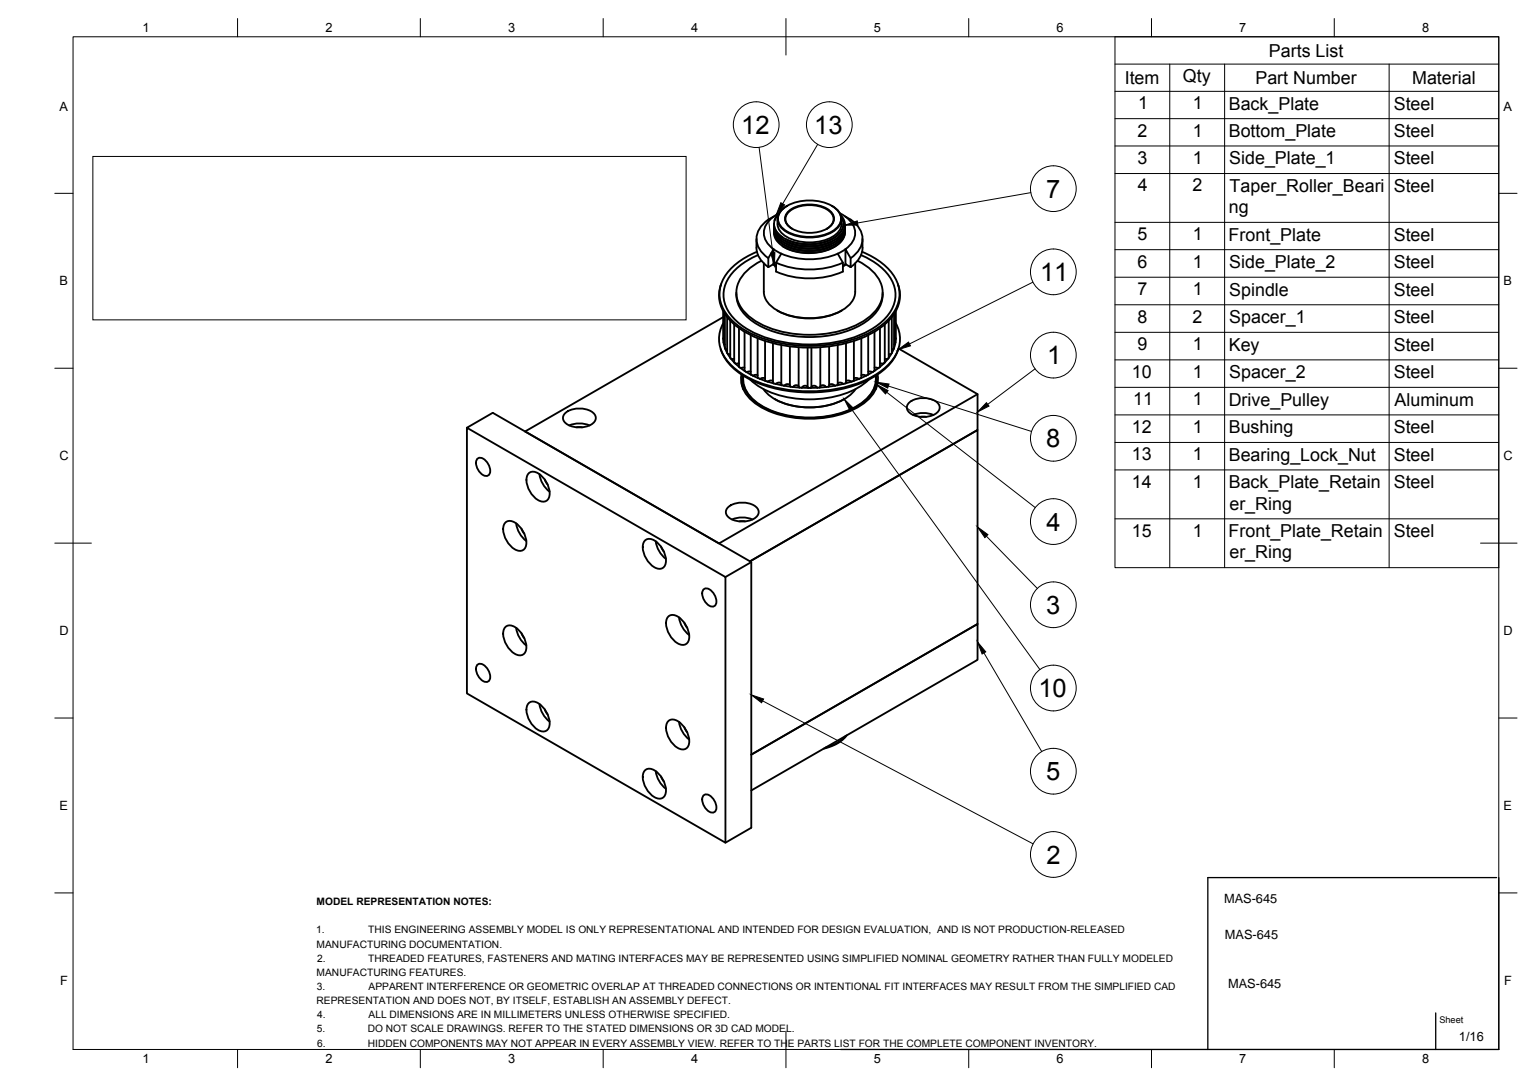
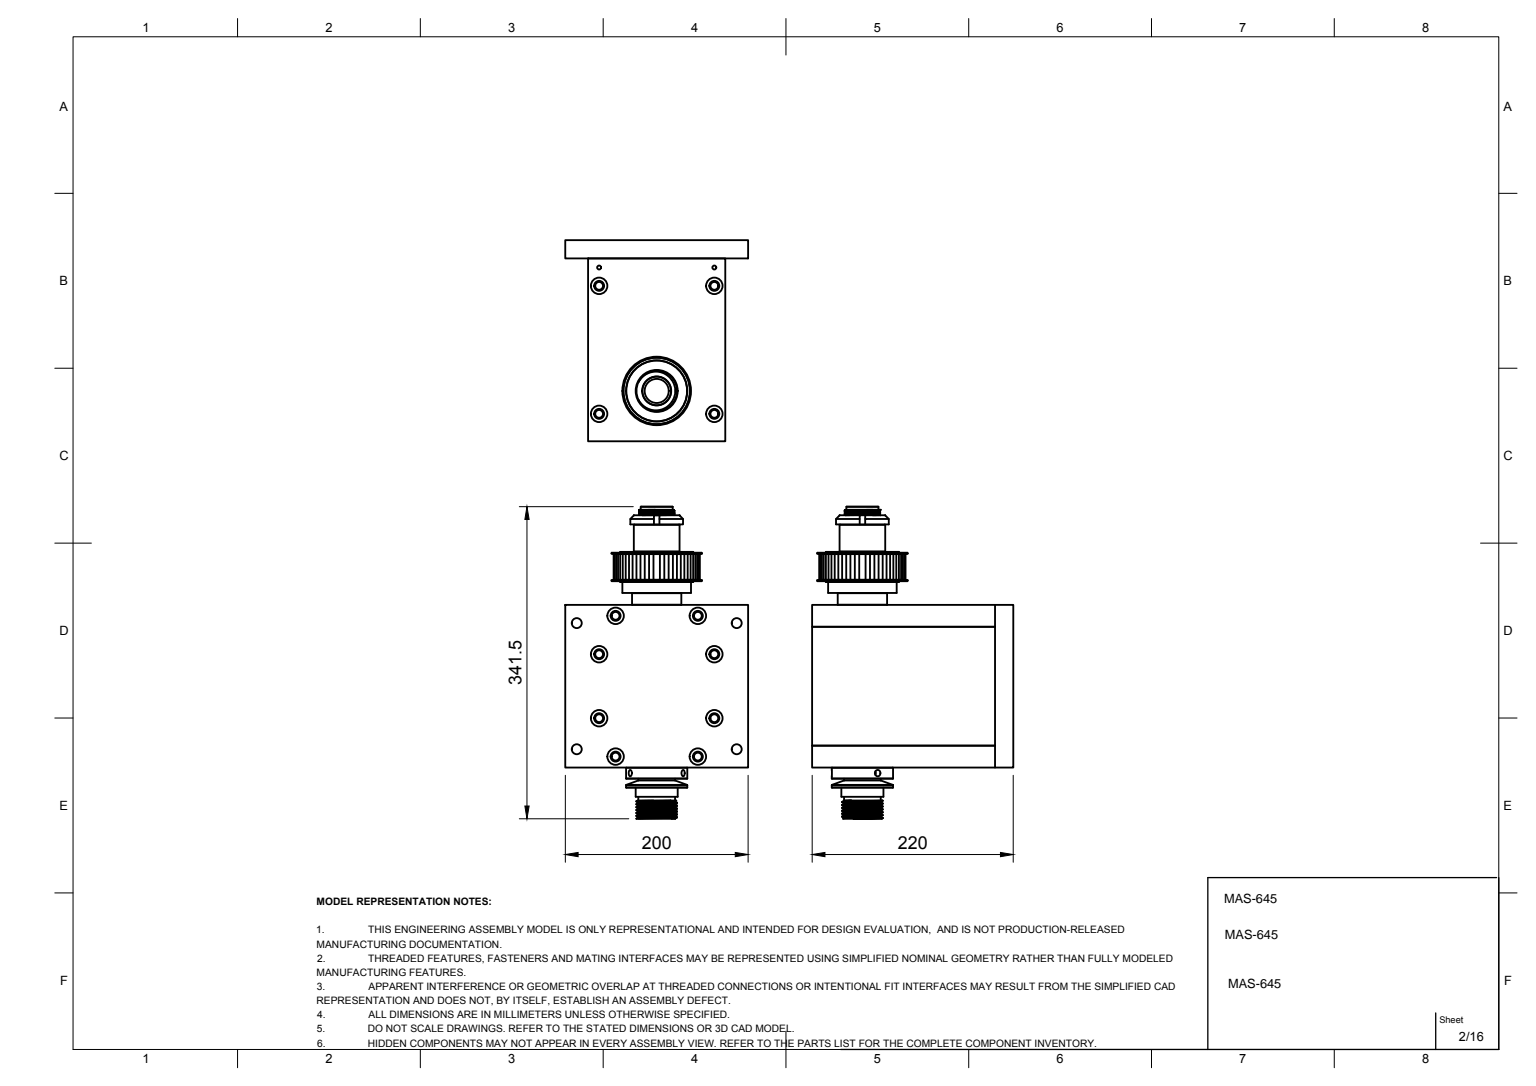
ISO-10303-21;
HEADER;
FILE_DESCRIPTION((''),'2;1');
FILE_NAME('MAS-645','2026-10-09T10:54:55-07:00',(''),(''),'','','');
FILE_SCHEMA (('AUTOMOTIVE_DESIGN { 1 0 10303 214 3 1 1 }'));
ENDSEC;
DATA;
#10 = MECHANICAL_DESIGN_GEOMETRIC_PRESENTATION_REPRESENTATION('',(#595,#596,
#597,#598,#599,#600,#601,#602,#603,#604,#605,#606,#607,#608,#609),#63824) ;
#11 = ITEM_DEFINED_TRANSFORMATION($,$,#15676,#17885) ;
#12 = ITEM_DEFINED_TRANSFORMATION($,$,#15762,#17886) ;
#13 = ITEM_DEFINED_TRANSFORMATION($,$,#15853,#17887) ;
#14 = ITEM_DEFINED_TRANSFORMATION($,$,#17272,#17888) ;
#15 = ITEM_DEFINED_TRANSFORMATION($,$,#15892,#17889) ;
#16 = ITEM_DEFINED_TRANSFORMATION($,$,#15986,#17890) ;
#17 = ITEM_DEFINED_TRANSFORMATION($,$,#16025,#17891) ;
#18 = ITEM_DEFINED_TRANSFORMATION($,$,#17802,#17892) ;
#19 = ITEM_DEFINED_TRANSFORMATION($,$,#16168,#17893) ;
#20 = ITEM_DEFINED_TRANSFORMATION($,$,#16191,#17894) ;
#21 = ITEM_DEFINED_TRANSFORMATION($,$,#16208,#17895) ;
#22 = ITEM_DEFINED_TRANSFORMATION($,$,#17207,#17896) ;
#23 = ITEM_DEFINED_TRANSFORMATION($,$,#17226,#17897) ;
#24 = ITEM_DEFINED_TRANSFORMATION($,$,#17272,#17898) ;
#25 = ITEM_DEFINED_TRANSFORMATION($,$,#17802,#17899) ;
#26 = ITEM_DEFINED_TRANSFORMATION($,$,#17819,#17900) ;
#27 = ITEM_DEFINED_TRANSFORMATION($,$,#17852,#17901) ;
#28 = (
REPRESENTATION_RELATIONSHIP($,$,#63879,#63878)
REPRESENTATION_RELATIONSHIP_WITH_TRANSFORMATION(#11)
SHAPE_REPRESENTATION_RELATIONSHIP()
) ;
#29 = (
REPRESENTATION_RELATIONSHIP($,$,#63880,#63878)
REPRESENTATION_RELATIONSHIP_WITH_TRANSFORMATION(#12)
SHAPE_REPRESENTATION_RELATIONSHIP()
) ;
#30 = (
REPRESENTATION_RELATIONSHIP($,$,#63881,#63878)
REPRESENTATION_RELATIONSHIP_WITH_TRANSFORMATION(#13)
SHAPE_REPRESENTATION_RELATIONSHIP()
) ;
#31 = (
REPRESENTATION_RELATIONSHIP($,$,#63890,#63878)
REPRESENTATION_RELATIONSHIP_WITH_TRANSFORMATION(#14)
SHAPE_REPRESENTATION_RELATIONSHIP()
) ;
#32 = (
REPRESENTATION_RELATIONSHIP($,$,#63882,#63878)
REPRESENTATION_RELATIONSHIP_WITH_TRANSFORMATION(#15)
SHAPE_REPRESENTATION_RELATIONSHIP()
) ;
#33 = (
REPRESENTATION_RELATIONSHIP($,$,#63883,#63878)
REPRESENTATION_RELATIONSHIP_WITH_TRANSFORMATION(#16)
SHAPE_REPRESENTATION_RELATIONSHIP()
) ;
#34 = (
REPRESENTATION_RELATIONSHIP($,$,#63884,#63878)
REPRESENTATION_RELATIONSHIP_WITH_TRANSFORMATION(#17)
SHAPE_REPRESENTATION_RELATIONSHIP()
) ;
#35 = (
REPRESENTATION_RELATIONSHIP($,$,#63891,#63878)
REPRESENTATION_RELATIONSHIP_WITH_TRANSFORMATION(#18)
SHAPE_REPRESENTATION_RELATIONSHIP()
) ;
#36 = (
REPRESENTATION_RELATIONSHIP($,$,#63885,#63878)
REPRESENTATION_RELATIONSHIP_WITH_TRANSFORMATION(#19)
SHAPE_REPRESENTATION_RELATIONSHIP()
) ;
#37 = (
REPRESENTATION_RELATIONSHIP($,$,#63886,#63878)
REPRESENTATION_RELATIONSHIP_WITH_TRANSFORMATION(#20)
SHAPE_REPRESENTATION_RELATIONSHIP()
) ;
#38 = (
REPRESENTATION_RELATIONSHIP($,$,#63887,#63878)
REPRESENTATION_RELATIONSHIP_WITH_TRANSFORMATION(#21)
SHAPE_REPRESENTATION_RELATIONSHIP()
) ;
#39 = (
REPRESENTATION_RELATIONSHIP($,$,#63888,#63878)
REPRESENTATION_RELATIONSHIP_WITH_TRANSFORMATION(#22)
SHAPE_REPRESENTATION_RELATIONSHIP()
) ;
#40 = (
REPRESENTATION_RELATIONSHIP($,$,#63889,#63878)
REPRESENTATION_RELATIONSHIP_WITH_TRANSFORMATION(#23)
SHAPE_REPRESENTATION_RELATIONSHIP()
) ;
#41 = (
REPRESENTATION_RELATIONSHIP($,$,#63890,#63878)
REPRESENTATION_RELATIONSHIP_WITH_TRANSFORMATION(#24)
SHAPE_REPRESENTATION_RELATIONSHIP()
) ;
#42 = (
REPRESENTATION_RELATIONSHIP($,$,#63891,#63878)
REPRESENTATION_RELATIONSHIP_WITH_TRANSFORMATION(#25)
SHAPE_REPRESENTATION_RELATIONSHIP()
) ;
#43 = (
REPRESENTATION_RELATIONSHIP($,$,#63892,#63878)
REPRESENTATION_RELATIONSHIP_WITH_TRANSFORMATION(#26)
SHAPE_REPRESENTATION_RELATIONSHIP()
) ;
#44 = (
REPRESENTATION_RELATIONSHIP($,$,#63893,#63878)
REPRESENTATION_RELATIONSHIP_WITH_TRANSFORMATION(#27)
SHAPE_REPRESENTATION_RELATIONSHIP()
) ;
#45 = CONTEXT_DEPENDENT_SHAPE_REPRESENTATION(#28,#63861) ;
#46 = CONTEXT_DEPENDENT_SHAPE_REPRESENTATION(#29,#63862) ;
#47 = CONTEXT_DEPENDENT_SHAPE_REPRESENTATION(#30,#63863) ;
#48 = CONTEXT_DEPENDENT_SHAPE_REPRESENTATION(#31,#63864) ;
#49 = CONTEXT_DEPENDENT_SHAPE_REPRESENTATION(#32,#63865) ;
#50 = CONTEXT_DEPENDENT_SHAPE_REPRESENTATION(#33,#63866) ;
#51 = CONTEXT_DEPENDENT_SHAPE_REPRESENTATION(#34,#63867) ;
#52 = CONTEXT_DEPENDENT_SHAPE_REPRESENTATION(#35,#63868) ;
#53 = CONTEXT_DEPENDENT_SHAPE_REPRESENTATION(#36,#63869) ;
#54 = CONTEXT_DEPENDENT_SHAPE_REPRESENTATION(#37,#63870) ;
#55 = CONTEXT_DEPENDENT_SHAPE_REPRESENTATION(#38,#63871) ;
#56 = CONTEXT_DEPENDENT_SHAPE_REPRESENTATION(#39,#63872) ;
#57 = CONTEXT_DEPENDENT_SHAPE_REPRESENTATION(#40,#63873) ;
#58 = CONTEXT_DEPENDENT_SHAPE_REPRESENTATION(#41,#63874) ;
#59 = CONTEXT_DEPENDENT_SHAPE_REPRESENTATION(#42,#63875) ;
#60 = CONTEXT_DEPENDENT_SHAPE_REPRESENTATION(#43,#63876) ;
#61 = CONTEXT_DEPENDENT_SHAPE_REPRESENTATION(#44,#63877) ;
#62 = NEXT_ASSEMBLY_USAGE_OCCURRENCE('Back_Plate:1','Back_Plate:1',
'Back_Plate:1',#63895,#63896,'Back_Plate:1') ;
#63 = NEXT_ASSEMBLY_USAGE_OCCURRENCE('Bottom_Plate:1','Bottom_Plate:1',
'Bottom_Plate:1',#63895,#63897,'Bottom_Plate:1') ;
#64 = NEXT_ASSEMBLY_USAGE_OCCURRENCE('Side_Plate_1:1','Side_Plate_1:1',
'Side_Plate_1:1',#63895,#63898,'Side_Plate_1:1') ;
#65 = NEXT_ASSEMBLY_USAGE_OCCURRENCE('Taper_Roller_Bearing:1',
'Taper_Roller_Bearing:1','Taper_Roller_Bearing:1',#63895,#63907,
'Taper_Roller_Bearing:1') ;
#66 = NEXT_ASSEMBLY_USAGE_OCCURRENCE('Front_Plate:1','Front_Plate:1',
'Front_Plate:1',#63895,#63899,'Front_Plate:1') ;
#67 = NEXT_ASSEMBLY_USAGE_OCCURRENCE('Side_Plate_2:1','Side_Plate_2:1',
'Side_Plate_2:1',#63895,#63900,'Side_Plate_2:1') ;
#68 = NEXT_ASSEMBLY_USAGE_OCCURRENCE('Spindle:1','Spindle:1','Spindle:1',
#63895,#63901,'Spindle:1') ;
#69 = NEXT_ASSEMBLY_USAGE_OCCURRENCE('Spacer_1:1','Spacer_1:1',
'Spacer_1:1',#63895,#63908,'Spacer_1:1') ;
#70 = NEXT_ASSEMBLY_USAGE_OCCURRENCE('Key:1','Key:1','Key:1',#63895,#63902,
'Key:1') ;
#71 = NEXT_ASSEMBLY_USAGE_OCCURRENCE('Spacer_2:1','Spacer_2:1',
'Spacer_2:1',#63895,#63903,'Spacer_2:1') ;
#72 = NEXT_ASSEMBLY_USAGE_OCCURRENCE('Drive_Pulley:1','Drive_Pulley:1',
'Drive_Pulley:1',#63895,#63904,'Drive_Pulley:1') ;
#73 = NEXT_ASSEMBLY_USAGE_OCCURRENCE('Bushing:1','Bushing:1','Bushing:1',
#63895,#63905,'Bushing:1') ;
#74 = NEXT_ASSEMBLY_USAGE_OCCURRENCE('Bearing_Lock_Nut:1',
'Bearing_Lock_Nut:1','Bearing_Lock_Nut:1',#63895,#63906,
'Bearing_Lock_Nut:1') ;
#75 = NEXT_ASSEMBLY_USAGE_OCCURRENCE('Taper_Roller_Bearing:2',
'Taper_Roller_Bearing:2','Taper_Roller_Bearing:2',#63895,#63907,
'Taper_Roller_Bearing:2') ;
#76 = NEXT_ASSEMBLY_USAGE_OCCURRENCE('Spacer_1:2','Spacer_1:2',
'Spacer_1:2',#63895,#63908,'Spacer_1:2') ;
#77 = NEXT_ASSEMBLY_USAGE_OCCURRENCE('Back_Plate_Retainer_Ring:1',
'Back_Plate_Retainer_Ring:1','Back_Plate_Retainer_Ring:1',#63895,#63909,
'Back_Plate_Retainer_Ring:1') ;
#78 = NEXT_ASSEMBLY_USAGE_OCCURRENCE('Front_Plate_Retainer_Ring:1',
'Front_Plate_Retainer_Ring:1','Front_Plate_Retainer_Ring:1',#63895,#63910,
'Front_Plate_Retainer_Ring:1') ;
#79 = TOROIDAL_SURFACE('',#17489,23.5,1.) ;
#80 = TOROIDAL_SURFACE('',#17493,36.5,1.) ;
#81 = TOROIDAL_SURFACE('',#17497,37.25,0.25) ;
#82 = TOROIDAL_SURFACE('',#17503,22.75,0.249999999999998) ;
#83 = (
BOUNDED_CURVE()
B_SPLINE_CURVE(2,(#53752,#53753,#53754),.UNSPECIFIED.,.F.,.F.)
B_SPLINE_CURVE_WITH_KNOTS((3,3),(0.,0.567460423251311),.UNSPECIFIED.)
CURVE()
GEOMETRIC_REPRESENTATION_ITEM()
RATIONAL_B_SPLINE_CURVE((1.,1.00278960134448,1.))
REPRESENTATION_ITEM('')
) ;
#84 = (
BOUNDED_CURVE()
B_SPLINE_CURVE(2,(#53763,#53764,#53765),.UNSPECIFIED.,.F.,.F.)
B_SPLINE_CURVE_WITH_KNOTS((3,3),(0.,0.567460423251311),.UNSPECIFIED.)
CURVE()
GEOMETRIC_REPRESENTATION_ITEM()
RATIONAL_B_SPLINE_CURVE((1.,1.00278960136551,1.))
REPRESENTATION_ITEM('')
) ;
#85 = (
BOUNDED_CURVE()
B_SPLINE_CURVE(2,(#53809,#53810,#53811),.UNSPECIFIED.,.F.,.F.)
B_SPLINE_CURVE_WITH_KNOTS((3,3),(0.,0.567460423251311),.UNSPECIFIED.)
CURVE()
GEOMETRIC_REPRESENTATION_ITEM()
RATIONAL_B_SPLINE_CURVE((1.,1.00278960136494,1.))
REPRESENTATION_ITEM('')
) ;
#86 = (
BOUNDED_CURVE()
B_SPLINE_CURVE(2,(#53815,#53816,#53817),.UNSPECIFIED.,.F.,.F.)
B_SPLINE_CURVE_WITH_KNOTS((3,3),(0.,0.567460423251311),.UNSPECIFIED.)
CURVE()
GEOMETRIC_REPRESENTATION_ITEM()
RATIONAL_B_SPLINE_CURVE((1.,1.0027896013635,1.))
REPRESENTATION_ITEM('')
) ;
#87 = (
BOUNDED_CURVE()
B_SPLINE_CURVE(2,(#53831,#53832,#53833),.UNSPECIFIED.,.F.,.F.)
B_SPLINE_CURVE_WITH_KNOTS((3,3),(0.,0.567460423251311),.UNSPECIFIED.)
CURVE()
GEOMETRIC_REPRESENTATION_ITEM()
RATIONAL_B_SPLINE_CURVE((1.,1.0027896013647,1.))
REPRESENTATION_ITEM('')
) ;
#88 = (
BOUNDED_CURVE()
B_SPLINE_CURVE(2,(#53837,#53838,#53839),.UNSPECIFIED.,.F.,.F.)
B_SPLINE_CURVE_WITH_KNOTS((3,3),(0.,0.567460423251311),.UNSPECIFIED.)
CURVE()
GEOMETRIC_REPRESENTATION_ITEM()
RATIONAL_B_SPLINE_CURVE((1.,1.002789601364,1.))
REPRESENTATION_ITEM('')
) ;
#89 = (
BOUNDED_CURVE()
B_SPLINE_CURVE(2,(#53853,#53854,#53855),.UNSPECIFIED.,.F.,.F.)
B_SPLINE_CURVE_WITH_KNOTS((3,3),(0.,0.56746042325131),.UNSPECIFIED.)
CURVE()
GEOMETRIC_REPRESENTATION_ITEM()
RATIONAL_B_SPLINE_CURVE((1.,1.00278960137803,1.))
REPRESENTATION_ITEM('')
) ;
#90 = (
BOUNDED_CURVE()
B_SPLINE_CURVE(2,(#53859,#53860,#53861),.UNSPECIFIED.,.F.,.F.)
B_SPLINE_CURVE_WITH_KNOTS((3,3),(0.,0.56746042325131),.UNSPECIFIED.)
CURVE()
GEOMETRIC_REPRESENTATION_ITEM()
RATIONAL_B_SPLINE_CURVE((1.,1.00278960137803,1.))
REPRESENTATION_ITEM('')
) ;
#91 = ELLIPSE('',#16171,7.07106781186547,5.) ;
#92 = ELLIPSE('',#16172,7.07106781186548,5.) ;
#93 = ELLIPSE('',#16174,7.07106781186548,5.) ;
#94 = ELLIPSE('',#16175,7.07106781186547,5.) ;
#95 = ELLIPSE('',#16178,7.07106781186546,4.99999999999999) ;
#96 = ELLIPSE('',#16180,7.07106781186546,4.99999999999999) ;
#97 = ELLIPSE('',#16181,7.07106781186546,4.99999999999999) ;
#98 = ELLIPSE('',#16183,7.07106781186546,4.99999999999999) ;
#99 = ELLIPSE('',#17336,29.1332609148258,28.6226076794831) ;
#100 = ELLIPSE('',#17338,29.1332609148259,28.622607679483) ;
#101 = ELLIPSE('',#17340,29.133260914826,28.6226076794829) ;
#102 = ELLIPSE('',#17342,29.1332609148258,28.622607679483) ;
#103 = ELLIPSE('',#17344,29.1332609148258,28.6226076794831) ;
#104 = ELLIPSE('',#17346,29.1332609148257,28.6226076794832) ;
#105 = ELLIPSE('',#17348,29.133260914826,28.6226076794829) ;
#106 = ELLIPSE('',#17350,29.1332609148257,28.6226076794832) ;
#107 = ELLIPSE('',#17353,29.1332609148258,28.622607679483) ;
#108 = ELLIPSE('',#17355,29.1332609148257,28.6226076794832) ;
#109 = ELLIPSE('',#17357,29.1332609148255,28.6226076794833) ;
#110 = ELLIPSE('',#17359,29.1332609148258,28.6226076794831) ;
#111 = ELLIPSE('',#17362,29.1332609148257,28.6226076794832) ;
#112 = ELLIPSE('',#17364,29.1332609148257,28.6226076794831) ;
#113 = ELLIPSE('',#17366,29.1332609148259,28.622607679483) ;
#114 = ELLIPSE('',#17368,29.1332609148258,28.6226076794831) ;
#115 = ELLIPSE('',#17370,29.1332609148257,28.6226076794831) ;
#116 = ELLIPSE('',#17372,29.1332609148258,28.6226076794831) ;
#117 = ELLIPSE('',#17374,29.1332609148258,28.6226076794831) ;
#118 = ELLIPSE('',#17376,29.1332609148258,28.6226076794831) ;
#119 = ELLIPSE('',#17378,29.1332609148259,28.622607679483) ;
#120 = ELLIPSE('',#17380,29.1332609148258,28.622607679483) ;
#121 = ELLIPSE('',#17382,29.1332609148258,28.6226076794831) ;
#122 = ELLIPSE('',#17384,29.1332609148258,28.622607679483) ;
#123 = ELLIPSE('',#17386,29.1332609148258,28.6226076794831) ;
#124 = ELLIPSE('',#17388,29.1332609148258,28.6226076794831) ;
#125 = ELLIPSE('',#17390,29.1332609148258,28.6226076794831) ;
#126 = ELLIPSE('',#17392,29.1332609148258,28.6226076794831) ;
#127 = ELLIPSE('',#17393,29.1332609148257,28.6226076794832) ;
#128 = ELLIPSE('',#17395,29.8160190680257,29.3077933083081) ;
#129 = ELLIPSE('',#17396,29.8160190680257,29.3077933083081) ;
#130 = ELLIPSE('',#17397,29.8160190680257,29.3077933083081) ;
#131 = ELLIPSE('',#17398,29.8160190680257,29.3077933083081) ;
#132 = ELLIPSE('',#17399,29.8160190680257,29.3077933083081) ;
#133 = ELLIPSE('',#17400,29.8160190680257,29.3077933083081) ;
#134 = ELLIPSE('',#17401,29.8160190680257,29.3077933083081) ;
#135 = ELLIPSE('',#17402,29.8160190680257,29.3077933083081) ;
#136 = ELLIPSE('',#17403,29.8160190680257,29.3077933083081) ;
#137 = ELLIPSE('',#17404,29.8160190680257,29.3077933083081) ;
#138 = ELLIPSE('',#17405,29.8160190680257,29.3077933083081) ;
#139 = ELLIPSE('',#17406,29.8160190680257,29.3077933083081) ;
#140 = ELLIPSE('',#17407,29.8160190680257,29.3077933083081) ;
#141 = ELLIPSE('',#17408,29.8160190680257,29.3077933083081) ;
#142 = ELLIPSE('',#17409,29.8160190680257,29.3077933083081) ;
#143 = ELLIPSE('',#17410,29.8160190680257,29.3077933083081) ;
#144 = ELLIPSE('',#17411,29.8160190680257,29.3077933083081) ;
#145 = ELLIPSE('',#17412,29.8160190680257,29.3077933083081) ;
#146 = ELLIPSE('',#17413,29.8160190680257,29.3077933083081) ;
#147 = ELLIPSE('',#17414,29.8160190680257,29.3077933083081) ;
#148 = ELLIPSE('',#17415,29.8160190680257,29.3077933083081) ;
#149 = ELLIPSE('',#17416,29.8160190680257,29.3077933083081) ;
#150 = ELLIPSE('',#17417,29.8160190680257,29.3077933083081) ;
#151 = ELLIPSE('',#17418,29.8160190680257,29.3077933083081) ;
#152 = ELLIPSE('',#17419,29.8160190680257,29.3077933083081) ;
#153 = ELLIPSE('',#17420,29.8160190680257,29.3077933083081) ;
#154 = ELLIPSE('',#17421,29.8160190680257,29.3077933083082) ;
#155 = ELLIPSE('',#17422,29.8160190680257,29.3077933083082) ;
#156 = ELLIPSE('',#17423,29.8160190680257,29.3077933083082) ;
#157 = ELLIPSE('',#17424,29.8160190680257,29.3077933083082) ;
#158 = ELLIPSE('',#17425,29.8160190680257,29.3077933083081) ;
#159 = ELLIPSE('',#17426,29.8160190680257,29.3077933083081) ;
#160 = ELLIPSE('',#17427,29.8160190680257,29.3077933083081) ;
#161 = ELLIPSE('',#17428,29.8160190680257,29.3077933083081) ;
#162 = ELLIPSE('',#17429,29.8160190680257,29.3077933083081) ;
#163 = ELLIPSE('',#17430,29.8160190680257,29.3077933083081) ;
#164 = ELLIPSE('',#17431,29.8160190680257,29.3077933083081) ;
#165 = ELLIPSE('',#17432,29.8160190680257,29.3077933083081) ;
#166 = ELLIPSE('',#17433,29.8160190680257,29.3077933083081) ;
#167 = ELLIPSE('',#17434,29.8160190680257,29.3077933083081) ;
#168 = ELLIPSE('',#17435,29.8160190680257,29.3077933083082) ;
#169 = ELLIPSE('',#17436,29.8160190680257,29.3077933083082) ;
#170 = ELLIPSE('',#17437,29.8160190680257,29.3077933083081) ;
#171 = ELLIPSE('',#17438,29.8160190680257,29.3077933083081) ;
#172 = ELLIPSE('',#17439,29.8160190680257,29.3077933083081) ;
#173 = ELLIPSE('',#17440,29.8160190680257,29.3077933083081) ;
#174 = ELLIPSE('',#17441,29.8160190680257,29.3077933083081) ;
#175 = ELLIPSE('',#17442,29.8160190680257,29.3077933083081) ;
#176 = ELLIPSE('',#17443,29.8160190680257,29.3077933083081) ;
#177 = ELLIPSE('',#17444,29.8160190680257,29.3077933083081) ;
#178 = ELLIPSE('',#17445,29.8160190680257,29.3077933083081) ;
#179 = ELLIPSE('',#17446,29.8160190680257,29.3077933083081) ;
#180 = ELLIPSE('',#17447,29.8160190680257,29.3077933083081) ;
#181 = ELLIPSE('',#17448,29.8160190680257,29.3077933083081) ;
#182 = ELLIPSE('',#17449,29.8160190680257,29.3077933083082) ;
#183 = ELLIPSE('',#17450,29.8160190680257,29.3077933083082) ;
#184 = ELLIPSE('',#17451,29.8160190680257,29.3077933083081) ;
#185 = ELLIPSE('',#17452,29.8160190680257,29.3077933083081) ;
#186 = ELLIPSE('',#17457,35.9515371622909,35.3123204328217) ;
#187 = ELLIPSE('',#17458,35.9515371622912,35.3123204328215) ;
#188 = ELLIPSE('',#17459,35.9515371622912,35.3123204328215) ;
#189 = ELLIPSE('',#17460,35.9515371622913,35.3123204328214) ;
#190 = ELLIPSE('',#17461,35.951537162291,35.3123204328217) ;
#191 = ELLIPSE('',#17462,35.9515371622911,35.3123204328216) ;
#192 = ELLIPSE('',#17463,35.9515371622911,35.3123204328216) ;
#193 = ELLIPSE('',#17464,35.9515371622911,35.3123204328216) ;
#194 = ELLIPSE('',#17465,35.9515371622913,35.3123204328214) ;
#195 = ELLIPSE('',#17466,35.951537162291,35.3123204328217) ;
#196 = ELLIPSE('',#17467,35.9515371622912,35.3123204328215) ;
#197 = ELLIPSE('',#17468,35.9515371622911,35.3123204328216) ;
#198 = ELLIPSE('',#17469,35.951537162291,35.3123204328217) ;
#199 = ELLIPSE('',#17470,35.9515371622913,35.3123204328214) ;
#200 = ELLIPSE('',#17471,35.951537162291,35.3123204328217) ;
#201 = ELLIPSE('',#17472,35.951537162291,35.3123204328217) ;
#202 = ELLIPSE('',#17473,35.9515371622912,35.3123204328215) ;
#203 = ELLIPSE('',#17474,35.9515371622911,35.3123204328216) ;
#204 = ELLIPSE('',#17475,35.9515371622911,35.3123204328216) ;
#205 = ELLIPSE('',#17476,35.951537162291,35.3123204328217) ;
#206 = ELLIPSE('',#17477,35.9515371622911,35.3123204328215) ;
#207 = ELLIPSE('',#17478,35.9515371622911,35.3123204328216) ;
#208 = ELLIPSE('',#17479,35.9515371622913,35.3123204328214) ;
#209 = ELLIPSE('',#17480,35.9515371622912,35.3123204328215) ;
#210 = ELLIPSE('',#17481,35.951537162291,35.3123204328217) ;
#211 = ELLIPSE('',#17482,35.9515371622911,35.3123204328216) ;
#212 = ELLIPSE('',#17483,35.9515371622913,35.3123204328214) ;
#213 = ELLIPSE('',#17484,35.9515371622912,35.3123204328215) ;
#214 = ELLIPSE('',#17485,35.9515371622911,35.3123204328216) ;
#215 = B_SPLINE_SURFACE_WITH_KNOTS('',3,1,((#48544,#48545),(#48546,#48547),
(#48548,#48549),(#48550,#48551),(#48552,#48553),(#48554,#48555),(#48556,
#48557),(#48558,#48559),(#48560,#48561),(#48562,#48563),(#48564,#48565),
(#48566,#48567),(#48568,#48569),(#48570,#48571),(#48572,#48573),(#48574,
#48575),(#48576,#48577),(#48578,#48579),(#48580,#48581),(#48582,#48583),
(#48584,#48585),(#48586,#48587),(#48588,#48589),(#48590,#48591),(#48592,
#48593),(#48594,#48595),(#48596,#48597),(#48598,#48599),(#48600,#48601),
(#48602,#48603),(#48604,#48605),(#48606,#48607),(#48608,#48609),(#48610,
#48611)),.UNSPECIFIED.,.T.,.F.,.F.,(4,2,2,2,2,2,2,2,2,2,2,2,2,2,2,2,4),
(2,2),(0.,0.131943994423176,0.263887988846351,0.395831447701094,0.527774906555838,
0.659718365410582,0.791661824265325,0.9236058186885,1.05554981311168,1.18749380753485,
1.31943780195803,1.45138126081277,1.58332471966751,1.71526817852226,1.847211637377,
1.97915563180018,2.11109962622335),(0.,1.00001320870816),.UNSPECIFIED.) ;
#216 = B_SPLINE_SURFACE_WITH_KNOTS('',3,1,((#48671,#48672),(#48673,#48674),
(#48675,#48676),(#48677,#48678),(#48679,#48680),(#48681,#48682),(#48683,
#48684),(#48685,#48686),(#48687,#48688),(#48689,#48690),(#48691,#48692),
(#48693,#48694),(#48695,#48696),(#48697,#48698),(#48699,#48700),(#48701,
#48702),(#48703,#48704),(#48705,#48706),(#48707,#48708),(#48709,#48710),
(#48711,#48712),(#48713,#48714),(#48715,#48716),(#48717,#48718),(#48719,
#48720),(#48721,#48722),(#48723,#48724),(#48725,#48726),(#48727,#48728),
(#48729,#48730),(#48731,#48732),(#48733,#48734),(#48735,#48736),(#48737,
#48738)),.UNSPECIFIED.,.T.,.F.,.F.,(4,2,2,2,2,2,2,2,2,2,2,2,2,2,2,2,4),
(2,2),(0.,0.131943994423175,0.263887988846351,0.395831447701094,0.527774906555838,
0.659718365410582,0.791661824265325,0.923605818688501,1.05554981311168,
1.18749380753485,1.31943780195803,1.45138126081277,1.58332471966751,1.71526817852226,
1.847211637377,1.97915563180018,2.11109962622335),(0.,1.00001320870815),
 .UNSPECIFIED.) ;
#217 = B_SPLINE_SURFACE_WITH_KNOTS('',3,1,((#48798,#48799),(#48800,#48801),
(#48802,#48803),(#48804,#48805),(#48806,#48807),(#48808,#48809),(#48810,
#48811),(#48812,#48813),(#48814,#48815),(#48816,#48817),(#48818,#48819),
(#48820,#48821),(#48822,#48823),(#48824,#48825),(#48826,#48827),(#48828,
#48829),(#48830,#48831),(#48832,#48833),(#48834,#48835),(#48836,#48837),
(#48838,#48839),(#48840,#48841),(#48842,#48843),(#48844,#48845),(#48846,
#48847),(#48848,#48849),(#48850,#48851),(#48852,#48853),(#48854,#48855),
(#48856,#48857),(#48858,#48859),(#48860,#48861),(#48862,#48863),(#48864,
#48865)),.UNSPECIFIED.,.T.,.F.,.F.,(4,2,2,2,2,2,2,2,2,2,2,2,2,2,2,2,4),
(2,2),(0.,0.131943994423175,0.26388798884635,0.395831447701094,0.527774906555837,
0.659718365410581,0.791661824265324,0.9236058186885,1.05554981311168,1.18749380753485,
1.31943780195803,1.45138126081277,1.58332471966751,1.71526817852226,1.847211637377,
1.97915563180018,2.11109962622335),(0.,1.00001320870816),.UNSPECIFIED.) ;
#218 = B_SPLINE_SURFACE_WITH_KNOTS('',3,3,((#48925,#48926,#48927,#48928,#48929,
#48930,#48931,#48932,#48933,#48934,#48935,#48936,#48937,#48938,#48939,#48940,
#48941,#48942,#48943,#48944,#48945,#48946,#48947,#48948,#48949,#48950,#48951,
#48952,#48953,#48954,#48955,#48956,#48957,#48958,#48959,#48960,#48961,#48962,
#48963,#48964,#48965,#48966,#48967,#48968,#48969,#48970,#48971,#48972,#48973,
#48974,#48975,#48976,#48977,#48978,#48979,#48980,#48981,#48982,#48983,#48984,
#48985,#48986,#48987,#48988,#48989,#48990,#48991,#48992,#48993,#48994,#48995,
#48996,#48997,#48998,#48999,#49000,#49001,#49002,#49003,#49004,#49005,#49006,
#49007,#49008,#49009,#49010,#49011,#49012,#49013,#49014,#49015,#49016,#49017,
#49018,#49019,#49020,#49021,#49022,#49023,#49024,#49025,#49026,#49027,#49028,
#49029,#49030,#49031,#49032,#49033,#49034,#49035,#49036,#49037,#49038,#49039,
#49040,#49041,#49042,#49043,#49044,#49045,#49046,#49047,#49048,#49049,#49050,
#49051,#49052,#49053,#49054,#49055,#49056,#49057,#49058,#49059,#49060,#49061,
#49062,#49063,#49064,#49065,#49066,#49067,#49068,#49069,#49070,#49071,#49072,
#49073,#49074,#49075,#49076,#49077,#49078,#49079,#49080,#49081,#49082,#49083,
#49084,#49085,#49086,#49087,#49088,#49089,#49090,#49091,#49092,#49093,#49094,
#49095,#49096,#49097),(#49098,#49099,#49100,#49101,#49102,#49103,#49104,
#49105,#49106,#49107,#49108,#49109,#49110,#49111,#49112,#49113,#49114,#49115,
#49116,#49117,#49118,#49119,#49120,#49121,#49122,#49123,#49124,#49125,#49126,
#49127,#49128,#49129,#49130,#49131,#49132,#49133,#49134,#49135,#49136,#49137,
#49138,#49139,#49140,#49141,#49142,#49143,#49144,#49145,#49146,#49147,#49148,
#49149,#49150,#49151,#49152,#49153,#49154,#49155,#49156,#49157,#49158,#49159,
#49160,#49161,#49162,#49163,#49164,#49165,#49166,#49167,#49168,#49169,#49170,
#49171,#49172,#49173,#49174,#49175,#49176,#49177,#49178,#49179,#49180,#49181,
#49182,#49183,#49184,#49185,#49186,#49187,#49188,#49189,#49190,#49191,#49192,
#49193,#49194,#49195,#49196,#49197,#49198,#49199,#49200,#49201,#49202,#49203,
#49204,#49205,#49206,#49207,#49208,#49209,#49210,#49211,#49212,#49213,#49214,
#49215,#49216,#49217,#49218,#49219,#49220,#49221,#49222,#49223,#49224,#49225,
#49226,#49227,#49228,#49229,#49230,#49231,#49232,#49233,#49234,#49235,#49236,
#49237,#49238,#49239,#49240,#49241,#49242,#49243,#49244,#49245,#49246,#49247,
#49248,#49249,#49250,#49251,#49252,#49253,#49254,#49255,#49256,#49257,#49258,
#49259,#49260,#49261,#49262,#49263,#49264,#49265,#49266,#49267,#49268,#49269,
#49270),(#49271,#49272,#49273,#49274,#49275,#49276,#49277,#49278,#49279,
#49280,#49281,#49282,#49283,#49284,#49285,#49286,#49287,#49288,#49289,#49290,
#49291,#49292,#49293,#49294,#49295,#49296,#49297,#49298,#49299,#49300,#49301,
#49302,#49303,#49304,#49305,#49306,#49307,#49308,#49309,#49310,#49311,#49312,
#49313,#49314,#49315,#49316,#49317,#49318,#49319,#49320,#49321,#49322,#49323,
#49324,#49325,#49326,#49327,#49328,#49329,#49330,#49331,#49332,#49333,#49334,
#49335,#49336,#49337,#49338,#49339,#49340,#49341,#49342,#49343,#49344,#49345,
#49346,#49347,#49348,#49349,#49350,#49351,#49352,#49353,#49354,#49355,#49356,
#49357,#49358,#49359,#49360,#49361,#49362,#49363,#49364,#49365,#49366,#49367,
#49368,#49369,#49370,#49371,#49372,#49373,#49374,#49375,#49376,#49377,#49378,
#49379,#49380,#49381,#49382,#49383,#49384,#49385,#49386,#49387,#49388,#49389,
#49390,#49391,#49392,#49393,#49394,#49395,#49396,#49397,#49398,#49399,#49400,
#49401,#49402,#49403,#49404,#49405,#49406,#49407,#49408,#49409,#49410,#49411,
#49412,#49413,#49414,#49415,#49416,#49417,#49418,#49419,#49420,#49421,#49422,
#49423,#49424,#49425,#49426,#49427,#49428,#49429,#49430,#49431,#49432,#49433,
#49434,#49435,#49436,#49437,#49438,#49439,#49440,#49441,#49442,#49443),
(#49444,#49445,#49446,#49447,#49448,#49449,#49450,#49451,#49452,#49453,
#49454,#49455,#49456,#49457,#49458,#49459,#49460,#49461,#49462,#49463,#49464,
#49465,#49466,#49467,#49468,#49469,#49470,#49471,#49472,#49473,#49474,#49475,
#49476,#49477,#49478,#49479,#49480,#49481,#49482,#49483,#49484,#49485,#49486,
#49487,#49488,#49489,#49490,#49491,#49492,#49493,#49494,#49495,#49496,#49497,
#49498,#49499,#49500,#49501,#49502,#49503,#49504,#49505,#49506,#49507,#49508,
#49509,#49510,#49511,#49512,#49513,#49514,#49515,#49516,#49517,#49518,#49519,
#49520,#49521,#49522,#49523,#49524,#49525,#49526,#49527,#49528,#49529,#49530,
#49531,#49532,#49533,#49534,#49535,#49536,#49537,#49538,#49539,#49540,#49541,
#49542,#49543,#49544,#49545,#49546,#49547,#49548,#49549,#49550,#49551,#49552,
#49553,#49554,#49555,#49556,#49557,#49558,#49559,#49560,#49561,#49562,#49563,
#49564,#49565,#49566,#49567,#49568,#49569,#49570,#49571,#49572,#49573,#49574,
#49575,#49576,#49577,#49578,#49579,#49580,#49581,#49582,#49583,#49584,#49585,
#49586,#49587,#49588,#49589,#49590,#49591,#49592,#49593,#49594,#49595,#49596,
#49597,#49598,#49599,#49600,#49601,#49602,#49603,#49604,#49605,#49606,#49607,
#49608,#49609,#49610,#49611,#49612,#49613,#49614,#49615,#49616)),
 .UNSPECIFIED.,.F.,.F.,.F.,(4,4),(4,1,1,1,1,1,1,1,1,1,1,1,1,1,1,1,1,1,1,
1,1,1,1,1,1,1,1,1,1,1,1,1,1,1,1,1,1,1,1,1,1,1,1,1,1,1,1,1,1,1,1,1,1,1,1,
1,1,1,1,1,1,1,1,1,1,1,1,1,1,1,1,1,1,1,1,1,1,1,1,1,1,1,1,1,1,1,1,1,1,1,1,
1,1,1,1,1,1,1,1,1,1,1,1,1,1,1,1,1,1,1,1,1,1,1,1,1,1,1,1,1,1,1,1,1,1,1,1,
1,1,1,1,1,1,1,1,1,1,1,1,1,1,1,1,1,1,1,1,1,1,1,1,1,1,1,1,1,1,1,1,1,1,1,1,
1,1,1,1,1,1,1,4),(-0.000231965532648874,0.0996290022117273),(8.29836425792185,
8.79750999747347,9.29636959945186,9.79522920143024,10.2940888034086,10.792948405387,
11.2918080073654,11.7906676093438,12.2895272113222,12.7883868133005,13.2872464152789,
13.7861060172573,14.2849656192357,14.7838252212141,15.2826848231925,15.7815444251708,
16.2804040271492,16.7792636291276,17.278123231106,17.7769828330844,18.2758424350628,
18.7747020370411,19.2735616390195,19.7724212409979,20.2712808429763,20.7701404449547,
21.2690000469331,21.7678596489115,22.2667192508898,22.7655788528682,23.2644384548466,
23.763298056825,24.2621576588034,24.7610172607818,25.2598768627601,25.7587364647385,
26.2575960667169,26.7564556686953,27.2553152706737,27.7541748726521,28.2530344746304,
28.7518940766088,29.2507536785872,29.7496132805656,30.248472882544,30.7473324845224,
31.2461920865007,31.7450516884791,32.2439112904575,32.7427708924359,33.2416304944143,
33.7404900963927,34.239349698371,34.7382093003494,35.2370689023278,35.7359285043062,
36.2347881062846,36.733647708263,37.2325073102413,37.7313669122197,38.2302265141981,
38.7290861161765,39.2279457181549,39.7268053201333,40.2256649221116,40.72452452409,
41.2233841260684,41.7222437280468,42.2211033300252,42.7199629320036,43.218822533982,
43.7176821359603,44.2165417379387,44.7154013399171,45.2142609418955,45.7131205438739,
46.2119801458523,46.7108397478306,47.209699349809,47.7085589517874,48.2074185537658,
48.7062781557442,49.2051377577226,49.7039973597009,50.2028569616793,50.7017165636577,
51.2005761656361,51.6994357676145,52.1982953695929,52.6971549715713,53.1960145735496,
53.694874175528,54.1937337775064,54.6925933794848,55.1914529814632,55.6903125834416,
56.1891721854199,56.6880317873983,57.1868913893767,57.6857509913551,58.1846105933335,
58.6834701953119,59.1823297972902,59.6811893992686,60.180049001247,60.6789086032254,
61.1777682052038,61.6766278071822,62.1754874091605,62.6743470111389,63.1732066131173,
63.6720662150957,64.1709258170741,64.6697854190525,65.1686450210308,65.6675046230092,
66.1663642249876,66.665223826966,67.1640834289444,67.6629430309227,68.1618026329011,
68.6606622348795,69.1595218368579,69.6583814388363,70.1572410408147,70.6561006427931,
71.1549602447714,71.6538198467498,72.1526794487282,72.6515390507066,73.150398652685,
73.6492582546634,74.1481178566417,74.6469774586201,75.1458370605985,75.6446966625769,
76.1435562645553,76.6424158665337,77.141275468512,77.6401350704904,78.1389946724688,
78.6378542744472,79.1367138764256,79.635573478404,80.1344330803824,80.6332926823607,
81.1321522843391,81.6310118863175,82.1298714882959,82.6287310902743,83.1275906922527,
83.626450294231,84.1253098962094,84.6241694981878,85.1230291001662,85.6218887021446,
86.120748304123,86.6196079061014,87.1184675080797,87.6173271100581,88.1161867120365,
88.6150463140149,89.1139059159933,89.6127655179716,90.11162511995,90.6104847219284,
91.1093443239068,91.6082039258852,92.1070635278636,92.605923129842,93.1050146973529),
 .UNSPECIFIED.) ;
#219 = B_SPLINE_SURFACE_WITH_KNOTS('',3,3,((#49897,#49898,#49899,#49900,#49901,
#49902,#49903,#49904,#49905,#49906,#49907,#49908,#49909,#49910,#49911,#49912,
#49913,#49914,#49915,#49916,#49917,#49918,#49919,#49920,#49921,#49922,#49923,
#49924,#49925,#49926,#49927,#49928,#49929,#49930,#49931,#49932,#49933,#49934,
#49935,#49936,#49937,#49938,#49939,#49940,#49941,#49942,#49943,#49944,#49945,
#49946,#49947,#49948,#49949,#49950,#49951,#49952,#49953,#49954,#49955,#49956,
#49957,#49958,#49959,#49960,#49961,#49962,#49963,#49964,#49965,#49966,#49967,
#49968,#49969,#49970,#49971,#49972,#49973,#49974,#49975,#49976,#49977,#49978,
#49979,#49980,#49981,#49982,#49983,#49984,#49985,#49986,#49987,#49988,#49989,
#49990,#49991,#49992,#49993,#49994,#49995,#49996,#49997,#49998,#49999,#50000,
#50001,#50002,#50003,#50004,#50005,#50006,#50007,#50008,#50009,#50010,#50011,
#50012,#50013,#50014,#50015,#50016,#50017,#50018,#50019,#50020,#50021,#50022,
#50023,#50024,#50025,#50026,#50027,#50028,#50029,#50030,#50031,#50032,#50033,
#50034,#50035,#50036,#50037,#50038,#50039,#50040,#50041,#50042,#50043,#50044,
#50045,#50046,#50047,#50048,#50049,#50050,#50051,#50052,#50053,#50054,#50055,
#50056,#50057,#50058,#50059,#50060,#50061,#50062,#50063,#50064,#50065,#50066,
#50067,#50068,#50069),(#50070,#50071,#50072,#50073,#50074,#50075,#50076,
#50077,#50078,#50079,#50080,#50081,#50082,#50083,#50084,#50085,#50086,#50087,
#50088,#50089,#50090,#50091,#50092,#50093,#50094,#50095,#50096,#50097,#50098,
#50099,#50100,#50101,#50102,#50103,#50104,#50105,#50106,#50107,#50108,#50109,
#50110,#50111,#50112,#50113,#50114,#50115,#50116,#50117,#50118,#50119,#50120,
#50121,#50122,#50123,#50124,#50125,#50126,#50127,#50128,#50129,#50130,#50131,
#50132,#50133,#50134,#50135,#50136,#50137,#50138,#50139,#50140,#50141,#50142,
#50143,#50144,#50145,#50146,#50147,#50148,#50149,#50150,#50151,#50152,#50153,
#50154,#50155,#50156,#50157,#50158,#50159,#50160,#50161,#50162,#50163,#50164,
#50165,#50166,#50167,#50168,#50169,#50170,#50171,#50172,#50173,#50174,#50175,
#50176,#50177,#50178,#50179,#50180,#50181,#50182,#50183,#50184,#50185,#50186,
#50187,#50188,#50189,#50190,#50191,#50192,#50193,#50194,#50195,#50196,#50197,
#50198,#50199,#50200,#50201,#50202,#50203,#50204,#50205,#50206,#50207,#50208,
#50209,#50210,#50211,#50212,#50213,#50214,#50215,#50216,#50217,#50218,#50219,
#50220,#50221,#50222,#50223,#50224,#50225,#50226,#50227,#50228,#50229,#50230,
#50231,#50232,#50233,#50234,#50235,#50236,#50237,#50238,#50239,#50240,#50241,
#50242),(#50243,#50244,#50245,#50246,#50247,#50248,#50249,#50250,#50251,
#50252,#50253,#50254,#50255,#50256,#50257,#50258,#50259,#50260,#50261,#50262,
#50263,#50264,#50265,#50266,#50267,#50268,#50269,#50270,#50271,#50272,#50273,
#50274,#50275,#50276,#50277,#50278,#50279,#50280,#50281,#50282,#50283,#50284,
#50285,#50286,#50287,#50288,#50289,#50290,#50291,#50292,#50293,#50294,#50295,
#50296,#50297,#50298,#50299,#50300,#50301,#50302,#50303,#50304,#50305,#50306,
#50307,#50308,#50309,#50310,#50311,#50312,#50313,#50314,#50315,#50316,#50317,
#50318,#50319,#50320,#50321,#50322,#50323,#50324,#50325,#50326,#50327,#50328,
#50329,#50330,#50331,#50332,#50333,#50334,#50335,#50336,#50337,#50338,#50339,
#50340,#50341,#50342,#50343,#50344,#50345,#50346,#50347,#50348,#50349,#50350,
#50351,#50352,#50353,#50354,#50355,#50356,#50357,#50358,#50359,#50360,#50361,
#50362,#50363,#50364,#50365,#50366,#50367,#50368,#50369,#50370,#50371,#50372,
#50373,#50374,#50375,#50376,#50377,#50378,#50379,#50380,#50381,#50382,#50383,
#50384,#50385,#50386,#50387,#50388,#50389,#50390,#50391,#50392,#50393,#50394,
#50395,#50396,#50397,#50398,#50399,#50400,#50401,#50402,#50403,#50404,#50405,
#50406,#50407,#50408,#50409,#50410,#50411,#50412,#50413,#50414,#50415),
(#50416,#50417,#50418,#50419,#50420,#50421,#50422,#50423,#50424,#50425,
#50426,#50427,#50428,#50429,#50430,#50431,#50432,#50433,#50434,#50435,#50436,
#50437,#50438,#50439,#50440,#50441,#50442,#50443,#50444,#50445,#50446,#50447,
#50448,#50449,#50450,#50451,#50452,#50453,#50454,#50455,#50456,#50457,#50458,
#50459,#50460,#50461,#50462,#50463,#50464,#50465,#50466,#50467,#50468,#50469,
#50470,#50471,#50472,#50473,#50474,#50475,#50476,#50477,#50478,#50479,#50480,
#50481,#50482,#50483,#50484,#50485,#50486,#50487,#50488,#50489,#50490,#50491,
#50492,#50493,#50494,#50495,#50496,#50497,#50498,#50499,#50500,#50501,#50502,
#50503,#50504,#50505,#50506,#50507,#50508,#50509,#50510,#50511,#50512,#50513,
#50514,#50515,#50516,#50517,#50518,#50519,#50520,#50521,#50522,#50523,#50524,
#50525,#50526,#50527,#50528,#50529,#50530,#50531,#50532,#50533,#50534,#50535,
#50536,#50537,#50538,#50539,#50540,#50541,#50542,#50543,#50544,#50545,#50546,
#50547,#50548,#50549,#50550,#50551,#50552,#50553,#50554,#50555,#50556,#50557,
#50558,#50559,#50560,#50561,#50562,#50563,#50564,#50565,#50566,#50567,#50568,
#50569,#50570,#50571,#50572,#50573,#50574,#50575,#50576,#50577,#50578,#50579,
#50580,#50581,#50582,#50583,#50584,#50585,#50586,#50587,#50588)),
 .UNSPECIFIED.,.F.,.F.,.F.,(4,4),(4,1,1,1,1,1,1,1,1,1,1,1,1,1,1,1,1,1,1,
1,1,1,1,1,1,1,1,1,1,1,1,1,1,1,1,1,1,1,1,1,1,1,1,1,1,1,1,1,1,1,1,1,1,1,1,
1,1,1,1,1,1,1,1,1,1,1,1,1,1,1,1,1,1,1,1,1,1,1,1,1,1,1,1,1,1,1,1,1,1,1,1,
1,1,1,1,1,1,1,1,1,1,1,1,1,1,1,1,1,1,1,1,1,1,1,1,1,1,1,1,1,1,1,1,1,1,1,1,
1,1,1,1,1,1,1,1,1,1,1,1,1,1,1,1,1,1,1,1,1,1,1,1,1,1,1,1,1,1,1,1,1,1,1,1,
1,1,1,1,1,1,1,4),(-0.000434450397776735,0.0994265044407978),(11.614740433148,
12.1138319898177,12.6126915917961,13.1115511937745,13.6104107957528,14.1092703977312,
14.6081299997096,15.106989601688,15.6058492036664,16.1047088056448,16.6035684076232,
17.1024280096015,17.6012876115799,18.1001472135583,18.5990068155367,19.0978664175151,
19.5967260194935,20.0955856214718,20.5944452234502,21.0933048254286,21.592164427407,
22.0910240293854,22.5898836313638,23.0887432333421,23.5876028353205,24.0864624372989,
24.5853220392773,25.0841816412557,25.5830412432341,26.0819008452124,26.5807604471908,
27.0796200491692,27.5784796511476,28.077339253126,28.5761988551044,29.0750584570828,
29.5739180590611,30.0727776610395,30.5716372630179,31.0704968649963,31.5693564669747,
32.0682160689531,32.5670756709314,33.0659352729098,33.5647948748882,34.0636544768666,
34.562514078845,35.0613736808234,35.5602332828017,36.0590928847801,36.5579524867585,
37.0568120887369,37.5556716907153,38.0545312926937,38.553390894672,39.0522504966504,
39.5511100986288,40.0499697006072,40.5488293025856,41.047688904564,41.5465485065424,
42.0454081085207,42.5442677104991,43.0431273124775,43.5419869144559,44.0408465164343,
44.5397061184127,45.038565720391,45.5374253223694,46.0362849243478,46.5351445263262,
47.0340041283046,47.532863730283,48.0317233322614,48.5305829342397,49.0294425362181,
49.5283021381965,50.0271617401749,50.5260213421533,51.0248809441317,51.52374054611,
52.0226001480884,52.5214597500668,53.0203193520452,53.5191789540236,54.018038556002,
54.5168981579803,55.0157577599587,55.5146173619371,56.0134769639155,56.5123365658939,
57.0111961678723,57.5100557698507,58.008915371829,58.5077749738074,59.0066345757858,
59.5054941777642,60.0043537797426,60.503213381721,61.0020729836993,61.5009325856777,
61.9997921876561,62.4986517896345,62.9975113916129,63.4963709935913,63.9952305955696,
64.494090197548,64.9929497995264,65.4918094015048,65.9906690034832,66.4895286054616,
66.98838820744,67.4872478094183,67.9861074113967,68.4849670133751,68.9838266153535,
69.4826862173319,69.9815458193102,70.4804054212886,70.979265023267,71.4781246252454,
71.9769842272238,72.4758438292022,72.9747034311806,73.4735630331589,73.9724226351373,
74.4712822371157,74.9701418390941,75.4690014410725,75.9678610430509,76.4667206450292,
76.9655802470076,77.464439848986,77.9632994509644,78.4621590529428,78.9610186549212,
79.4598782568995,79.9587378588779,80.4575974608563,80.9564570628347,81.4553166648131,
81.9541762667915,82.4530358687698,82.9518954707482,83.4507550727266,83.949614674705,
84.4484742766834,84.9473338786618,85.4461934806401,85.9450530826185,86.4439126845969,
86.9427722865753,87.4416318885537,87.9404914905321,88.4393510925105,88.9382106944888,
89.4370702964672,89.9359298984456,90.434789500424,90.9336491024024,91.4325087043808,
91.9313683063591,92.4302279083375,92.9290875103159,93.4279471122943,93.9268067142727,
94.4256663162511,94.9245259182294,95.4233855202078,95.9222451221862,96.421393347443),
 .UNSPECIFIED.) ;
#220 = B_SPLINE_SURFACE_WITH_KNOTS('',3,3,((#50861,#50862,#50863,#50864,#50865,
#50866,#50867,#50868,#50869,#50870,#50871,#50872,#50873,#50874,#50875,#50876,
#50877,#50878,#50879,#50880,#50881,#50882,#50883,#50884,#50885,#50886,#50887,
#50888,#50889,#50890,#50891,#50892,#50893,#50894,#50895,#50896,#50897,#50898,
#50899,#50900,#50901,#50902,#50903,#50904,#50905,#50906,#50907,#50908,#50909,
#50910,#50911,#50912,#50913,#50914,#50915,#50916,#50917,#50918,#50919,#50920,
#50921,#50922,#50923,#50924,#50925,#50926,#50927,#50928,#50929,#50930,#50931,
#50932,#50933,#50934,#50935,#50936,#50937,#50938,#50939,#50940,#50941,#50942,
#50943,#50944,#50945,#50946,#50947),(#50948,#50949,#50950,#50951,#50952,
#50953,#50954,#50955,#50956,#50957,#50958,#50959,#50960,#50961,#50962,#50963,
#50964,#50965,#50966,#50967,#50968,#50969,#50970,#50971,#50972,#50973,#50974,
#50975,#50976,#50977,#50978,#50979,#50980,#50981,#50982,#50983,#50984,#50985,
#50986,#50987,#50988,#50989,#50990,#50991,#50992,#50993,#50994,#50995,#50996,
#50997,#50998,#50999,#51000,#51001,#51002,#51003,#51004,#51005,#51006,#51007,
#51008,#51009,#51010,#51011,#51012,#51013,#51014,#51015,#51016,#51017,#51018,
#51019,#51020,#51021,#51022,#51023,#51024,#51025,#51026,#51027,#51028,#51029,
#51030,#51031,#51032,#51033,#51034),(#51035,#51036,#51037,#51038,#51039,
#51040,#51041,#51042,#51043,#51044,#51045,#51046,#51047,#51048,#51049,#51050,
#51051,#51052,#51053,#51054,#51055,#51056,#51057,#51058,#51059,#51060,#51061,
#51062,#51063,#51064,#51065,#51066,#51067,#51068,#51069,#51070,#51071,#51072,
#51073,#51074,#51075,#51076,#51077,#51078,#51079,#51080,#51081,#51082,#51083,
#51084,#51085,#51086,#51087,#51088,#51089,#51090,#51091,#51092,#51093,#51094,
#51095,#51096,#51097,#51098,#51099,#51100,#51101,#51102,#51103,#51104,#51105,
#51106,#51107,#51108,#51109,#51110,#51111,#51112,#51113,#51114,#51115,#51116,
#51117,#51118,#51119,#51120,#51121),(#51122,#51123,#51124,#51125,#51126,
#51127,#51128,#51129,#51130,#51131,#51132,#51133,#51134,#51135,#51136,#51137,
#51138,#51139,#51140,#51141,#51142,#51143,#51144,#51145,#51146,#51147,#51148,
#51149,#51150,#51151,#51152,#51153,#51154,#51155,#51156,#51157,#51158,#51159,
#51160,#51161,#51162,#51163,#51164,#51165,#51166,#51167,#51168,#51169,#51170,
#51171,#51172,#51173,#51174,#51175,#51176,#51177,#51178,#51179,#51180,#51181,
#51182,#51183,#51184,#51185,#51186,#51187,#51188,#51189,#51190,#51191,#51192,
#51193,#51194,#51195,#51196,#51197,#51198,#51199,#51200,#51201,#51202,#51203,
#51204,#51205,#51206,#51207,#51208)),.UNSPECIFIED.,.F.,.F.,.F.,(4,4),(4,
1,1,1,1,1,1,1,1,1,1,1,1,1,1,1,1,1,1,1,1,1,1,1,1,1,1,1,1,1,1,1,1,1,1,1,1,
1,1,1,1,1,1,1,1,1,1,1,1,1,1,1,1,1,1,1,1,1,1,1,1,1,1,1,1,1,1,1,1,1,1,1,1,
1,1,1,1,1,1,1,1,1,1,1,4),(-0.000240669354260341,0.207692603139416),(8.31441726003343,
8.81032130755511,9.30590986525221,9.8014984229493,10.2970869806464,10.7926755383435,
11.2882640960406,11.7838526537377,12.2794412114348,12.7750297691319,13.270618326829,
13.7662068845261,14.2617954422232,14.7573839999203,15.2529725576174,15.7485611153145,
16.2441496730116,16.7397382307087,17.2353267884057,17.7309153461028,18.2265039037999,
18.722092461497,19.2176810191941,19.7132695768912,20.2088581345883,20.7044466922854,
21.2000352499825,21.6956238076796,22.1912123653767,22.6868009230738,23.1823894807709,
23.677978038468,24.1735665961651,24.6691551538622,25.1647437115593,25.6603322692564,
26.1559208269535,26.6515093846506,27.1470979423477,27.6426865000448,28.1382750577419,
28.633863615439,29.1294521731361,29.6250407308331,30.1206292885302,30.6162178462273,
31.1118064039244,31.6073949616215,32.1029835193186,32.5985720770157,33.0941606347128,
33.5897491924099,34.085337750107,34.5809263078041,35.0765148655012,35.5721034231983,
36.0676919808954,36.5632805385925,37.0588690962896,37.5544576539867,38.0500462116838,
38.5456347693809,39.041223327078,39.5368118847751,40.0324004424722,40.5279890001693,
41.0235775578664,41.5191661155635,42.0147546732606,42.5103432309577,43.0059317886547,
43.5015203463518,43.9971089040489,44.492697461746,44.9882860194431,45.4838745771402,
45.9794631348373,46.4750516925344,46.9706402502315,47.4662288079286,47.9618173656257,
48.4574059233228,48.9529944810199,49.448583038717,49.9444122657684),
 .UNSPECIFIED.) ;
#221 = B_SPLINE_SURFACE_WITH_KNOTS('',3,3,((#51336,#51337,#51338,#51339,#51340,
#51341,#51342,#51343,#51344,#51345,#51346,#51347,#51348,#51349,#51350,#51351,
#51352,#51353,#51354,#51355,#51356,#51357,#51358,#51359,#51360,#51361,#51362,
#51363,#51364,#51365,#51366,#51367,#51368,#51369,#51370,#51371,#51372,#51373,
#51374,#51375,#51376,#51377,#51378,#51379,#51380,#51381,#51382,#51383,#51384,
#51385,#51386,#51387,#51388,#51389,#51390,#51391,#51392,#51393,#51394,#51395,
#51396,#51397,#51398,#51399,#51400,#51401,#51402,#51403,#51404,#51405,#51406,
#51407,#51408,#51409,#51410,#51411,#51412,#51413,#51414,#51415,#51416,#51417,
#51418,#51419,#51420,#51421,#51422),(#51423,#51424,#51425,#51426,#51427,
#51428,#51429,#51430,#51431,#51432,#51433,#51434,#51435,#51436,#51437,#51438,
#51439,#51440,#51441,#51442,#51443,#51444,#51445,#51446,#51447,#51448,#51449,
#51450,#51451,#51452,#51453,#51454,#51455,#51456,#51457,#51458,#51459,#51460,
#51461,#51462,#51463,#51464,#51465,#51466,#51467,#51468,#51469,#51470,#51471,
#51472,#51473,#51474,#51475,#51476,#51477,#51478,#51479,#51480,#51481,#51482,
#51483,#51484,#51485,#51486,#51487,#51488,#51489,#51490,#51491,#51492,#51493,
#51494,#51495,#51496,#51497,#51498,#51499,#51500,#51501,#51502,#51503,#51504,
#51505,#51506,#51507,#51508,#51509),(#51510,#51511,#51512,#51513,#51514,
#51515,#51516,#51517,#51518,#51519,#51520,#51521,#51522,#51523,#51524,#51525,
#51526,#51527,#51528,#51529,#51530,#51531,#51532,#51533,#51534,#51535,#51536,
#51537,#51538,#51539,#51540,#51541,#51542,#51543,#51544,#51545,#51546,#51547,
#51548,#51549,#51550,#51551,#51552,#51553,#51554,#51555,#51556,#51557,#51558,
#51559,#51560,#51561,#51562,#51563,#51564,#51565,#51566,#51567,#51568,#51569,
#51570,#51571,#51572,#51573,#51574,#51575,#51576,#51577,#51578,#51579,#51580,
#51581,#51582,#51583,#51584,#51585,#51586,#51587,#51588,#51589,#51590,#51591,
#51592,#51593,#51594,#51595,#51596),(#51597,#51598,#51599,#51600,#51601,
#51602,#51603,#51604,#51605,#51606,#51607,#51608,#51609,#51610,#51611,#51612,
#51613,#51614,#51615,#51616,#51617,#51618,#51619,#51620,#51621,#51622,#51623,
#51624,#51625,#51626,#51627,#51628,#51629,#51630,#51631,#51632,#51633,#51634,
#51635,#51636,#51637,#51638,#51639,#51640,#51641,#51642,#51643,#51644,#51645,
#51646,#51647,#51648,#51649,#51650,#51651,#51652,#51653,#51654,#51655,#51656,
#51657,#51658,#51659,#51660,#51661,#51662,#51663,#51664,#51665,#51666,#51667,
#51668,#51669,#51670,#51671,#51672,#51673,#51674,#51675,#51676,#51677,#51678,
#51679,#51680,#51681,#51682,#51683)),.UNSPECIFIED.,.F.,.F.,.F.,(4,4),(4,
1,1,1,1,1,1,1,1,1,1,1,1,1,1,1,1,1,1,1,1,1,1,1,1,1,1,1,1,1,1,1,1,1,1,1,1,
1,1,1,1,1,1,1,1,1,1,1,1,1,1,1,1,1,1,1,1,1,1,1,1,1,1,1,1,1,1,1,1,1,1,1,1,
1,1,1,1,1,1,1,1,1,1,1,4),(-0.000480856812830276,0.207452754717094),(11.6258564355357,
12.1216855816372,12.6172741393343,13.1128626970314,13.6084512547285,14.1040398124256,
14.5996283701227,15.0952169278198,15.5908054855169,16.086394043214,16.5819826009111,
17.0775711586082,17.5731597163053,18.0687482740024,18.5643368316995,19.0599253893966,
19.5555139470937,20.0511025047908,20.5466910624879,21.042279620185,21.5378681778821,
22.0334567355792,22.5290452932763,23.0246338509733,23.5202224086704,24.0158109663675,
24.5113995240646,25.0069880817617,25.5025766394588,25.9981651971559,26.493753754853,
26.9893423125501,27.4849308702472,27.9805194279443,28.4761079856414,28.9716965433385,
29.4672851010356,29.9628736587327,30.4584622164298,30.9540507741269,31.449639331824,
31.9452278895211,32.4408164472182,32.9364050049153,33.4319935626124,33.9275821203095,
34.4231706780066,34.9187592357037,35.4143477934008,35.9099363510978,36.4055249087949,
36.901113466492,37.3967020241891,37.8922905818862,38.3878791395833,38.8834676972804,
39.3790562549775,39.8746448126746,40.3702333703717,40.8658219280688,41.3614104857659,
41.856999043463,42.3525876011601,42.8481761588572,43.3437647165543,43.8393532742514,
44.3349418319485,44.8305303896456,45.3261189473427,45.8217075050398,46.3172960627369,
46.812884620434,47.3084731781311,47.8040617358281,48.2996502935252,48.7952388512223,
49.2908274089194,49.7864159666165,50.2820045243136,50.7775930820107,51.2731816397078,
51.7687701974049,52.264358755102,52.7599473127991,53.2558559415817),
 .UNSPECIFIED.) ;
#222 = B_SPLINE_CURVE_WITH_KNOTS('',3,(#23804,#23805,#23806,#23807,#23808,
#23809,#23810,#23811,#23812,#23813,#23814,#23815,#23816,#23817,#23818,#23819,
#23820,#23821,#23822,#23823,#23824,#23825,#23826,#23827,#23828,#23829,#23830,
#23831,#23832,#23833,#23834,#23835,#23836,#23837,#23838,#23839,#23840,#23841,
#23842,#23843,#23844,#23845,#23846,#23847,#23848,#23849,#23850,#23851,#23852,
#23853,#23854,#23855,#23856,#23857,#23858,#23859,#23860,#23861,#23862,#23863,
#23864,#23865,#23866,#23867,#23868,#23869,#23870,#23871,#23872,#23873,#23874,
#23875,#23876,#23877,#23878,#23879,#23880,#23881,#23882,#23883,#23884,#23885,
#23886,#23887,#23888,#23889,#23890,#23891,#23892,#23893,#23894,#23895,#23896,
#23897,#23898,#23899,#23900,#23901,#23902,#23903,#23904,#23905,#23906,#23907,
#23908,#23909,#23910,#23911,#23912,#23913,#23914,#23915,#23916,#23917,#23918,
#23919,#23920,#23921,#23922,#23923,#23924,#23925,#23926,#23927,#23928,#23929,
#23930,#23931,#23932,#23933,#23934,#23935),.UNSPECIFIED.,.F.,.F.,(4,2,2,
2,2,2,2,2,2,2,2,2,2,2,2,2,2,2,2,2,2,2,2,2,2,2,2,2,2,2,2,2,2,2,2,2,2,2,2,
2,2,2,2,2,2,2,2,2,2,2,2,2,2,2,2,2,2,2,2,2,2,2,2,2,2,4),(-16.1229693507328,
-15.9135799066995,-15.8630188232808,-15.8258339769541,-15.7900643273633,
-15.7493447314678,-15.6804351503378,-15.4438875959545,-15.382716929369,
-15.3511867583258,-15.3490515343236,-15.3474738962906,-15.3462861030307,
-15.3453772206255,-15.3446721805859,-15.3422209639646,-15.3399838267774,
-15.3379087228275,-15.335949913756,-15.3340653838625,-15.3322140707189,
-15.312299721018,-15.2933483093209,-15.2575988936463,-15.1101303960858,
-14.9770661832259,-14.9147347649729,-14.8645510943747,-14.8321428783299,
-14.7941984330884,-14.7474930119732,-14.5824427622385,-14.4236499865968,
-14.3733286233332,-14.3496260871508,-14.3296916779127,-14.3001338022836,
-14.205790025479,-14.1493019577269,-14.0104112561113,-13.9672600709325,
-13.902906436049,-13.8630630143224,-13.8252061120945,-13.7790024342338,
-13.6144737469252,-13.4558833048607,-13.4046920450664,-13.3808187973035,
-13.360892241764,-13.3315240504932,-13.239398973681,-13.112513364983,-12.9674714651803,
-12.9174417478242,-12.8799279430778,-12.838125864583,-12.7648688910664,
-12.7000821654783,-12.5248339492791,-12.4451057288507,-12.4174885325345,
-12.399593032763,-12.3756627482975,-12.3240898597893,-12.2072680143011),
 .UNSPECIFIED.) ;
#223 = B_SPLINE_CURVE_WITH_KNOTS('',3,(#23938,#23939,#23940,#23941,#23942,
#23943,#23944,#23945,#23946,#23947,#23948,#23949,#23950,#23951,#23952,#23953,
#23954,#23955,#23956,#23957,#23958,#23959,#23960,#23961,#23962,#23963,#23964,
#23965,#23966,#23967,#23968,#23969,#23970,#23971,#23972,#23973,#23974,#23975,
#23976,#23977,#23978,#23979,#23980,#23981,#23982,#23983,#23984,#23985,#23986,
#23987,#23988,#23989,#23990,#23991,#23992,#23993,#23994,#23995,#23996,#23997,
#23998,#23999,#24000,#24001,#24002,#24003,#24004,#24005,#24006,#24007,#24008,
#24009),.UNSPECIFIED.,.F.,.F.,(4,2,2,2,2,2,2,2,2,2,2,2,2,2,2,2,2,2,2,2,
2,2,2,2,2,2,2,2,2,2,2,2,2,2,2,4),(0.000310445151374366,0.0115408935467113,
0.0246665289368376,0.0621056912317256,0.260884109848728,0.378907191384278,
0.417457177688961,0.45359225385393,0.489222506445489,0.54948956411632,0.725511782450542,
0.865407477841949,0.915570228192533,0.936508372302185,0.957197100440422,
0.975194107826528,0.99626310266181,1.0317648914341,1.16397106478206,1.30320971966519,
1.36670318110169,1.40294750827005,1.41439432286191,1.44931608805952,1.48713481040049,
1.5418368243862,1.75235977753755,1.88243028398069,1.91902241857432,1.94008923532906,
1.9615202035756,1.99897338198793,2.08917556360275,2.10566915491795,2.13232522116834,
2.18817716271853),.UNSPECIFIED.) ;
#224 = B_SPLINE_CURVE_WITH_KNOTS('',3,(#24014,#24015,#24016,#24017,#24018,
#24019,#24020,#24021,#24022,#24023,#24024,#24025,#24026,#24027,#24028,#24029,
#24030,#24031,#24032,#24033,#24034,#24035,#24036,#24037,#24038,#24039,#24040,
#24041,#24042,#24043,#24044,#24045,#24046,#24047,#24048,#24049,#24050,#24051,
#24052,#24053,#24054,#24055,#24056,#24057,#24058,#24059,#24060,#24061,#24062,
#24063,#24064,#24065,#24066,#24067,#24068,#24069,#24070,#24071,#24072,#24073,
#24074,#24075,#24076,#24077,#24078,#24079,#24080,#24081,#24082,#24083,#24084,
#24085,#24086,#24087,#24088,#24089,#24090,#24091,#24092,#24093,#24094,#24095,
#24096,#24097,#24098,#24099,#24100,#24101,#24102,#24103,#24104,#24105,#24106,
#24107,#24108,#24109,#24110,#24111,#24112,#24113,#24114,#24115,#24116,#24117,
#24118,#24119,#24120,#24121,#24122,#24123,#24124,#24125,#24126,#24127,#24128,
#24129,#24130,#24131,#24132,#24133,#24134,#24135,#24136,#24137,#24138,#24139,
#24140,#24141,#24142,#24143,#24144,#24145,#24146,#24147,#24148,#24149,#24150,
#24151,#24152,#24153,#24154,#24155,#24156,#24157,#24158,#24159,#24160,#24161,
#24162,#24163,#24164,#24165,#24166,#24167,#24168,#24169,#24170,#24171,#24172,
#24173,#24174,#24175,#24176,#24177,#24178,#24179,#24180,#24181,#24182,#24183,
#24184,#24185,#24186,#24187,#24188,#24189,#24190,#24191,#24192,#24193,#24194,
#24195,#24196,#24197,#24198,#24199,#24200,#24201,#24202,#24203,#24204,#24205,
#24206,#24207,#24208,#24209,#24210,#24211,#24212,#24213,#24214,#24215,#24216,
#24217,#24218,#24219,#24220,#24221,#24222,#24223,#24224,#24225,#24226,#24227,
#24228,#24229,#24230,#24231,#24232,#24233,#24234,#24235,#24236,#24237,#24238,
#24239,#24240,#24241,#24242,#24243,#24244,#24245,#24246,#24247,#24248,#24249,
#24250,#24251,#24252,#24253,#24254,#24255,#24256,#24257,#24258,#24259,#24260,
#24261,#24262,#24263,#24264,#24265,#24266,#24267,#24268,#24269,#24270,#24271,
#24272,#24273,#24274,#24275,#24276,#24277,#24278,#24279,#24280,#24281,#24282,
#24283,#24284,#24285,#24286,#24287,#24288,#24289,#24290,#24291,#24292,#24293,
#24294,#24295,#24296,#24297,#24298,#24299,#24300,#24301,#24302,#24303,#24304,
#24305,#24306,#24307,#24308,#24309,#24310,#24311,#24312,#24313,#24314,#24315,
#24316,#24317,#24318,#24319,#24320,#24321,#24322,#24323,#24324,#24325,#24326,
#24327,#24328,#24329,#24330,#24331,#24332,#24333,#24334,#24335,#24336,#24337,
#24338,#24339,#24340,#24341,#24342,#24343,#24344,#24345,#24346,#24347,#24348,
#24349,#24350,#24351,#24352,#24353,#24354,#24355),.UNSPECIFIED.,.F.,.F.,
(4,2,2,2,2,2,2,2,2,2,2,2,2,2,2,2,2,2,2,2,2,2,2,2,2,2,2,2,2,2,2,2,2,2,2,
2,2,2,2,2,2,2,2,2,2,2,2,2,2,2,2,2,2,2,2,2,2,2,2,2,2,2,2,2,2,2,2,2,2,2,2,
2,2,2,2,2,2,2,2,2,2,2,2,2,2,2,2,2,2,2,2,2,2,2,2,2,2,2,2,2,2,2,2,2,2,2,2,
2,2,2,2,2,2,2,2,2,2,2,2,2,2,2,2,2,2,2,2,2,2,2,2,2,2,2,2,2,2,2,2,2,2,2,2,
2,2,2,2,2,2,2,2,2,2,2,2,2,2,2,2,2,2,2,2,2,2,2,2,2,2,2,4),(-12.2072680143011,
-12.1214316325864,-12.0348137295484,-11.9673727988363,-11.9269792152918,
-11.8889951798646,-11.8354617297945,-11.615155934698,-11.4926371450886,
-11.4567462368015,-11.4357130176028,-11.4169088168123,-11.3819692573798,
-11.2753908522613,-11.0659613648654,-10.9982933482017,-10.9578545775686,
-10.919881999828,-10.866456417054,-10.7484568701481,-10.5837678213848,-10.5450462648772,
-10.4960146050613,-10.4725095334352,-10.4524974952048,-10.4224502327544,
-10.3093369784509,-10.2224431927978,-10.1144447738829,-10.0365217618984,
-9.99428594351171,-9.95687012854156,-9.90853845623905,-9.7794505566006,
-9.61462525448062,-9.57588749294409,-9.52684296406612,-9.50333752228509,
-9.48332735686028,-9.45328875884435,-9.34062140172601,-9.21399657064198,
-9.12730295634282,-9.05982032737858,-9.01941609794039,-8.98143018783511,
-8.93636895026983,-8.80735611467015,-8.64484772170618,-8.60637781831352,
-8.55756026874535,-8.53409283329303,-8.51407078986009,-8.48395034743693,
-8.37518456547857,-8.34399557902459,-8.19873504568114,-8.10613967829615,
-8.06157709065096,-8.02810934960208,-7.98401608757255,-7.89456466392264,
-7.7582671599074,-7.61585865112676,-7.58000855002441,-7.56104370400703,
-7.5401903997776,-7.50523201263521,-7.26025892497224,-7.14755908688535,
-7.09984468888507,-7.06249093535267,-7.01988569946944,-6.93977085594752,
-6.69088410769133,-6.62674460165974,-6.60070971340099,-6.58101006716034,
-6.55508595815767,-6.49001828517347,-6.37409284031265,-6.31557441951567,
-6.18244765878282,-6.13318015851525,-6.09565470845379,-6.05391590447638,
-5.97889669698792,-5.8771619883261,-5.67448067858958,-5.64019149258949,
-5.62150014994861,-5.60031687680764,-5.56367573660035,-5.43426584477831,
-5.22452145485842,-5.16997775976138,-5.13221214200042,-5.0922198482054,
-5.02702365776805,-4.9830435683078,-4.83945447753678,-4.70766533110664,
-4.67208618909627,-4.65316940855279,-4.63226428501289,-4.59703789099837,
-4.42032405949409,-4.34154390172734,-4.23761631495814,-4.19022786076316,
-4.15296687672001,-4.10961863244128,-4.02495046492125,-3.82755257418756,
-3.7266387684387,-3.6970509612286,-3.67710061387468,-3.65336156746934,-3.60294539519532,
-3.44449865278867,-3.27845839873617,-3.23226040626606,-3.19440753104968,
-3.15456903235772,-3.09022638220154,-3.0470830704392,-2.90822062929407,
-2.84901726335752,-2.75694936493455,-2.72759521858757,-2.70767440564304,
-2.68380864659361,-2.63263287327469,-2.47402511406729,-2.30942096653791,
-2.26316889515377,-2.2253042136077,-2.18548599498706,-2.12125537850627,
-2.07822126784755,-1.93996303018653,-1.88739961108352,-1.78860071682233,
-1.75885926938661,-1.73888901059928,-1.71523115206963,-1.66529595529032,
-1.62550000660333,-1.45109008988929,-1.33257085340842,-1.2847708639072,
-1.2474088803859,-1.23704712794801,-1.23271077082133,-1.22810693380001,
-1.18084215915745,-1.12292612799538,-1.00764929421452,-0.825471155663644,
-0.792760620363109,-0.774333300655851,-0.759230550740772,-0.73650450015082,
-0.6598266807045,-0.49922070704633,-0.366888604665163,-0.317766506712928,
-0.280259080447408,-0.245357825619976,-0.203857388925526,-4.21440357605785E-5),
 .UNSPECIFIED.) ;
#225 = B_SPLINE_CURVE_WITH_KNOTS('',3,(#24356,#24357,#24358,#24359,#24360,
#24361,#24362,#24363,#24364,#24365,#24366,#24367,#24368,#24369,#24370,#24371,
#24372,#24373,#24374,#24375,#24376,#24377,#24378,#24379,#24380,#24381,#24382,
#24383,#24384,#24385,#24386,#24387,#24388,#24389,#24390,#24391,#24392,#24393,
#24394,#24395,#24396,#24397,#24398,#24399,#24400,#24401,#24402,#24403,#24404,
#24405,#24406,#24407,#24408,#24409,#24410,#24411,#24412,#24413,#24414,#24415,
#24416,#24417,#24418,#24419,#24420,#24421,#24422,#24423,#24424,#24425,#24426,
#24427,#24428,#24429,#24430,#24431,#24432,#24433,#24434,#24435,#24436,#24437,
#24438,#24439,#24440,#24441,#24442,#24443,#24444,#24445,#24446,#24447,#24448,
#24449,#24450,#24451,#24452,#24453,#24454,#24455,#24456,#24457,#24458,#24459,
#24460,#24461,#24462,#24463,#24464,#24465,#24466,#24467,#24468,#24469,#24470,
#24471,#24472,#24473,#24474,#24475,#24476,#24477,#24478,#24479,#24480,#24481,
#24482,#24483,#24484,#24485,#24486,#24487,#24488,#24489,#24490,#24491,#24492,
#24493,#24494,#24495,#24496,#24497,#24498,#24499,#24500,#24501,#24502,#24503,
#24504,#24505,#24506,#24507,#24508,#24509,#24510,#24511,#24512,#24513,#24514,
#24515,#24516,#24517,#24518,#24519,#24520,#24521,#24522,#24523,#24524,#24525,
#24526,#24527,#24528,#24529,#24530,#24531,#24532,#24533,#24534,#24535,#24536,
#24537,#24538,#24539,#24540,#24541,#24542,#24543,#24544,#24545,#24546,#24547,
#24548,#24549,#24550,#24551,#24552,#24553,#24554,#24555,#24556,#24557,#24558,
#24559,#24560,#24561,#24562,#24563,#24564,#24565,#24566,#24567,#24568,#24569,
#24570,#24571,#24572,#24573,#24574,#24575,#24576,#24577,#24578,#24579,#24580,
#24581,#24582,#24583,#24584,#24585,#24586,#24587,#24588,#24589,#24590,#24591,
#24592,#24593,#24594,#24595,#24596,#24597,#24598,#24599,#24600,#24601,#24602,
#24603,#24604,#24605,#24606,#24607,#24608,#24609,#24610,#24611,#24612,#24613,
#24614,#24615,#24616,#24617,#24618,#24619,#24620,#24621,#24622,#24623,#24624,
#24625,#24626,#24627,#24628,#24629,#24630,#24631,#24632,#24633,#24634,#24635,
#24636,#24637,#24638,#24639,#24640,#24641,#24642,#24643,#24644,#24645,#24646,
#24647,#24648,#24649,#24650,#24651,#24652,#24653,#24654,#24655,#24656,#24657,
#24658,#24659,#24660,#24661,#24662,#24663,#24664,#24665,#24666,#24667,#24668,
#24669,#24670,#24671,#24672,#24673,#24674,#24675,#24676,#24677,#24678,#24679,
#24680,#24681,#24682,#24683,#24684,#24685,#24686,#24687,#24688,#24689,#24690,
#24691,#24692,#24693,#24694,#24695,#24696,#24697,#24698,#24699,#24700,#24701,
#24702,#24703,#24704,#24705,#24706,#24707),.UNSPECIFIED.,.F.,.F.,(4,2,2,
2,2,2,2,2,2,2,2,2,2,2,2,2,2,2,2,2,2,2,2,2,2,2,2,2,2,2,2,2,2,2,2,2,2,2,2,
2,2,2,2,2,2,2,2,2,2,2,2,2,2,2,2,2,2,2,2,2,2,2,2,2,2,2,2,2,2,2,2,2,2,2,2,
2,2,2,2,2,2,2,2,2,2,2,2,2,2,2,2,2,2,2,2,2,2,2,2,2,2,2,2,2,2,2,2,2,2,2,2,
2,2,2,2,2,2,2,2,2,2,2,2,2,2,2,2,2,2,2,2,2,2,2,2,2,2,2,2,2,2,2,2,2,2,2,2,
2,2,2,2,2,2,2,2,2,2,2,2,2,2,2,2,2,2,2,2,2,2,2,2,2,2,2,2,4),(2.18817716271853,
2.27258985578313,2.31604363060642,2.38083993956034,2.42101112656157,2.45925672133389,
2.50608966252046,2.67030192185054,2.80070882856306,2.84896253681468,2.88582472444221,
2.90720085914843,2.92594015309928,2.96052122729631,3.13558019513664,3.29691169508635,
3.35412793258946,3.39256123443125,3.42709759077454,3.48388809280466,3.63441718908193,
3.76995307059931,3.84067309963547,3.86719537629394,3.88681756102699,3.9120457363662,
3.96990045621053,4.22743789373958,4.30759701363214,4.35027338084236,4.38772330967091,
4.43562518983659,4.5500003783448,4.72657464056413,4.7665750812795,4.81670405179479,
4.84044726256082,4.86045284261538,4.89026606925306,4.98883636689778,5.18495913352847,
5.2462668736371,5.29914506260869,5.33701066629752,5.37757909946605,5.44608794428359,
5.68485825800973,5.74625569619831,5.78987912174619,5.81239607270393,5.83250681328118,
5.86453556595654,6.0535504441511,6.1656218068973,6.24536847052205,6.28791548716059,
6.32528363131567,6.37310775308717,6.49117238849288,6.66574065634653,6.70554889136079,
6.75549574276886,6.77916055802478,6.79913681140632,6.82889398711347,6.92755915224754,
6.9646146930374,7.07893349649339,7.19783297962598,7.24568051399259,7.28297798784249,
7.32602002229107,7.40877437224083,7.61642909110148,7.71021325152551,7.73974802479294,
7.75969129539594,7.78345667537042,7.83403679037394,7.99229976566751,8.15831221921274,
8.20449621568462,8.24234309080218,8.28218038007358,8.34653217890775,8.38968559157436,
8.52860532650486,8.58521464561437,8.679350844392,8.70891274535028,8.72885850696504,
8.75260920747026,8.80309335979099,8.96146589839134,9.12751138397173,9.17369993230231,
9.21155217066301,9.25139742988831,9.31577013706904,9.35894245804052,9.49796962270571,
9.54934695754393,9.64811878745205,9.67786314318781,9.69783460214745,9.72149243353714,
9.77142886870925,9.81122661178085,9.98565408529672,10.1041854649933,10.1519711614567,
10.189330449529,10.2318884386356,10.3117264710507,10.4240185480195,10.612574726657,
10.644619733548,10.6647404808281,10.6872974545491,10.7310286658147,10.7637600340689,
10.8843189994301,10.9390691633499,11.0698512951672,11.1189664111175,11.1564731071566,
11.1982887945662,11.273753523903,11.3764315412984,11.5759792595209,11.6110296504896,
11.6298532425524,11.6508654825314,11.6866422059215,11.8081309959872,12.030510862482,
12.0836747704508,12.1216061472386,12.1621272563688,12.2302642106318,12.2771873613173,
12.4389310397248,12.5454060943917,12.5803373501216,12.599139745995,12.6201769173334,
12.6560810550213,12.7787069726977,12.9987615041652,13.0523392943701,13.0903327787884,
13.125102134132,13.179271971074,13.2485400062385,13.4155621854189,13.5241216925213,
13.5542315609061,13.573930635645,13.5888938238053,13.5907128182226,13.5925919389256,
13.5945711446099,13.5966932123652,13.5990062508306,13.6015661956319,13.602590316265,
13.6039528520496,13.6336689090568,13.6892734768506,13.8691088931611,13.9813352653587,
14.0289878310402,14.0663352143452,14.1013385267474,14.143671946755,14.3953830185734),
 .UNSPECIFIED.) ;
#226 = B_SPLINE_CURVE_WITH_KNOTS('',3,(#24712,#24713,#24714,#24715,#24716,
#24717,#24718,#24719,#24720,#24721,#24722,#24723,#24724,#24725,#24726,#24727,
#24728,#24729,#24730,#24731,#24732,#24733,#24734,#24735,#24736,#24737,#24738,
#24739,#24740,#24741,#24742,#24743,#24744,#24745,#24746,#24747,#24748,#24749,
#24750,#24751,#24752,#24753,#24754,#24755,#24756,#24757,#24758,#24759,#24760,
#24761,#24762,#24763,#24764,#24765,#24766,#24767,#24768,#24769,#24770,#24771,
#24772,#24773,#24774,#24775,#24776,#24777,#24778,#24779,#24780,#24781,#24782,
#24783,#24784,#24785,#24786,#24787,#24788,#24789,#24790,#24791,#24792,#24793,
#24794,#24795,#24796,#24797,#24798,#24799,#24800,#24801,#24802,#24803,#24804,
#24805,#24806,#24807,#24808,#24809,#24810,#24811,#24812,#24813,#24814,#24815,
#24816,#24817,#24818,#24819,#24820,#24821,#24822,#24823,#24824,#24825,#24826,
#24827,#24828,#24829,#24830,#24831,#24832,#24833,#24834,#24835,#24836,#24837,
#24838,#24839,#24840,#24841,#24842,#24843,#24844,#24845,#24846,#24847,#24848,
#24849,#24850,#24851,#24852,#24853,#24854,#24855,#24856,#24857,#24858,#24859,
#24860,#24861,#24862,#24863,#24864,#24865,#24866,#24867,#24868,#24869,#24870,
#24871,#24872,#24873,#24874,#24875,#24876,#24877,#24878,#24879,#24880,#24881,
#24882,#24883,#24884,#24885,#24886,#24887,#24888,#24889,#24890,#24891,#24892,
#24893,#24894,#24895,#24896,#24897,#24898,#24899,#24900,#24901,#24902,#24903,
#24904,#24905,#24906,#24907,#24908,#24909,#24910,#24911,#24912,#24913,#24914,
#24915,#24916,#24917,#24918,#24919,#24920,#24921,#24922,#24923,#24924,#24925,
#24926,#24927,#24928,#24929,#24930,#24931,#24932,#24933,#24934,#24935,#24936,
#24937,#24938,#24939,#24940,#24941,#24942,#24943,#24944,#24945,#24946,#24947,
#24948,#24949,#24950,#24951,#24952,#24953,#24954,#24955,#24956,#24957,#24958,
#24959,#24960,#24961,#24962,#24963,#24964,#24965,#24966,#24967,#24968,#24969,
#24970,#24971,#24972,#24973,#24974,#24975,#24976,#24977,#24978,#24979,#24980,
#24981,#24982,#24983,#24984,#24985,#24986,#24987,#24988,#24989,#24990,#24991,
#24992,#24993,#24994,#24995,#24996,#24997,#24998,#24999,#25000,#25001,#25002,
#25003,#25004,#25005,#25006,#25007,#25008,#25009,#25010,#25011,#25012,#25013,
#25014,#25015),.UNSPECIFIED.,.F.,.F.,(4,3,3,3,3,3,3,3,3,3,3,3,3,3,3,3,3,
3,3,3,3,3,3,3,3,3,3,3,3,3,3,3,3,3,3,3,3,3,3,3,3,3,3,3,3,3,3,3,3,3,3,3,3,
3,3,3,3,3,3,3,3,3,3,3,3,3,3,3,3,3,3,3,3,3,3,3,3,3,3,3,3,3,3,3,3,3,3,3,3,
3,3,3,3,3,3,3,3,3,3,3,3,4),(-16.6593614944316,-16.5954782572781,-16.5289225612824,
-16.4623668652867,-16.4000094150394,-16.3376992006281,-16.2753956730767,
-16.2130959318694,-16.1506987647291,-16.0883926326437,-16.025949947976,
-15.9635072633083,-15.901149813061,-15.8388395986498,-15.7765360710986,
-15.7142363298915,-15.6518391627511,-15.5895330306658,-15.5270903459979,
-15.4646476613299,-15.4022902110826,-15.3399799966714,-15.2776764691201,
-15.2153767279131,-15.1529795607727,-15.0906734286873,-15.0282307440194,
-14.9657880593515,-14.9034306091042,-14.841120394693,-14.7788168671418,
-14.7165171259347,-14.6541199587943,-14.5918138267091,-14.5293711420411,
-14.4669284573731,-14.4045710071258,-14.3422607927144,-14.2799572651628,
-14.2176575239555,-14.1552603568154,-14.0929542247299,-14.0305115400623,
-13.9680688553948,-13.9057114051475,-13.8434011907372,-13.7810976631868,
-13.7187979219806,-13.6564007548396,-13.5940946227552,-13.5316519380858,
-13.4692092534164,-13.4068518031691,-13.3445415887561,-13.282238061203,
-13.2199383199941,-13.1575411528551,-13.0952350207681,-13.0327923361031,
-12.970349651438,-12.9079922011907,-12.8456819867821,-12.7833784592334,
-12.7210787180288,-12.6586815508865,-12.5963754188038,-12.5339327341317,
-12.4714900494596,-12.4091325992123,-12.3468223847994,-12.2845188572466,
-12.2222191160378,-12.1598219488986,-12.0975158168117,-12.0350731321465,
-11.9726304474812,-11.9102729972339,-11.8479627828177,-11.7856592552614,
-11.7233595140491,-11.6609623469126,-11.5986562148222,-11.5362135301625,
-11.4737708455028,-11.4114133952555,-11.3491031808696,-11.2867996533438,
-11.2244999121623,-11.1621027450028,-11.0997966129428,-11.0373539282336,
-10.9749112435245,-10.9125537932772,-10.8502435787957,-10.7879400511739,
-10.7256403098962,-10.6632431428086,-10.6009370106539,-10.5384943261,-10.4760516415461,
-10.4098345567239,-10.3761761872893),.UNSPECIFIED.) ;
#227 = B_SPLINE_CURVE_WITH_KNOTS('',3,(#25016,#25017,#25018,#25019,#25020,
#25021,#25022,#25023,#25024,#25025,#25026,#25027,#25028,#25029,#25030,#25031,
#25032,#25033,#25034,#25035,#25036,#25037,#25038,#25039,#25040,#25041,#25042,
#25043,#25044,#25045,#25046,#25047,#25048,#25049,#25050,#25051,#25052,#25053,
#25054,#25055,#25056,#25057,#25058,#25059,#25060,#25061,#25062,#25063,#25064,
#25065,#25066,#25067,#25068,#25069,#25070,#25071,#25072,#25073,#25074,#25075,
#25076,#25077,#25078,#25079,#25080,#25081,#25082,#25083,#25084,#25085,#25086,
#25087,#25088,#25089,#25090,#25091,#25092,#25093,#25094,#25095,#25096,#25097,
#25098,#25099,#25100,#25101,#25102,#25103,#25104,#25105,#25106,#25107,#25108,
#25109,#25110,#25111,#25112,#25113,#25114,#25115,#25116,#25117,#25118,#25119,
#25120,#25121,#25122,#25123,#25124,#25125,#25126,#25127,#25128,#25129,#25130,
#25131,#25132,#25133,#25134,#25135,#25136,#25137,#25138,#25139,#25140,#25141,
#25142,#25143,#25144,#25145,#25146,#25147,#25148,#25149,#25150,#25151,#25152,
#25153,#25154,#25155,#25156,#25157,#25158,#25159,#25160,#25161,#25162,#25163,
#25164,#25165,#25166,#25167,#25168,#25169,#25170,#25171,#25172,#25173,#25174,
#25175,#25176,#25177,#25178,#25179,#25180,#25181,#25182,#25183,#25184,#25185,
#25186,#25187,#25188,#25189,#25190,#25191,#25192,#25193,#25194,#25195,#25196,
#25197,#25198,#25199,#25200,#25201,#25202,#25203,#25204,#25205,#25206,#25207,
#25208,#25209,#25210,#25211,#25212,#25213,#25214,#25215,#25216,#25217,#25218,
#25219,#25220,#25221,#25222,#25223,#25224,#25225,#25226,#25227,#25228,#25229,
#25230,#25231,#25232,#25233,#25234,#25235,#25236,#25237,#25238,#25239,#25240,
#25241,#25242,#25243,#25244,#25245,#25246,#25247,#25248,#25249,#25250,#25251,
#25252,#25253,#25254,#25255,#25256,#25257,#25258,#25259,#25260,#25261,#25262,
#25263,#25264,#25265,#25266,#25267,#25268,#25269,#25270,#25271,#25272,#25273,
#25274,#25275,#25276,#25277,#25278,#25279,#25280,#25281,#25282,#25283,#25284,
#25285,#25286,#25287,#25288,#25289,#25290,#25291,#25292,#25293,#25294,#25295,
#25296,#25297,#25298,#25299,#25300,#25301,#25302,#25303,#25304,#25305,#25306,
#25307,#25308,#25309,#25310,#25311,#25312,#25313,#25314,#25315,#25316,#25317,
#25318,#25319,#25320,#25321,#25322,#25323,#25324,#25325,#25326,#25327,#25328,
#25329,#25330,#25331,#25332,#25333,#25334,#25335,#25336,#25337,#25338,#25339,
#25340,#25341,#25342,#25343,#25344,#25345,#25346,#25347,#25348,#25349,#25350,
#25351,#25352,#25353,#25354,#25355,#25356,#25357,#25358,#25359,#25360,#25361,
#25362,#25363,#25364,#25365,#25366,#25367,#25368,#25369,#25370,#25371,#25372,
#25373,#25374,#25375,#25376,#25377,#25378,#25379,#25380,#25381,#25382,#25383,
#25384,#25385,#25386,#25387,#25388,#25389,#25390,#25391,#25392,#25393,#25394,
#25395,#25396,#25397,#25398,#25399,#25400,#25401,#25402,#25403,#25404,#25405),
 .UNSPECIFIED.,.F.,.F.,(4,2,2,2,2,2,2,2,2,2,2,2,2,2,2,2,2,2,2,2,2,2,2,2,
2,2,2,2,2,2,2,2,2,2,2,2,2,2,2,2,2,2,2,2,2,2,2,2,2,2,2,2,2,2,2,2,2,2,2,2,
2,2,2,2,2,2,2,2,2,2,2,2,2,2,2,2,2,2,2,2,2,2,2,2,2,2,2,2,2,2,2,2,2,2,2,2,
2,2,2,2,2,2,2,2,2,2,2,2,2,2,2,2,2,2,2,2,2,2,2,2,2,2,2,2,2,2,2,2,2,2,2,2,
2,2,2,2,2,2,2,2,2,2,2,2,2,2,2,2,2,2,2,2,2,2,2,2,2,2,2,2,2,2,2,2,2,2,2,2,
2,2,2,2,2,2,2,2,2,2,2,2,2,2,2,2,2,2,2,2,2,2,2,2,2,2,4),(6.54590052552168E-5,
0.0660743354571956,0.103646198129629,0.1252023219725,0.143355746835144,
0.16207812232254,0.196548198026947,0.364599260483942,0.530414938452012,
0.563373596596461,0.589086313045187,0.623967302147303,0.661850038598023,
0.708184547062534,0.96964444084449,1.03777847100332,1.07140718005652,1.09885832328466,
1.11306927385535,1.13190624320692,1.16703366806672,1.33681292915678,1.45677425094401,
1.51591602316336,1.52067111789573,1.52476468859033,1.52832269269611,1.53144559951978,
1.53421362971229,1.53669108928998,1.5389298436005,1.54097205554933,1.54285232749387,
1.54459937456026,1.54623733703716,1.54778681886104,1.54926572133688,1.55068992711668,
1.55207387897404,1.55343109095958,1.55477462589866,1.55611757297875,1.55747356314925,
1.5588573698539,1.59408144255242,1.63209985338781,1.67903832309788,1.84154000799963,
2.00028928923424,2.05155362069965,2.07543402909437,2.09535154223313,2.12467914335601,
2.21652710044626,2.24569141154283,2.4050812360259,2.45164657977742,2.51943120454188,
2.55988944332175,2.59784982310284,2.65120519507239,2.87248814984226,2.99452113975738,
3.03035923015238,3.05138364080831,3.07019711407189,3.10519029423227,3.2124988329447,
3.22937708618387,3.37879241285159,3.42376313105816,3.48995977422986,3.53013228964512,
3.56780382128332,3.62173376307465,3.83971854740559,3.96339735836579,3.99941880927593,
4.0204793111109,4.03926364197498,4.07408997537889,4.17913571272868,4.21352263299063,
4.35297971909989,4.39622995004449,4.46068209329239,4.50054032269965,4.53838163473991,
4.59340962187226,4.7035779351548,4.77050878541039,4.88795941750521,4.95349857385879,
4.97948430158276,4.99918292756109,5.02515497019942,5.08560122530602,5.17513098832738,
5.31957831295779,5.36370711060574,5.42905416069796,5.46907362879258,5.50682450200796,
5.55255303132238,5.6790786642144,5.84209677309376,5.88062597494018,5.92949393068853,
5.95296982544281,5.97298923678071,6.00309139095167,6.1069188961213,6.24168575063817,
6.3286708128752,6.39630705601036,6.43673881669355,6.47471170407527,6.52814902418533,
6.74898021993785,6.87123375025607,6.90709669588237,6.92812608271242,6.94693571741768,
6.98190649947664,7.08890827239652,7.25023590060713,7.29709675142791,7.36517279691773,
7.40568360148085,7.44362079455436,7.49681933001752,7.7190028270069,7.84059300385476,
7.87638152186083,7.89739631457088,7.9162180052221,7.95125752430234,8.1508609250141,
8.25353079054083,8.328992286189,8.37080771702598,8.40831483255875,8.45743136325945,
8.58895408285465,8.64289928696326,8.76350317435513,8.80985943264742,8.84560889744294,
8.86661597948867,8.88544394006687,8.9205194826862,9.10716755185701,9.12225749881739,
9.2236941365127,9.29857174501226,9.3402859599525,9.37781742511362,9.42713395574194,
9.5644409129488,9.72075816499905,9.75848990013041,9.80667613990164,9.83003414494448,
9.85008828593659,9.88043509359002,9.99059322055077,10.156125442796,10.2036112691254,
10.2359891066826,10.2886633017569,10.3265234965363,10.3672152888013,10.4363011155497,
10.6736725170651,10.734943384144,10.7785105700521,10.8010374018716,10.8211737117607,
10.8533063210872,11.0415303876383,11.18253517616,11.2460005498542,11.2856813892659,
11.3236317291432,11.3702673983871,11.533682275802,11.6923778519106,11.743607978469,
11.7674829130203,11.7874019596289,11.8167403325837,11.9086749671978,12.0355647832628,
12.1338726876243,12.2072456703103),.UNSPECIFIED.) ;
#228 = B_SPLINE_CURVE_WITH_KNOTS('',3,(#25410,#25411,#25412,#25413,#25414,
#25415,#25416,#25417,#25418,#25419,#25420,#25421,#25422,#25423,#25424,#25425,
#25426,#25427,#25428,#25429,#25430,#25431,#25432,#25433,#25434,#25435,#25436,
#25437,#25438,#25439,#25440,#25441,#25442,#25443,#25444,#25445,#25446,#25447,
#25448,#25449,#25450,#25451,#25452,#25453,#25454,#25455,#25456,#25457,#25458,
#25459,#25460,#25461,#25462,#25463,#25464,#25465,#25466,#25467,#25468,#25469,
#25470,#25471,#25472,#25473,#25474,#25475,#25476,#25477,#25478,#25479,#25480,
#25481,#25482,#25483,#25484,#25485,#25486,#25487,#25488,#25489,#25490,#25491,
#25492,#25493,#25494,#25495,#25496,#25497,#25498,#25499,#25500,#25501,#25502,
#25503,#25504,#25505,#25506,#25507,#25508,#25509,#25510,#25511,#25512,#25513,
#25514,#25515,#25516,#25517,#25518,#25519,#25520,#25521,#25522,#25523,#25524,
#25525,#25526,#25527,#25528,#25529,#25530,#25531,#25532,#25533,#25534,#25535,
#25536,#25537,#25538,#25539,#25540,#25541,#25542,#25543,#25544,#25545,#25546,
#25547,#25548,#25549,#25550,#25551,#25552,#25553,#25554,#25555,#25556,#25557,
#25558,#25559,#25560,#25561,#25562,#25563,#25564,#25565,#25566,#25567,#25568,
#25569,#25570,#25571,#25572,#25573,#25574,#25575,#25576,#25577,#25578,#25579,
#25580,#25581,#25582,#25583,#25584,#25585,#25586,#25587,#25588,#25589,#25590,
#25591,#25592,#25593,#25594,#25595,#25596,#25597,#25598,#25599,#25600,#25601,
#25602,#25603,#25604,#25605,#25606,#25607,#25608,#25609,#25610,#25611,#25612,
#25613,#25614,#25615,#25616,#25617,#25618,#25619,#25620,#25621,#25622,#25623,
#25624,#25625,#25626,#25627,#25628,#25629,#25630,#25631,#25632,#25633,#25634,
#25635,#25636,#25637,#25638,#25639,#25640,#25641,#25642,#25643,#25644,#25645,
#25646,#25647,#25648,#25649,#25650,#25651,#25652,#25653,#25654,#25655,#25656,
#25657,#25658,#25659,#25660,#25661,#25662,#25663,#25664,#25665,#25666,#25667,
#25668,#25669,#25670,#25671,#25672,#25673,#25674,#25675,#25676,#25677,#25678,
#25679,#25680,#25681,#25682,#25683,#25684,#25685,#25686,#25687,#25688,#25689,
#25690,#25691,#25692,#25693,#25694,#25695,#25696,#25697,#25698,#25699,#25700,
#25701,#25702,#25703,#25704,#25705,#25706,#25707,#25708,#25709,#25710,#25711,
#25712,#25713,#25714,#25715,#25716,#25717,#25718,#25719,#25720,#25721,#25722,
#25723,#25724,#25725,#25726,#25727,#25728,#25729,#25730,#25731,#25732,#25733,
#25734,#25735,#25736,#25737,#25738,#25739,#25740,#25741,#25742,#25743,#25744,
#25745,#25746,#25747,#25748,#25749,#25750,#25751,#25752,#25753,#25754,#25755,
#25756,#25757,#25758,#25759,#25760,#25761,#25762,#25763,#25764,#25765,#25766,
#25767,#25768,#25769,#25770,#25771,#25772,#25773,#25774,#25775,#25776,#25777,
#25778,#25779,#25780,#25781,#25782,#25783,#25784,#25785,#25786,#25787,#25788,
#25789,#25790,#25791,#25792,#25793,#25794,#25795,#25796,#25797,#25798,#25799,
#25800,#25801,#25802,#25803,#25804,#25805,#25806,#25807,#25808,#25809,#25810,
#25811,#25812,#25813,#25814,#25815,#25816,#25817,#25818,#25819,#25820,#25821,
#25822,#25823,#25824,#25825,#25826,#25827,#25828,#25829,#25830,#25831,#25832,
#25833,#25834,#25835,#25836,#25837,#25838,#25839,#25840,#25841,#25842,#25843,
#25844,#25845,#25846,#25847,#25848,#25849,#25850,#25851,#25852,#25853,#25854,
#25855,#25856,#25857,#25858,#25859,#25860,#25861,#25862,#25863,#25864,#25865,
#25866,#25867,#25868,#25869,#25870,#25871,#25872,#25873,#25874,#25875,#25876,
#25877,#25878,#25879,#25880,#25881),.UNSPECIFIED.,.F.,.F.,(4,2,2,2,2,2,
2,2,2,2,2,2,2,2,2,2,2,2,2,2,2,2,2,2,2,2,2,2,2,2,2,2,2,2,2,2,2,2,2,2,2,2,
2,2,2,2,2,2,2,2,2,2,2,2,2,2,2,2,2,2,2,2,2,2,2,2,2,2,2,2,2,2,2,2,2,2,2,2,
2,2,2,2,2,2,2,2,2,2,2,2,2,2,2,2,2,2,2,2,2,2,2,2,2,2,2,2,2,2,2,2,2,2,2,2,
2,2,2,2,2,2,2,2,2,2,2,2,2,2,2,2,2,2,2,2,2,2,2,2,2,2,2,2,2,2,2,2,2,2,2,2,
2,2,2,2,2,2,2,2,2,2,2,2,2,2,2,2,2,2,2,2,2,2,2,2,2,2,2,2,2,2,2,2,2,2,2,2,
2,2,2,2,2,2,2,2,2,2,2,2,2,2,2,2,2,2,2,2,2,2,2,2,2,2,2,2,2,2,2,2,2,2,2,2,
2,2,2,2,2,2,2,2,2,2,2,2,2,4),(12.2072906505637,12.2333995230658,12.2998920652981,
12.4204853076344,12.4746294858109,12.6059734111218,12.6550894061824,12.6925963981913,
12.7344119738802,12.8098747078753,12.9125471786017,13.1121343210669,13.1471771244674,
13.1659993677865,13.1870133994815,13.2227982146858,13.3443555734894,13.5666085535278,
13.619795761001,13.6577312089582,13.6982456861688,13.7663425696405,13.8132246011097,
13.9746937416869,14.0815144599795,14.1164717439445,14.1352789917533,14.1563111994805,
14.1921886888268,14.3145723171371,14.5351379620659,14.5886240749683,14.6266042491524,
14.6670199966474,14.7345675613066,14.8213843933541,14.9480065971356,15.0604443260453,
15.0904788517653,15.1104888354367,15.1339980265039,15.18306001687,15.2218179084713,
15.3868202369665,15.5148871547583,15.5635152706309,15.6009650600216,15.6430383627059,
15.7200011187959,15.8258947711875,15.8926597645677,15.9399753637726,16.0312743658349,
16.0605325499453,16.0804416019661,16.1043607935269,16.1558597319316,16.3149858635752,
16.4701698017627,16.5251213385783,16.562950421573,16.6028289716119,16.6673950459589,
16.7107567540235,16.8508379093865,16.8761607749545,16.906370006885,16.9999039644488,
17.0294141907173,17.0493544398992,17.0731346433331,17.1237973782612,17.2819685123973,
17.4479777167766,17.4941531132684,17.5320007288664,17.571847058112,17.6362348917337,
17.6794224762023,17.8185324364809,17.8665906361654,17.9370164162362,17.9846775334201,
18.0079436938594,18.0280262756519,18.0585692200623,18.1838462680258,18.4180055990733,
18.4638778223217,18.501659307889,18.5416213709074,18.6066518327291,18.6504690683125,
18.7931269099642,18.823958030315,18.9278349860858,18.9625848584942,18.9813557107571,
19.0024326816713,19.0385385652653,19.1629850145529,19.3799199640003,19.4339055464632,
19.471585145455,19.5117401022612,19.5778412768407,19.6227172196298,19.7715658839122,
19.8021551667263,19.9062357434439,19.9363309993209,19.9563491777512,19.9798277948077,
20.0287130877471,20.0672630437681,20.2304614994038,20.3560953414037,20.4020660760878,
20.4398687809886,20.4797923610338,20.5446100498309,20.7116044997462,20.7573909757551,
20.865623977585,20.9006842262204,20.9195092636372,20.9405190157294,20.9762835009882,
21.0008894822945,21.1590469701795,21.3248235295797,21.3709615298301,21.4088007590458,
21.4486607337168,21.5131253400588,21.5563880460295,21.695916972558,21.727860631611,
21.8349492965941,21.8699257819381,21.8887361337303,21.9097636543885,21.9456187257387,
22.0678060336367,22.2887686798031,22.3421808380487,22.380149271758,22.4205879504804,
22.4882662660198,22.575331937019,22.7019456534822,22.8139126481655,22.8439389453787,
22.8639474710601,22.8796255428054,22.8798710868697,22.8801208893376,22.8803751977609,
22.8806342700849,22.8808983754389,22.8811677948888,22.8814428223748,22.8817237656049,
22.8820109469831,22.8823047046758,22.882605393669,22.8829133869871,22.8832290768713,
22.8835528761049,22.8838852194455,22.8842265651085,22.8845773963741,22.8849382232655,
22.8853095843748,22.8856920488534,22.8860862184288,22.8864927296133,22.8869122561194,
22.8873455113299,22.8877932510179,22.8882562762144,22.8887354362864,22.8892316322082,
22.8897458200612,22.8902790147546,22.8908322940296,22.8914068027022,22.8920037571857,
22.8926244503446,22.893270256656,22.8939426377042,22.8946431480831,22.8953734416365,
22.8961352781657,22.8963728185666,22.8966383520258,22.8969353318644,22.8972676697636,
22.8976398025119,22.8980567694588,22.8985243020402,22.8990489274648,22.8996380885287,
22.9003002817726,22.901045216305,22.9018839955778,22.9028293242095,22.9038957414864,
22.9050998824483,22.9064607661696,22.9080001089037,22.9097426571472,22.9117165315429,
22.9553119449238,23.0625266937836,23.2514205529398,23.3077527107458,23.3454329646705,
23.3777691992466,23.4269424204246,23.4879482197223,23.5553218510742,23.6819455263177,
23.7834993556504,23.8133239900265,23.8333050193339,23.8519007961556,23.8816510206883,
23.8896786880865,23.9833988046422,24.1196332017496,24.2390329191062,24.2870761464822,
24.3229922517165,24.3578991392153,24.4142930285787),.UNSPECIFIED.) ;
#229 = B_SPLINE_CURVE_WITH_KNOTS('',3,(#25882,#25883,#25884,#25885,#25886,
#25887,#25888,#25889,#25890,#25891,#25892,#25893,#25894,#25895,#25896,#25897,
#25898,#25899,#25900,#25901,#25902,#25903,#25904,#25905,#25906,#25907,#25908,
#25909,#25910,#25911,#25912,#25913,#25914,#25915,#25916,#25917,#25918,#25919,
#25920,#25921,#25922,#25923,#25924,#25925,#25926,#25927,#25928,#25929,#25930,
#25931,#25932,#25933,#25934,#25935,#25936,#25937,#25938,#25939,#25940,#25941,
#25942,#25943,#25944,#25945,#25946,#25947,#25948,#25949,#25950,#25951,#25952,
#25953,#25954,#25955,#25956,#25957,#25958,#25959,#25960,#25961,#25962,#25963,
#25964,#25965,#25966,#25967,#25968,#25969,#25970,#25971,#25972,#25973,#25974,
#25975,#25976,#25977,#25978,#25979,#25980,#25981,#25982,#25983,#25984,#25985,
#25986,#25987,#25988,#25989,#25990,#25991,#25992,#25993,#25994,#25995,#25996,
#25997,#25998,#25999,#26000,#26001,#26002,#26003,#26004,#26005,#26006,#26007,
#26008,#26009,#26010,#26011,#26012,#26013,#26014,#26015,#26016,#26017,#26018,
#26019,#26020,#26021,#26022,#26023,#26024,#26025,#26026,#26027,#26028,#26029,
#26030,#26031,#26032,#26033,#26034,#26035,#26036,#26037,#26038,#26039,#26040,
#26041,#26042,#26043,#26044,#26045,#26046,#26047,#26048,#26049,#26050,#26051,
#26052,#26053,#26054,#26055,#26056,#26057,#26058,#26059,#26060,#26061,#26062,
#26063,#26064,#26065,#26066,#26067,#26068,#26069,#26070,#26071,#26072,#26073,
#26074,#26075,#26076,#26077,#26078,#26079,#26080,#26081,#26082,#26083,#26084,
#26085,#26086,#26087,#26088,#26089,#26090,#26091,#26092,#26093,#26094,#26095,
#26096,#26097,#26098,#26099,#26100,#26101,#26102,#26103,#26104,#26105,#26106,
#26107,#26108,#26109,#26110,#26111,#26112,#26113,#26114,#26115,#26116,#26117,
#26118,#26119,#26120,#26121,#26122,#26123,#26124,#26125,#26126,#26127,#26128,
#26129,#26130,#26131,#26132,#26133,#26134,#26135,#26136,#26137,#26138,#26139,
#26140,#26141,#26142,#26143,#26144,#26145,#26146,#26147,#26148,#26149,#26150,
#26151,#26152,#26153,#26154,#26155,#26156,#26157,#26158,#26159,#26160,#26161,
#26162,#26163,#26164,#26165,#26166,#26167,#26168,#26169,#26170,#26171,#26172,
#26173,#26174,#26175,#26176,#26177,#26178,#26179,#26180,#26181,#26182,#26183,
#26184,#26185,#26186,#26187,#26188,#26189,#26190,#26191,#26192,#26193,#26194,
#26195,#26196,#26197,#26198,#26199,#26200,#26201,#26202,#26203,#26204,#26205,
#26206,#26207,#26208,#26209,#26210,#26211,#26212,#26213,#26214,#26215,#26216,
#26217,#26218,#26219,#26220,#26221,#26222,#26223,#26224,#26225,#26226,#26227,
#26228,#26229,#26230,#26231,#26232,#26233,#26234,#26235),.UNSPECIFIED.,
 .F.,.F.,(4,2,2,2,2,2,2,2,2,2,2,2,2,2,2,2,2,2,2,2,2,2,2,2,2,2,2,2,2,2,2,
2,2,2,2,2,2,2,2,2,2,2,2,2,2,2,2,2,2,2,2,2,2,2,2,2,2,2,2,2,2,2,2,2,2,2,2,
2,2,2,2,2,2,2,2,2,2,2,2,2,2,2,2,2,2,2,2,2,2,2,2,2,2,2,2,2,2,2,2,2,2,2,2,
2,2,2,2,2,2,2,2,2,2,2,2,2,2,2,2,2,2,2,2,2,2,2,2,2,2,2,2,2,2,2,2,2,2,2,2,
2,2,2,2,2,2,2,2,2,2,2,2,2,2,2,2,2,2,2,2,2,2,2,2,2,2,2,2,2,2,2,2,2,2,2,2,
2,4),(12.2072456703103,12.2486977382348,12.2862991346331,12.3370675853609,
12.4955056945959,12.6723064111662,12.7165364236069,12.7391860550326,12.7595074682699,
12.7915485636307,12.8314569706321,12.9227553177696,13.1407849364068,13.1947105076481,
13.2323818102843,13.2725564714223,13.3387627942662,13.4561514293095,13.6585370836615,
13.6928946928717,13.7115979590741,13.7327653686174,13.7693258959595,13.8979719074965,
14.108548001842,14.1631311423434,14.2009032660361,14.2408851037059,14.3060212698353,
14.3499419636041,14.4931891857176,14.5541961935573,14.6395264434425,14.6680975226309,
14.6879299393261,14.7122594485561,14.7662943566752,14.8510953181161,15.0865196191968,
15.1323492953002,15.1701221666306,15.2101020929185,15.2752284435875,15.3191395794418,
15.4623325335554,15.4979301920437,15.6054949295739,15.6355678551499,15.6555832804525,
15.6790737572924,15.7280260735791,15.7666545126145,15.9305281011558,16.0528048640956,
16.0997150011174,16.1377272874295,16.1773138358134,16.2402544764528,16.2820392513916,
16.4135664983527,16.4593764288642,16.56517460133,16.6000563850533,16.6188504597195,
16.6398990102012,16.6758594576763,16.7989868423694,17.01802376967,17.0717863210419,
17.1094327589452,17.1496568773599,17.2161392823434,17.30095135273,17.4123212286938,
17.5329590784149,17.5686136285624,17.5875438179729,17.6084343884826,17.6435855486997,
17.6676047878321,17.707172586896,17.8794535122686,17.9648471064293,18.0294516412634,
18.0693374199954,18.107599066136,18.1628843422288,18.2280923016221,18.3740617889961,
18.4108101264105,18.5134536822447,18.5433407488112,18.5633306086471,18.5869139438179,
18.6364094567011,18.6756807452355,18.8452506629214,18.9464257791202,19.0047585507113,
19.039664322051,19.0781107971785,19.13452402533,19.2884483576653,19.4776528089821,
19.5099864957067,19.5301567007405,19.552611715689,19.5957942459034,19.6279335709638,
19.7448230752108,19.8090063387367,19.9357316367902,19.9847596060258,20.0222559995674,
20.0641168322337,20.139841803154,20.2430719388833,20.4191025263796,20.467737281041,
20.491173005453,20.5112040083972,20.5413885849518,20.6574709219083,20.9027636167975,
20.9482081267957,20.9858985819515,21.0260337314445,21.0920226627224,21.1759153590753,
21.2884491584225,21.3908037678933,21.4378195218731,21.4609722025259,21.4810928752659,
21.5118887521058,21.6459575211512,21.8635283825155,21.9175082296144,21.9551873756986,
21.9953448636759,22.0614578718175,22.106345289338,22.2552610128412,22.2839220264468,
22.3903933354499,22.4202267376629,22.4402093140805,22.4638198895315,22.513475814836,
22.5529380950516,22.7242489607561,22.8152070971007,22.8775374852681,22.9170144222158,
22.9555507746083,23.0081366376917,23.2596158863234,23.3598101309815,23.3890076525042,
23.4041051946206,23.4185004054957,23.4390365433674,23.4688488899205,23.5247468046023,
23.706992854538,23.817547422462,23.8652438975169,23.9025270406034,23.9376075996493,
23.9804287313472,24.1651712231583,24.2505805506159,24.3322618369051,24.3577837539985,
24.3775616024521,24.3948373796966,24.414543948155),.UNSPECIFIED.) ;
#230 = B_SPLINE_CURVE_WITH_KNOTS('',3,(#26240,#26241,#26242,#26243,#26244,
#26245,#26246,#26247,#26248,#26249,#26250,#26251,#26252,#26253,#26254,#26255,
#26256,#26257,#26258,#26259,#26260,#26261,#26262,#26263,#26264,#26265,#26266,
#26267,#26268,#26269,#26270,#26271,#26272,#26273,#26274,#26275,#26276,#26277,
#26278,#26279,#26280,#26281,#26282,#26283,#26284,#26285,#26286,#26287,#26288,
#26289,#26290,#26291,#26292,#26293,#26294,#26295,#26296,#26297,#26298,#26299,
#26300,#26301,#26302,#26303,#26304,#26305,#26306,#26307,#26308,#26309,#26310,
#26311,#26312,#26313,#26314,#26315,#26316,#26317,#26318,#26319,#26320,#26321,
#26322,#26323,#26324,#26325,#26326,#26327,#26328,#26329,#26330,#26331,#26332,
#26333,#26334,#26335,#26336,#26337,#26338,#26339,#26340,#26341,#26342,#26343,
#26344,#26345,#26346,#26347,#26348,#26349,#26350,#26351,#26352,#26353,#26354,
#26355,#26356,#26357,#26358,#26359,#26360,#26361,#26362,#26363,#26364,#26365,
#26366,#26367,#26368,#26369,#26370,#26371,#26372,#26373,#26374,#26375,#26376,
#26377,#26378,#26379,#26380,#26381,#26382,#26383,#26384,#26385,#26386,#26387,
#26388,#26389,#26390,#26391,#26392,#26393,#26394,#26395,#26396,#26397,#26398,
#26399,#26400,#26401,#26402,#26403,#26404,#26405,#26406,#26407,#26408,#26409,
#26410,#26411,#26412,#26413,#26414,#26415,#26416,#26417,#26418,#26419,#26420,
#26421,#26422,#26423,#26424,#26425,#26426,#26427,#26428,#26429,#26430,#26431,
#26432,#26433,#26434,#26435,#26436,#26437,#26438,#26439,#26440,#26441,#26442,
#26443,#26444,#26445,#26446,#26447,#26448,#26449,#26450,#26451,#26452,#26453,
#26454,#26455,#26456,#26457,#26458,#26459,#26460,#26461,#26462,#26463,#26464,
#26465,#26466,#26467,#26468,#26469,#26470,#26471,#26472,#26473,#26474,#26475,
#26476,#26477,#26478,#26479,#26480,#26481,#26482,#26483,#26484,#26485,#26486,
#26487,#26488,#26489,#26490,#26491,#26492,#26493,#26494,#26495,#26496,#26497,
#26498,#26499,#26500,#26501,#26502,#26503,#26504,#26505,#26506,#26507,#26508,
#26509,#26510,#26511,#26512,#26513,#26514,#26515,#26516,#26517,#26518,#26519,
#26520,#26521,#26522,#26523,#26524,#26525,#26526,#26527,#26528,#26529,#26530,
#26531,#26532,#26533,#26534,#26535,#26536,#26537,#26538,#26539,#26540,#26541,
#26542,#26543,#26544,#26545,#26546,#26547,#26548,#26549,#26550,#26551,#26552,
#26553,#26554,#26555,#26556,#26557,#26558,#26559,#26560,#26561,#26562,#26563,
#26564,#26565,#26566,#26567,#26568,#26569,#26570,#26571,#26572,#26573,#26574,
#26575,#26576,#26577,#26578,#26579,#26580,#26581,#26582,#26583,#26584,#26585,
#26586,#26587,#26588,#26589,#26590,#26591,#26592,#26593,#26594,#26595,#26596,
#26597,#26598,#26599,#26600,#26601,#26602,#26603,#26604,#26605,#26606,#26607,
#26608,#26609,#26610,#26611,#26612,#26613,#26614,#26615,#26616,#26617,#26618,
#26619,#26620,#26621,#26622,#26623,#26624,#26625,#26626,#26627,#26628,#26629,
#26630,#26631,#26632,#26633,#26634,#26635,#26636,#26637,#26638,#26639,#26640,
#26641,#26642,#26643,#26644,#26645,#26646,#26647,#26648,#26649,#26650,#26651,
#26652,#26653),.UNSPECIFIED.,.F.,.F.,(4,2,2,2,2,2,2,2,2,2,2,2,2,2,2,2,2,
2,2,2,2,2,2,2,2,2,2,2,2,2,2,2,2,2,2,2,2,2,2,2,2,2,2,2,2,2,2,2,2,2,2,2,2,
2,2,2,2,2,2,2,2,2,2,2,2,2,2,2,2,2,2,2,2,2,2,2,2,2,2,2,2,2,2,2,2,2,2,2,2,
2,2,2,2,2,2,2,2,2,2,2,2,2,2,2,2,2,2,2,2,2,2,2,2,2,2,2,2,2,2,2,2,2,2,2,2,
2,2,2,2,2,2,2,2,2,2,2,2,2,2,2,2,2,2,2,2,2,2,2,2,2,2,2,2,2,2,2,2,2,2,2,2,
2,2,2,2,2,2,2,2,2,2,2,2,2,2,2,2,2,2,2,2,2,2,2,2,2,2,2,2,2,2,2,2,2,2,2,2,
2,2,2,2,2,2,2,2,2,4),(8.33097403985845E-5,0.037924742923994,0.0723184899431885,
0.108380290041682,0.156714991299736,0.280103304901921,0.417705952640096,
0.420982404833398,0.425206806614123,0.430689472612384,0.454416149801046,
0.52869592538976,0.550033669237741,0.570400687153203,0.592952016895259,
0.636652157922749,0.813935734611086,0.920813221386165,0.97642504527676,
1.02383562632131,1.05434606689617,1.08921156671304,1.1453040955072,1.32097494979816,
1.43620600469129,1.4814893668784,1.48269234458807,1.48354804559005,1.4841557118606,
1.48458676224817,1.48655803406899,1.48830150331304,1.48984406973238,1.4912095796305,
1.49241909838386,1.49349118516626,1.49444215930972,1.49528635161025,1.49603633674722,
1.49670314481816,1.49729645157753,1.49782474777846,1.498295488897,1.49871522661799,
1.49908972385428,1.49942405501724,1.49972269326349,1.49998958623333,1.50022822184291,
1.50096734386075,1.50167606978337,1.52202439888614,1.53644654344062,1.55510281038928,
1.58918819506854,1.75838878910648,1.87988919515148,1.96362838272971,2.00682733499522,
2.04410319658965,2.09170609555358,2.20196652287321,2.21156263283878,2.38645095865376,
2.4262977436429,2.47627536272184,2.49994037767516,2.51990878827355,2.54963638925063,
2.64660470158102,2.70100888497496,2.83927934713902,2.88231565042999,2.94654849259009,
2.98636707769959,3.02423146550515,3.07048235755101,3.2350934482223,3.39369887739012,
3.44487325321878,3.46873876266709,3.48865960655727,3.51801413236063,3.61008539349427,
3.63884740392259,3.79832223152826,3.84490066303349,3.9126982415971,3.95315885195754,
3.9911182407047,4.04446668963585,4.26578912901904,4.38780317245995,4.42363917301473,
4.44466319658567,4.46347704422078,4.4984722576448,4.60580792659009,4.64956654788277,
4.78128857765866,4.84332530544383,4.89666764583297,4.93462618020398,4.97508891347651,
5.04289805390158,5.12067555119254,5.29431532066301,5.3340291652571,5.35811064851171,
5.39332715136781,5.41423032493115,5.43314881398654,5.46873769315376,5.60051985904766,
5.74410091778763,5.78807956191048,5.85327424280867,5.89326621779936,5.9310319155375,
5.98557643098345,6.19521783291394,6.32471181045928,6.36136178221986,6.38254678536875,
6.4012367865757,6.43551841279528,6.63823198419296,6.73995614476405,6.81497027405884,
6.85670810204116,6.89423362662374,6.94350260917837,7.07638563387608,7.13509845021154,
7.29555995338409,7.33130216692823,7.35230776716117,7.37113680573451,7.40621880436233,
7.51474489469923,7.67485389935436,7.72152941057088,7.78942274470131,7.82990053763285,
7.86785210557337,7.92114844542685,8.14276439872491,8.26463458314003,8.30045442391829,
8.32147526494929,8.3402917050924,8.37530177149167,8.48284009898151,8.52633597229078,
8.6580785394766,8.69990422582333,8.76288722725818,8.80248121932488,8.84048811415104,
8.89655058126913,9.00383877176518,9.17237633495223,9.21153292551815,9.26093187098583,
9.28449872510489,9.30449296336996,9.33441247871471,9.43774001426987,9.60883250797868,
9.65711220598767,9.72657348511125,9.76733241057447,9.80516566371884,9.85765296710003,
10.1191234071707,10.1857677606014,10.2319131742954,10.2549109195941,10.2748552302506,
10.3057903605918,10.3801341012346,10.6562804474052,10.710663549089,10.7487816986966,
10.7889203435939,10.8549283417174,10.9369559331857,11.1098303728143,11.1494620486647,
11.1735085210119,11.2086883037301,11.2295844051551,11.2485094706637,11.2841352330492,
11.4158790133166,11.5594414126286,11.6034168628817,11.6686083556248,11.708599831746,
11.7463659613795,11.7921652693021,11.9369634128778,11.967222552164,12.0932113976351,
12.1612847697981,12.1875932308972,12.2072906505637),.UNSPECIFIED.) ;
#231 = B_SPLINE_CURVE_WITH_KNOTS('',3,(#26654,#26655,#26656,#26657,#26658,
#26659,#26660,#26661,#26662,#26663,#26664,#26665,#26666,#26667,#26668,#26669,
#26670,#26671,#26672,#26673,#26674,#26675,#26676,#26677,#26678,#26679,#26680,
#26681,#26682,#26683,#26684,#26685,#26686,#26687,#26688,#26689,#26690,#26691,
#26692,#26693,#26694,#26695,#26696,#26697,#26698,#26699,#26700,#26701,#26702,
#26703,#26704,#26705,#26706,#26707,#26708,#26709,#26710,#26711,#26712,#26713,
#26714,#26715,#26716,#26717,#26718,#26719,#26720,#26721,#26722,#26723,#26724,
#26725,#26726,#26727,#26728,#26729,#26730,#26731,#26732,#26733,#26734,#26735,
#26736,#26737,#26738,#26739,#26740,#26741,#26742,#26743,#26744,#26745,#26746,
#26747,#26748,#26749,#26750,#26751,#26752,#26753,#26754,#26755,#26756,#26757,
#26758,#26759,#26760,#26761,#26762,#26763,#26764,#26765,#26766,#26767,#26768,
#26769,#26770,#26771,#26772,#26773,#26774,#26775,#26776,#26777,#26778,#26779,
#26780,#26781,#26782,#26783,#26784,#26785,#26786,#26787,#26788,#26789,#26790,
#26791,#26792,#26793,#26794,#26795,#26796,#26797,#26798,#26799,#26800,#26801,
#26802,#26803,#26804,#26805,#26806,#26807,#26808,#26809,#26810,#26811,#26812,
#26813,#26814,#26815,#26816,#26817,#26818,#26819,#26820,#26821,#26822,#26823,
#26824,#26825,#26826,#26827,#26828,#26829,#26830,#26831,#26832,#26833,#26834,
#26835,#26836,#26837,#26838,#26839,#26840,#26841,#26842,#26843,#26844,#26845,
#26846,#26847,#26848,#26849,#26850,#26851,#26852,#26853,#26854,#26855,#26856,
#26857,#26858,#26859,#26860,#26861,#26862,#26863,#26864,#26865,#26866,#26867,
#26868,#26869,#26870,#26871,#26872,#26873,#26874,#26875,#26876,#26877,#26878,
#26879,#26880,#26881,#26882,#26883,#26884,#26885,#26886,#26887,#26888,#26889,
#26890,#26891,#26892,#26893,#26894,#26895,#26896,#26897,#26898,#26899,#26900,
#26901,#26902,#26903,#26904,#26905,#26906,#26907,#26908,#26909,#26910,#26911,
#26912,#26913,#26914,#26915,#26916,#26917,#26918,#26919,#26920,#26921,#26922,
#26923,#26924,#26925,#26926,#26927,#26928,#26929,#26930,#26931,#26932,#26933,
#26934,#26935,#26936,#26937,#26938,#26939,#26940,#26941,#26942,#26943,#26944,
#26945,#26946,#26947,#26948,#26949,#26950,#26951,#26952,#26953,#26954,#26955,
#26956,#26957,#26958,#26959,#26960,#26961,#26962,#26963,#26964,#26965,#26966,
#26967,#26968,#26969,#26970,#26971,#26972,#26973,#26974,#26975,#26976,#26977,
#26978,#26979,#26980,#26981,#26982,#26983,#26984,#26985,#26986,#26987,#26988,
#26989,#26990,#26991,#26992,#26993,#26994,#26995,#26996,#26997,#26998,#26999,
#27000,#27001,#27002,#27003),.UNSPECIFIED.,.F.,.F.,(4,2,2,2,2,2,2,2,2,2,
2,2,2,2,2,2,2,2,2,2,2,2,2,2,2,2,2,2,2,2,2,2,2,2,2,2,2,2,2,2,2,2,2,2,2,2,
2,2,2,2,2,2,2,2,2,2,2,2,2,2,2,2,2,2,2,2,2,2,2,2,2,2,2,2,2,2,2,2,2,2,2,2,
2,2,2,2,2,2,2,2,2,2,2,2,2,2,2,2,2,2,2,2,2,2,2,2,2,2,2,2,2,2,2,2,2,2,2,2,
2,2,2,2,2,2,2,2,2,2,2,2,2,2,2,2,2,2,2,2,2,2,2,2,2,2,2,2,2,2,2,2,2,2,2,2,
2,2,2,2,2,2,2,2,2,2,2,2,2,2,2,2,2,2,2,2,4),(8.71340497090936E-5,0.0431462393397145,
0.181910412010808,0.302714611116052,0.362072461948706,0.402214388992738,
0.437051944320088,0.474994746927191,0.528233256846255,0.75017799640711,
0.839953070808968,0.879482969901102,0.903609086629516,0.906634849381504,
0.909353999597516,0.912022049628397,0.915012628127877,0.934015672618608,
0.957952767559258,1.00558432627594,1.19433084553241,1.29030967439327,1.34272491498296,
1.38047054742223,1.39814501856307,1.43540911818344,1.48284794697211,1.58893166624209,
1.6654774828848,1.84253608693549,1.87753985098077,1.89840180679442,1.9173582960463,
1.95316163448382,2.08463940622617,2.22815983867,2.27212777975579,2.33731142170937,
2.37730117437565,2.41506759426198,2.46961832702716,2.67980497491144,2.80882575826391,
2.84542549106478,2.86660038316869,2.88529741711737,2.91962055116382,3.11215955905958,
3.21958255490145,3.2972448655286,3.3394372176361,3.37686277535162,3.42527526889042,
3.55407063353732,3.71894157041404,3.75768410043355,3.80673297543037,3.83023980332077,
3.85025024582739,3.88028896781445,3.99296148202705,4.1195876398833,4.20627884229904,
4.27375983542273,4.31416341062241,4.35214883047807,4.40567119924325,4.62603025926647,
4.7485091963076,4.78439713372531,4.80543129520775,4.82423668190984,4.85918389276147,
4.96586967618732,5.12744806913989,5.17434658198585,5.24245946577088,5.28297660984649,
5.32091045160027,5.37408840784635,5.59638784963516,5.71791751129297,5.75369900268019,
5.77471228137251,5.79353487511399,5.82858024712498,6.02815762939676,6.13083354153618,
6.20629762365978,6.24811322208642,6.28561983795941,6.33473477056653,6.46581316357391,
6.62742172267578,6.66578636547734,6.7145141712988,6.73796583700825,6.75799201983952,
6.78814321635514,6.89738942528884,7.06386478617193,7.1114877160055,7.18031033146228,
7.22095481272212,7.25883410989398,7.31164121235167,7.53638617710364,7.62500520997337,
7.66424512477582,7.69588958143311,7.71614459764995,7.73894444327569,7.78399561338899,
7.96463276113703,8.08637008875333,8.15208915214763,8.19217549882729,8.22989065090505,
8.27545264837787,8.51791709249546,8.59875626306783,8.65117096721831,8.67524022380368,
8.69511861441865,8.72411589629726,8.81249850409033,8.87080148252813,9.01319238265485,
9.05696315441157,9.12194654049746,9.16190046891161,9.19968719212972,9.2543668302558,
9.36551960605822,9.53340711272466,9.57249116503908,9.62182896216429,9.64538538638823,
9.66538245307504,9.69532268345045,9.79911773625038,9.99818357310984,10.0794701347149,
10.1222696918792,10.1595951438513,10.2070039239542,10.318236627621,10.3720808854931,
10.5110095745858,10.5606997473462,10.5982860122506,10.6196580071804,10.6382222380849,
10.6717632605593,10.877981421532,10.9785429751086,11.0137461608897,11.0696045947159,
11.1079593650195,11.1429607274567,11.2019041813594,11.3217285549136,11.4755952362156,
11.5276685515026,11.5665353112394,11.5881610618419,11.6065771347512,11.6392174588903,
11.7096407439587,11.9011260415366,12.00661533188,12.0529301905531,12.0865352830313,
12.1292147869275,12.207327736701),.UNSPECIFIED.) ;
#232 = B_SPLINE_CURVE_WITH_KNOTS('',3,(#27008,#27009,#27010,#27011,#27012,
#27013,#27014,#27015,#27016,#27017,#27018,#27019,#27020,#27021,#27022,#27023,
#27024,#27025,#27026,#27027,#27028,#27029,#27030,#27031,#27032,#27033,#27034,
#27035,#27036,#27037,#27038,#27039,#27040,#27041,#27042,#27043,#27044,#27045,
#27046,#27047,#27048,#27049,#27050,#27051,#27052,#27053,#27054,#27055,#27056,
#27057,#27058,#27059,#27060,#27061,#27062,#27063,#27064,#27065,#27066,#27067,
#27068,#27069,#27070,#27071,#27072,#27073,#27074,#27075,#27076,#27077,#27078,
#27079,#27080,#27081,#27082,#27083,#27084,#27085,#27086,#27087,#27088,#27089,
#27090,#27091,#27092,#27093,#27094,#27095,#27096,#27097,#27098,#27099,#27100,
#27101,#27102,#27103,#27104,#27105,#27106,#27107,#27108,#27109,#27110,#27111,
#27112,#27113,#27114,#27115,#27116,#27117,#27118,#27119,#27120,#27121,#27122,
#27123,#27124,#27125,#27126,#27127,#27128,#27129,#27130,#27131,#27132,#27133,
#27134,#27135,#27136,#27137,#27138,#27139,#27140,#27141,#27142,#27143,#27144,
#27145,#27146,#27147,#27148,#27149,#27150,#27151,#27152,#27153,#27154,#27155,
#27156,#27157,#27158,#27159,#27160,#27161,#27162,#27163,#27164,#27165,#27166,
#27167,#27168,#27169,#27170,#27171,#27172,#27173,#27174,#27175,#27176,#27177,
#27178,#27179,#27180,#27181,#27182,#27183,#27184,#27185,#27186,#27187,#27188,
#27189,#27190,#27191,#27192,#27193,#27194,#27195,#27196,#27197,#27198,#27199,
#27200,#27201,#27202,#27203,#27204,#27205,#27206,#27207,#27208,#27209,#27210,
#27211,#27212,#27213,#27214,#27215,#27216,#27217,#27218,#27219,#27220,#27221,
#27222,#27223,#27224,#27225,#27226,#27227,#27228,#27229,#27230,#27231,#27232,
#27233,#27234,#27235,#27236,#27237,#27238,#27239,#27240,#27241,#27242,#27243,
#27244,#27245,#27246,#27247,#27248,#27249,#27250,#27251,#27252,#27253,#27254,
#27255,#27256,#27257,#27258,#27259,#27260,#27261,#27262,#27263,#27264,#27265,
#27266,#27267,#27268,#27269,#27270,#27271,#27272,#27273,#27274,#27275,#27276,
#27277,#27278,#27279,#27280,#27281,#27282,#27283,#27284,#27285,#27286,#27287,
#27288,#27289,#27290,#27291,#27292,#27293,#27294,#27295,#27296,#27297,#27298,
#27299,#27300,#27301,#27302,#27303,#27304,#27305,#27306,#27307,#27308,#27309,
#27310,#27311,#27312,#27313,#27314,#27315,#27316,#27317,#27318,#27319,#27320,
#27321,#27322,#27323,#27324,#27325,#27326,#27327,#27328,#27329,#27330,#27331,
#27332,#27333,#27334,#27335,#27336,#27337,#27338,#27339,#27340,#27341,#27342,
#27343,#27344,#27345,#27346,#27347,#27348,#27349,#27350,#27351,#27352,#27353,
#27354,#27355,#27356,#27357,#27358,#27359,#27360,#27361,#27362,#27363,#27364,
#27365,#27366,#27367),.UNSPECIFIED.,.F.,.F.,(4,2,2,2,2,2,2,2,2,2,2,2,2,
2,2,2,2,2,2,2,2,2,2,2,2,2,2,2,2,2,2,2,2,2,2,2,2,2,2,2,2,2,2,2,2,2,2,2,2,
2,2,2,2,2,2,2,2,2,2,2,2,2,2,2,2,2,2,2,2,2,2,2,2,2,2,2,2,2,2,2,2,2,2,2,2,
2,2,2,2,2,2,2,2,2,2,2,2,2,2,2,2,2,2,2,2,2,2,2,2,2,2,2,2,2,2,2,2,2,2,2,2,
2,2,2,2,2,2,2,2,2,2,2,2,2,2,2,2,2,2,2,2,2,2,2,2,2,2,2,2,2,2,2,2,2,2,2,2,
2,2,2,2,2,2,2,2,2,2,2,2,2,2,2,2,2,2,2,2,2,2,4),(12.2075745498797,12.3262656338311,
12.3619799132888,12.3809205220066,12.40179923522,12.4368901463382,12.4608521887084,
12.5002863457929,12.6713410935888,12.7637780156581,12.8255142107852,12.8648847006477,
12.9035025005532,12.9609363993553,13.0297220988503,13.1940375782104,13.3065495849622,
13.3365851096342,13.3565950453348,13.380103289859,13.4291607943439,13.467913616835,
13.6328736557849,13.7611697099932,13.8097291715017,13.8471708606928,13.8892810420357,
13.9664617258692,14.0728304943579,14.2488431086171,14.2938968453501,14.3166970330802,
14.3369516420502,14.3685944472407,14.5180413907856,14.7142330118598,14.7701250277482,
14.8081039637735,14.8477388963176,14.9109518103223,14.9529991818009,15.0859152238612,
15.1049128584893,15.1375766918174,15.2448629786792,15.274923039628,15.2949363417486,
15.3184323560644,15.3674187760068,15.5294021536682,15.6932977991888,15.7397747005401,
15.7776888813061,15.8174246025427,15.8811988808129,15.9610349670388,16.0916551067236,
16.1219689559579,16.2152561674053,16.2447424284249,16.2646794758532,16.2884722309518,
16.3392109897658,16.4972951791983,16.6632894705936,16.7094587940107,16.7473047942463,
16.7871528141012,16.8515516277932,16.8947501342632,17.033921858492,17.0793243534708,
17.1831088277998,17.2132110703781,17.2332301097813,17.2567050186198,17.3055693841273,
17.3440948555309,17.5070834158003,17.6337430137899,17.6794338420895,17.7171759490474,
17.757209060919,17.8226357099702,17.8668435123017,18.0117523825704,18.0534922684096,
18.1530689629708,18.1827909262348,18.2027582911727,18.226425495008,18.2764177677676,
18.316282522179,18.4913421604818,18.510414580487,18.6123123496834,18.659436163935,
18.6966788096134,18.7402145210129,18.8260699123708,18.8931276785117,19.0197420309939,
19.1219162354014,19.1517788528257,19.1717649053111,19.1953594498315,19.2449236235016,
19.2842771920227,19.4545999815899,19.5512977124525,19.6113494801581,19.6465255305553,
19.6847274228018,19.7396467257866,19.905489994391,20.0840613813005,20.1174047867361,
20.1359356258587,20.1573598092236,20.1952103209491,20.2453889442275,20.387243261883,
20.4033374639141,20.5369441268338,20.58941456322,20.6272444503295,20.6680076236605,
20.7374977202671,20.7858078662379,20.9571258856279,21.0601566271548,21.0900615246835,
21.1100532790556,21.1336263041982,21.183064223829,21.2222677242819,21.3912314081192,
21.4959662401701,21.5529624231092,21.5876612035588,21.6263293809405,21.6840624487702,
21.7533530491582,21.9205065892055,22.0288939434272,22.0589958410839,22.0790146702706,
22.1024893564889,22.1513533254384,22.1898785245784,22.3528664700775,22.4795196019357,
22.5252113609124,22.5629533806562,22.602985521628,22.6684083890041,22.7126126667274,
22.8575022074562,22.9004294695854,22.9987949696125,23.028539523143,23.0485097053532,
23.0679043092712,23.0923169440898,23.1326322607895,23.2255946490421,23.4407720122268,
23.4938299072249,23.5312696663016,23.5658907766766,23.6114338851711,23.792588410267,
23.9590681836148,23.9932717857122,24.0119479115602,24.0300697997594,24.0516791077489,
24.0844064158757,24.1495428583943,24.4143137504503),.UNSPECIFIED.) ;
#233 = B_SPLINE_CURVE_WITH_KNOTS('',3,(#27368,#27369,#27370,#27371,#27372,
#27373,#27374,#27375,#27376,#27377,#27378,#27379,#27380,#27381,#27382,#27383,
#27384,#27385,#27386,#27387,#27388,#27389,#27390,#27391,#27392,#27393,#27394,
#27395,#27396,#27397,#27398,#27399,#27400,#27401,#27402,#27403,#27404,#27405,
#27406,#27407,#27408,#27409,#27410,#27411,#27412,#27413,#27414,#27415,#27416,
#27417,#27418,#27419,#27420,#27421,#27422,#27423,#27424,#27425,#27426,#27427,
#27428,#27429,#27430,#27431,#27432,#27433,#27434,#27435,#27436,#27437,#27438,
#27439,#27440,#27441,#27442,#27443,#27444,#27445,#27446,#27447,#27448,#27449,
#27450,#27451,#27452,#27453,#27454,#27455,#27456,#27457,#27458,#27459,#27460,
#27461,#27462,#27463,#27464,#27465,#27466,#27467,#27468,#27469,#27470,#27471,
#27472,#27473,#27474,#27475,#27476,#27477,#27478,#27479,#27480,#27481,#27482,
#27483,#27484,#27485,#27486,#27487,#27488,#27489,#27490,#27491,#27492,#27493,
#27494,#27495,#27496,#27497,#27498,#27499,#27500,#27501,#27502,#27503,#27504,
#27505,#27506,#27507,#27508,#27509,#27510,#27511,#27512,#27513,#27514,#27515,
#27516,#27517,#27518,#27519,#27520,#27521,#27522,#27523,#27524,#27525,#27526,
#27527,#27528,#27529,#27530,#27531,#27532,#27533,#27534,#27535,#27536,#27537,
#27538,#27539,#27540,#27541,#27542,#27543,#27544,#27545,#27546,#27547,#27548,
#27549,#27550,#27551,#27552,#27553,#27554,#27555,#27556,#27557,#27558,#27559,
#27560,#27561,#27562,#27563,#27564,#27565,#27566,#27567,#27568,#27569,#27570,
#27571,#27572,#27573,#27574,#27575,#27576,#27577,#27578,#27579,#27580,#27581,
#27582,#27583,#27584,#27585,#27586,#27587,#27588,#27589,#27590,#27591,#27592,
#27593,#27594,#27595,#27596,#27597,#27598,#27599,#27600,#27601,#27602,#27603,
#27604,#27605,#27606,#27607,#27608,#27609,#27610,#27611,#27612,#27613,#27614,
#27615,#27616,#27617,#27618,#27619,#27620,#27621,#27622,#27623,#27624,#27625,
#27626,#27627,#27628,#27629,#27630,#27631,#27632,#27633,#27634,#27635,#27636,
#27637,#27638,#27639,#27640,#27641,#27642,#27643,#27644,#27645,#27646,#27647,
#27648,#27649,#27650,#27651,#27652,#27653,#27654,#27655,#27656,#27657,#27658,
#27659,#27660,#27661,#27662,#27663,#27664,#27665,#27666,#27667,#27668,#27669,
#27670,#27671,#27672,#27673,#27674,#27675,#27676,#27677,#27678,#27679,#27680,
#27681,#27682,#27683,#27684,#27685,#27686,#27687,#27688,#27689,#27690,#27691,
#27692,#27693,#27694,#27695,#27696,#27697,#27698,#27699,#27700,#27701,#27702,
#27703,#27704,#27705,#27706,#27707,#27708,#27709,#27710,#27711,#27712,#27713,
#27714,#27715,#27716,#27717,#27718,#27719,#27720,#27721,#27722,#27723,#27724,
#27725,#27726,#27727,#27728,#27729,#27730,#27731,#27732,#27733),
 .UNSPECIFIED.,.F.,.F.,(4,2,2,2,2,2,2,2,2,2,2,2,2,2,2,2,2,2,2,2,2,2,2,2,
2,2,2,2,2,2,2,2,2,2,2,2,2,2,2,2,2,2,2,2,2,2,2,2,2,2,2,2,2,2,2,2,2,2,2,2,
2,2,2,2,2,2,2,2,2,2,2,2,2,2,2,2,2,2,2,2,2,2,2,2,2,2,2,2,2,2,2,2,2,2,2,2,
2,2,2,2,2,2,2,2,2,2,2,2,2,2,2,2,2,2,2,2,2,2,2,2,2,2,2,2,2,2,2,2,2,2,2,2,
2,2,2,2,2,2,2,2,2,2,2,2,2,2,2,2,2,2,2,2,2,2,2,2,2,2,2,2,2,2,2,2,2,2,2,2,
2,2,2,2,2,2,2,2,2,2,2,2,2,2,4),(12.207327736701,12.3178091535815,12.5100743794467,
12.5418117813965,12.5618825409038,12.5845557468051,12.6289149326578,12.6918105994009,
12.9520503301033,13.0079775049734,13.0459622936337,13.085588895521,13.1487545277891,
13.1907561957183,13.3234292736677,13.3484659519424,13.37024182797,13.4828099779603,
13.5128466304612,13.5328567817399,13.5563646121386,13.6054193728659,13.6441688869385,
13.8090993676656,13.9375679680787,13.9860769341604,14.0235131123492,14.0656514968094,
14.1429969316421,14.2497252201926,14.4266607863629,14.4707378225575,14.4933589249592,
14.5136928400826,14.5458095020569,14.6954878462602,14.8901329126284,14.9461938982554,
14.984200324635,15.0237942440784,15.0867781451114,15.1286048024763,15.2603535862527,
15.3037427392678,15.4113596570535,15.4463751684567,15.4651924629181,15.4862119103093,
15.5220252580706,15.6438389155786,15.8655708085405,15.9188467216112,15.9567949966148,
15.9972790931677,16.0652088532836,16.111921452303,16.2722757918865,16.3804874319662,
16.415546306964,16.4343711876278,16.4553814189954,16.4911478746352,16.6068788644865,
16.8368836909677,16.8892617473599,16.9270789901272,16.9678770350268,17.0375595302559,
17.0860681619753,17.258817442158,17.3025004445771,17.3677833610841,17.3939329753429,
17.4136347980508,17.4394477574176,17.5036765935167,17.6169356864953,17.6615704496211,
17.8084344473779,17.8547379396401,17.8926137546589,17.9324125853187,17.9965368067468,
18.039467367389,18.1771560689096,18.3176876765218,18.3533854613398,18.3723231472201,
18.3932050273094,18.4283122853703,18.6052107732637,18.682904262808,18.7877998404064,
18.8352429535751,18.8725072571318,18.9158161638107,19.0002408803156,19.1234292203653,
19.289575381956,19.3238163707776,19.3424992520199,19.3636936472215,19.40039159649,
19.4484575823164,19.5781284894148,19.6060531490213,19.7475213408503,19.7935510376247,
19.831366781637,19.8712681793573,19.9359616162522,19.9794480723337,20.1202300879615,
20.1576768412232,20.2668746076173,20.2970218335619,20.3170473471543,20.3405006672809,
20.389238701331,20.4276155161417,20.5893276240276,20.720276259877,20.7693910090018,
20.8068973726441,20.8487125732679,20.9241756589133,21.0268497502248,21.2264229268091,
21.2614680033038,21.2802904532003,21.3013035745517,21.3370848289635,21.4586135417284,
21.6809163642699,21.7340937384932,21.7720272702546,21.8125441664727,21.8806569094721,
21.9275554030667,22.0891358617711,22.1958129621524,22.230759234421,22.2495643634196,
22.2705985026272,22.3064868979792,22.4289711190001,22.6493206586609,22.702844768519,
22.7408302258397,22.7812327937582,22.7825642676513,22.7839416949544,22.7853787528071,
22.7868907252314,22.7884950545104,22.790212008366,22.7920655063888,22.7940841609254,
22.7963026032125,22.8443807907027,22.9266898391829,23.0405125053488,23.0594391175267,
23.165137508115,23.2000113966874,23.2188038453493,23.2330053580524,23.2596792309956,
23.3346895057409,23.4944949105014,23.6274693338759,23.6767372189328,23.714262211541,
23.7520563198239,23.7760108174523,23.8855779476864,24.1118905529006,24.1596988100813,
24.1832773027337,24.2025205472974,24.2228626976231,24.2521404093967,24.4143563453461),
 .UNSPECIFIED.) ;
#234 = B_SPLINE_CURVE_WITH_KNOTS('',3,(#27738,#27739,#27740,#27741,#27742,
#27743,#27744,#27745,#27746,#27747,#27748,#27749,#27750,#27751,#27752,#27753,
#27754,#27755,#27756,#27757,#27758,#27759,#27760,#27761,#27762,#27763,#27764,
#27765,#27766,#27767,#27768,#27769,#27770,#27771,#27772,#27773,#27774,#27775,
#27776,#27777,#27778,#27779,#27780,#27781,#27782,#27783,#27784,#27785,#27786,
#27787,#27788,#27789,#27790,#27791,#27792,#27793,#27794,#27795,#27796,#27797,
#27798,#27799,#27800,#27801,#27802,#27803,#27804,#27805,#27806,#27807,#27808,
#27809,#27810,#27811,#27812,#27813,#27814,#27815,#27816,#27817,#27818,#27819,
#27820,#27821,#27822,#27823,#27824,#27825,#27826,#27827,#27828,#27829,#27830,
#27831,#27832,#27833,#27834,#27835,#27836,#27837,#27838,#27839,#27840,#27841,
#27842,#27843,#27844,#27845,#27846,#27847,#27848,#27849,#27850,#27851,#27852,
#27853,#27854,#27855,#27856,#27857,#27858,#27859,#27860,#27861,#27862,#27863,
#27864,#27865,#27866,#27867,#27868,#27869,#27870,#27871,#27872,#27873,#27874,
#27875,#27876,#27877,#27878,#27879,#27880,#27881,#27882,#27883,#27884,#27885,
#27886,#27887,#27888,#27889,#27890,#27891,#27892,#27893,#27894,#27895,#27896,
#27897,#27898,#27899,#27900,#27901,#27902,#27903,#27904,#27905,#27906,#27907,
#27908,#27909,#27910,#27911,#27912,#27913,#27914,#27915,#27916,#27917,#27918,
#27919,#27920,#27921,#27922,#27923,#27924,#27925,#27926,#27927,#27928,#27929,
#27930,#27931,#27932,#27933,#27934,#27935,#27936,#27937,#27938,#27939,#27940,
#27941,#27942,#27943,#27944,#27945,#27946,#27947,#27948,#27949,#27950,#27951,
#27952,#27953,#27954,#27955,#27956,#27957,#27958,#27959,#27960,#27961,#27962,
#27963,#27964,#27965,#27966,#27967,#27968,#27969,#27970,#27971,#27972,#27973,
#27974,#27975,#27976,#27977,#27978,#27979,#27980,#27981,#27982,#27983,#27984,
#27985,#27986,#27987,#27988,#27989,#27990,#27991,#27992,#27993,#27994,#27995,
#27996,#27997,#27998,#27999,#28000,#28001,#28002,#28003,#28004,#28005,#28006,
#28007,#28008,#28009,#28010,#28011,#28012,#28013,#28014,#28015,#28016,#28017,
#28018,#28019,#28020,#28021,#28022,#28023,#28024,#28025,#28026,#28027,#28028,
#28029,#28030,#28031,#28032,#28033,#28034,#28035,#28036,#28037,#28038,#28039,
#28040,#28041,#28042,#28043,#28044,#28045,#28046,#28047,#28048,#28049,#28050,
#28051,#28052,#28053,#28054,#28055,#28056,#28057,#28058,#28059,#28060,#28061,
#28062,#28063,#28064,#28065,#28066,#28067,#28068,#28069,#28070,#28071,#28072,
#28073,#28074,#28075,#28076,#28077),.UNSPECIFIED.,.F.,.F.,(4,2,2,2,2,2,
2,2,2,2,2,2,2,2,2,2,2,2,2,2,2,2,2,2,2,2,2,2,2,2,2,2,2,2,2,2,2,2,2,2,2,2,
2,2,2,2,2,2,2,2,2,2,2,2,2,2,2,2,2,2,2,2,2,2,2,2,2,2,2,2,2,2,2,2,2,2,2,2,
2,2,2,2,2,2,2,2,2,2,2,2,2,2,2,2,2,2,2,2,2,2,2,2,2,2,2,2,2,2,2,2,2,2,2,2,
2,2,2,2,2,2,2,2,2,2,2,2,2,2,2,2,2,2,2,2,2,2,2,2,2,2,2,2,2,2,2,2,2,2,2,2,
2,2,2,2,2,2,2,2,2,2,2,2,2,2,2,2,2,2,2,4),(0.000300129334749554,0.170465605201082,
0.214637287488896,0.249980507413532,0.283690260726543,0.327926523715331,
0.418325202517395,0.625914115324944,0.710601461913576,0.734601505583537,
0.75288144025282,0.771791205841507,0.807331235707942,0.922372580218292,
1.07735723027461,1.14439175336905,1.19718502406728,1.23119397558456,1.26885562888494,
1.32272110109602,1.5663565353341,1.64165365566064,1.66583171542758,1.70114944642875,
1.72207220203394,1.74097283993035,1.77646121213289,1.89073012681927,2.06011175954378,
2.10136034790645,2.16374171685343,2.20322772394761,2.24130902597476,2.29782783579101,
2.44545568475422,2.58202574778774,2.63131319296772,2.66868035420441,2.69000854808319,
2.70860064223467,2.74230781710601,2.94717425486887,3.04830685954465,3.08364420536323,
3.13965165022443,3.17803074202575,3.21300556545503,3.27178104262712,3.42241596180073,
3.55322533087405,3.60149741138596,3.63830885096753,3.65952591970968,3.67819284370369,
3.71234052207645,3.91564545314322,4.03249736151204,4.09870746168942,4.1388821666574,
4.17655212825755,4.23047331559905,4.44721933963644,4.57194332415861,4.60807974270388,
4.62916280319412,4.65063485526444,4.68872480648082,4.92902139295812,5.00763059519555,
5.07072319130099,5.11033650613542,5.14832968813457,5.20430984495815,5.40572489476059,
5.54326374723279,5.57826773895211,5.59912968855381,5.61808604561732,5.65388889218677,
5.78536681143262,5.92888681078269,5.9728546110497,6.03803803799565,6.07802765170954,
6.11579393536218,6.17034446111403,6.37968776190185,6.50941613108775,6.54609055206226,
6.56728025879866,6.58596647804041,6.62022697135088,6.82302906606593,6.92472319746984,
6.99972276014687,7.04145772361579,7.07898338791301,7.12825652116853,7.2634165000218,
7.42149409749689,7.45943896159524,7.50780792108265,7.53119743466352,7.55124167182216,
7.58152106393081,7.69155709053772,7.8572732465834,7.90478559705969,7.97350007778487,
8.01412496788776,8.05201203658566,8.1048739416702,8.22460674778463,8.25994604508097,
8.39706702613442,8.44644900246894,8.48386757826114,8.50520594649681,8.52379124003589,
8.55745857534416,8.76303535135153,8.87912816591802,8.94501396227604,8.98513011922795,
9.02282939732705,9.06831763163212,9.20844413813766,9.23043327241713,9.3665852366911,
9.41580029743774,9.45312790975155,9.47444807492814,9.4930450945367,9.52678216465161,
9.70430907774216,9.86525919965067,9.92256964739479,9.96116636547169,10.0005632205022,
10.0624478544322,10.1545107458112,10.3256265502277,10.3650670819695,10.3890318007783,
10.4241255136066,10.4450047085898,10.4639446937056,10.4996558087116,10.618226283471,
10.7705657941295,10.8370779122678,10.8931514127444,10.9315410977742,10.9712236694182,
11.0347024647697,11.122825319912,11.2946224940449,11.3341372028636,11.3838368902229,
11.4074546806538,11.4274349945917,11.457253245552,11.5634988816045,11.7326325700872,
11.7806363762068,11.8498296065167,11.890540121213,11.9283917584273,11.9810105037408,
12.2075745498797),.UNSPECIFIED.) ;
#235 = B_SPLINE_CURVE_WITH_KNOTS('',3,(#28078,#28079,#28080,#28081,#28082,
#28083,#28084,#28085,#28086,#28087,#28088,#28089,#28090,#28091,#28092,#28093,
#28094,#28095,#28096,#28097,#28098,#28099,#28100,#28101,#28102,#28103,#28104,
#28105,#28106,#28107,#28108,#28109,#28110,#28111,#28112,#28113,#28114,#28115,
#28116,#28117,#28118,#28119,#28120,#28121,#28122,#28123,#28124,#28125,#28126,
#28127,#28128,#28129,#28130,#28131,#28132,#28133,#28134,#28135,#28136,#28137,
#28138,#28139,#28140,#28141,#28142,#28143,#28144,#28145,#28146,#28147,#28148,
#28149,#28150,#28151,#28152,#28153,#28154,#28155,#28156,#28157,#28158,#28159,
#28160,#28161,#28162,#28163,#28164,#28165,#28166,#28167,#28168,#28169,#28170,
#28171,#28172,#28173,#28174,#28175,#28176,#28177,#28178,#28179,#28180,#28181,
#28182,#28183,#28184,#28185,#28186,#28187,#28188,#28189,#28190,#28191,#28192,
#28193,#28194,#28195,#28196,#28197,#28198,#28199,#28200,#28201,#28202,#28203,
#28204,#28205,#28206,#28207,#28208,#28209,#28210,#28211,#28212,#28213,#28214,
#28215,#28216,#28217,#28218,#28219,#28220,#28221,#28222,#28223,#28224,#28225,
#28226,#28227,#28228,#28229,#28230,#28231,#28232,#28233,#28234,#28235,#28236,
#28237,#28238,#28239,#28240,#28241,#28242,#28243,#28244,#28245,#28246,#28247,
#28248,#28249,#28250,#28251,#28252,#28253,#28254,#28255,#28256,#28257,#28258,
#28259,#28260,#28261,#28262,#28263,#28264,#28265,#28266,#28267,#28268,#28269,
#28270,#28271,#28272,#28273,#28274,#28275,#28276,#28277,#28278,#28279,#28280,
#28281,#28282,#28283,#28284,#28285,#28286,#28287,#28288,#28289,#28290,#28291,
#28292,#28293,#28294,#28295,#28296,#28297,#28298,#28299,#28300,#28301,#28302,
#28303,#28304,#28305,#28306,#28307,#28308,#28309,#28310,#28311,#28312,#28313,
#28314,#28315,#28316,#28317,#28318,#28319,#28320,#28321,#28322,#28323,#28324,
#28325,#28326,#28327,#28328,#28329,#28330,#28331,#28332,#28333,#28334,#28335,
#28336,#28337,#28338,#28339,#28340,#28341,#28342,#28343,#28344,#28345,#28346,
#28347,#28348,#28349,#28350,#28351,#28352,#28353,#28354,#28355,#28356,#28357,
#28358,#28359,#28360,#28361,#28362,#28363,#28364,#28365,#28366,#28367,#28368,
#28369,#28370,#28371,#28372,#28373,#28374,#28375,#28376,#28377,#28378,#28379,
#28380,#28381,#28382,#28383,#28384,#28385,#28386,#28387,#28388,#28389,#28390,
#28391,#28392,#28393,#28394,#28395,#28396,#28397,#28398,#28399,#28400,#28401,
#28402,#28403,#28404,#28405,#28406,#28407,#28408,#28409,#28410,#28411,#28412,
#28413,#28414,#28415,#28416,#28417,#28418,#28419,#28420,#28421,#28422,#28423,
#28424,#28425,#28426,#28427,#28428,#28429,#28430,#28431,#28432,#28433,#28434,
#28435,#28436,#28437,#28438,#28439),.UNSPECIFIED.,.F.,.F.,(4,2,2,2,2,2,
2,2,2,2,2,2,2,2,2,2,2,2,2,2,2,2,2,2,2,2,2,2,2,2,2,2,2,2,2,2,2,2,2,2,2,2,
2,2,2,2,2,2,2,2,2,2,2,2,2,2,2,2,2,2,2,2,2,2,2,2,2,2,2,2,2,2,2,2,2,2,2,2,
2,2,2,2,2,2,2,2,2,2,2,2,2,2,2,2,2,2,2,2,2,2,2,2,2,2,2,2,2,2,2,2,2,2,2,2,
2,2,2,2,2,2,2,2,2,2,2,2,2,2,2,2,2,2,2,2,2,2,2,2,2,2,2,2,2,2,2,2,2,2,2,2,
2,2,2,2,2,2,2,2,2,2,2,2,2,2,2,2,2,2,2,2,2,2,2,2,2,2,2,2,2,2,4),(4.23208308298446E-5,
0.125359044082082,0.188807359086395,0.226619635936491,0.261894632939479,
0.301516669984305,0.364656721856589,0.61174494231358,0.701792257972909,
0.726120374666445,0.7443308594801,0.763137486151525,0.798091618841933,0.904870341165865,
1.06637480891283,1.1346478809672,1.18801517880547,1.22249963161744,1.26051544834448,
1.31423745572013,1.55868437822124,1.63369005301111,1.68361916086748,1.7072760983078,
1.72724677703,1.75699053571378,1.85474710861021,1.87800506345815,1.92125906900328,
2.08751035155991,2.1528800725541,2.19290369839278,2.23065248806155,2.27637097063721,
2.41948400187062,2.56957920845577,2.62107711579589,2.65963718064942,2.68120248947268,
2.69965185280298,2.73249751267298,2.91344854070258,3.07305960022707,3.13020302263844,
3.16877198440148,3.20820629324407,3.27029768947247,3.36184935782567,3.53305642683296,
3.57250728691684,3.59647654667502,3.63157520846381,3.65245561014531,3.67139515469671,
3.70710253008245,3.84781568567189,3.98538126159972,4.02828973948332,4.09239148125162,
4.13218662328738,4.17006543016343,4.21638090087466,4.36464709054382,4.40849224309567,
4.52130023446569,4.58538569184048,4.6111797275287,4.6308823001479,4.65705252053155,
4.72247211276768,4.79779163748163,4.91060303536709,4.99420300781514,5.0600341082905,
5.10014084484866,5.13784586064497,5.18335914962703,5.42701725234172,5.50720117219997,
5.55934285500671,5.58336772698827,5.60325506408137,5.63232890046331,5.72125832396878,
5.84828674542808,5.94848543588946,5.98360317020306,6.03936667202018,6.07770613764213,
6.1174675128258,6.18138062525257,6.26844950686896,6.44043502187367,6.47997068112303,
6.52968833490125,6.55330954558013,6.57328960624022,6.60310304900225,6.70924258213049,
6.76838856406456,6.89762208222835,6.93896693259228,7.00144919678329,7.04095371300572,
7.07902292296772,7.13546531115045,7.24171428897968,7.30926201508716,7.42686290205341,
7.45911835407648,7.47987746782347,7.51151874063607,7.53177340356168,7.55457489041168,
7.59963416754486,7.77566893744542,7.92260413226695,7.97807940928382,8.01637185866739,
8.05620748142914,8.12053330743185,8.20659960122973,8.37876032725485,8.41831494587016,
8.46804846269441,8.49167234136789,8.51165166613299,8.54145979676041,8.64720944667967,
8.66543450543302,8.6900939667173,8.83004828358448,8.87338770827212,8.93793126485065,
8.97780620088743,9.01563831209363,9.06174053721773,9.17318043634505,9.34743776759368,
9.38721780003057,9.43713997440076,9.46079587793659,9.48076705789845,9.5105134961185,
9.60872403283247,9.63158564408396,9.67396915947893,9.80444882423844,9.86619223250518,
9.91935329872147,9.95728516743988,9.99780902479776,10.0659565583404,10.1195530796605,
10.3124948241768,10.3954032270064,10.4233305459428,10.4431037317468,10.4678643137253,
10.5246840232667,10.7851174757713,10.8650978148507,10.907680974549,10.9450386874909,
10.9927901013387,11.1112053664767,11.2858111189896,11.3256282138407,11.3755813085676,
11.3992424135982,11.419212220799,11.4489485073966,11.5462389152137,11.5902958510401,
11.7351763810448,11.7793800795842,11.8448032398245,11.8848367095948,11.9225806732416,
11.9682756484446,12.2073821909332),.UNSPECIFIED.) ;
#236 = B_SPLINE_CURVE_WITH_KNOTS('',3,(#28444,#28445,#28446,#28447,#28448,
#28449,#28450,#28451,#28452,#28453,#28454,#28455,#28456,#28457,#28458,#28459,
#28460,#28461,#28462,#28463,#28464,#28465,#28466,#28467,#28468,#28469,#28470,
#28471,#28472,#28473,#28474,#28475,#28476,#28477,#28478,#28479,#28480,#28481,
#28482,#28483,#28484,#28485,#28486,#28487,#28488,#28489,#28490,#28491,#28492,
#28493,#28494,#28495,#28496,#28497,#28498,#28499,#28500,#28501,#28502,#28503,
#28504,#28505,#28506,#28507,#28508,#28509,#28510,#28511,#28512,#28513,#28514,
#28515,#28516,#28517,#28518,#28519,#28520,#28521,#28522,#28523,#28524,#28525,
#28526,#28527,#28528,#28529,#28530,#28531,#28532,#28533,#28534,#28535,#28536,
#28537,#28538,#28539,#28540,#28541,#28542,#28543,#28544,#28545,#28546,#28547,
#28548,#28549,#28550,#28551,#28552,#28553,#28554,#28555,#28556,#28557,#28558,
#28559,#28560,#28561,#28562,#28563,#28564,#28565,#28566,#28567,#28568,#28569,
#28570,#28571,#28572,#28573,#28574,#28575,#28576,#28577,#28578,#28579,#28580,
#28581,#28582,#28583,#28584,#28585,#28586,#28587,#28588,#28589,#28590,#28591,
#28592,#28593,#28594,#28595,#28596,#28597,#28598,#28599,#28600,#28601,#28602,
#28603,#28604,#28605,#28606,#28607,#28608,#28609,#28610,#28611,#28612,#28613,
#28614,#28615,#28616,#28617,#28618,#28619,#28620,#28621,#28622,#28623,#28624,
#28625,#28626,#28627,#28628,#28629,#28630,#28631,#28632,#28633,#28634,#28635,
#28636,#28637,#28638,#28639,#28640,#28641,#28642,#28643,#28644,#28645,#28646,
#28647,#28648,#28649,#28650,#28651,#28652,#28653,#28654,#28655,#28656,#28657,
#28658,#28659,#28660,#28661,#28662,#28663,#28664,#28665,#28666,#28667,#28668,
#28669,#28670,#28671,#28672,#28673,#28674,#28675,#28676,#28677,#28678,#28679,
#28680,#28681,#28682,#28683,#28684,#28685,#28686,#28687,#28688,#28689,#28690,
#28691,#28692,#28693,#28694,#28695,#28696,#28697,#28698,#28699,#28700,#28701,
#28702,#28703,#28704,#28705,#28706,#28707,#28708,#28709,#28710,#28711,#28712,
#28713,#28714,#28715,#28716,#28717,#28718,#28719,#28720,#28721,#28722,#28723,
#28724,#28725,#28726,#28727,#28728,#28729,#28730,#28731,#28732,#28733,#28734,
#28735,#28736,#28737,#28738,#28739,#28740,#28741,#28742,#28743,#28744,#28745,
#28746,#28747),.UNSPECIFIED.,.F.,.F.,(4,3,3,3,3,3,3,3,3,3,3,3,3,3,3,3,3,
3,3,3,3,3,3,3,3,3,3,3,3,3,3,3,3,3,3,3,3,3,3,3,3,3,3,3,3,3,3,3,3,3,3,3,3,
3,3,3,3,3,3,3,3,3,3,3,3,3,3,3,3,3,3,3,3,3,3,3,3,3,3,3,3,3,3,3,3,3,3,3,3,
3,3,3,3,3,3,3,3,3,3,3,3,4),(-48.0752879938944,-48.0111765274951,-47.9470448098061,
-47.8905217899249,-47.8281643396776,-47.7658541252663,-47.7035505977148,
-47.6412508565077,-47.5788536893674,-47.5165475572819,-47.4541048726142,
-47.3916621879465,-47.3293047376992,-47.266994523288,-47.2046909957368,
-47.1423912545299,-47.0799940873895,-47.0176879553043,-46.9552452706362,
-46.8928025859681,-46.8304451357208,-46.7681349213095,-46.7058313937583,
-46.643531652551,-46.5811344854107,-46.5188283533254,-46.4563856686576,
-46.3939429839897,-46.3315855337424,-46.2692753193313,-46.2069717917801,
-46.144672050573,-46.0822748834326,-46.0199687513474,-45.9575260666794,
-45.8950833820114,-45.8327259317641,-45.7704157173528,-45.7081121898015,
-45.6458124485943,-45.583415281454,-45.5211091493687,-45.4586664647008,
-45.396223780033,-45.3338663297857,-45.2715561153745,-45.2092525878232,
-45.1469528466161,-45.0845556794757,-45.0222495473905,-44.9598068627226,
-44.8973641780546,-44.8350067278073,-44.7726965133961,-44.7103929858449,
-44.6480932446378,-44.5856960774974,-44.5233899454122,-44.4609472607442,
-44.3985045760762,-44.3361471258289,-44.2738369114177,-44.2115333838663,
-44.1492336426592,-44.0868364755189,-44.0245303434336,-43.9620876587657,
-43.8996449740978,-43.8372875238505,-43.7749773094393,-43.712673781888,
-43.6503740406809,-43.5879768735405,-43.5256707414552,-43.4632280567873,
-43.4007853721194,-43.3384279218721,-43.2761177074608,-43.2138141799096,
-43.1515144387025,-43.0891172715621,-43.0268111394768,-42.9643684548089,
-42.901925770141,-42.8395683198937,-42.7772581054827,-42.7149545779317,
-42.6526548367248,-42.5902576695843,-42.527951537499,-42.4655088528309,
-42.4030661681627,-42.3407087179154,-42.2783985035042,-42.2160949759529,
-42.153795234746,-42.0913980676056,-42.0290919355203,-41.9666492508523,
-41.9042065661843,-41.8383523791251,-41.7921027231872),.UNSPECIFIED.) ;
#237 = B_SPLINE_CURVE_WITH_KNOTS('',3,(#28748,#28749,#28750,#28751,#28752,
#28753,#28754,#28755,#28756,#28757,#28758,#28759,#28760,#28761,#28762,#28763,
#28764,#28765,#28766,#28767,#28768,#28769,#28770,#28771,#28772,#28773,#28774,
#28775,#28776,#28777,#28778,#28779,#28780,#28781,#28782,#28783,#28784,#28785,
#28786,#28787,#28788,#28789,#28790,#28791,#28792,#28793,#28794,#28795,#28796,
#28797,#28798,#28799,#28800,#28801,#28802,#28803,#28804,#28805,#28806,#28807,
#28808,#28809,#28810,#28811,#28812,#28813,#28814,#28815,#28816,#28817,#28818,
#28819,#28820,#28821,#28822,#28823,#28824,#28825,#28826,#28827,#28828,#28829,
#28830,#28831,#28832,#28833,#28834,#28835,#28836,#28837,#28838,#28839,#28840,
#28841,#28842,#28843,#28844,#28845,#28846,#28847,#28848,#28849,#28850,#28851,
#28852,#28853,#28854,#28855,#28856,#28857,#28858,#28859,#28860,#28861,#28862,
#28863,#28864,#28865,#28866,#28867,#28868,#28869,#28870,#28871,#28872,#28873,
#28874,#28875,#28876,#28877,#28878,#28879,#28880,#28881,#28882,#28883,#28884,
#28885,#28886,#28887,#28888,#28889,#28890,#28891,#28892,#28893,#28894,#28895,
#28896,#28897,#28898,#28899,#28900,#28901,#28902,#28903,#28904,#28905,#28906,
#28907,#28908,#28909,#28910,#28911,#28912,#28913,#28914,#28915,#28916,#28917,
#28918,#28919,#28920,#28921,#28922,#28923,#28924,#28925,#28926,#28927,#28928,
#28929,#28930,#28931,#28932,#28933,#28934,#28935,#28936,#28937,#28938,#28939,
#28940,#28941,#28942,#28943,#28944,#28945,#28946,#28947,#28948,#28949,#28950,
#28951,#28952,#28953,#28954,#28955,#28956,#28957,#28958,#28959,#28960,#28961,
#28962,#28963,#28964,#28965,#28966,#28967,#28968,#28969,#28970,#28971,#28972,
#28973,#28974,#28975,#28976,#28977,#28978,#28979,#28980,#28981,#28982,#28983,
#28984,#28985,#28986,#28987,#28988,#28989,#28990,#28991,#28992,#28993,#28994,
#28995,#28996,#28997,#28998,#28999,#29000,#29001,#29002,#29003,#29004,#29005,
#29006,#29007,#29008,#29009,#29010,#29011,#29012,#29013,#29014,#29015,#29016,
#29017,#29018,#29019,#29020,#29021,#29022,#29023,#29024,#29025,#29026,#29027,
#29028,#29029,#29030,#29031,#29032,#29033,#29034,#29035,#29036,#29037,#29038,
#29039,#29040,#29041,#29042,#29043,#29044,#29045,#29046,#29047,#29048,#29049,
#29050,#29051,#29052,#29053,#29054,#29055,#29056,#29057,#29058,#29059,#29060,
#29061,#29062,#29063,#29064,#29065,#29066,#29067,#29068,#29069,#29070,#29071,
#29072,#29073,#29074,#29075,#29076,#29077,#29078,#29079,#29080,#29081,#29082,
#29083,#29084,#29085,#29086,#29087,#29088,#29089,#29090,#29091,#29092,#29093,
#29094,#29095,#29096,#29097,#29098,#29099,#29100,#29101,#29102,#29103,#29104,
#29105,#29106,#29107),.UNSPECIFIED.,.F.,.F.,(4,2,2,2,2,2,2,2,2,2,2,2,2,
2,2,2,2,2,2,2,2,2,2,2,2,2,2,2,2,2,2,2,2,2,2,2,2,2,2,2,2,2,2,2,2,2,2,2,2,
2,2,2,2,2,2,2,2,2,2,2,2,2,2,2,2,2,2,2,2,2,2,2,2,2,2,2,2,2,2,2,2,2,2,2,2,
2,2,2,2,2,2,2,2,2,2,2,2,2,2,2,2,2,2,2,2,2,2,2,2,2,2,2,2,2,2,2,2,2,2,2,2,
2,2,2,2,2,2,2,2,2,2,2,2,2,2,2,2,2,2,2,2,2,2,2,2,2,2,2,2,2,2,2,2,2,2,2,2,
2,2,2,2,2,2,2,2,2,2,2,2,2,2,2,2,2,2,2,2,2,2,4),(12.2073821909332,12.2335108175185,
12.3299598799027,12.359669725321,12.379636103873,12.4033111185916,12.4533462044853,
12.4932615289407,12.66879152795,12.6866512872709,12.7890113437492,12.8362015980871,
12.8734497250337,12.9169400247124,13.0025007637647,13.1285337363769,13.2892804868801,
13.3239529316366,13.3427106131057,13.3638055097289,13.4000005239578,13.6698456745913,
13.763805228594,13.8091048954636,13.846284188843,13.8913684087509,13.9875932290115,
14.1440986993087,14.1602490901029,14.2676653884496,14.2977332044632,14.3177478629965,
14.3412407243228,14.3902072356886,14.4288524664773,14.592872378819,14.7144029361213,
14.7666914242695,14.8044963844781,14.8453284056641,14.9151990047304,14.9639021863386,
15.1380718922427,15.2375839381707,15.2673088456427,15.2872770337817,15.3109437657025,
15.3609308073712,15.4007887503178,15.5757787134379,15.5801640021051,15.6932087792408,
15.7411479955948,15.7785240519513,15.8209922723131,15.9002867660881,16.0113452242571,
16.2016950323066,16.233895139588,16.2540426958676,16.2765450004068,16.3199810428799,
16.3523932020669,16.4709609251633,16.5407207889432,16.6301590977717,16.6931043977956,
16.7326916193452,16.7711479806587,16.8276208164989,16.9820013316163,17.1710067511695,
17.2031455466139,17.2232827939903,17.2458071437963,17.2893615554697,17.3506067208589,
17.5876451688366,17.6569439452046,17.6976736459204,17.735518169528,17.7880852689427,
17.9692824278461,18.1363571134062,18.1705080951362,18.1891756527205,18.210392060249,
18.247199862594,18.2954653410335,18.4262365426923,18.5742167558884,18.6343215100856,
18.6695067476063,18.7077031839726,18.7625828700015,18.7969096618638,18.8937932623165,
19.0205917530423,19.1147345320124,19.1442990317169,19.164246283408,19.1879975186905,
19.2384868622976,19.3968527023198,19.5628872508156,19.6090775458069,19.6469285652457,
19.6867696000186,19.7511273021494,19.7942853784863,19.9332309222493,19.9885447352403,
20.0837452695773,20.1133884240324,20.1333457652756,20.1570550352196,20.2072950257437,
20.2474569200636,20.4253465244089,20.5393278456696,20.5872168681035,20.624587592034,
20.6670854383346,20.7465582805782,20.8058214030132,20.9189734423972,20.952383185187,
21.0528086576659,21.0824986058953,21.1024619896055,21.1261464813385,21.1762398477189,
21.2162255841325,21.3924288319422,21.4236285255905,21.5174088990174,21.5626807125665,
21.5998592239767,21.6449692039608,21.7413815390771,21.8985009085148,21.9281635907577,
22.0222563778361,22.0518164267903,22.0717629267108,22.0955160994496,22.1460180188203,
22.3043673793578,22.4703984770611,22.5165870426842,22.5544373713324,22.5942784111169,
22.6586379002873,22.7017979415561,22.8407555262912,22.8954534513049,22.9911796912393,
23.0208541392432,23.0408153794863,23.0574552138452,23.0807058927684,23.1178562351819,
23.1984496194167,23.4275355100229,23.4830345879557,23.5208986404524,23.5544995671929,
23.6090937621864,23.6741041743715,23.8191415988856,23.8541325148862,23.9600830243459,
23.9898913709594,24.0098702272613,24.0284682795909,24.0524962523772,24.0917586445026,
24.1804682782649,24.3558152153503,24.41439747201),.UNSPECIFIED.) ;
#238 = B_SPLINE_CURVE_WITH_KNOTS('',3,(#29112,#29113,#29114,#29115,#29116,
#29117,#29118,#29119,#29120,#29121,#29122,#29123,#29124,#29125,#29126,#29127,
#29128,#29129,#29130,#29131,#29132,#29133,#29134,#29135,#29136,#29137,#29138,
#29139,#29140,#29141,#29142,#29143,#29144,#29145,#29146,#29147,#29148,#29149,
#29150,#29151,#29152,#29153,#29154,#29155,#29156,#29157,#29158,#29159,#29160,
#29161,#29162,#29163,#29164,#29165,#29166,#29167,#29168,#29169,#29170,#29171,
#29172,#29173,#29174,#29175,#29176,#29177,#29178,#29179,#29180,#29181,#29182,
#29183,#29184,#29185,#29186,#29187,#29188,#29189,#29190,#29191,#29192,#29193,
#29194,#29195,#29196,#29197,#29198,#29199,#29200,#29201,#29202,#29203,#29204,
#29205,#29206,#29207,#29208,#29209,#29210,#29211,#29212,#29213,#29214,#29215,
#29216,#29217,#29218,#29219,#29220,#29221,#29222,#29223,#29224,#29225,#29226,
#29227,#29228,#29229,#29230,#29231,#29232,#29233,#29234,#29235,#29236,#29237,
#29238,#29239,#29240,#29241,#29242,#29243,#29244,#29245,#29246,#29247,#29248,
#29249,#29250,#29251,#29252,#29253,#29254,#29255,#29256,#29257,#29258,#29259,
#29260,#29261,#29262,#29263,#29264,#29265,#29266,#29267,#29268,#29269,#29270,
#29271,#29272,#29273,#29274,#29275,#29276,#29277,#29278,#29279,#29280,#29281,
#29282,#29283,#29284,#29285,#29286,#29287,#29288,#29289,#29290,#29291,#29292,
#29293,#29294,#29295,#29296,#29297,#29298,#29299,#29300,#29301,#29302,#29303,
#29304,#29305,#29306,#29307,#29308,#29309,#29310,#29311,#29312,#29313,#29314,
#29315,#29316,#29317,#29318,#29319,#29320,#29321,#29322,#29323,#29324,#29325,
#29326,#29327,#29328,#29329,#29330,#29331,#29332,#29333,#29334,#29335,#29336,
#29337,#29338,#29339,#29340,#29341,#29342,#29343,#29344,#29345,#29346,#29347,
#29348,#29349,#29350,#29351,#29352,#29353,#29354,#29355,#29356,#29357,#29358,
#29359,#29360,#29361,#29362,#29363,#29364,#29365,#29366,#29367,#29368,#29369,
#29370,#29371,#29372,#29373,#29374,#29375,#29376,#29377,#29378,#29379,#29380,
#29381,#29382,#29383,#29384,#29385,#29386,#29387,#29388,#29389,#29390,#29391,
#29392,#29393,#29394,#29395,#29396,#29397,#29398,#29399,#29400,#29401,#29402,
#29403,#29404,#29405,#29406,#29407,#29408,#29409,#29410,#29411,#29412,#29413,
#29414,#29415),.UNSPECIFIED.,.F.,.F.,(4,3,3,3,3,3,3,3,3,3,3,3,3,3,3,3,3,
3,3,3,3,3,3,3,3,3,3,3,3,3,3,3,3,3,3,3,3,3,3,3,3,3,3,3,3,3,3,3,3,3,3,3,3,
3,3,3,3,3,3,3,3,3,3,3,3,3,3,3,3,3,3,3,3,3,3,3,3,3,3,3,3,3,3,3,3,3,3,3,3,
3,3,3,3,3,3,3,3,3,3,3,3,4),(-54.3584733375017,-54.2962473358395,-54.2340310509242,
-54.1718213867751,-54.1096152496348,-54.0474030002711,-53.9851897965479,
-53.9229636429728,-53.8768370136655,-53.8144795634182,-53.752169349007,
-53.6898658214558,-53.6275660802489,-53.5651689131085,-53.5028627810232,
-53.4404200963551,-53.3779774116871,-53.3156199614398,-53.2533097470287,
-53.1910062194775,-53.1287064782702,-53.0663093111299,-53.0040031790443,
-52.9415604943765,-52.8791178097087,-52.8167603594614,-52.7544501450502,
-52.6921466174993,-52.6298468762923,-52.5674497091518,-52.5051435770666,
-52.4427008923984,-52.3802582077303,-52.317900757483,-52.2555905430719,
-52.1932870155204,-52.1309872743138,-52.0685901071733,-52.0062839750878,
-51.9438412904198,-51.8813986057519,-51.8190411555046,-51.7567309410938,
-51.6944274135426,-51.6321276723354,-51.569730505195,-51.5074243731099,
-51.4449816884418,-51.3825390037736,-51.3201815535263,-51.2578713391152,
-51.1955678115636,-51.1332680703565,-51.0708709032162,-51.0085647711309,
-50.9461220864631,-50.8836794017952,-50.8213219515479,-50.7590117371368,
-50.6967082095859,-50.6344084683787,-50.5720113012383,-50.5097051691533,
-50.447262484485,-50.3848197998168,-50.3224623495695,-50.2601521351584,
-50.1978486076073,-50.1355488664007,-50.0731516992601,-50.0108455671745,
-49.9484028825064,-49.8859601978384,-49.8236027475911,-49.7612925331797,
-49.6989890056283,-49.6366892644216,-49.5742920972812,-49.5119859651957,
-49.4495432805279,-49.38710059586,-49.3247431456127,-49.2624329312014,-49.2001294036503,
-49.1378296624429,-49.0754324953026,-49.0131263632179,-48.9506836785498,
-48.8882409938817,-48.8258835436344,-48.7635733292232,-48.7012698016721,
-48.6389700604652,-48.5765728933247,-48.5142667612395,-48.4518240765714,
-48.3893813919033,-48.3269379190192,-48.264025446856,-48.2015992973433,
-48.138443663855,-48.0752880303667),.UNSPECIFIED.) ;
#239 = B_SPLINE_CURVE_WITH_KNOTS('',3,(#29416,#29417,#29418,#29419,#29420,
#29421,#29422,#29423,#29424,#29425,#29426,#29427,#29428,#29429,#29430,#29431,
#29432,#29433,#29434,#29435,#29436,#29437,#29438,#29439,#29440,#29441,#29442,
#29443,#29444,#29445,#29446,#29447,#29448,#29449,#29450,#29451,#29452,#29453,
#29454,#29455,#29456,#29457,#29458,#29459,#29460,#29461,#29462,#29463,#29464,
#29465,#29466,#29467,#29468,#29469,#29470,#29471,#29472,#29473,#29474,#29475,
#29476,#29477,#29478,#29479,#29480,#29481,#29482,#29483,#29484,#29485,#29486,
#29487,#29488,#29489,#29490,#29491,#29492,#29493,#29494,#29495,#29496,#29497,
#29498,#29499,#29500,#29501,#29502,#29503,#29504,#29505,#29506,#29507,#29508,
#29509,#29510,#29511,#29512,#29513,#29514,#29515,#29516,#29517,#29518,#29519,
#29520,#29521,#29522,#29523,#29524,#29525,#29526,#29527,#29528,#29529,#29530,
#29531,#29532,#29533,#29534,#29535,#29536,#29537,#29538,#29539,#29540,#29541,
#29542,#29543,#29544,#29545,#29546,#29547,#29548,#29549,#29550,#29551,#29552,
#29553,#29554,#29555,#29556,#29557,#29558,#29559,#29560,#29561,#29562,#29563,
#29564,#29565,#29566,#29567,#29568,#29569,#29570,#29571,#29572,#29573,#29574,
#29575,#29576,#29577,#29578,#29579,#29580,#29581,#29582,#29583,#29584,#29585,
#29586,#29587,#29588,#29589,#29590,#29591,#29592,#29593,#29594,#29595,#29596,
#29597,#29598,#29599,#29600,#29601,#29602,#29603,#29604,#29605,#29606,#29607,
#29608,#29609,#29610,#29611,#29612,#29613,#29614,#29615,#29616,#29617,#29618,
#29619,#29620,#29621,#29622,#29623,#29624,#29625,#29626,#29627,#29628,#29629,
#29630,#29631,#29632,#29633,#29634,#29635,#29636,#29637,#29638,#29639,#29640,
#29641,#29642,#29643,#29644,#29645,#29646,#29647,#29648,#29649,#29650,#29651,
#29652,#29653,#29654,#29655,#29656,#29657,#29658,#29659,#29660,#29661,#29662,
#29663,#29664,#29665,#29666,#29667,#29668,#29669,#29670,#29671,#29672,#29673,
#29674,#29675,#29676,#29677,#29678,#29679,#29680,#29681,#29682,#29683,#29684,
#29685,#29686,#29687,#29688,#29689,#29690,#29691,#29692,#29693,#29694,#29695,
#29696,#29697,#29698,#29699,#29700,#29701,#29702,#29703,#29704,#29705,#29706,
#29707,#29708,#29709,#29710,#29711,#29712,#29713,#29714,#29715,#29716,#29717,
#29718,#29719,#29720,#29721,#29722,#29723,#29724,#29725,#29726,#29727,#29728,
#29729,#29730,#29731,#29732,#29733,#29734,#29735,#29736,#29737,#29738,#29739,
#29740,#29741,#29742,#29743,#29744,#29745,#29746,#29747,#29748,#29749,#29750,
#29751,#29752,#29753,#29754,#29755,#29756,#29757,#29758,#29759,#29760,#29761,
#29762,#29763,#29764,#29765,#29766,#29767,#29768,#29769,#29770,#29771,#29772,
#29773,#29774,#29775,#29776,#29777,#29778,#29779,#29780,#29781,#29782,#29783,
#29784,#29785,#29786,#29787,#29788,#29789,#29790,#29791,#29792,#29793,#29794,
#29795,#29796,#29797,#29798,#29799,#29800,#29801,#29802,#29803,#29804,#29805,
#29806,#29807,#29808,#29809),.UNSPECIFIED.,.F.,.F.,(4,2,2,2,2,2,2,2,2,2,
2,2,2,2,2,2,2,2,2,2,2,2,2,2,2,2,2,2,2,2,2,2,2,2,2,2,2,2,2,2,2,2,2,2,2,2,
2,2,2,2,2,2,2,2,2,2,2,2,2,2,2,2,2,2,2,2,2,2,2,2,2,2,2,2,2,2,2,2,2,2,2,2,
2,2,2,2,2,2,2,2,2,2,2,2,2,2,2,2,2,2,2,2,2,2,2,2,2,2,2,2,2,2,2,2,2,2,2,2,
2,2,2,2,2,2,2,2,2,2,2,2,2,2,2,2,2,2,2,2,2,2,2,2,2,2,2,2,2,2,2,2,2,2,2,2,
2,2,2,2,2,2,2,2,2,2,2,2,2,2,2,2,2,2,2,2,2,2,2,2,2,2,2,2,2,2,2,2,2,2,2,2,
2,2,2,2,2,2,4),(8.42914463236037E-5,0.0379717091092616,0.0736004856464233,
0.111473526474535,0.167020001785984,0.317233552160938,0.505139405702036,
0.534949880889817,0.55357464234073,0.573529591958853,0.603153569578424,
0.698067353575928,0.824841874188393,0.921254879414346,0.973802149138873,
1.01159198463408,1.04328096525734,1.08124253197859,1.13727922809431,1.31362105569038,
1.42846726630663,1.47367222863448,1.475123949699,1.47616049958101,1.47826043255324,
1.48011910574621,1.48176445634631,1.48322140215602,1.48451207107788,1.4856560462315,
1.48667061299986,1.48757099891463,1.48837060052546,1.48908119374871,1.48971312584074,
1.49027548848422,1.49077627235489,1.49122250407503,1.49162036687352,1.49197530637639,
1.4922921231375,1.49257505325408,1.49282783861581,1.49356172595305,1.49426540413618,
1.51454008506316,1.52896115409072,1.54771820193755,1.58238781940073,1.743496899363,
1.92963920949245,1.98222828653364,2.02007603697584,2.06079794993105,2.13005292476935,
2.36715764379405,2.42840755269984,2.47196437793416,2.49448920784632,2.51462629013244,
2.54676395544301,2.73577335762321,2.89015668344801,2.94663001587642,2.98508651664267,
3.02467371278034,3.0876186215798,3.17705649078552,3.34862863024698,3.38811925433987,
3.43779904785868,3.46141373843161,3.48139534210748,3.51122103003068,3.61278413786048,
3.81457167343543,3.89570451511808,3.93847874779858,3.9758077862152,4.02325584262599,
4.13461652018255,4.14179323143894,4.31696781496736,4.35684517903941,4.40684849789668,
4.43051802538501,4.45048558308685,4.48020536235353,4.57988215993593,4.630397590054,
4.76945331042978,4.81263152939806,4.87701005759037,4.91685518757331,4.95470452532019,
5.0008856662727,5.16690394656811,5.32514240431074,5.37574589160291,5.3995164322811,
5.41945938440006,5.44898877434882,5.54272584624629,5.59981405266092,5.73872353145172,
5.78187549420257,5.84622720775365,5.88606762328978,5.92391998744518,5.97011438487237,
6.13615207424831,6.29455448153151,6.3450121274628,6.36875828692691,6.38870716422874,
6.41828234765136,6.51254958461194,6.56898841175525,6.7079126232618,6.75106731360748,
6.81542190354679,6.85526295200383,6.89311519239849,6.93930851464101,7.10534542211121,
7.2637337335032,7.28812340851755,7.3236626930908,7.34462883399883,7.36349196989876,
7.39876669505061,7.59746873301997,7.70040152346541,7.77598702393112,7.81782410906911,
7.85532652117246,7.90440190090633,8.03097055259366,8.19623428326075,8.23502212293775,
8.28410973392786,8.30762352669691,8.32763259646727,8.35765893967885,8.46955534934651,
8.59617419100339,8.68328405047701,8.75098629434154,8.79143024598732,8.82939818498459,
8.88280028053755,9.10383230051427,9.22599132024928,9.26184394033772,9.28287146140896,
9.30168304254138,9.33666410090269,9.44380113818884,9.60502335128768,9.65186851590099,
9.71992938011551,9.76043778765256,9.79837669551035,9.85158440980379,10.0737203701549,
10.1953370549295,10.2311288128344,10.2521444038105,10.2709658545005,10.3060031643562,
10.5056190625521,10.6082871429532,10.6837481119395,10.7255637860518,10.7630713946087,
10.812188969959,10.9438134631646,11.1049940917399,11.1433088797067,11.1919945336148,
11.2154392507245,11.235468013524,11.2656351550321,11.3750567230316,11.4127992358692,
11.553222914681,11.5966462616358,11.6612757849033,11.7011664832244,11.7389900921116,
11.7850521901086,11.9269428949954,12.0772646034911,12.1287980077517,12.1673772153281,
12.1889465269692,12.2073941385125),.UNSPECIFIED.) ;
#240 = B_SPLINE_CURVE_WITH_KNOTS('',3,(#29814,#29815,#29816,#29817,#29818,
#29819,#29820,#29821,#29822,#29823,#29824,#29825,#29826,#29827,#29828,#29829,
#29830,#29831,#29832,#29833,#29834,#29835,#29836,#29837,#29838,#29839,#29840,
#29841,#29842,#29843,#29844,#29845,#29846,#29847,#29848,#29849,#29850,#29851,
#29852,#29853,#29854,#29855,#29856,#29857,#29858,#29859,#29860,#29861,#29862,
#29863,#29864,#29865,#29866,#29867,#29868,#29869,#29870,#29871,#29872,#29873,
#29874,#29875,#29876,#29877,#29878,#29879,#29880,#29881,#29882,#29883,#29884,
#29885,#29886,#29887,#29888,#29889,#29890,#29891,#29892,#29893,#29894,#29895,
#29896,#29897,#29898,#29899,#29900,#29901,#29902,#29903,#29904,#29905,#29906,
#29907,#29908,#29909,#29910,#29911,#29912,#29913,#29914,#29915,#29916,#29917,
#29918,#29919,#29920,#29921,#29922,#29923,#29924,#29925,#29926,#29927,#29928,
#29929,#29930,#29931,#29932,#29933,#29934,#29935,#29936,#29937,#29938,#29939,
#29940,#29941,#29942,#29943,#29944,#29945,#29946,#29947,#29948,#29949,#29950,
#29951,#29952,#29953,#29954,#29955,#29956,#29957,#29958,#29959,#29960,#29961,
#29962,#29963,#29964,#29965,#29966,#29967,#29968,#29969,#29970,#29971,#29972,
#29973,#29974,#29975,#29976,#29977,#29978,#29979,#29980,#29981,#29982,#29983,
#29984,#29985,#29986,#29987,#29988,#29989,#29990,#29991,#29992,#29993,#29994,
#29995,#29996,#29997,#29998,#29999,#30000,#30001,#30002,#30003,#30004,#30005,
#30006,#30007,#30008,#30009,#30010,#30011,#30012,#30013,#30014,#30015,#30016,
#30017,#30018,#30019,#30020,#30021,#30022,#30023,#30024,#30025,#30026,#30027,
#30028,#30029,#30030,#30031,#30032,#30033,#30034,#30035,#30036,#30037,#30038,
#30039,#30040,#30041,#30042,#30043,#30044,#30045,#30046,#30047,#30048,#30049,
#30050,#30051,#30052,#30053,#30054,#30055,#30056,#30057,#30058,#30059,#30060,
#30061,#30062,#30063,#30064,#30065,#30066,#30067,#30068,#30069,#30070,#30071,
#30072,#30073,#30074,#30075,#30076,#30077,#30078,#30079,#30080,#30081,#30082,
#30083,#30084,#30085,#30086,#30087,#30088,#30089,#30090,#30091,#30092,#30093,
#30094,#30095,#30096,#30097,#30098,#30099,#30100,#30101,#30102,#30103,#30104,
#30105,#30106,#30107,#30108,#30109,#30110,#30111,#30112,#30113,#30114,#30115,
#30116,#30117,#30118,#30119,#30120,#30121,#30122,#30123,#30124,#30125,#30126,
#30127,#30128,#30129,#30130,#30131,#30132,#30133,#30134,#30135,#30136,#30137,
#30138,#30139,#30140,#30141,#30142,#30143,#30144,#30145,#30146,#30147,#30148,
#30149,#30150,#30151,#30152,#30153,#30154,#30155,#30156,#30157,#30158,#30159,
#30160,#30161,#30162,#30163,#30164,#30165,#30166,#30167,#30168,#30169,#30170,
#30171,#30172,#30173,#30174,#30175,#30176,#30177,#30178,#30179,#30180,#30181,
#30182,#30183,#30184,#30185,#30186,#30187,#30188,#30189,#30190,#30191),
 .UNSPECIFIED.,.F.,.F.,(4,2,2,2,2,2,2,2,2,2,2,2,2,2,2,2,2,2,2,2,2,2,2,2,
2,2,2,2,2,2,2,2,2,2,2,2,2,2,2,2,2,2,2,2,2,2,2,2,2,2,2,2,2,2,2,2,2,2,2,2,
2,2,2,2,2,2,2,2,2,2,2,2,2,2,2,2,2,2,2,2,2,2,2,2,2,2,2,2,2,2,2,2,2,2,2,2,
2,2,2,2,2,2,2,2,2,2,2,2,2,2,2,2,2,2,2,2,2,2,2,2,2,2,2,2,2,2,2,2,2,2,2,2,
2,2,2,2,2,2,2,2,2,2,2,2,2,2,2,2,2,2,2,2,2,2,2,2,2,2,2,2,2,2,2,2,2,2,2,2,
2,2,2,2,2,2,2,2,2,2,2,2,2,2,2,2,2,2,2,2,4),(12.2074643523629,12.2510803881761,
12.2883180320074,12.3353371243011,12.4466774321583,12.6682126897982,12.7204788088286,
12.7445241480605,12.7624004881259,12.7898456193121,12.8678923586911,13.0347194994456,
13.1521854717311,13.2047004583025,13.2425381103645,13.2832878345502,13.3526954514402,
13.4009193969484,13.5716118896449,13.6758492046428,13.7056014738285,13.72557350327,
13.7492265568158,13.7991314627909,13.8388907598491,14.0129509107426,14.0976376388995,
14.1614522369843,14.2011960752979,14.2395472969524,14.2953814613993,14.3305625597964,
14.4310296607404,14.637522630409,14.6710105909773,14.6895661291709,14.7109526919714,
14.7486110615429,14.7984339371305,14.9381464093486,15.0815732664283,15.1381033189386,
15.1761870585934,15.2156715395401,15.2780412003025,15.3553589401022,15.5816945830979,
15.6294915144264,15.6530683724527,15.6730604222033,15.7029616079101,15.813172166321,
16.054776135241,16.1095205494218,16.1473178936361,16.1872547210646,16.252140473882,
16.295814959929,16.437656944076,16.5719371037958,16.6075966722555,16.6265279426321,
16.6474179656736,16.682565196325,16.7065805514402,16.7461389990475,16.9183306199123,
17.0042489247897,17.0686379592868,17.1084853493193,17.1467713642115,17.2022045788382,
17.2370257813654,17.5022201977551,17.5612904440889,17.5870846028357,17.6067822251668,
17.6329485882213,17.6998887355955,17.8219833864515,17.8374754768821,17.9940003069029,
18.0484104745623,18.0861561469217,18.1261879729017,18.1915998603211,18.2357920985166,
18.3806051357199,18.4299954355254,18.5227153760692,18.5521439148391,18.5720743712274,
18.5959001827515,18.6468333446375,18.805055771765,18.9707261747319,19.0168654435275,
19.0547059901497,19.0945676323238,19.1590356171313,19.202300884865,19.341840284446,
19.3736248368375,19.4808515432485,19.5158392026574,19.5346519865175,19.5556781893222,
19.5915238804521,19.7136200462538,19.9347883507604,19.9881669652328,20.0261314839503,
20.0665833334768,20.1343290372588,20.2215211384079,20.3481368979375,20.4573827572483,
20.488607745454,20.5085968812826,20.531473449926,20.5769455195891,20.6421622662813,
20.8944472580128,20.9521848115145,20.9869984733818,21.0255408652821,21.0825251729922,
21.2408749872914,21.4235403121264,21.4563279828499,21.4747680524404,21.4963505854128,
21.5349972264426,21.5866571617766,21.737799702797,21.8788098486998,21.9248047933719,
21.9626135807268,22.0025295478043,22.0673003824412,22.1108622458796,22.2520671713703,
22.2707721174684,22.3881315118216,22.4233417510973,22.4421935090534,22.4631728105367,
22.4987796572793,22.52323410308,22.6814825622351,22.847505797266,22.8936874985564,
22.9315371282327,22.9669806785719,22.9685774877449,22.9702809011894,22.9721163437289,
22.9741135066938,22.976307552976,22.978740559645,22.9814632409231,22.9845369755012,
22.9880361193795,22.9920504992698,22.996687822658,22.9987967732181,23.0019792913726,
23.1299912527637,23.237551300046,23.3568775224537,23.3916479673123,23.406909112261,
23.4214491618102,23.4406719877125,23.4667344349675,23.5116352457113,23.6250013681698,
23.6699341512628,23.8162833611432,23.8626152147707,23.9004979981165,23.9353795627966,
23.974761624626,24.1173917648754,24.3050605783251,24.3522425303142,24.3759138015097,
24.3947801408357,24.4149503713271),.UNSPECIFIED.) ;
#241 = B_SPLINE_CURVE_WITH_KNOTS('',3,(#30192,#30193,#30194,#30195,#30196,
#30197,#30198,#30199,#30200,#30201,#30202,#30203,#30204,#30205,#30206,#30207,
#30208,#30209,#30210,#30211,#30212,#30213,#30214,#30215,#30216,#30217,#30218,
#30219,#30220,#30221,#30222,#30223,#30224,#30225,#30226,#30227,#30228,#30229,
#30230,#30231,#30232,#30233,#30234,#30235,#30236,#30237,#30238,#30239,#30240,
#30241,#30242,#30243,#30244,#30245,#30246,#30247,#30248,#30249,#30250,#30251,
#30252,#30253,#30254,#30255,#30256,#30257,#30258,#30259,#30260,#30261,#30262,
#30263,#30264,#30265,#30266,#30267,#30268,#30269,#30270,#30271,#30272,#30273,
#30274,#30275,#30276,#30277,#30278,#30279,#30280,#30281,#30282,#30283,#30284,
#30285,#30286,#30287,#30288,#30289,#30290,#30291,#30292,#30293,#30294,#30295,
#30296,#30297,#30298,#30299,#30300,#30301,#30302,#30303,#30304,#30305,#30306,
#30307,#30308,#30309,#30310,#30311,#30312,#30313,#30314,#30315,#30316,#30317,
#30318,#30319,#30320,#30321,#30322,#30323,#30324,#30325,#30326,#30327,#30328,
#30329,#30330,#30331,#30332,#30333,#30334,#30335,#30336,#30337,#30338,#30339,
#30340,#30341,#30342,#30343,#30344,#30345,#30346,#30347,#30348,#30349,#30350,
#30351,#30352,#30353,#30354,#30355,#30356,#30357,#30358,#30359,#30360,#30361,
#30362,#30363,#30364,#30365,#30366,#30367,#30368,#30369,#30370,#30371,#30372,
#30373,#30374,#30375,#30376,#30377,#30378,#30379,#30380,#30381,#30382,#30383,
#30384,#30385,#30386,#30387,#30388,#30389,#30390,#30391,#30392,#30393,#30394,
#30395,#30396,#30397,#30398,#30399,#30400,#30401,#30402,#30403,#30404,#30405,
#30406,#30407,#30408,#30409,#30410,#30411,#30412,#30413,#30414,#30415,#30416,
#30417,#30418,#30419,#30420,#30421,#30422,#30423,#30424,#30425,#30426,#30427,
#30428,#30429,#30430,#30431,#30432,#30433,#30434,#30435,#30436,#30437,#30438,
#30439,#30440,#30441,#30442,#30443,#30444,#30445,#30446,#30447,#30448,#30449,
#30450,#30451,#30452,#30453,#30454,#30455,#30456,#30457,#30458,#30459,#30460,
#30461,#30462,#30463,#30464,#30465,#30466,#30467,#30468,#30469,#30470,#30471,
#30472,#30473,#30474,#30475,#30476,#30477,#30478,#30479,#30480,#30481,#30482,
#30483,#30484,#30485,#30486,#30487,#30488,#30489,#30490,#30491,#30492,#30493,
#30494,#30495,#30496,#30497,#30498,#30499,#30500,#30501,#30502,#30503,#30504,
#30505,#30506,#30507,#30508,#30509,#30510,#30511,#30512,#30513,#30514,#30515,
#30516,#30517,#30518,#30519,#30520,#30521,#30522,#30523,#30524,#30525,#30526,
#30527,#30528,#30529,#30530,#30531,#30532,#30533,#30534,#30535,#30536,#30537,
#30538,#30539,#30540,#30541,#30542,#30543,#30544,#30545,#30546,#30547,#30548,
#30549,#30550,#30551,#30552,#30553,#30554,#30555,#30556,#30557,#30558,#30559,
#30560,#30561,#30562,#30563,#30564,#30565,#30566,#30567,#30568,#30569,#30570,
#30571,#30572,#30573,#30574,#30575,#30576,#30577,#30578,#30579,#30580,#30581,
#30582,#30583,#30584,#30585,#30586,#30587,#30588,#30589,#30590,#30591,#30592,
#30593,#30594,#30595),.UNSPECIFIED.,.F.,.F.,(4,2,2,2,2,2,2,2,2,2,2,2,2,
2,2,2,2,2,2,2,2,2,2,2,2,2,2,2,2,2,2,2,2,2,2,2,2,2,2,2,2,2,2,2,2,2,2,2,2,
2,2,2,2,2,2,2,2,2,2,2,2,2,2,2,2,2,2,2,2,2,2,2,2,2,2,2,2,2,2,2,2,2,2,2,2,
2,2,2,2,2,2,2,2,2,2,2,2,2,2,2,2,2,2,2,2,2,2,2,2,2,2,2,2,2,2,2,2,2,2,2,2,
2,2,2,2,2,2,2,2,2,2,2,2,2,2,2,2,2,2,2,2,2,2,2,2,2,2,2,2,2,2,2,2,2,2,2,2,
2,2,2,2,2,2,2,2,2,2,2,2,2,2,2,2,2,2,2,2,2,2,2,2,2,2,2,2,2,2,2,2,2,2,2,2,
2,2,2,2,2,2,2,2,4),(12.2073941385125,12.2402277463726,12.2620763310274,
12.3272670935593,12.5802781988266,12.6376944261202,12.672458709584,12.7110554746234,
12.7683607958391,12.929260864507,13.1070412498584,13.1406838558017,13.1592653645263,
13.1806110691908,13.2180644095471,13.2675098091101,13.4049956667988,13.4603376119083,
13.5718096540163,13.6192907211529,13.6566232879607,13.6993774303379,13.7803859555984,
13.985102861166,14.0841261389353,14.1138642469289,14.133834455417,14.1574949936934,
14.2074438455509,14.2472556898354,14.4218081857704,14.5402824015585,14.5880396880502,
14.6253982920502,14.6679785308719,14.7479397534326,15.0101718030228,15.0650846189291,
15.0898977721188,15.1094767154397,15.1371860434586,15.2178389622492,15.3979808805493,
15.5099669470672,15.557576848642,15.5949215325385,15.637594074765,15.7181090672836,
15.8319512896149,16.0170989026736,16.0495351425806,16.0697231547625,16.0921431083163,
16.1351367198853,16.1952448931677,16.4184621045062,16.4961897031074,16.5388011696546,
16.5724162675553,16.6188316749206,16.7251238282469,16.9202378288812,16.9373526937547,
16.9997737458706,17.0257826125564,17.0454821922326,17.0714327270402,17.1366993754574,
17.2532640785524,17.3156173902785,17.4401716471949,17.4864430803509,17.5243127165114,
17.5641251944169,17.6283200941376,17.6713188645151,17.8093800675466,17.8327271117422,
17.9498780016721,17.9852861878183,18.0041729606285,18.0251123281562,18.0605137665094,
18.0847715613042,18.1248997809032,18.3024587782809,18.4169858554173,18.4648290923152,
18.5021962697318,18.544724127103,18.6243709266633,18.6838364470958,18.8196312704273,
18.9292916969126,18.9594869148141,18.9795196804231,19.0029508627655,19.0515578999591,
19.0897805304463,19.2501783583851,19.3827794571685,19.4319061182526,19.4694148995634,
19.5112260819638,19.5866607633317,19.6892728136684,19.8890747185072,19.9240638087518,
19.9428768412877,19.9639027354199,19.9997468652963,20.1218291408583,20.3430258769336,
20.396399366038,20.4343631114911,20.4748166376966,20.5425716953716,20.6297815788976,
20.756396931293,20.8659003903521,20.8969824554747,20.9169494013343,20.9398852354991,
20.9856854428877,21.051595639326,21.2372716604169,21.3338551891554,21.3789900859218,
21.4161695752109,21.4614187244392,21.5588225609816,21.7192223136479,21.8273847351294,
21.8624407136265,21.8812654043188,21.902276959806,21.9380483773288,21.9626607089466,
22.1208406636643,22.2865907302731,22.3327294816639,22.3705697553468,22.4104312634578,
22.4748994070042,22.5181649442971,22.6577064435626,22.6894020266327,22.7967023059467,
22.8316952164351,22.8505088468344,22.8647992054061,22.8839837746901,22.8845685791001,
22.8851763591001,22.8858084486113,22.8864662668027,22.8871513239457,22.8878652276767,
22.8886096896721,22.8893865327876,22.8896415311894,22.8899266823925,22.8902457310949,
22.8906029244097,22.8910030861364,22.89145170288,22.8919550240197,22.8925201774645,
22.8931553036475,22.8938697102046,22.8946740498672,22.8955805241163,22.8966031147916,
22.8977578452999,22.8990630721213,22.9005398055998,22.9022120567559,22.9041072032384,
22.947517097388,23.0538776382587,23.2440538574769,23.3003757495573,23.3384253462907,
23.3709547725524,23.4205897152378,23.4823122802948,23.6127045873432,23.6546966511943,
23.6758343404169,23.7764285743187,23.8061122741945,23.8260752302238,23.8446917280693,
23.8747983291818,23.8838035469633,23.9768535759189,24.1132601416553,24.2318215601649,
24.2798122853754,24.3157026486367,24.3506131919194,24.4148629559983),
 .UNSPECIFIED.) ;
#242 = B_SPLINE_CURVE_WITH_KNOTS('',3,(#30600,#30601,#30602,#30603,#30604,
#30605,#30606,#30607,#30608,#30609,#30610,#30611,#30612,#30613,#30614,#30615,
#30616,#30617,#30618,#30619,#30620,#30621,#30622,#30623,#30624,#30625,#30626,
#30627,#30628,#30629,#30630,#30631,#30632,#30633,#30634,#30635,#30636,#30637,
#30638,#30639,#30640,#30641,#30642,#30643,#30644,#30645,#30646,#30647,#30648,
#30649,#30650,#30651,#30652,#30653,#30654,#30655,#30656,#30657,#30658,#30659,
#30660,#30661,#30662,#30663,#30664,#30665,#30666,#30667,#30668,#30669,#30670,
#30671,#30672,#30673,#30674,#30675,#30676,#30677,#30678,#30679,#30680,#30681,
#30682,#30683,#30684,#30685,#30686,#30687,#30688,#30689,#30690,#30691,#30692,
#30693,#30694,#30695,#30696,#30697,#30698,#30699,#30700,#30701,#30702,#30703,
#30704,#30705,#30706,#30707,#30708,#30709,#30710,#30711,#30712,#30713,#30714,
#30715,#30716,#30717,#30718,#30719,#30720,#30721,#30722,#30723,#30724,#30725,
#30726,#30727,#30728,#30729,#30730,#30731,#30732,#30733,#30734,#30735,#30736,
#30737,#30738,#30739,#30740,#30741,#30742,#30743,#30744,#30745,#30746,#30747,
#30748,#30749,#30750,#30751,#30752,#30753,#30754,#30755,#30756,#30757,#30758,
#30759,#30760,#30761,#30762,#30763,#30764,#30765,#30766,#30767,#30768,#30769,
#30770,#30771,#30772,#30773,#30774,#30775,#30776,#30777,#30778,#30779,#30780,
#30781,#30782,#30783,#30784,#30785,#30786,#30787,#30788,#30789,#30790,#30791,
#30792,#30793,#30794,#30795,#30796,#30797,#30798,#30799,#30800,#30801,#30802,
#30803,#30804,#30805,#30806,#30807,#30808,#30809,#30810,#30811,#30812,#30813,
#30814,#30815,#30816,#30817,#30818,#30819,#30820,#30821,#30822,#30823,#30824,
#30825,#30826,#30827,#30828,#30829,#30830,#30831,#30832,#30833,#30834,#30835,
#30836,#30837,#30838,#30839,#30840,#30841,#30842,#30843,#30844,#30845,#30846,
#30847,#30848,#30849,#30850,#30851,#30852,#30853,#30854,#30855,#30856,#30857,
#30858,#30859,#30860,#30861,#30862,#30863,#30864,#30865,#30866,#30867,#30868,
#30869,#30870,#30871,#30872,#30873,#30874,#30875,#30876,#30877,#30878,#30879,
#30880,#30881,#30882,#30883,#30884,#30885,#30886,#30887,#30888,#30889,#30890,
#30891,#30892,#30893,#30894,#30895,#30896,#30897,#30898,#30899,#30900,#30901,
#30902,#30903,#30904,#30905,#30906,#30907,#30908,#30909,#30910,#30911,#30912,
#30913,#30914,#30915,#30916,#30917,#30918,#30919,#30920,#30921,#30922,#30923,
#30924,#30925,#30926,#30927,#30928,#30929,#30930,#30931,#30932,#30933,#30934,
#30935,#30936,#30937,#30938,#30939,#30940,#30941,#30942,#30943,#30944,#30945,
#30946,#30947,#30948,#30949,#30950,#30951,#30952,#30953,#30954,#30955,#30956,
#30957,#30958,#30959,#30960,#30961,#30962,#30963,#30964,#30965,#30966,#30967,
#30968,#30969,#30970,#30971,#30972,#30973,#30974,#30975,#30976,#30977,#30978,
#30979,#30980,#30981,#30982,#30983,#30984,#30985,#30986,#30987,#30988,#30989,
#30990,#30991,#30992,#30993,#30994,#30995,#30996,#30997,#30998,#30999,#31000,
#31001),.UNSPECIFIED.,.F.,.F.,(4,2,2,2,2,2,2,2,2,2,2,2,2,2,2,2,2,2,2,2,
2,2,2,2,2,2,2,2,2,2,2,2,2,2,2,2,2,2,2,2,2,2,2,2,2,2,2,2,2,2,2,2,2,2,2,2,
2,2,2,2,2,2,2,2,2,2,2,2,2,2,2,2,2,2,2,2,2,2,2,2,2,2,2,2,2,2,2,2,2,2,2,2,
2,2,2,2,2,2,2,2,2,2,2,2,2,2,2,2,2,2,2,2,2,2,2,2,2,2,2,2,2,2,2,2,2,2,2,2,
2,2,2,2,2,2,2,2,2,2,2,2,2,2,2,2,2,2,2,2,2,2,2,2,2,2,2,2,2,2,2,2,2,2,2,2,
2,2,2,2,2,2,2,2,2,2,2,2,2,2,2,2,2,2,2,2,2,2,2,2,2,2,2,2,2,2,2,2,2,2,2,2,
4),(0.000300064236370683,0.0723647523763316,0.111708964416556,0.133287846849445,
0.151427998569037,0.17013081821157,0.204487533123056,0.373915727662253,
0.537245797439023,0.570889420460193,0.596385588041295,0.631244919618651,
0.668999717700598,0.714747735427124,0.952409100978459,1.03593112393576,
1.07385966190513,1.10398883900008,1.11932044457847,1.13772612486928,1.17030222790595,
1.35876937254578,1.47049448971958,1.52745299964897,1.53168771270016,1.53535849172675,
1.53857162794452,1.54141187276103,1.5439470340794,1.54623167307539,1.54831002122938,
1.55021826097559,1.55198630429099,1.55363918342455,1.55519814630363,1.55668153004232,
1.55810547054093,1.559484494541,1.56083203232386,1.56216088437471,1.56348367356664,
1.56481331618967,1.56616355164705,1.60155322785786,1.63946693853557,1.68594048847265,
1.94848653822088,2.01577373849035,2.06221959112931,2.08527095315853,2.10519629497473,
2.13084457801574,2.21445944474567,2.23554690278583,2.3621746902663,2.42952807234498,
2.47051079859878,2.53261391621636,2.57205030529448,2.61016783628193,2.66690564154787,
2.81677996189875,2.97663844412068,3.0285960169111,3.05259073381019,3.07248411879497,
3.10161000549298,3.1919375061799,3.23252290104051,3.38535656667436,3.45196785765083,
3.50810142678944,3.54650165838166,3.58617065584388,3.64957052680161,3.73789184711398,
3.80749417098868,3.92634500745432,3.95880285775157,4.00228136249625,4.02479165207644,
4.04493560566148,4.07711391642218,4.26440509197348,4.40632405735721,4.46975103458349,
4.50942489693709,4.54737955021244,4.59403475245416,4.75738974052942,4.91941144723466,
4.96841971448581,4.99191978946321,5.01193249829625,5.04198595384655,5.14906647062526,
5.18878183592139,5.32960245465832,5.39370579429852,5.44831832084239,5.48647268635229,
5.52171219460949,5.58215554063168,5.67786011361571,5.84835696426342,5.88773025204314,
5.91166638340001,5.94673027626426,5.96760405128236,5.98655002035884,6.02229310404073,
6.16357791017453,6.16860445723978,6.30251128132899,6.34474497558316,6.40815118598117,
6.44782139163533,6.48577857146016,6.53244468854559,6.69576748855268,6.85779174181329,
6.90680135080787,6.93030169649483,6.95031440070281,6.98036751682532,7.08733849819573,
7.11498834189863,7.12643693941062,7.26773736289183,7.33194569648429,7.38662239240289,
7.42478697794578,7.46484105145289,7.53037852391577,7.61353026912302,7.78620615773346,
7.82581658647806,7.84985405055683,7.88502445212145,7.90591884726129,7.92484577643522,
7.96048149047412,8.09221411801463,8.23577394466106,8.27974909469319,8.34494044159996,
8.38493211014731,8.42269859623056,8.47724622664784,8.68674670184714,8.8163574987617,
8.85302003660045,8.8742076859909,8.89289613642419,8.92716796190361,9.09303206713614,
9.1304372160529,9.23185397379078,9.30672239106383,9.34843529249482,9.38596755269279,
9.4352880210662,9.57271885683992,9.59274033742292,9.73358572025248,9.78359783189059,
9.82135874652594,9.84276566457034,9.86130838133924,9.89471999765144,10.1016103456568,
10.201940253525,10.2370889597033,10.2928869478137,10.3312320888182,10.3709847738933,
10.4348494268077,10.522036558219,10.6940016560854,10.7335351245911,10.7832509602547,
10.8068718782516,10.8268520418335,10.8566661305089,10.9628188449026,10.9918644932046,
11.1407696282762,11.1856556229305,11.2517673867061,11.2919249703653,11.3296047038382,
11.3835863047801,11.6004953681049,11.7249773570164,11.7610876730576,11.7821658752364,
11.8009366502485,11.8356842599261,11.9930366547178,12.1211061577448,12.2074643523629),
 .UNSPECIFIED.) ;
#243 = B_SPLINE_CURVE_WITH_KNOTS('',3,(#31002,#31003,#31004,#31005,#31006,
#31007,#31008,#31009,#31010,#31011,#31012,#31013,#31014,#31015,#31016,#31017,
#31018,#31019,#31020,#31021,#31022,#31023,#31024,#31025,#31026,#31027,#31028,
#31029,#31030,#31031,#31032,#31033,#31034,#31035,#31036,#31037,#31038,#31039,
#31040,#31041,#31042,#31043,#31044,#31045,#31046,#31047,#31048,#31049,#31050,
#31051,#31052,#31053,#31054,#31055,#31056,#31057,#31058,#31059,#31060,#31061,
#31062,#31063,#31064,#31065,#31066,#31067,#31068,#31069,#31070,#31071,#31072,
#31073,#31074,#31075,#31076,#31077,#31078,#31079,#31080,#31081,#31082,#31083,
#31084,#31085,#31086,#31087,#31088,#31089,#31090,#31091,#31092,#31093,#31094,
#31095,#31096,#31097,#31098,#31099,#31100,#31101,#31102,#31103,#31104,#31105,
#31106,#31107,#31108,#31109,#31110,#31111,#31112,#31113,#31114,#31115,#31116,
#31117,#31118,#31119,#31120,#31121,#31122,#31123,#31124,#31125,#31126,#31127,
#31128,#31129,#31130,#31131,#31132,#31133,#31134,#31135,#31136,#31137,#31138,
#31139,#31140,#31141,#31142,#31143,#31144,#31145,#31146,#31147,#31148,#31149,
#31150,#31151,#31152,#31153,#31154,#31155,#31156,#31157,#31158,#31159,#31160,
#31161,#31162,#31163,#31164,#31165,#31166,#31167,#31168,#31169,#31170,#31171,
#31172,#31173,#31174,#31175,#31176,#31177,#31178,#31179,#31180,#31181,#31182,
#31183,#31184,#31185,#31186,#31187,#31188,#31189,#31190,#31191,#31192,#31193,
#31194,#31195,#31196,#31197,#31198,#31199,#31200,#31201,#31202,#31203,#31204,
#31205,#31206,#31207,#31208,#31209,#31210,#31211,#31212,#31213,#31214,#31215,
#31216,#31217,#31218,#31219,#31220,#31221,#31222,#31223,#31224,#31225,#31226,
#31227,#31228,#31229,#31230,#31231,#31232,#31233,#31234,#31235,#31236,#31237,
#31238,#31239,#31240,#31241,#31242,#31243,#31244,#31245,#31246,#31247,#31248,
#31249,#31250,#31251,#31252,#31253,#31254,#31255,#31256,#31257,#31258,#31259,
#31260,#31261,#31262,#31263,#31264,#31265,#31266,#31267,#31268,#31269,#31270,
#31271,#31272,#31273,#31274,#31275,#31276,#31277,#31278,#31279,#31280,#31281,
#31282,#31283,#31284,#31285,#31286,#31287,#31288,#31289,#31290,#31291,#31292,
#31293,#31294,#31295,#31296,#31297,#31298,#31299,#31300,#31301,#31302,#31303,
#31304,#31305,#31306,#31307,#31308,#31309,#31310,#31311,#31312,#31313,#31314,
#31315,#31316,#31317,#31318,#31319,#31320,#31321,#31322,#31323,#31324,#31325,
#31326,#31327,#31328,#31329,#31330,#31331,#31332,#31333,#31334,#31335,#31336,
#31337,#31338,#31339,#31340,#31341,#31342,#31343,#31344,#31345,#31346,#31347,
#31348,#31349,#31350,#31351,#31352,#31353,#31354,#31355,#31356,#31357,#31358,
#31359,#31360,#31361,#31362,#31363,#31364,#31365,#31366,#31367,#31368,#31369,
#31370,#31371,#31372,#31373),.UNSPECIFIED.,.F.,.F.,(4,2,2,2,2,2,2,2,2,2,
2,2,2,2,2,2,2,2,2,2,2,2,2,2,2,2,2,2,2,2,2,2,2,2,2,2,2,2,2,2,2,2,2,2,2,2,
2,2,2,2,2,2,2,2,2,2,2,2,2,2,2,2,2,2,2,2,2,2,2,2,2,2,2,2,2,2,2,2,2,2,2,2,
2,2,2,2,2,2,2,2,2,2,2,2,2,2,2,2,2,2,2,2,2,2,2,2,2,2,2,2,2,2,2,2,2,2,2,2,
2,2,2,2,2,2,2,2,2,2,2,2,2,2,2,2,2,2,2,2,2,2,2,2,2,2,2,2,2,2,2,2,2,2,2,2,
2,2,2,2,2,2,2,2,2,2,2,2,2,2,2,2,2,2,2,2,2,2,2,2,2,2,2,2,2,2,2,4),(7.92263036594461E-5,
0.285439410797672,0.325676368230994,0.350060823789353,0.368760547286798,
0.388654969438788,0.417789629828308,0.507173101801483,0.689783397735617,
0.761619798396612,0.806150156115514,0.827146881759627,0.861764633508179,
0.896566139823352,0.954226345151844,1.13569588276715,1.24609044475653,1.29036866305543,
1.32257183830718,1.32300963011027,1.32346132062348,1.3239268511748,1.3244061461291,
1.32489911478138,1.32540565331693,1.32592564675978,1.32613706685496,1.32638366586913,
1.32667045895257,1.32700290726294,1.34528641022483,1.36420141855042,1.39977043093359,
1.51981062658116,1.62960186208969,1.71559627827994,1.7827085910791,1.82304611173117,
1.86106343668104,1.91479418490189,2.13400773413672,2.25704484647675,2.2929952128078,
2.31404178075911,2.3328374434696,2.36772835947233,2.47364901716055,2.50518289537555,
2.64586136325104,2.68932978949199,2.75400507063272,2.7939036207803,2.83172188411034,
2.87776125777176,3.01935189475744,3.07313293165803,3.18418266974929,3.22859936087,
3.26325525692269,3.28405066236122,3.30588196070914,3.34579788186677,3.4662822281287,
3.47076102233836,3.6138137466388,3.65770040213656,3.72280170143627,3.76277694874762,
3.80055202583491,3.85515631618018,4.06586733540959,4.16094638922756,4.20177335680755,
4.23435557358773,4.25477000579239,4.27722637779772,4.32041608244396,4.50351224128716,
4.60756120622037,4.68366923759432,4.7255960500385,4.76307743179355,4.8119789307011,
4.92772763216422,5.10200867745599,5.14179105332943,5.16590172698441,5.20114885299746,
5.22205796169431,5.24097105199415,5.27652947274814,5.39645726740062,5.50594777158999,
5.59216120249817,5.65938958444144,5.69974789728489,5.73775505200043,5.79141963594927,
6.01100098193801,6.1338570920963,6.16978724043466,6.19082978590478,6.20962858270671,
6.24453766784338,6.35070530251803,6.51270087106321,6.61057590871916,6.65588980040333,
6.69306901824452,6.73813895419844,6.83426310658243,7.03479453419374,7.1189348794266,
7.14697721537695,7.16675976898853,7.1914391192938,7.24772529496063,7.50892187453285,
7.58889300767342,7.63147429440938,7.66883179318164,7.71658489294355,7.83401819784822,
8.00940902891725,8.04930912411433,8.07346985049825,8.10876940680438,8.12968861911999,
8.14859240034251,8.18409860511552,8.378267319018,8.48350894297163,8.56017071346663,
8.60219237603552,8.63965275564109,8.68837534228286,8.81611979692329,8.98117508921895,
9.01993874606655,9.06900556021672,9.09251549839319,9.11252513281466,9.14255775762738,
9.25488838855663,9.38151021911214,9.46838523109454,9.53596328585282,9.57638437438618,
9.61436176961882,9.66783051638161,9.88848482264557,10.0108220173771,10.0466941582192,
10.0677252465313,10.0865332200554,10.121495054378,10.2283782003239,10.2589239251033,
10.3995307482353,10.4429863047724,10.5076483007207,10.5475442572115,10.5853635758931,
10.6314086883711,10.7730793282653,10.9235986574593,10.9606072834236,11.0081686762797,
11.0314174879324,11.0515059445415,11.0820875706546,11.1922514526446,11.3574293215483,
11.4263707271137,11.4838971873268,11.5225310618414,11.5572614879215,11.6144595637865,
11.7972060660193,11.9073918645691,11.9516257385787,11.9861775610999,12.0069530834011,
12.0259950927627,12.0622764357232,12.2072718274533),.UNSPECIFIED.) ;
#244 = B_SPLINE_CURVE_WITH_KNOTS('',3,(#31378,#31379,#31380,#31381,#31382,
#31383,#31384,#31385,#31386,#31387,#31388,#31389,#31390,#31391,#31392,#31393,
#31394,#31395,#31396,#31397,#31398,#31399,#31400,#31401,#31402,#31403,#31404,
#31405,#31406,#31407,#31408,#31409,#31410,#31411,#31412,#31413,#31414,#31415,
#31416,#31417,#31418,#31419,#31420,#31421,#31422,#31423,#31424,#31425,#31426,
#31427,#31428,#31429,#31430,#31431,#31432,#31433,#31434,#31435,#31436,#31437,
#31438,#31439,#31440,#31441,#31442,#31443,#31444,#31445,#31446,#31447,#31448,
#31449,#31450,#31451,#31452,#31453,#31454,#31455,#31456,#31457,#31458,#31459,
#31460,#31461,#31462,#31463,#31464,#31465,#31466,#31467,#31468,#31469,#31470,
#31471,#31472,#31473,#31474,#31475,#31476,#31477,#31478,#31479,#31480,#31481,
#31482,#31483,#31484,#31485,#31486,#31487,#31488,#31489,#31490,#31491,#31492,
#31493,#31494,#31495,#31496,#31497,#31498,#31499,#31500,#31501,#31502,#31503,
#31504,#31505,#31506,#31507,#31508,#31509,#31510,#31511,#31512,#31513,#31514,
#31515,#31516,#31517,#31518,#31519,#31520,#31521,#31522,#31523,#31524,#31525,
#31526,#31527,#31528,#31529,#31530,#31531,#31532,#31533,#31534,#31535,#31536,
#31537,#31538,#31539,#31540,#31541,#31542,#31543,#31544,#31545,#31546,#31547,
#31548,#31549,#31550,#31551,#31552,#31553,#31554,#31555,#31556,#31557,#31558,
#31559,#31560,#31561,#31562,#31563,#31564,#31565,#31566,#31567,#31568,#31569,
#31570,#31571,#31572,#31573,#31574,#31575,#31576,#31577,#31578,#31579,#31580,
#31581,#31582,#31583,#31584,#31585,#31586,#31587,#31588,#31589,#31590,#31591,
#31592,#31593,#31594,#31595,#31596,#31597,#31598,#31599,#31600,#31601,#31602,
#31603,#31604,#31605,#31606,#31607,#31608,#31609,#31610,#31611,#31612,#31613,
#31614,#31615,#31616,#31617,#31618,#31619,#31620,#31621,#31622,#31623,#31624,
#31625,#31626,#31627,#31628,#31629,#31630,#31631,#31632,#31633,#31634,#31635,
#31636,#31637,#31638,#31639,#31640,#31641,#31642,#31643,#31644,#31645,#31646,
#31647,#31648,#31649,#31650,#31651,#31652,#31653,#31654,#31655,#31656,#31657,
#31658,#31659,#31660,#31661,#31662,#31663,#31664,#31665,#31666,#31667,#31668,
#31669,#31670,#31671,#31672,#31673,#31674,#31675,#31676,#31677,#31678,#31679,
#31680,#31681),.UNSPECIFIED.,.F.,.F.,(4,3,3,3,3,3,3,3,3,3,3,3,3,3,3,3,3,
3,3,3,3,3,3,3,3,3,3,3,3,3,3,3,3,3,3,3,3,3,3,3,3,3,3,3,3,3,3,3,3,3,3,3,3,
3,3,3,3,3,3,3,3,3,3,3,3,3,3,3,3,3,3,3,3,3,3,3,3,3,3,3,3,3,3,3,3,3,3,3,3,
3,3,3,3,3,3,3,3,3,3,3,3,4),(-73.2080292590851,-73.1459143162487,-73.083804333767,
-73.0212287225363,-72.9591134095751,-72.8963076492096,-72.8335018888441,
-72.7711444385968,-72.7088342241839,-72.6465306966311,-72.5842309554224,
-72.5218337882832,-72.4595276561961,-72.3970849715309,-72.3346422868657,
-72.2722848366184,-72.2099746222097,-72.147671094661,-72.0853713534566,
-72.0229741863143,-71.9606680542315,-71.8982253695594,-71.8357826848873,
-71.77342523464,-71.711115020227,-71.6488114926738,-71.5865117514652,-71.5241145843261,
-71.4618084522392,-71.399365767574,-71.3369230829089,-71.2745656326616,
-71.2122554182513,-71.1499518907003,-71.0876521494938,-71.025254982353,
-70.9629488502689,-70.9005061655997,-70.8380634809305,-70.7757060306832,
-70.7133958162715,-70.6510922887201,-70.5887925475126,-70.5263953803724,
-70.4640892482871,-70.4016465636196,-70.3392038789521,-70.2768464287048,
-70.2145362142939,-70.1522326867427,-70.0899329455366,-70.0275357783959,
-69.9652296463107,-69.9027869616422,-69.8403442769738,-69.7779868267265,
-69.7156766123153,-69.6533730847636,-69.5910733435567,-69.5286761764164,
-69.4663700443315,-69.4039273596635,-69.3414846749954,-69.2791272247481,
-69.2168170103367,-69.1545134827852,-69.0922137415786,-69.0298165744382,
-68.9675104423528,-68.9050677576849,-68.842625073017,-68.7802676227697,
-68.7179574083583,-68.6556538808074,-68.5933541396007,-68.5309569724601,
-68.4686508403746,-68.4062081557066,-68.3437654710386,-68.2814080207913,
-68.2190978063795,-68.1567942788276,-68.09449453762,-68.0320973704801,-67.9697912383952,
-67.9073485537277,-67.8449058690602,-67.7825484188129,-67.7202382044018,
-67.6579346768496,-67.5956349356414,-67.5332377685015,-67.4709316364168,
-67.4084889517493,-67.3460462670818,-67.2839762765568,-67.2219166211779,
-67.1598638956407,-67.0978094185812,-67.0357563242646,-66.9736929977926,
-66.9248439817473),.UNSPECIFIED.) ;
#245 = B_SPLINE_CURVE_WITH_KNOTS('',3,(#31682,#31683,#31684,#31685,#31686,
#31687,#31688,#31689,#31690,#31691,#31692,#31693,#31694,#31695,#31696,#31697,
#31698,#31699,#31700,#31701,#31702,#31703,#31704,#31705,#31706,#31707,#31708,
#31709,#31710,#31711,#31712,#31713,#31714,#31715,#31716,#31717,#31718,#31719,
#31720,#31721,#31722,#31723,#31724,#31725,#31726,#31727,#31728,#31729,#31730,
#31731,#31732,#31733,#31734,#31735,#31736,#31737,#31738,#31739,#31740,#31741,
#31742,#31743,#31744,#31745,#31746,#31747,#31748,#31749,#31750,#31751,#31752,
#31753,#31754,#31755,#31756,#31757,#31758,#31759,#31760,#31761,#31762,#31763,
#31764,#31765,#31766,#31767,#31768,#31769,#31770,#31771,#31772,#31773,#31774,
#31775,#31776,#31777,#31778,#31779,#31780,#31781,#31782,#31783,#31784,#31785,
#31786,#31787,#31788,#31789,#31790,#31791,#31792,#31793,#31794,#31795,#31796,
#31797,#31798,#31799,#31800,#31801,#31802,#31803,#31804,#31805,#31806,#31807,
#31808,#31809,#31810,#31811,#31812,#31813,#31814,#31815,#31816,#31817,#31818,
#31819,#31820,#31821,#31822,#31823,#31824,#31825,#31826,#31827,#31828,#31829,
#31830,#31831,#31832,#31833,#31834,#31835,#31836,#31837,#31838,#31839,#31840,
#31841,#31842,#31843,#31844,#31845,#31846,#31847,#31848,#31849,#31850,#31851,
#31852,#31853,#31854,#31855,#31856,#31857,#31858,#31859,#31860,#31861,#31862,
#31863,#31864,#31865,#31866,#31867,#31868,#31869,#31870,#31871,#31872,#31873,
#31874,#31875,#31876,#31877,#31878,#31879,#31880,#31881,#31882,#31883,#31884,
#31885,#31886,#31887,#31888,#31889,#31890,#31891,#31892,#31893,#31894,#31895,
#31896,#31897,#31898,#31899,#31900,#31901,#31902,#31903,#31904,#31905,#31906,
#31907,#31908,#31909,#31910,#31911,#31912,#31913,#31914,#31915,#31916,#31917,
#31918,#31919,#31920,#31921,#31922,#31923,#31924,#31925,#31926,#31927,#31928,
#31929,#31930,#31931,#31932,#31933,#31934,#31935,#31936,#31937,#31938,#31939,
#31940,#31941,#31942,#31943,#31944,#31945,#31946,#31947,#31948,#31949,#31950,
#31951,#31952,#31953,#31954,#31955,#31956,#31957,#31958,#31959,#31960,#31961,
#31962,#31963,#31964,#31965,#31966,#31967,#31968,#31969,#31970,#31971,#31972,
#31973,#31974,#31975,#31976,#31977,#31978,#31979,#31980,#31981,#31982,#31983,
#31984,#31985,#31986,#31987,#31988,#31989,#31990,#31991,#31992,#31993,#31994,
#31995,#31996,#31997,#31998,#31999,#32000,#32001,#32002,#32003,#32004,#32005,
#32006,#32007,#32008,#32009,#32010,#32011,#32012,#32013,#32014,#32015,#32016,
#32017,#32018,#32019,#32020,#32021,#32022,#32023,#32024,#32025,#32026,#32027,
#32028,#32029,#32030,#32031,#32032,#32033,#32034,#32035,#32036,#32037,#32038,
#32039,#32040,#32041,#32042,#32043,#32044,#32045,#32046,#32047,#32048,#32049,
#32050,#32051),.UNSPECIFIED.,.F.,.F.,(4,2,2,2,2,2,2,2,2,2,2,2,2,2,2,2,2,
2,2,2,2,2,2,2,2,2,2,2,2,2,2,2,2,2,2,2,2,2,2,2,2,2,2,2,2,2,2,2,2,2,2,2,2,
2,2,2,2,2,2,2,2,2,2,2,2,2,2,2,2,2,2,2,2,2,2,2,2,2,2,2,2,2,2,2,2,2,2,2,2,
2,2,2,2,2,2,2,2,2,2,2,2,2,2,2,2,2,2,2,2,2,2,2,2,2,2,2,2,2,2,2,2,2,2,2,2,
2,2,2,2,2,2,2,2,2,2,2,2,2,2,2,2,2,2,2,2,2,2,2,2,2,2,2,2,2,2,2,2,2,2,2,2,
2,2,2,2,2,2,2,2,2,2,2,2,2,2,2,2,2,2,2,2,2,2,2,4),(12.2072718274533,12.3977497167711,
12.4542601641789,12.492340157742,12.5318281998818,12.5942206404381,12.6354797337976,
12.8330913798462,12.9304389954081,12.9601760835259,12.9801458178146,13.0038060585305,
13.0537550543852,13.0935674945261,13.2681298160631,13.3865875607127,13.4343428119366,
13.4717005257048,13.5142804954632,13.5942438157573,13.8561141395262,13.906722921667,
13.9307678299505,13.9506034283396,13.9749116314301,14.0288133857135,14.1132843107081,
14.345980084663,14.3930210529472,14.4310628889466,14.4706052945446,14.5333012545417,
14.5748511353524,14.7051500962768,14.7469377194739,14.768758474474,14.8689820838145,
14.8986805456691,14.9186451485686,14.9423254319356,14.9923932900624,15.0323482812315,
15.2082579481845,15.2554131694779,15.3399116421206,15.3832324915028,15.4204957737368,
15.467922240178,15.5828877701329,15.815116838862,15.8573604795725,15.8796388035456,
15.9001484229358,15.9332670072165,16.0831770575733,16.2749317396433,16.3313129842835,
16.369371793282,16.4088898500396,16.4714498617669,16.549106901566,16.7789207200217,
16.8245616193987,16.8474685011202,16.8676799806685,16.8990561683132,16.9195755448626,
16.9793178593975,17.1984043708695,17.2800333779453,17.3228892807793,17.3564722659033,
17.4025394623861,17.5060744367043,17.6892054292528,17.7780476655874,17.807109446059,
17.8269953075165,17.8510269814867,17.9032107517015,17.9834956909541,18.2269717953508,
18.2724926696637,18.3101991603103,18.3503025013178,18.4161155464988,18.4996820679835,
18.6125184861236,18.6843704966532,18.7523022276742,18.7765449539403,18.7964094801789,
18.8205513045987,18.8734142187059,18.9553366890172,19.1958506793755,19.2414905949628,
19.279222241373,19.3192767259005,19.3848195962123,19.4291419028953,19.5747160340016,
19.6135170462254,19.707978132078,19.7411832809283,19.7596914432612,19.7811542150584,
19.8191975518346,19.8697330190019,20.0137621064173,20.1632170884288,20.2095196347705,
20.247395277952,20.2871945323048,20.3513208955801,20.3942535155513,20.531953412779,
20.6724696534244,20.7081667428062,20.7271043221114,20.7479863724557,20.7830944133269,
20.9599919924138,21.0376929821642,21.1425816252534,21.1900246095976,21.2272889499342,
21.2705980495207,21.3550237204654,21.4782143097203,21.6443564483648,21.6785979390088,
21.6972809236204,21.7184752379256,21.7551726872479,21.8032377402809,21.9329033386672,
21.9602240229548,22.1031732687599,22.1488840141077,22.1866308273941,22.2266568842223,
22.2920419213765,22.3362083313097,22.4808751952126,22.5437265258313,22.625444393919,
22.6510891019342,22.6710135673878,22.6940667156398,22.7405233697114,22.7762714348927,
22.9172470237126,22.9361918323935,23.0744560047225,23.1238018227702,23.1613365295802,
23.1999601848588,23.2691837177158,23.3602921810928,23.4629378081837,23.5046776914714,
23.5932273095291,23.6222480465391,23.642128924908,23.6590527974992,23.660973926847,
23.6630216957833,23.6652412710208,23.6676848669956,23.6682091844828,23.6688922373065,
23.6697911582846,23.6709889349966,23.6726089671795,23.6748389801266,23.7445416256931,
23.8828363914229,23.946311966082,24.0502159880961,24.0976017790855,24.1348620029846,
24.1699782283782,24.2130079824613,24.4145864482893),.UNSPECIFIED.) ;
#246 = B_SPLINE_CURVE_WITH_KNOTS('',3,(#32056,#32057,#32058,#32059,#32060,
#32061,#32062,#32063,#32064,#32065,#32066,#32067,#32068,#32069,#32070,#32071,
#32072,#32073,#32074,#32075,#32076,#32077,#32078,#32079,#32080,#32081,#32082,
#32083,#32084,#32085,#32086,#32087,#32088,#32089,#32090,#32091,#32092,#32093,
#32094,#32095,#32096,#32097,#32098,#32099,#32100,#32101,#32102,#32103,#32104,
#32105,#32106,#32107,#32108,#32109,#32110,#32111,#32112,#32113,#32114,#32115,
#32116,#32117,#32118,#32119,#32120,#32121,#32122,#32123,#32124,#32125,#32126,
#32127,#32128,#32129,#32130,#32131,#32132,#32133,#32134,#32135,#32136,#32137,
#32138,#32139,#32140,#32141,#32142,#32143,#32144,#32145,#32146,#32147,#32148,
#32149,#32150,#32151,#32152,#32153,#32154,#32155,#32156,#32157,#32158,#32159,
#32160,#32161,#32162,#32163,#32164,#32165,#32166,#32167,#32168,#32169,#32170,
#32171,#32172,#32173,#32174,#32175,#32176,#32177,#32178,#32179,#32180,#32181,
#32182,#32183,#32184,#32185,#32186,#32187,#32188,#32189,#32190,#32191,#32192,
#32193,#32194,#32195,#32196,#32197,#32198,#32199,#32200,#32201,#32202,#32203,
#32204,#32205,#32206,#32207,#32208,#32209,#32210,#32211,#32212,#32213,#32214,
#32215,#32216,#32217,#32218,#32219,#32220,#32221,#32222,#32223,#32224,#32225,
#32226,#32227,#32228,#32229,#32230,#32231,#32232,#32233,#32234,#32235,#32236,
#32237,#32238,#32239,#32240,#32241,#32242,#32243,#32244,#32245,#32246,#32247,
#32248,#32249,#32250,#32251,#32252,#32253,#32254,#32255,#32256,#32257,#32258,
#32259,#32260,#32261,#32262,#32263,#32264,#32265,#32266,#32267,#32268,#32269,
#32270,#32271,#32272,#32273,#32274,#32275,#32276,#32277,#32278,#32279,#32280,
#32281,#32282,#32283,#32284,#32285,#32286,#32287,#32288,#32289,#32290,#32291,
#32292,#32293,#32294,#32295,#32296,#32297,#32298,#32299,#32300,#32301,#32302,
#32303,#32304,#32305,#32306,#32307,#32308,#32309,#32310,#32311,#32312,#32313,
#32314,#32315,#32316,#32317,#32318,#32319,#32320,#32321,#32322,#32323,#32324,
#32325,#32326,#32327,#32328,#32329,#32330,#32331,#32332,#32333,#32334,#32335,
#32336,#32337,#32338,#32339,#32340,#32341,#32342,#32343,#32344,#32345,#32346,
#32347,#32348,#32349,#32350,#32351,#32352,#32353,#32354,#32355,#32356,#32357,
#32358,#32359),.UNSPECIFIED.,.F.,.F.,(4,3,3,3,3,3,3,3,3,3,3,3,3,3,3,3,3,
3,3,3,3,3,3,3,3,3,3,3,3,3,3,3,3,3,3,3,3,3,3,3,3,3,3,3,3,3,3,3,3,3,3,3,3,
3,3,3,3,3,3,3,3,3,3,3,3,3,3,3,3,3,3,3,3,3,3,3,3,3,3,3,3,3,3,3,3,3,3,3,3,
3,3,3,3,3,3,3,3,3,3,3,3,4),(-79.4912145612532,-79.4268580816011,-79.3624817745964,
-79.3186767145631,-79.2563192643158,-79.194009049235,-79.1317055211391,
-79.0694057795137,-79.0070086127814,-78.9447024805901,-78.8822597965874,
-78.8198171125847,-78.7574596623374,-78.6951494239939,-78.6328458722586,
-78.5705461066667,-78.5081489576516,-78.445842800927,-78.3834001557667,
-78.3209575106063,-78.258600060359,-78.1962898663862,-78.1339863594574,
-78.0716866390136,-78.0092894564172,-77.9469833452384,-77.8845406269331,
-77.8220979086279,-77.7597404583806,-77.6974302322208,-77.6351266928235,
-77.5728269396977,-77.5104297814357,-77.44812363737,-77.3856809720097,-77.3232383066495,
-77.2608808564022,-77.1985706471886,-77.1362671248746,-77.0739673889335,
-77.0115702178679,-76.9492640910678,-76.8868213978695,-76.8243787046712,
-76.7620212544239,-76.6997110383436,-76.6374075091123,-76.5751077662177,
-76.5127106003365,-76.4504044665619,-76.3879617846274,-76.3255191026928,
-76.2631616524455,-76.2008514382385,-76.1385479108915,-76.0762481698883,
-76.0138510025948,-75.9515448707106,-75.8891021857125,-75.8266595007144,
-75.7643020504671,-75.7019918362715,-75.6396883089383,-75.5773885679514,
-75.5149914006475,-75.4526852687853,-75.3902425837607,-75.327799898736,
-75.2654424484887,-75.2031322338472,-75.1408287060635,-75.0785289646224,
-75.0161317976562,-74.9538256653351,-74.8913829810463,-74.8289402967576,
-74.7665828465103,-74.704272632244,-74.641969104839,-74.5796693637792,-74.5172721965292,
-74.454966064592,-74.3925233796856,-74.3300806947792,-74.2677232445319,
-74.2054130300514,-74.1431095024306,-74.0808097611533,-74.0184125940652,
-73.9561064619095,-73.8936637773551,-73.8312210928008,-73.7688636425535,
-73.7065534281674,-73.6442499006414,-73.5819501594596,-73.5195529923003,
-73.4572468602403,-73.3948041755314,-73.3323614908225,-73.2668472050594,
-73.2080292600168),.UNSPECIFIED.) ;
#247 = B_SPLINE_CURVE_WITH_KNOTS('',3,(#32360,#32361,#32362,#32363,#32364,
#32365,#32366,#32367,#32368,#32369,#32370,#32371,#32372,#32373,#32374,#32375,
#32376,#32377,#32378,#32379,#32380,#32381,#32382,#32383,#32384,#32385,#32386,
#32387,#32388,#32389,#32390,#32391,#32392,#32393,#32394,#32395,#32396,#32397,
#32398,#32399,#32400,#32401,#32402,#32403,#32404,#32405,#32406,#32407,#32408,
#32409,#32410,#32411,#32412,#32413,#32414,#32415,#32416,#32417,#32418,#32419,
#32420,#32421,#32422,#32423,#32424,#32425,#32426,#32427,#32428,#32429,#32430,
#32431,#32432,#32433,#32434,#32435,#32436,#32437,#32438,#32439,#32440,#32441,
#32442,#32443,#32444,#32445,#32446,#32447,#32448,#32449,#32450,#32451,#32452,
#32453,#32454,#32455,#32456,#32457,#32458,#32459,#32460,#32461,#32462,#32463,
#32464,#32465,#32466,#32467,#32468,#32469,#32470,#32471,#32472,#32473,#32474,
#32475,#32476,#32477,#32478,#32479,#32480,#32481,#32482,#32483,#32484,#32485,
#32486,#32487,#32488,#32489,#32490,#32491,#32492,#32493,#32494,#32495,#32496,
#32497,#32498,#32499,#32500,#32501,#32502,#32503,#32504,#32505,#32506,#32507,
#32508,#32509,#32510,#32511,#32512,#32513,#32514,#32515,#32516,#32517,#32518,
#32519,#32520,#32521,#32522,#32523,#32524,#32525,#32526,#32527,#32528,#32529,
#32530,#32531,#32532,#32533,#32534,#32535,#32536,#32537,#32538,#32539,#32540,
#32541,#32542,#32543,#32544,#32545,#32546,#32547,#32548,#32549,#32550,#32551,
#32552,#32553,#32554,#32555,#32556,#32557,#32558,#32559,#32560,#32561,#32562,
#32563,#32564,#32565,#32566,#32567,#32568,#32569,#32570,#32571,#32572,#32573,
#32574,#32575,#32576,#32577,#32578,#32579,#32580,#32581,#32582,#32583,#32584,
#32585,#32586,#32587,#32588,#32589,#32590,#32591,#32592,#32593,#32594,#32595,
#32596,#32597,#32598,#32599,#32600,#32601,#32602,#32603,#32604,#32605,#32606,
#32607,#32608,#32609,#32610,#32611,#32612,#32613,#32614,#32615,#32616,#32617,
#32618,#32619,#32620,#32621,#32622,#32623,#32624,#32625,#32626,#32627,#32628,
#32629,#32630,#32631,#32632,#32633,#32634,#32635,#32636,#32637,#32638,#32639,
#32640,#32641,#32642,#32643,#32644,#32645,#32646,#32647,#32648,#32649,#32650,
#32651,#32652,#32653,#32654,#32655,#32656,#32657,#32658,#32659,#32660,#32661,
#32662,#32663,#32664,#32665,#32666,#32667,#32668,#32669,#32670,#32671,#32672,
#32673,#32674,#32675,#32676,#32677,#32678,#32679,#32680,#32681,#32682,#32683,
#32684,#32685,#32686,#32687,#32688,#32689,#32690,#32691,#32692,#32693,#32694,
#32695,#32696,#32697,#32698,#32699,#32700,#32701,#32702,#32703,#32704,#32705,
#32706,#32707,#32708,#32709,#32710,#32711,#32712,#32713,#32714,#32715,#32716,
#32717,#32718,#32719,#32720,#32721,#32722,#32723,#32724,#32725,#32726,#32727,
#32728,#32729,#32730,#32731,#32732,#32733,#32734,#32735,#32736,#32737,#32738,
#32739,#32740,#32741,#32742,#32743),.UNSPECIFIED.,.F.,.F.,(4,2,2,2,2,2,
2,2,2,2,2,2,2,2,2,2,2,2,2,2,2,2,2,2,2,2,2,2,2,2,2,2,2,2,2,2,2,2,2,2,2,2,
2,2,2,2,2,2,2,2,2,2,2,2,2,2,2,2,2,2,2,2,2,2,2,2,2,2,2,2,2,2,2,2,2,2,2,2,
2,2,2,2,2,2,2,2,2,2,2,2,2,2,2,2,2,2,2,2,2,2,2,2,2,2,2,2,2,2,2,2,2,2,2,2,
2,2,2,2,2,2,2,2,2,2,2,2,2,2,2,2,2,2,2,2,2,2,2,2,2,2,2,2,2,2,2,2,2,2,2,2,
2,2,2,2,2,2,2,2,2,2,2,2,2,2,2,2,2,2,2,2,2,2,2,2,2,2,2,2,2,2,2,2,2,2,2,2,
2,2,2,2,2,4),(5.2387363187429E-5,0.1405308078795,0.165124190737373,0.183885119107637,
0.203738040115377,0.232506750144318,0.319290774131082,0.371642125817686,
0.519414229923385,0.60985617636824,0.636520703677487,0.671400516008268,
0.709276099436823,0.75557745570598,0.902321740580871,0.949174461745862,
1.06096782730526,1.12291765042536,1.14829962710164,1.14917706987226,1.14954701645056,
1.15025320562604,1.15158559594079,1.15271509751055,1.16637849569789,1.19067113203141,
1.2444751441704,1.42807348775699,1.52295990086329,1.57504189836203,1.57808789692835,
1.58078667485465,1.58320080112759,1.58538064790428,1.58736709006859,1.5891936032842,
1.59088789389522,1.59247317004041,1.59396914073202,1.5953928107427,1.59675912418272,
1.5980814985439,1.59937228309313,1.60064317046535,1.60190558840903,1.63800769101212,
1.67595402831942,1.72921571476367,1.95102839234152,2.07280111762692,2.10860996914406,
2.12962862765459,2.14844680189936,2.18346689838626,2.29114286070091,2.45192942298535,
2.4987081052802,2.56670309223246,2.60719912377983,2.64514246625316,2.69838384251997,
2.92031401043612,3.04202877521207,3.07783113743871,3.09884853868992,3.11766779297178,
3.15269396899841,3.26045260830269,3.4211734331033,3.46794215432795,3.53592735543642,
3.57642166201242,3.61436584012224,3.66761258984043,3.88951236659545,4.01124248192391,
4.04704659527464,4.0680643562044,4.08688335485402,4.12190798922611,4.22964512057845,
4.39038340247107,4.43715480200092,4.50514266638918,4.54563748378574,4.58358149785494,
4.63682691619637,4.8587349765706,4.98046124868621,5.01626495545068,5.03728265270326,
5.05610174569895,5.0911268348381,5.19886975695654,5.35960369772108,5.40637446330416,
5.47436172849374,5.51485647088167,5.5528005831335,5.60604642787711,5.86649630065179,
5.93270562666728,5.97864667804191,6.00160770838509,6.0215651460436,6.05258644346674,
6.16219854515578,6.2888140889046,6.37603201315851,6.44379098055487,6.48424491503088,
6.52220786735582,6.57557823168696,6.69375388075133,6.85842528766969,6.89714530466782,
6.9461753718782,6.96967923000966,6.98969095468523,7.01973698793249,7.13275354873733,
7.25938679694259,7.34589523015528,7.41328000525393,7.45366675955542,7.49166104476944,
7.53676175779244,7.6753807065217,7.70864742204927,7.83836787042646,7.88644321797574,
7.92314659309218,7.9443423614454,7.96302496087448,7.99726278780776,8.16345188463413,
8.28662582603297,8.3710454478524,8.41435417208961,8.45161934510122,8.49906496438502,
8.60403012089681,8.68165096613729,8.85855072499019,8.89365876266852,8.91454108634465,
8.93347914361499,8.96917759230719,9.10970932898925,9.2474057180307,9.29033812857189,
9.35446460887873,9.39426442675673,9.43214090035472,9.47844483613853,9.64443274742685,
9.80554922683034,9.85403831555512,9.87744897776189,9.89748754233686,9.92772462730858,
10.0376180736525,10.1732045969089,10.232623032307,10.3122293422575,10.3547501960325,
10.3921181337826,10.4399718695478,10.5584051231605,10.732774186249,10.7725662042014,
10.8224984500119,10.8461561121503,10.8661269329768,10.8958702435779,10.994578182696,
11.0460476076368,11.1850829479737,11.2282576846174,11.2926328486577,11.3324776536624,
11.3703277908964,11.4165113183186,11.5825345314837,11.7408001323303,11.7913812512808,
11.8151482008142,11.835092272962,11.8598176811538,11.9309094264544,12.1305249554991,
12.2072423730149),.UNSPECIFIED.) ;
#248 = B_SPLINE_CURVE_WITH_KNOTS('',3,(#32749,#32750,#32751,#32752,#32753,
#32754,#32755,#32756,#32757,#32758,#32759,#32760,#32761,#32762,#32763,#32764,
#32765,#32766,#32767,#32768,#32769,#32770,#32771,#32772,#32773,#32774,#32775,
#32776,#32777,#32778,#32779,#32780,#32781,#32782,#32783,#32784,#32785,#32786,
#32787,#32788,#32789,#32790,#32791,#32792,#32793,#32794,#32795,#32796,#32797,
#32798),.UNSPECIFIED.,.F.,.F.,(4,2,2,2,2,2,2,2,2,2,2,2,2,2,2,2,2,2,2,2,
2,2,2,2,4),(41.7287185600906,41.8375642754602,41.9723397523482,42.0760090490107,
42.223976254466,42.4899520935777,42.6571500039819,42.8888759482191,43.0565538258593,
43.1530925035041,43.4139782595738,43.6194950036453,43.7994553691564,44.0331432752365,
44.1674373114751,44.271451812564,44.4207260572351,44.6841181869952,44.8508350319949,
45.0843043610434,45.2522594766109,45.3495974165661,45.7530389442282,45.906737536888,
46.2267394719888),.UNSPECIFIED.) ;
#249 = B_SPLINE_CURVE_WITH_KNOTS('',3,(#32801,#32802,#32803,#32804,#32805,
#32806,#32807,#32808,#32809,#32810,#32811,#32812,#32813,#32814,#32815,#32816,
#32817,#32818,#32819,#32820,#32821,#32822,#32823,#32824,#32825,#32826,#32827,
#32828,#32829,#32830,#32831,#32832),.UNSPECIFIED.,.F.,.F.,(4,2,2,2,2,2,
2,2,2,2,2,2,2,2,2,4),(0.000341622627806292,0.0673400657444466,0.227847209082467,
0.411559779210653,0.57815132892849,0.812417356253106,1.04496426355356,1.13432835898471,
1.33790194751096,1.52715641261998,1.69498193634874,1.96835421119834,2.11155443311271,
2.21386703158126,2.42160026776052,2.45788151536469),.UNSPECIFIED.) ;
#250 = B_SPLINE_CURVE_WITH_KNOTS('',3,(#32837,#32838,#32839,#32840,#32841,
#32842,#32843,#32844,#32845,#32846,#32847,#32848,#32849,#32850,#32851,#32852,
#32853,#32854,#32855,#32856,#32857,#32858,#32859,#32860,#32861,#32862,#32863,
#32864,#32865,#32866,#32867,#32868,#32869,#32870,#32871,#32872,#32873,#32874,
#32875,#32876,#32877,#32878,#32879,#32880,#32881,#32882,#32883,#32884,#32885,
#32886,#32887,#32888,#32889,#32890,#32891,#32892,#32893,#32894,#32895,#32896,
#32897,#32898,#32899,#32900,#32901,#32902,#32903,#32904,#32905,#32906,#32907,
#32908,#32909,#32910,#32911,#32912,#32913,#32914,#32915,#32916,#32917,#32918,
#32919,#32920,#32921,#32922,#32923,#32924,#32925,#32926,#32927,#32928,#32929,
#32930,#32931,#32932,#32933,#32934,#32935,#32936,#32937,#32938,#32939,#32940,
#32941,#32942,#32943,#32944,#32945,#32946,#32947,#32948,#32949,#32950,#32951,
#32952,#32953,#32954,#32955,#32956,#32957,#32958,#32959,#32960,#32961,#32962,
#32963,#32964,#32965,#32966,#32967,#32968,#32969,#32970,#32971,#32972,#32973,
#32974,#32975,#32976,#32977,#32978,#32979,#32980,#32981,#32982,#32983,#32984,
#32985,#32986,#32987,#32988,#32989,#32990),.UNSPECIFIED.,.F.,.F.,(4,2,2,
2,2,2,2,2,2,2,2,2,2,2,2,2,2,2,2,2,2,2,2,2,2,2,2,2,2,2,2,2,2,2,2,2,2,2,2,
2,2,2,2,2,2,2,2,2,2,2,2,2,2,2,2,2,2,2,2,2,2,2,2,2,2,2,2,2,2,2,2,2,2,2,2,
2,4),(27.8190516686995,28.0540235284573,28.2596408606393,28.4393565434381,
28.6723158521103,28.8069846106989,28.9108641731384,29.0595232512103,29.3239631514734,
29.4910804091608,29.7230468328308,29.8906690727476,29.9870524844356,30.2446291280341,
30.4523398010245,30.6312239858078,30.8610367252987,31.0025169158246,31.1075312692734,
31.2598656914219,31.5169605627561,31.6838216517124,31.9173531199209,32.0850718077781,
32.1815366645503,32.4423589581098,32.6479885134352,32.8277093378174,33.0606711957569,
33.1953481304821,33.299225384594,33.4478701785114,33.7123598734217,33.8794843925669,
34.1114512397397,34.2790790990271,34.375465620232,34.633051245024,34.840771283573,
35.0196619820374,35.2494823254115,35.3909693236478,35.4959885973176,35.6483316549986,
35.9054290247319,36.0722964432488,36.3058352920589,36.4735590354038,36.570023962846,
36.8308511488704,37.0364974251052,37.2162166432378,37.4491597061846,37.5838559375489,
37.687721235687,37.8363163400969,38.1009267038591,38.2680694397395,38.4999965555923,
38.6676240359239,38.7639977290439,39.0215672768671,39.2293360539831,39.4081912845709,
39.637886369621,39.7795604418841,39.8845711602258,40.0368694462086,40.294084744372,
40.4609885606339,40.69445452348,40.8621804866196,40.958636438836,41.2194417914166,
41.4251129111561,41.6047817746195,41.7287185600906),.UNSPECIFIED.) ;
#251 = B_SPLINE_CURVE_WITH_KNOTS('',3,(#32991,#32992,#32993,#32994,#32995,
#32996,#32997,#32998,#32999,#33000,#33001,#33002,#33003,#33004,#33005,#33006,
#33007,#33008,#33009,#33010,#33011,#33012,#33013,#33014,#33015,#33016,#33017,
#33018,#33019,#33020,#33021,#33022,#33023,#33024,#33025,#33026,#33027,#33028,
#33029,#33030,#33031,#33032,#33033,#33034,#33035,#33036,#33037,#33038,#33039,
#33040,#33041,#33042,#33043,#33044,#33045,#33046,#33047,#33048,#33049,#33050,
#33051,#33052,#33053,#33054,#33055,#33056,#33057,#33058,#33059,#33060,#33061,
#33062,#33063,#33064,#33065,#33066,#33067,#33068,#33069,#33070,#33071,#33072,
#33073,#33074,#33075,#33076,#33077,#33078,#33079,#33080,#33081,#33082,#33083,
#33084,#33085,#33086,#33087,#33088,#33089,#33090,#33091,#33092,#33093,#33094,
#33095,#33096,#33097,#33098,#33099,#33100,#33101,#33102,#33103,#33104,#33105,
#33106,#33107,#33108,#33109,#33110,#33111,#33112,#33113,#33114,#33115,#33116,
#33117,#33118,#33119,#33120,#33121,#33122,#33123,#33124,#33125,#33126,#33127,
#33128,#33129,#33130,#33131,#33132,#33133,#33134,#33135,#33136,#33137,#33138,
#33139,#33140,#33141,#33142),.UNSPECIFIED.,.F.,.F.,(4,2,2,2,2,2,2,2,2,2,
2,2,2,2,2,2,2,2,2,2,2,2,2,2,2,2,2,2,2,2,2,2,2,2,2,2,2,2,2,2,2,2,2,2,2,2,
2,2,2,2,2,2,2,2,2,2,2,2,2,2,2,2,2,2,2,2,2,2,2,2,2,2,2,2,2,4),(2.45788151536469,
2.61572539621936,2.78598388195183,3.08078171023571,3.21465083221518,3.31432199203162,
3.46437731498878,3.68336366443902,3.85866608787174,4.06937792176419,4.32664895588177,
4.42141259903627,4.58806490653788,4.81302279923895,4.98186528234662,5.2643125384097,
5.40439542228602,5.5058086928236,5.63875899112841,5.86989141345836,6.04899095963599,
6.25466890087166,6.51329933433767,6.61027514846681,6.79807166592806,6.99695763716408,
7.16745943789951,7.47298648500569,7.60501576704184,7.70392271308596,7.92851927930397,
8.18428585977036,8.35194201046475,8.58095157831059,8.74838260263357,8.84457212200991,
9.10183145747964,9.31016312720026,9.48877639729143,9.71759798271826,9.8605031233545,
9.96525293206253,10.1167206115351,10.3755787449451,10.5425322324869,10.7756652500631,
10.9433779405392,11.0398442315285,11.3006610830669,11.506319792173,11.6860162797535,
11.9188817453385,12.0536204870947,12.157383004324,12.3056508006402,12.5709461774572,
12.7381165289833,12.9699010332766,13.1375293398637,13.2339189450469,13.4915109933954,
13.6992538133391,13.8781451816648,14.1079472058251,14.249486161008,14.3544968433405,
14.5068036390699,14.76400349011,14.9308824549095,15.1644181044631,15.332151221201,
15.428624657939,15.6894701986197,15.8951196283019,16.0475649733886,16.3682710977173),
 .UNSPECIFIED.) ;
#252 = B_SPLINE_CURVE_WITH_KNOTS('',3,(#33147,#33148,#33149,#33150,#33151,
#33152,#33153,#33154,#33155,#33156,#33157,#33158,#33159,#33160,#33161,#33162,
#33163,#33164,#33165,#33166,#33167,#33168,#33169,#33170,#33171,#33172,#33173,
#33174,#33175,#33176,#33177,#33178,#33179,#33180,#33181,#33182,#33183,#33184,
#33185,#33186,#33187,#33188,#33189,#33190,#33191,#33192,#33193,#33194,#33195,
#33196,#33197,#33198,#33199,#33200,#33201,#33202,#33203,#33204,#33205,#33206,
#33207,#33208,#33209,#33210,#33211,#33212,#33213,#33214,#33215,#33216,#33217,
#33218,#33219,#33220,#33221,#33222,#33223,#33224,#33225,#33226,#33227,#33228,
#33229,#33230,#33231,#33232,#33233,#33234,#33235,#33236,#33237,#33238,#33239,
#33240,#33241,#33242,#33243,#33244,#33245,#33246,#33247,#33248,#33249,#33250,
#33251,#33252,#33253,#33254,#33255,#33256,#33257,#33258,#33259,#33260,#33261,
#33262,#33263,#33264,#33265,#33266,#33267,#33268,#33269,#33270,#33271,#33272,
#33273,#33274,#33275,#33276,#33277,#33278,#33279,#33280,#33281,#33282,#33283,
#33284,#33285,#33286,#33287,#33288,#33289,#33290,#33291,#33292,#33293,#33294,
#33295,#33296,#33297,#33298,#33299,#33300,#33301,#33302),.UNSPECIFIED.,
 .F.,.F.,(4,2,2,2,2,2,2,2,2,2,2,2,2,2,2,2,2,2,2,2,2,2,2,2,2,2,2,2,2,2,2,
2,2,2,2,2,2,2,2,2,2,2,2,2,2,2,2,2,2,2,2,2,2,2,2,2,2,2,2,2,2,2,2,2,2,2,2,
2,2,2,2,2,2,2,2,2,2,4),(13.9103642396951,14.059290140731,14.3237983625056,
14.4724210040941,14.5762901521091,14.7109677686707,14.943922753552,15.123638578108,
15.329262085377,15.5900705656506,15.6865317966044,15.8542477597018,16.0877656548719,
16.2546245954422,16.511761847043,16.6640612199289,16.7690634207516,16.9105862528965,
17.1403657262307,17.3192378820909,17.5269617415358,17.7845148316813,17.8808886684624,
18.048500856383,18.2803347085067,18.4474698768279,18.7124781184351,18.8608450506072,
18.9646331944916,19.0993477918314,19.3322130954862,19.511900790291,19.7175675247081,
19.978338496364,20.0747801450231,20.242471329193,20.4756670603556,20.6425710537004,
20.9012441620136,21.0527546018228,21.1575112070697,21.3003433500153,21.5291973969586,
21.7078186505762,21.9161865574636,22.1733999212904,22.2695732864486,22.4369325533377,
22.6649689996637,22.8327644295761,23.1136426005817,23.3162890235833,23.4164490753815,
23.5528962226204,23.8237852586347,23.9883724044378,24.0776389286475,24.4097814047875,
24.5080062088504,24.6377712884637,24.9354426049739,25.1024882127116,25.3348355091553,
25.5024751812084,25.598874840555,25.8564748147422,26.0641135164308,26.2430155267256,
26.4729116887741,26.6142560450411,26.7192918204235,26.871702545449,27.1286270367516,
27.2954768834071,27.529031415055,27.6967457248573,27.7932084143236,27.8190516686995),
 .UNSPECIFIED.) ;
#253 = B_SPLINE_CURVE_WITH_KNOTS('',3,(#33303,#33304,#33305,#33306,#33307,
#33308,#33309,#33310,#33311,#33312,#33313,#33314,#33315,#33316,#33317,#33318,
#33319,#33320,#33321,#33322,#33323,#33324,#33325,#33326,#33327,#33328,#33329,
#33330,#33331,#33332,#33333,#33334,#33335,#33336,#33337,#33338,#33339,#33340,
#33341,#33342,#33343,#33344,#33345,#33346,#33347,#33348,#33349,#33350,#33351,
#33352,#33353,#33354,#33355,#33356,#33357,#33358,#33359,#33360,#33361,#33362,
#33363,#33364,#33365,#33366,#33367,#33368,#33369,#33370,#33371,#33372,#33373,
#33374,#33375,#33376,#33377,#33378,#33379,#33380,#33381,#33382,#33383,#33384,
#33385,#33386,#33387,#33388,#33389,#33390,#33391,#33392,#33393,#33394,#33395,
#33396,#33397,#33398,#33399,#33400,#33401,#33402,#33403,#33404,#33405,#33406,
#33407,#33408,#33409,#33410,#33411,#33412,#33413,#33414,#33415,#33416,#33417,
#33418,#33419,#33420,#33421,#33422,#33423,#33424,#33425,#33426,#33427,#33428,
#33429,#33430,#33431,#33432,#33433,#33434,#33435,#33436,#33437,#33438,#33439,
#33440,#33441,#33442,#33443,#33444,#33445,#33446,#33447,#33448,#33449,#33450,
#33451,#33452,#33453,#33454,#33455,#33456,#33457,#33458),.UNSPECIFIED.,
 .F.,.F.,(4,2,2,2,2,2,2,2,2,2,2,2,2,2,2,2,2,2,2,2,2,2,2,2,2,2,2,2,2,2,2,
2,2,2,2,2,2,2,2,2,2,2,2,2,2,2,2,2,2,2,2,2,2,2,2,2,2,2,2,2,2,2,2,2,2,2,2,
2,2,2,2,2,2,2,2,2,2,4),(8.88234718024114E-5,0.0601731981236326,0.110544207433153,
0.280019453746977,0.526557105931961,0.686420100604339,0.94582691662437,
1.0970123777365,1.2016778533486,1.34515029285172,1.573614889418,1.75215096620334,
1.96086205048697,2.21796096889079,2.31405837721316,2.48132234554296,2.71655350383365,
2.88303392076658,3.12529198286448,3.28553078281349,3.39298102298311,3.53575118406741,
3.76636756107163,3.94547424543211,4.15265776878262,4.41052553945569,4.50708440246902,
4.6749158123924,4.91021311217619,5.07680440524432,5.32415911551499,5.48160075826832,
5.58819192173581,5.73025418571335,5.96076037630328,6.13983557684914,6.34708723007708,
6.60491304823191,6.70144736191669,6.86925036137248,7.10409881782883,7.27075703608349,
7.52082435426871,7.67681151042562,7.78295420614849,7.92462507781732,8.15507438766519,
8.33413226772008,8.54141594843493,8.79921842941794,8.89573962148368,9.06352678642508,
9.29814912360071,9.46483942112775,9.71618375185056,9.87149161696981,9.97742405377179,
10.1189058542712,10.3493268332367,10.5283749724368,10.7356711879939,10.9934603611286,
11.0899745710014,11.257752759487,11.4922692505847,11.6589725815367,11.910884678648,
12.0658891807724,12.1717270734666,12.3052477517957,12.5402382400976,12.7204909057877,
12.9248764487335,13.1863693694132,13.2832324775336,13.4935240406713,13.7449391001076,
13.9098688392401),.UNSPECIFIED.) ;
#254 = B_SPLINE_CURVE_WITH_KNOTS('',3,(#33463,#33464,#33465,#33466,#33467,
#33468,#33469,#33470,#33471,#33472,#33473,#33474,#33475,#33476,#33477,#33478,
#33479,#33480,#33481,#33482,#33483,#33484,#33485,#33486,#33487,#33488,#33489,
#33490,#33491,#33492,#33493,#33494,#33495,#33496,#33497,#33498,#33499,#33500,
#33501,#33502,#33503,#33504,#33505,#33506,#33507,#33508,#33509,#33510,#33511,
#33512,#33513,#33514,#33515,#33516,#33517,#33518,#33519,#33520,#33521,#33522,
#33523,#33524,#33525,#33526,#33527,#33528,#33529,#33530,#33531,#33532,#33533,
#33534,#33535,#33536,#33537,#33538,#33539,#33540,#33541,#33542,#33543,#33544,
#33545,#33546,#33547,#33548,#33549,#33550,#33551,#33552,#33553,#33554,#33555,
#33556,#33557,#33558,#33559,#33560,#33561,#33562,#33563,#33564,#33565,#33566,
#33567,#33568,#33569,#33570,#33571,#33572,#33573,#33574,#33575,#33576,#33577,
#33578,#33579,#33580,#33581,#33582,#33583,#33584,#33585,#33586,#33587,#33588,
#33589,#33590,#33591,#33592,#33593,#33594,#33595,#33596,#33597,#33598,#33599,
#33600,#33601,#33602,#33603,#33604,#33605,#33606,#33607,#33608,#33609,#33610,
#33611,#33612,#33613,#33614,#33615,#33616,#33617,#33618),.UNSPECIFIED.,
 .F.,.F.,(4,2,2,2,2,2,2,2,2,2,2,2,2,2,2,2,2,2,2,2,2,2,2,2,2,2,2,2,2,2,2,
2,2,2,2,2,2,2,2,2,2,2,2,2,2,2,2,2,2,2,2,2,2,2,2,2,2,2,2,2,2,2,2,2,2,2,2,
2,2,2,2,2,2,2,2,2,2,4),(0.000358256576057275,0.228881878662184,0.285883905039836,
0.392988116828161,0.733898218813132,0.893503238773272,1.15802559996168,
1.3066728138271,1.41055610600951,1.54524765423352,1.77823150756874,1.95796833075757,
2.16361352921898,2.42445237999845,2.52092502082217,2.68866053278439,2.92221456396537,
3.08909080129259,3.34620855128427,3.49854988914389,3.60357160178668,3.7450705602412,
3.97490407266984,4.15380392840545,4.36153168449772,4.61912391930075,4.71551468909243,
4.88315305759357,5.11513116765748,5.28226528591404,5.54677768360417,5.69541928404525,
5.79929865587834,5.93398512494897,6.16696018842095,6.34669023172362,6.55232767503622,
6.81315668675464,6.90962568839495,7.07735487321628,7.31090008676587,7.47777003123677,
7.73487812554999,7.88721369588314,7.99223144067999,8.13372509674368,8.36354991594576,
8.54244301745753,8.75016295551668,9.00774546577109,9.1041325946582,9.27176463391636,
9.5037338916022,9.67086172323557,9.93536460275411,10.084000371521,10.1878757558121,
10.3225571827991,10.5555233861152,10.735246631149,10.9408763640544,11.2016955129446,
11.2981608616184,11.4658837034878,11.6994198261313,11.8662835226502,12.1233833316115,
12.2757124374329,12.3807259994421,12.5222154765817,12.7520308131936,12.9309169506701,
13.1386296230641,13.396202127569,13.4925854459245,13.6602109532714,13.8921680337048,
13.9103642396951),.UNSPECIFIED.) ;
#255 = B_SPLINE_CURVE_WITH_KNOTS('',3,(#33619,#33620,#33621,#33622,#33623,
#33624,#33625,#33626,#33627,#33628,#33629,#33630,#33631,#33632,#33633,#33634,
#33635,#33636,#33637,#33638,#33639,#33640,#33641,#33642,#33643,#33644,#33645,
#33646,#33647,#33648,#33649,#33650,#33651,#33652,#33653,#33654,#33655,#33656,
#33657,#33658,#33659,#33660,#33661,#33662,#33663,#33664,#33665,#33666,#33667,
#33668,#33669,#33670,#33671,#33672,#33673,#33674,#33675,#33676,#33677,#33678,
#33679,#33680,#33681,#33682,#33683,#33684,#33685,#33686,#33687,#33688,#33689,
#33690,#33691,#33692,#33693,#33694,#33695,#33696,#33697,#33698,#33699,#33700,
#33701,#33702,#33703,#33704,#33705,#33706,#33707,#33708,#33709,#33710,#33711,
#33712,#33713,#33714,#33715,#33716,#33717,#33718,#33719,#33720,#33721,#33722,
#33723,#33724,#33725,#33726,#33727,#33728,#33729,#33730,#33731,#33732,#33733,
#33734,#33735,#33736,#33737,#33738,#33739,#33740,#33741,#33742,#33743,#33744,
#33745,#33746,#33747,#33748,#33749,#33750,#33751,#33752,#33753,#33754,#33755,
#33756,#33757,#33758,#33759,#33760,#33761,#33762,#33763,#33764,#33765,#33766,
#33767,#33768,#33769,#33770,#33771,#33772),.UNSPECIFIED.,.F.,.F.,(4,2,2,
2,2,2,2,2,2,2,2,2,2,2,2,2,2,2,2,2,2,2,2,2,2,2,2,2,2,2,2,2,2,2,2,2,2,2,2,
2,2,2,2,2,2,2,2,2,2,2,2,2,2,2,2,2,2,2,2,2,2,2,2,2,2,2,2,2,2,2,2,2,2,2,2,
2,4),(13.9098688392401,14.1556640945556,14.3228458792463,14.4188879587625,
14.6758880360635,14.8847408681272,15.0632003858644,15.2914213689572,15.4351943825689,
15.5397975605937,15.6907999063745,15.9505284316708,16.1174774019243,16.3504696402124,
16.5181559164659,16.6145926296687,16.8753658706323,17.0810835460594,17.2607658518236,
17.4935838069903,17.6283345220276,17.7320751647221,17.8802772177466,18.1456688450993,
18.3128274245213,18.5445902888266,18.7122051875404,18.8085807795861,19.0661478292541,
19.2739013729509,19.4527775282826,19.6825454438916,19.8241052324821,19.9291087000797,
20.0814014988205,20.3385969942852,20.5054666418987,20.7389878885708,20.9067110744443,
21.0031778248,21.264006667204,21.4696471635165,21.6493715566429,21.882332452245,
22.0170184957055,22.1208909453636,22.269513722124,22.5340676516857,22.7012001115818,
22.933162201478,23.100794947581,23.1971838319584,23.4547765389269,23.6625060379139,
23.8414008388903,24.0712225297513,24.2127230657623,24.3177427228717,24.4700810655704,
24.7272075613882,24.8940807985462,25.1276263420014,25.2953566309189,25.3918277354045,
25.6526675765619,25.858313103886,26.0380451905918,26.2710187231217,26.4057076175683,
26.5095877573895,26.6582285391607,26.9227667038272,27.082368010658,27.4239759561574,
27.5307307926211,27.585780009175,27.8196846114232),.UNSPECIFIED.) ;
#256 = B_SPLINE_CURVE_WITH_KNOTS('',3,(#33777,#33778,#33779,#33780,#33781,
#33782,#33783,#33784,#33785,#33786,#33787,#33788,#33789,#33790,#33791,#33792,
#33793,#33794,#33795,#33796,#33797,#33798,#33799,#33800,#33801,#33802,#33803,
#33804,#33805,#33806,#33807,#33808,#33809,#33810,#33811,#33812,#33813,#33814,
#33815,#33816,#33817,#33818,#33819,#33820,#33821,#33822,#33823,#33824,#33825,
#33826,#33827,#33828,#33829,#33830,#33831,#33832,#33833,#33834,#33835,#33836,
#33837,#33838,#33839,#33840,#33841,#33842,#33843,#33844,#33845,#33846,#33847,
#33848,#33849,#33850,#33851,#33852,#33853,#33854,#33855,#33856,#33857,#33858,
#33859,#33860,#33861,#33862,#33863,#33864,#33865,#33866,#33867,#33868,#33869,
#33870,#33871,#33872,#33873,#33874,#33875,#33876,#33877,#33878,#33879,#33880,
#33881,#33882,#33883,#33884,#33885,#33886,#33887,#33888,#33889,#33890,#33891,
#33892,#33893,#33894,#33895,#33896,#33897,#33898,#33899,#33900,#33901,#33902,
#33903,#33904,#33905,#33906,#33907,#33908,#33909,#33910,#33911,#33912,#33913,
#33914,#33915,#33916,#33917,#33918,#33919,#33920,#33921,#33922,#33923,#33924,
#33925,#33926,#33927,#33928,#33929,#33930,#33931,#33932,#33933,#33934,#33935,
#33936,#33937,#33938,#33939,#33940,#33941,#33942,#33943,#33944,#33945,#33946,
#33947,#33948,#33949,#33950,#33951,#33952,#33953,#33954,#33955,#33956,#33957,
#33958,#33959,#33960,#33961,#33962,#33963,#33964,#33965,#33966,#33967,#33968,
#33969,#33970,#33971,#33972,#33973,#33974,#33975,#33976,#33977,#33978,#33979,
#33980,#33981,#33982,#33983,#33984,#33985,#33986,#33987,#33988,#33989,#33990,
#33991,#33992,#33993,#33994,#33995,#33996,#33997,#33998,#33999,#34000,#34001,
#34002,#34003,#34004,#34005,#34006,#34007,#34008,#34009,#34010,#34011,#34012,
#34013,#34014,#34015,#34016,#34017,#34018,#34019,#34020,#34021,#34022,#34023,
#34024,#34025,#34026,#34027,#34028,#34029,#34030,#34031,#34032,#34033,#34034,
#34035,#34036,#34037,#34038,#34039,#34040,#34041,#34042,#34043,#34044,#34045,
#34046,#34047,#34048,#34049,#34050,#34051,#34052,#34053,#34054,#34055,#34056,
#34057,#34058,#34059,#34060,#34061,#34062,#34063,#34064,#34065,#34066,#34067,
#34068,#34069,#34070,#34071,#34072,#34073,#34074,#34075,#34076,#34077,#34078,
#34079,#34080,#34081,#34082,#34083,#34084,#34085,#34086,#34087,#34088,#34089,
#34090,#34091,#34092,#34093,#34094,#34095,#34096,#34097,#34098,#34099,#34100,
#34101,#34102,#34103,#34104,#34105,#34106,#34107,#34108,#34109,#34110,#34111,
#34112,#34113,#34114,#34115,#34116),.UNSPECIFIED.,.F.,.F.,(4,3,3,3,3,3,
3,3,3,3,3,3,3,3,3,3,3,3,3,3,3,3,3,3,3,3,3,3,3,3,3,3,3,3,3,3,3,3,3,3,3,3,
3,3,3,3,3,3,3,3,3,3,3,3,3,3,3,3,3,3,3,3,3,3,3,3,3,3,3,3,3,3,3,3,3,3,3,3,
3,3,3,3,3,3,3,3,3,3,3,3,3,3,3,3,3,3,3,3,3,3,3,3,3,3,3,3,3,3,3,3,3,3,3,4),
(-29.2146074456426,-29.1543978565729,-29.0941972193378,-29.034002687827,
-28.9738114178698,-28.9136143857649,-28.8534164946886,-28.7932062199675,
-28.7441363464316,-28.6821877767195,-28.6218625733065,-28.5615435728776,
-28.501228171081,-28.4380580754944,-28.3777368279562,-28.317412879575,-28.2570789068001,
-28.2485477887345,-28.1865992190224,-28.126274015621,-28.065955015204,-28.0056396134189,
-27.9424695178235,-27.8821482702971,-27.8218243219273,-27.7614903491642,
-27.7529592310374,-27.6910106613253,-27.630685457917,-27.5703664574931,
-27.5100510557013,-27.4468809601111,-27.3865597125778,-27.3262357642009,
-27.2659017914312,-27.2573706733403,-27.1954221036282,-27.1350969002231,
-27.0747778998024,-27.0144624980132,-26.9512924024207,-26.8909711548904,
-26.8306472065173,-26.7703132337501,-26.7617821156432,-26.6998335459311,
-26.639508342525,-26.5791893421032,-26.5188739403131,-26.4557038447214,
-26.3953825971904,-26.3350586488164,-26.2747246760482,-26.2661935579461,
-26.204244988234,-26.1439197848279,-26.0836007844062,-26.0232853826161,
-25.9601152870243,-25.8997940394931,-25.83947009112,-25.7791361183522,-25.770605000249,
-25.7086564305369,-25.6483312271311,-25.5880122267092,-25.5276968249196,
-25.4645267293277,-25.4042054817964,-25.3438815334227,-25.2835475606549,
-25.2750164425519,-25.2130678728398,-25.1527426694337,-25.0924236690117,
-25.0321082672212,-24.9689381716296,-24.9086169240982,-24.8482929757248,
-24.7879590029576,-24.7794278848548,-24.7174793151427,-24.6571541117367,
-24.5968351113151,-24.536519709526,-24.4733496139339,-24.4130283664028,
-24.3527044180278,-24.292370445261,-24.2838393271577,-24.2218907574456,
-24.1615655540396,-24.101246553618,-24.0409311518278,-23.977761056236,-23.9174398087045,
-23.8571158603309,-23.7967818875636,-23.7882507694606,-23.7263021997485,
-23.6659769963423,-23.6056579959201,-23.5453425941303,-23.4821724985386,
-23.4218512510077,-23.361527302633,-23.3011933298654,-23.2926622117635,
-23.2324753090154,-23.1722980607319,-23.1120790869358,-23.0519100205918,
-22.9916660930697,-22.9314221655476),.UNSPECIFIED.) ;
#257 = B_SPLINE_CURVE_WITH_KNOTS('',3,(#34117,#34118,#34119,#34120,#34121,
#34122,#34123,#34124,#34125,#34126,#34127,#34128,#34129,#34130,#34131,#34132,
#34133,#34134,#34135,#34136,#34137,#34138,#34139,#34140,#34141,#34142,#34143,
#34144,#34145,#34146,#34147,#34148,#34149,#34150,#34151,#34152,#34153,#34154,
#34155,#34156,#34157,#34158,#34159,#34160,#34161,#34162,#34163,#34164,#34165,
#34166,#34167,#34168,#34169,#34170,#34171,#34172,#34173,#34174,#34175,#34176,
#34177,#34178,#34179,#34180,#34181,#34182,#34183,#34184,#34185,#34186,#34187,
#34188,#34189,#34190,#34191,#34192,#34193,#34194,#34195,#34196,#34197,#34198,
#34199,#34200,#34201,#34202,#34203,#34204,#34205,#34206,#34207,#34208,#34209,
#34210,#34211,#34212,#34213,#34214,#34215,#34216,#34217,#34218,#34219,#34220,
#34221,#34222,#34223,#34224,#34225,#34226,#34227,#34228,#34229,#34230,#34231,
#34232,#34233,#34234,#34235,#34236,#34237,#34238,#34239,#34240,#34241,#34242,
#34243,#34244,#34245,#34246,#34247,#34248,#34249,#34250,#34251,#34252,#34253,
#34254,#34255,#34256,#34257,#34258,#34259,#34260,#34261,#34262,#34263,#34264,
#34265,#34266,#34267,#34268,#34269,#34270,#34271,#34272,#34273,#34274,#34275,
#34276,#34277,#34278,#34279,#34280,#34281,#34282,#34283,#34284,#34285,#34286,
#34287,#34288,#34289,#34290,#34291,#34292,#34293,#34294,#34295,#34296,#34297,
#34298,#34299,#34300,#34301,#34302,#34303,#34304,#34305,#34306,#34307,#34308,
#34309,#34310,#34311,#34312,#34313,#34314,#34315,#34316,#34317,#34318,#34319,
#34320,#34321,#34322,#34323,#34324,#34325,#34326,#34327,#34328,#34329,#34330,
#34331,#34332,#34333,#34334,#34335,#34336,#34337,#34338,#34339,#34340,#34341,
#34342,#34343,#34344,#34345,#34346,#34347,#34348,#34349,#34350,#34351,#34352,
#34353,#34354,#34355,#34356,#34357,#34358,#34359,#34360,#34361,#34362,#34363,
#34364,#34365,#34366,#34367,#34368,#34369,#34370,#34371,#34372,#34373,#34374,
#34375,#34376,#34377,#34378,#34379,#34380,#34381,#34382,#34383,#34384,#34385,
#34386,#34387,#34388,#34389,#34390,#34391,#34392,#34393,#34394,#34395,#34396,
#34397,#34398,#34399,#34400,#34401,#34402,#34403,#34404,#34405,#34406,#34407,
#34408,#34409,#34410,#34411,#34412,#34413,#34414,#34415,#34416,#34417,#34418,
#34419,#34420,#34421,#34422,#34423,#34424,#34425,#34426,#34427,#34428,#34429,
#34430,#34431,#34432,#34433,#34434,#34435,#34436,#34437,#34438,#34439,#34440,
#34441,#34442,#34443,#34444,#34445,#34446,#34447,#34448,#34449,#34450,#34451,
#34452,#34453,#34454,#34455,#34456),.UNSPECIFIED.,.F.,.F.,(4,3,3,3,3,3,
3,3,3,3,3,3,3,3,3,3,3,3,3,3,3,3,3,3,3,3,3,3,3,3,3,3,3,3,3,3,3,3,3,3,3,3,
3,3,3,3,3,3,3,3,3,3,3,3,3,3,3,3,3,3,3,3,3,3,3,3,3,3,3,3,3,3,3,3,3,3,3,3,
3,3,3,3,3,3,3,3,3,3,3,3,3,3,3,3,3,3,3,3,3,3,3,3,3,3,3,3,3,3,3,3,3,3,3,4),
(19.9596011324501,20.0197790710957,20.079953312403,20.1401332122979,20.2003136007354,
20.2605071303629,20.3191308655809,20.381079435293,20.4414046386991,20.5017236391209,
20.5620390409103,20.6252091365022,20.6855303840333,20.7458543324078,20.8061883051758,
20.814719423278,20.8766679929901,20.9369931963961,20.9973121968177,21.0576275986076,
21.1207976941995,21.1811189417305,21.2414428901052,21.301776862873,21.3103079809751,
21.3722565506872,21.4325817540933,21.492900754515,21.5532161563048,21.6163862518967,
21.6767074994277,21.7370314478021,21.7973654205698,21.8058965386722,21.8678451083843,
21.9281703117903,21.988489312212,22.0488047140018,22.1119748095937,22.1722960571249,
22.2326200054995,22.292953978267,22.3014850963693,22.3634336660814,22.4237588694873,
22.4840778699091,22.5443932716994,22.6075633672911,22.6678846148225,22.7282085631966,
22.7885425359647,22.7970736540664,22.8590222237785,22.9193474271845,22.9796664276061,
23.0399818293961,23.103151924988,23.1634731725189,23.2237971208939,23.2841310936618,
23.2926622117635,23.3546107814756,23.4149359848817,23.4752549853033,23.5355703870933,
23.5987404826852,23.6590617302163,23.7193856785906,23.7797196513582,23.7882507694606,
23.8501993391727,23.9105245425788,23.9708435430002,24.0311589447903,24.0943290403821,
24.1546502879132,24.2149742362876,24.2753082090551,24.2838393271577,24.3457878968698,
24.4061131002758,24.4664321006976,24.5267475024869,24.5899175980789,24.6502388456092,
24.7105627939837,24.7708967667503,24.7794278848548,24.8413764545669,24.9017016579728,
24.9620206583941,25.0223360601837,25.0855061557758,25.145827403307,25.2061513516832,
25.2664853244505,25.2750164425519,25.336965012264,25.3972902156699,25.4576092160917,
25.517924617882,25.5810947134737,25.6414159610052,25.7017399093814,25.7620738821499,
25.770605000249,25.8308224790742,25.8910307598749,25.9512326757154,26.0114310576459,
26.0716348337217,26.1318391994483,26.1920557052503,26.2427864138602),
 .UNSPECIFIED.) ;
#258 = B_SPLINE_CURVE_WITH_KNOTS('',3,(#34461,#34462,#34463,#34464,#34465,
#34466,#34467,#34468,#34469,#34470,#34471,#34472,#34473,#34474,#34475,#34476,
#34477,#34478,#34479,#34480,#34481,#34482,#34483,#34484,#34485,#34486,#34487,
#34488,#34489,#34490,#34491,#34492,#34493,#34494,#34495,#34496,#34497,#34498,
#34499,#34500,#34501,#34502,#34503,#34504,#34505,#34506,#34507,#34508,#34509,
#34510,#34511,#34512,#34513,#34514,#34515,#34516,#34517,#34518,#34519,#34520,
#34521,#34522,#34523,#34524,#34525,#34526,#34527,#34528,#34529,#34530,#34531,
#34532,#34533,#34534,#34535,#34536,#34537,#34538,#34539,#34540,#34541,#34542,
#34543,#34544,#34545,#34546,#34547,#34548,#34549,#34550,#34551,#34552,#34553,
#34554,#34555,#34556,#34557,#34558,#34559,#34560,#34561,#34562,#34563,#34564,
#34565,#34566,#34567,#34568,#34569,#34570,#34571,#34572,#34573,#34574,#34575,
#34576,#34577,#34578,#34579,#34580,#34581,#34582,#34583,#34584,#34585,#34586,
#34587,#34588,#34589,#34590,#34591,#34592,#34593,#34594,#34595,#34596,#34597,
#34598,#34599,#34600,#34601,#34602,#34603,#34604,#34605,#34606,#34607,#34608,
#34609,#34610,#34611,#34612,#34613,#34614,#34615,#34616,#34617,#34618,#34619,
#34620,#34621,#34622,#34623,#34624,#34625,#34626,#34627,#34628,#34629,#34630,
#34631,#34632,#34633,#34634,#34635,#34636,#34637,#34638,#34639,#34640,#34641,
#34642,#34643,#34644,#34645,#34646,#34647,#34648,#34649,#34650,#34651,#34652,
#34653,#34654,#34655,#34656,#34657,#34658,#34659,#34660,#34661,#34662,#34663,
#34664,#34665,#34666,#34667,#34668,#34669,#34670,#34671,#34672,#34673,#34674,
#34675,#34676,#34677,#34678,#34679,#34680,#34681,#34682,#34683,#34684,#34685,
#34686,#34687,#34688,#34689,#34690,#34691,#34692,#34693,#34694,#34695,#34696,
#34697,#34698,#34699,#34700,#34701,#34702,#34703,#34704,#34705,#34706,#34707,
#34708,#34709,#34710,#34711,#34712,#34713,#34714,#34715,#34716,#34717,#34718,
#34719,#34720,#34721,#34722,#34723,#34724,#34725,#34726,#34727,#34728,#34729,
#34730,#34731,#34732,#34733,#34734,#34735,#34736,#34737,#34738,#34739,#34740,
#34741,#34742,#34743,#34744,#34745,#34746,#34747,#34748,#34749,#34750,#34751,
#34752,#34753,#34754,#34755,#34756,#34757,#34758,#34759,#34760,#34761,#34762,
#34763,#34764,#34765,#34766,#34767,#34768,#34769,#34770,#34771,#34772,#34773,
#34774,#34775,#34776,#34777,#34778,#34779,#34780,#34781,#34782,#34783,#34784,
#34785,#34786,#34787,#34788,#34789,#34790,#34791,#34792,#34793,#34794,#34795,
#34796,#34797,#34798,#34799,#34800,#34801,#34802,#34803,#34804,#34805,#34806),
 .UNSPECIFIED.,.F.,.F.,(4,3,3,3,3,3,3,3,3,3,3,3,3,3,3,3,3,3,3,3,3,3,3,3,
3,3,3,3,3,3,3,3,3,3,3,3,3,3,3,3,3,3,3,3,3,3,3,3,3,3,3,3,3,3,3,3,3,3,3,3,
3,3,3,3,3,3,3,3,3,3,3,3,3,3,3,3,3,3,3,3,3,3,3,3,3,3,3,3,3,3,3,3,3,3,3,3,
3,3,3,3,3,3,3,3,3,3,3,3,3,3,3,3,3,3,3,4),(-35.4977927799067,-35.4373549022818,
-35.3747130758348,-35.314266582531,-35.2538167087216,-35.1933564437769,
-35.1867875964938,-35.1248390267817,-35.0645138625596,-35.0041949016703,
-34.9438795396833,-34.8807094144617,-34.8203882070317,-34.7600642987708,
-34.699730365999,-34.6911990387967,-34.6292504690846,-34.5689252380228,
-34.5086062097224,-34.4482907798863,-34.3851207051896,-34.3247994294596,
-34.2644754528975,-34.2041414520523,-34.1956104810996,-34.1336619113875,
-34.0733367226025,-34.0130177369113,-33.9527023499317,-33.8895322432994,
-33.8292110106377,-33.7688870771199,-33.7085531191401,-33.7000219234025,
-33.6380733536904,-33.577748144358,-33.5174291379697,-33.4571137301851,
-33.3939436390652,-33.3336223855255,-33.2732984311522,-33.2129644524189,
-33.2044333657054,-33.1424847959933,-33.0821595941034,-33.0218405952054,
-32.9615251949437,-32.8983550982098,-32.8380338522037,-32.7777099053508,
-32.7173759340923,-32.7088448080083,-32.6468962382962,-32.5865710350704,
-32.5262520348324,-32.4659366332302,-32.4027665375005,-32.3424452901631,
-32.2821213419845,-32.2217873694142,-32.2132562503113,-32.1513076805991,
-32.0909824766373,-32.0306634756543,-31.9703480732994,-31.9071779781281,
-31.8468567300272,-31.7865327810836,-31.7261988077471,-31.7176676926141,
-31.655719122902,-31.5953939199476,-31.5350749199809,-31.4747595186488,
-31.4115894227158,-31.3512681756456,-31.2909442277319,-31.2306102554234,
-31.2220791349171,-31.160130565205,-31.0998053615387,-31.0394863608549,
-30.9791709588018,-30.9160008634064,-30.8556796156103,-30.7953556669706,
-30.7350216939395,-30.72649057722,-30.6645420075079,-30.604216804218,-30.5438978039128,
-30.4835824022401,-30.4204123065608,-30.3600910591481,-30.2997671108904,
-30.2394331382394,-30.2309020195229,-30.1689534498108,-30.108628246368,
-30.0483092459097,-29.9879938440825,-29.9248237485183,-29.8645025009507,
-29.8041785525403,-29.7438445797366,-29.7353134618258,-29.6733648921137,
-29.6130396887101,-29.5527206882902,-29.4924052865024,-29.429235190909,
-29.36891394338,-29.3085899950081,-29.2482560222431,-29.2397249041287,-29.2146074727272),
 .UNSPECIFIED.) ;
#259 = B_SPLINE_CURVE_WITH_KNOTS('',3,(#34807,#34808,#34809,#34810,#34811,
#34812,#34813,#34814,#34815,#34816,#34817,#34818,#34819,#34820,#34821,#34822,
#34823,#34824,#34825,#34826,#34827,#34828,#34829,#34830,#34831,#34832,#34833,
#34834,#34835,#34836,#34837,#34838,#34839,#34840,#34841,#34842,#34843,#34844,
#34845,#34846,#34847,#34848,#34849,#34850,#34851,#34852,#34853,#34854,#34855,
#34856,#34857,#34858,#34859,#34860,#34861,#34862,#34863,#34864,#34865,#34866,
#34867,#34868,#34869,#34870,#34871,#34872,#34873,#34874,#34875,#34876,#34877,
#34878,#34879,#34880,#34881,#34882,#34883,#34884,#34885,#34886,#34887,#34888,
#34889,#34890,#34891,#34892,#34893,#34894,#34895,#34896,#34897,#34898,#34899,
#34900,#34901,#34902,#34903,#34904,#34905,#34906,#34907,#34908,#34909,#34910,
#34911,#34912,#34913,#34914,#34915,#34916,#34917,#34918,#34919,#34920,#34921,
#34922,#34923,#34924,#34925,#34926,#34927,#34928,#34929,#34930,#34931,#34932,
#34933,#34934,#34935,#34936,#34937,#34938,#34939,#34940,#34941,#34942,#34943,
#34944,#34945,#34946,#34947,#34948,#34949,#34950,#34951,#34952,#34953,#34954,
#34955,#34956,#34957,#34958,#34959,#34960,#34961,#34962,#34963,#34964,#34965,
#34966,#34967,#34968,#34969,#34970,#34971,#34972,#34973,#34974,#34975,#34976,
#34977,#34978,#34979,#34980,#34981,#34982,#34983,#34984,#34985,#34986,#34987,
#34988,#34989,#34990,#34991,#34992,#34993,#34994,#34995,#34996,#34997,#34998,
#34999,#35000,#35001,#35002,#35003,#35004,#35005,#35006,#35007,#35008,#35009,
#35010,#35011,#35012,#35013,#35014,#35015,#35016,#35017,#35018,#35019,#35020,
#35021,#35022,#35023,#35024,#35025,#35026,#35027,#35028,#35029,#35030,#35031,
#35032,#35033,#35034,#35035,#35036,#35037,#35038,#35039,#35040,#35041,#35042,
#35043,#35044,#35045,#35046,#35047,#35048,#35049,#35050,#35051,#35052,#35053,
#35054,#35055,#35056,#35057,#35058,#35059,#35060,#35061,#35062,#35063,#35064,
#35065,#35066,#35067,#35068,#35069,#35070,#35071,#35072,#35073,#35074,#35075,
#35076,#35077,#35078,#35079,#35080,#35081,#35082,#35083,#35084,#35085,#35086,
#35087,#35088,#35089,#35090,#35091,#35092,#35093,#35094,#35095,#35096,#35097,
#35098,#35099,#35100,#35101,#35102,#35103,#35104,#35105,#35106,#35107,#35108,
#35109,#35110,#35111,#35112,#35113,#35114,#35115,#35116,#35117,#35118,#35119,
#35120,#35121,#35122,#35123,#35124,#35125,#35126,#35127,#35128,#35129,#35130,
#35131,#35132,#35133,#35134,#35135,#35136,#35137,#35138,#35139,#35140,#35141,
#35142,#35143,#35144,#35145,#35146,#35147,#35148,#35149,#35150,#35151,#35152),
 .UNSPECIFIED.,.F.,.F.,(4,3,3,3,3,3,3,3,3,3,3,3,3,3,3,3,3,3,3,3,3,3,3,3,
3,3,3,3,3,3,3,3,3,3,3,3,3,3,3,3,3,3,3,3,3,3,3,3,3,3,3,3,3,3,3,3,3,3,3,3,
3,3,3,3,3,3,3,3,3,3,3,3,3,3,3,3,3,3,3,3,3,3,3,3,3,3,3,3,3,3,3,3,3,3,3,3,
3,3,3,3,3,3,3,3,3,3,3,3,3,3,3,3,3,3,3,4),(26.2427864396297,26.2661935579461,
26.3281421276582,26.388467331065,26.4487863314875,26.509101733278,26.5722718288693,
26.6325930764013,26.6929170247759,26.7532509975444,26.7617821156432,26.8237306853553,
26.8840558887602,26.9443748891806,27.0046902909692,27.067860386562,27.128181634092,
27.1885055824644,27.2488395552309,27.2573706733403,27.3193192430524,27.3796444464606,
27.4399634468845,27.5002788486765,27.5634489442667,27.6237701918,27.6840941401761,
27.744428112946,27.7529592310374,27.8149078007495,27.875233004151,27.9355520045683,
27.9958674063536,28.0590375019488,28.1193587494755,28.1796826978451,28.2400166706085,
28.2485477887345,28.3104963584466,28.3708215618596,28.4311405622883,28.4914559640852,
28.5546260596718,28.6149473072098,28.6752712555904,28.735605228365,28.7441363464316,
28.8060849161437,28.8664101195424,28.9267291199569,28.9870445217396,29.0502146173369,
29.1105358648609,29.1708598132279,29.2311937859887,29.2397249041287,29.3016734738408,
29.3619986772444,29.4223176776636,29.482633079451,29.5458031750447,29.6061244225732,
29.6664483709447,29.7267823437097,29.7353134618258,29.7972620315379,29.8575872349799,
29.9179062354377,29.9782216372637,30.0413917328285,30.1017129803954,30.1620369288052,
30.2223709016083,30.2309020195229,30.292850589235,30.3531757925255,30.4134947928316,
30.4738101945057,30.5369802901843,30.597301537601,30.6576254858612,30.7179594585165,
30.72649057722,30.7884391469321,30.848764350598,30.9090833512799,30.9693987533295,
31.0325688487264,31.0928900965141,31.1532140451428,31.2135480181622,31.2220791349171,
31.2840277046292,31.3443529075824,31.4046719075513,31.4649873088892,31.5281574048204,
31.5884786519057,31.6488025998371,31.709136572168,31.7176676926141,31.7796162623263,
31.839941466294,31.9002604672771,31.9605758696268,32.0237459647979,32.0840672128796,
32.1443911617988,32.2047251351045,32.2132562503113,32.2737037987142,32.336770785738,
32.397202128338,32.457628314494,32.5180533031214,32.5259717468093),
 .UNSPECIFIED.) ;
#260 = B_SPLINE_CURVE_WITH_KNOTS('',3,(#35159,#35160,#35161,#35162,#35163,
#35164,#35165,#35166,#35167,#35168,#35169,#35170,#35171,#35172,#35173,#35174,
#35175,#35176,#35177,#35178,#35179,#35180,#35181,#35182,#35183,#35184,#35185,
#35186,#35187,#35188,#35189,#35190,#35191,#35192,#35193,#35194,#35195,#35196,
#35197,#35198,#35199,#35200,#35201,#35202,#35203,#35204,#35205,#35206,#35207,
#35208,#35209,#35210,#35211,#35212,#35213,#35214,#35215,#35216,#35217,#35218,
#35219,#35220,#35221,#35222,#35223,#35224,#35225,#35226,#35227,#35228,#35229,
#35230,#35231,#35232,#35233,#35234,#35235,#35236,#35237,#35238,#35239,#35240,
#35241,#35242,#35243,#35244,#35245,#35246,#35247,#35248,#35249,#35250,#35251,
#35252,#35253,#35254,#35255,#35256,#35257,#35258,#35259,#35260,#35261,#35262,
#35263,#35264,#35265,#35266,#35267,#35268,#35269,#35270,#35271,#35272,#35273,
#35274,#35275,#35276,#35277,#35278,#35279,#35280,#35281,#35282,#35283,#35284,
#35285,#35286,#35287,#35288,#35289,#35290,#35291,#35292,#35293,#35294,#35295,
#35296,#35297,#35298,#35299,#35300,#35301,#35302,#35303,#35304,#35305,#35306,
#35307,#35308,#35309,#35310,#35311,#35312,#35313,#35314,#35315,#35316,#35317,
#35318,#35319,#35320,#35321,#35322,#35323,#35324,#35325,#35326,#35327,#35328,
#35329,#35330,#35331,#35332,#35333,#35334,#35335,#35336,#35337,#35338,#35339,
#35340,#35341,#35342,#35343,#35344,#35345,#35346,#35347,#35348,#35349,#35350,
#35351,#35352,#35353,#35354,#35355,#35356,#35357,#35358,#35359,#35360,#35361,
#35362,#35363,#35364,#35365,#35366,#35367,#35368,#35369,#35370,#35371,#35372,
#35373,#35374,#35375,#35376,#35377,#35378,#35379,#35380,#35381,#35382,#35383,
#35384,#35385,#35386,#35387,#35388,#35389,#35390,#35391,#35392,#35393,#35394,
#35395,#35396,#35397,#35398,#35399,#35400,#35401,#35402,#35403,#35404,#35405,
#35406,#35407,#35408,#35409,#35410,#35411,#35412,#35413,#35414,#35415,#35416,
#35417,#35418,#35419,#35420,#35421,#35422,#35423,#35424,#35425,#35426,#35427,
#35428,#35429,#35430,#35431,#35432,#35433,#35434,#35435,#35436,#35437,#35438,
#35439,#35440,#35441,#35442,#35443,#35444,#35445,#35446,#35447,#35448,#35449,
#35450,#35451,#35452,#35453,#35454,#35455,#35456,#35457,#35458,#35459,#35460,
#35461,#35462,#35463,#35464,#35465,#35466,#35467,#35468,#35469,#35470,#35471,
#35472,#35473,#35474,#35475,#35476,#35477,#35478,#35479,#35480,#35481,#35482,
#35483,#35484,#35485,#35486,#35487,#35488,#35489,#35490,#35491,#35492),
 .UNSPECIFIED.,.F.,.F.,(4,3,3,3,3,3,3,3,3,3,3,3,3,3,3,3,3,3,3,3,3,3,3,3,
3,3,3,3,3,3,3,3,3,3,3,3,3,3,3,3,3,3,3,3,3,3,3,3,3,3,3,3,3,3,3,3,3,3,3,3,
3,3,3,3,3,3,3,3,3,3,3,3,3,3,3,3,3,3,3,3,3,3,3,3,3,3,3,3,3,3,3,3,3,3,3,3,
3,3,3,3,3,3,3,3,3,3,3,3,3,3,3,4),(-41.6294388465561,-41.567490276844,-41.5068129036286,
-41.4461373909485,-41.3854619060442,-41.3225590017479,-41.2618724615581,
-41.2011823182609,-41.1404821935598,-41.133850288859,-41.0719017191469,
-41.0117574354034,-40.9516209847975,-40.8914894119347,-40.8313597630322,
-40.7712239022798,-40.7110856043998,-40.650936698952,-40.6382617311619,
-40.5763131614498,-40.5158900890388,-40.4554724366547,-40.3950577994203,
-40.3319616429314,-40.2715406611331,-40.2111170377586,-40.1506838110237,
-40.1426731734648,-40.0807246037527,-40.0204417302746,-39.9601653570302,
-39.8998927959327,-39.8366907508915,-39.7764124738498,-39.7161314439029,
-39.6558401732367,-39.6470846157677,-39.5851360460556,-39.5247976669795,
-39.4644654135086,-39.4041367076079,-39.3409765452236,-39.2806419927029,
-39.2203047694599,-39.1599576085501,-39.1514960580706,-39.0895474883585,
-39.0292231358422,-38.968904978419,-38.9085904100647,-38.8454196826419,
-38.7850992366082,-38.7247760768171,-38.6644428719227,-38.6559075003735,
-38.5939589306614,-38.5336363799959,-38.4733200593599,-38.4130073590988,
-38.3498352549932,-38.2895167377735,-38.2291955234812,-38.1688642808967,
-38.1603189426764,-38.0983703729643,-38.038042569437,-37.9777209466698,
-37.9174029055051,-37.8542347753736,-37.7939108709406,-37.7335842656406,
-37.6732476448322,-37.6647303849793,-37.6027818152672,-37.5424582539623,
-37.4821409085262,-37.4218271713306,-37.3586558353185,-37.2983362606098,
-37.2380139841017,-37.1776816762533,-37.1691418272822,-37.1071932575701,
-37.0468672569077,-36.9865474534408,-36.9262312444077,-36.863061750702,
-36.8027396930987,-36.7424149355172,-36.6820801574679,-36.6735532695851,
-36.611604699873,-36.551279784747,-36.4909610744466,-36.4306459640453,-36.367475651006,
-36.3071546952618,-36.2468310381478,-36.1864973549261,-36.177964711888,
-36.1160161421759,-36.0556908873698,-35.9953718354003,-35.9350563820169,
-35.8718863250604,-35.811565026313,-35.7512410269701,-35.6909070037518,
-35.6823761541909,-35.6203299863175,-35.5582978922954,-35.4977928149021),
 .UNSPECIFIED.) ;
#261 = B_SPLINE_CURVE_WITH_KNOTS('',3,(#35493,#35494,#35495,#35496,#35497,
#35498,#35499,#35500,#35501,#35502,#35503,#35504,#35505,#35506,#35507,#35508,
#35509,#35510,#35511,#35512,#35513,#35514,#35515,#35516,#35517,#35518,#35519,
#35520,#35521,#35522,#35523,#35524,#35525,#35526,#35527,#35528,#35529,#35530,
#35531,#35532,#35533,#35534,#35535,#35536,#35537,#35538,#35539,#35540,#35541,
#35542,#35543,#35544,#35545,#35546,#35547,#35548,#35549,#35550,#35551,#35552,
#35553,#35554,#35555,#35556,#35557,#35558,#35559,#35560,#35561,#35562,#35563,
#35564,#35565,#35566,#35567,#35568,#35569,#35570,#35571,#35572,#35573,#35574,
#35575,#35576,#35577,#35578,#35579,#35580,#35581,#35582,#35583,#35584,#35585,
#35586,#35587,#35588,#35589,#35590,#35591,#35592,#35593,#35594,#35595,#35596,
#35597,#35598,#35599,#35600,#35601,#35602,#35603,#35604,#35605,#35606,#35607,
#35608,#35609,#35610,#35611,#35612,#35613,#35614,#35615,#35616,#35617,#35618,
#35619,#35620,#35621,#35622,#35623,#35624,#35625,#35626,#35627,#35628,#35629,
#35630,#35631,#35632,#35633,#35634,#35635,#35636,#35637,#35638,#35639,#35640,
#35641,#35642,#35643,#35644,#35645,#35646,#35647,#35648,#35649,#35650,#35651,
#35652,#35653,#35654,#35655,#35656,#35657,#35658,#35659,#35660,#35661,#35662,
#35663,#35664,#35665,#35666,#35667,#35668,#35669,#35670,#35671,#35672,#35673,
#35674,#35675,#35676,#35677,#35678,#35679,#35680,#35681,#35682,#35683,#35684,
#35685,#35686,#35687,#35688,#35689,#35690,#35691,#35692,#35693,#35694,#35695,
#35696,#35697,#35698,#35699,#35700,#35701,#35702,#35703,#35704,#35705,#35706,
#35707,#35708,#35709,#35710,#35711,#35712,#35713,#35714,#35715,#35716,#35717,
#35718,#35719,#35720,#35721,#35722,#35723,#35724,#35725,#35726,#35727,#35728,
#35729,#35730,#35731,#35732,#35733,#35734,#35735,#35736,#35737,#35738,#35739,
#35740,#35741,#35742,#35743,#35744,#35745,#35746,#35747,#35748,#35749,#35750,
#35751,#35752,#35753,#35754,#35755,#35756,#35757,#35758,#35759,#35760,#35761,
#35762,#35763,#35764,#35765,#35766,#35767,#35768,#35769,#35770,#35771,#35772,
#35773,#35774,#35775,#35776,#35777,#35778,#35779,#35780,#35781,#35782,#35783,
#35784,#35785,#35786,#35787,#35788,#35789,#35790,#35791,#35792,#35793,#35794,
#35795,#35796,#35797,#35798,#35799,#35800,#35801,#35802,#35803,#35804,#35805,
#35806,#35807,#35808,#35809,#35810,#35811,#35812,#35813,#35814,#35815,#35816,
#35817,#35818,#35819,#35820,#35821,#35822,#35823,#35824,#35825,#35826,#35827,
#35828,#35829,#35830,#35831,#35832,#35833,#35834,#35835),.UNSPECIFIED.,
 .F.,.F.,(4,3,3,3,3,3,3,3,3,3,3,3,3,3,3,3,3,3,3,3,3,3,3,3,3,3,3,3,3,3,3,
3,3,3,3,3,3,3,3,3,3,3,3,3,3,3,3,3,3,3,3,3,3,3,3,3,3,3,3,3,3,3,3,3,3,3,3,
3,3,3,3,3,3,3,3,3,3,3,3,3,3,3,3,3,3,3,3,3,3,3,3,3,3,3,3,3,3,3,3,3,3,3,3,
3,3,3,3,3,3,3,3,3,3,3,4),(32.5259717819584,32.588029893979,32.6501070318688,
32.7088448080084,32.7707933777205,32.8311185796354,32.8914375785607,32.951752978852,
33.0149230755653,33.0752443216065,33.1355682684968,33.1959022397947,33.2044333657054,
33.2663819354175,33.3267071447261,33.3870261510605,33.4473415587615,33.5105116499217,
33.5708329033046,33.6311568574965,33.6914908360153,33.7000219234025,33.7619704931146,
33.8222956818779,33.8826146676421,33.9429300547883,34.0061001613661,34.066421394426,
34.1267453284214,34.1870792869874,34.1956104810996,34.2575590508117,34.3178842820452,
34.3782033103068,34.4385187398944,34.50168881462,34.5620100895816,34.6223340651971,
34.6826680648513,34.6911990387967,34.7531476085088,34.8134727722351,34.8737917329921,
34.9341070952092,34.9972772205304,35.0575984290914,35.1179223387918,35.1782562734283,
35.1867875964938,35.2487361662059,35.3090613994056,35.369380429522,35.4296958608503,
35.4928659341855,35.5531872105891,35.6135111875406,35.6738451883794,35.6823761541909,
35.744324723903,35.8046499773561,35.8649690281093,35.9252844804149,35.9884545382831,
36.0487758363077,36.1090998350517,36.1694338578468,36.177964711888,36.2399132816001,
36.300238197271,36.3605569093567,36.4208720227762,36.4840423344784,36.5443632962832,
36.6046869604949,36.6650206522349,36.6735532695851,36.7355018392972,36.7958278437611,
36.8561476462205,36.9164638494562,36.9796333439127,37.0399553838398,37.1002801196819,
37.1606148704077,37.1691418272822,37.2310903969943,37.291413942665,37.3517312842844,
37.4120450294478,37.4752163683307,37.5355359802912,37.5958583040811,37.6561906730196,
37.6647303849793,37.7266789546914,37.7870067972581,37.8473284367508,37.9076464723714,
37.9708145899476,38.031138433411,38.0914649587342,38.1518014733698,38.1603189426764,
38.2222675123885,38.2825899914703,38.3429062719906,38.4032189635737,38.4663910977737,
38.5267096847223,38.5870309956665,38.6473623720695,38.6559075003735,38.7185947802169,
38.7812660984336,38.8091570245189),.UNSPECIFIED.) ;
#262 = B_SPLINE_CURVE_WITH_KNOTS('',3,(#35841,#35842,#35843,#35844,#35845,
#35846,#35847,#35848,#35849,#35850,#35851,#35852,#35853,#35854,#35855,#35856,
#35857,#35858,#35859,#35860,#35861,#35862,#35863,#35864,#35865,#35866,#35867,
#35868,#35869,#35870,#35871,#35872,#35873,#35874,#35875,#35876,#35877,#35878,
#35879,#35880,#35881,#35882,#35883,#35884,#35885,#35886,#35887,#35888,#35889,
#35890,#35891,#35892,#35893,#35894,#35895,#35896,#35897,#35898,#35899,#35900,
#35901,#35902,#35903,#35904,#35905,#35906,#35907,#35908,#35909,#35910,#35911,
#35912,#35913,#35914,#35915,#35916,#35917,#35918,#35919,#35920,#35921,#35922,
#35923,#35924,#35925,#35926,#35927,#35928,#35929,#35930,#35931,#35932,#35933,
#35934,#35935,#35936,#35937,#35938),.UNSPECIFIED.,.F.,.F.,(4,2,2,2,2,2,
2,2,2,2,2,2,2,2,2,2,2,2,2,2,2,2,2,2,2,2,2,2,2,2,2,2,2,2,2,2,2,2,2,2,2,2,
2,2,2,2,2,2,4),(-8.6283049271654,-8.44563511642056,-8.26252267487022,-8.09546352263789,
-7.93482896054982,-7.81992734806337,-7.62625451933204,-7.42468926409441,
-7.23019569314527,-6.99118982362461,-6.89161836480484,-6.7080558318219,
-6.44464309997694,-6.27048108699121,-6.05333123482325,-5.92170915794646,
-5.81119227905867,-5.63452184767797,-5.42175995687018,-5.23923964233179,
-5.11200558695375,-4.92271658910161,-4.82048727563227,-4.67440773777088,
-4.43080365520216,-4.25778980550549,-4.04526002899663,-3.90739432205506,
-3.79929099426129,-3.63162373705064,-3.42044304635338,-3.24652543009668,
-3.03042830592731,-2.89736788090823,-2.78721938360196,-2.61200305571173,
-2.39899408459298,-2.21760220863657,-1.97106907021256,-1.8636225674043,
-1.67308020303453,-1.4019990020959,-1.22784167090017,-1.01012824950624,
-0.871498618028422,-0.746912125939072,-0.403443808576563,-0.30289397028493,
-1.00000000635703E-6),.UNSPECIFIED.) ;
#263 = B_SPLINE_CURVE_WITH_KNOTS('',3,(#35941,#35942,#35943,#35944,#35945,
#35946,#35947,#35948,#35949,#35950,#35951,#35952,#35953,#35954,#35955,#35956,
#35957,#35958,#35959,#35960,#35961,#35962,#35963,#35964,#35965,#35966,#35967,
#35968,#35969,#35970,#35971,#35972,#35973,#35974,#35975,#35976,#35977,#35978,
#35979,#35980,#35981,#35982,#35983,#35984,#35985,#35986,#35987,#35988,#35989,
#35990,#35991,#35992,#35993,#35994,#35995,#35996,#35997,#35998,#35999,#36000,
#36001,#36002,#36003,#36004,#36005,#36006,#36007,#36008,#36009,#36010,#36011,
#36012),.UNSPECIFIED.,.F.,.F.,(4,2,2,2,2,2,2,2,2,2,2,2,2,2,2,2,2,2,2,2,
2,2,2,2,2,2,2,2,2,2,2,2,2,2,2,4),(-80.5246266814036,-80.1666400655345,-80.0053224599515,
-79.7602571484243,-79.6065532257719,-79.5034892892416,-79.3649560014289,
-79.149023933939,-78.9752478356705,-78.7288342161045,-78.5853061673665,
-78.4835684711015,-78.3013460459308,-78.1711839038137,-77.986351085049,
-77.7720026203175,-77.5968503405372,-77.4864799335814,-77.3241970195642,
-77.124749503217,-76.9556934438728,-76.6796488708706,-76.5012330945668,
-76.3898224188898,-76.1560480763953,-75.9710887556106,-75.7582801102011,
-75.5807809927086,-75.4699172140184,-75.3359737020451,-75.1206153925808,
-74.9470295109835,-74.7403046328623,-74.569427574836,-74.4605084889714,
-74.4589523653195),.UNSPECIFIED.) ;
#264 = B_SPLINE_CURVE_WITH_KNOTS('',3,(#36017,#36018,#36019,#36020,#36021,
#36022,#36023,#36024,#36025,#36026,#36027,#36028,#36029,#36030,#36031,#36032,
#36033,#36034,#36035,#36036,#36037,#36038,#36039,#36040,#36041,#36042,#36043,
#36044,#36045,#36046,#36047,#36048,#36049,#36050,#36051,#36052,#36053,#36054,
#36055,#36056,#36057,#36058,#36059,#36060,#36061,#36062,#36063,#36064,#36065,
#36066,#36067,#36068,#36069,#36070,#36071,#36072,#36073,#36074,#36075,#36076,
#36077,#36078,#36079,#36080,#36081,#36082,#36083,#36084,#36085,#36086,#36087,
#36088,#36089,#36090,#36091,#36092,#36093,#36094,#36095,#36096,#36097,#36098,
#36099,#36100,#36101,#36102,#36103,#36104,#36105,#36106,#36107,#36108,#36109,
#36110,#36111,#36112,#36113,#36114,#36115,#36116,#36117,#36118,#36119,#36120,
#36121,#36122,#36123,#36124,#36125,#36126,#36127,#36128,#36129,#36130,#36131,
#36132,#36133,#36134,#36135,#36136,#36137,#36138,#36139,#36140,#36141,#36142,
#36143,#36144,#36145,#36146,#36147,#36148,#36149,#36150,#36151,#36152,#36153,
#36154,#36155,#36156,#36157,#36158,#36159,#36160),.UNSPECIFIED.,.F.,.F.,
(4,2,2,2,2,2,2,2,2,2,2,2,2,2,2,2,2,2,2,2,2,2,2,2,2,2,2,2,2,2,2,2,2,2,2,
2,2,2,2,2,2,2,2,2,2,2,2,2,2,2,2,2,2,2,2,2,2,2,2,2,2,2,2,2,2,2,2,2,2,2,2,
4),(-21.4112482236887,-21.395018839335,-21.1786168465405,-21.0460115238846,
-20.9359359568184,-20.7609107582667,-20.5479128146165,-20.3669372388779,
-20.1219005459217,-20.01212254847,-19.8210807003159,-19.5511547240092,-19.3765640904682,
-19.1576946106882,-19.0206800954041,-18.8974475163927,-18.5178607380296,
-18.3260088901507,-18.0897196278096,-17.9872267539132,-17.7957545253425,
-17.5358887773981,-17.3619377606238,-17.1456460818616,-17.0129023635293,
-16.9028860341006,-16.7280790286043,-16.5150805001345,-16.3343156219491,
-16.0901169990782,-15.9796193960046,-15.7901984333427,-15.517685168774,
-15.3429409300139,-15.1234403336084,-14.9873344434116,-14.8636672269134,
-14.4862875752506,-14.2959466369376,-14.0612755975542,-13.9567916457698,
-13.7788983270654,-13.5003576759277,-13.3252913165706,-13.10447614829,-12.9775670876658,
-12.8648511184702,-12.6797428835252,-12.4739818922446,-12.2873174175172,
-11.9780281867481,-11.8741210996828,-11.7218506369985,-11.489466218588,
-11.3168413061589,-11.105915354737,-10.9663548850042,-10.8594637224488,
-10.6962625606892,-10.4804969704791,-10.3075555629212,-10.0953574493798,
-9.95702541736544,-9.84903262735902,-9.68177387436709,-9.47012502269245,
-9.29625963443787,-9.08033275022843,-8.94708756555045,-8.83727055637995,
-8.66321978929217,-8.6283049271654),.UNSPECIFIED.) ;
#265 = B_SPLINE_CURVE_WITH_KNOTS('',3,(#36161,#36162,#36163,#36164,#36165,
#36166,#36167,#36168,#36169,#36170,#36171,#36172,#36173,#36174,#36175,#36176,
#36177,#36178,#36179,#36180,#36181,#36182,#36183,#36184,#36185,#36186,#36187,
#36188,#36189,#36190,#36191,#36192,#36193,#36194,#36195,#36196,#36197,#36198,
#36199,#36200,#36201,#36202,#36203,#36204,#36205,#36206,#36207,#36208,#36209,
#36210,#36211,#36212,#36213,#36214,#36215,#36216,#36217,#36218,#36219,#36220,
#36221,#36222,#36223,#36224,#36225,#36226,#36227,#36228,#36229,#36230,#36231,
#36232,#36233,#36234,#36235,#36236,#36237,#36238,#36239,#36240,#36241,#36242,
#36243,#36244,#36245,#36246,#36247,#36248,#36249,#36250,#36251,#36252,#36253,
#36254,#36255,#36256,#36257,#36258,#36259,#36260,#36261,#36262,#36263,#36264,
#36265,#36266,#36267,#36268,#36269,#36270,#36271,#36272,#36273,#36274,#36275,
#36276,#36277,#36278,#36279,#36280,#36281,#36282,#36283,#36284,#36285,#36286,
#36287,#36288,#36289,#36290,#36291,#36292,#36293,#36294,#36295,#36296,#36297,
#36298,#36299,#36300,#36301,#36302,#36303,#36304,#36305,#36306,#36307,#36308,
#36309,#36310,#36311,#36312),.UNSPECIFIED.,.F.,.F.,(4,2,2,2,2,2,2,2,2,2,
2,2,2,2,2,2,2,2,2,2,2,2,2,2,2,2,2,2,2,2,2,2,2,2,2,2,2,2,2,2,2,2,2,2,2,2,
2,2,2,2,2,2,2,2,2,2,2,2,2,2,2,2,2,2,2,2,2,2,2,2,2,2,2,2,2,4),(-74.4589523653195,
-74.3265007778098,-74.1110963267903,-73.9373025312386,-73.7347057927969,
-73.561860568035,-73.4523376858543,-73.3176312089985,-73.1027395663676,
-72.9291097723617,-72.726632241673,-72.5536717587562,-72.4441399440812,
-72.3004543074962,-72.0903185907499,-71.9178862184339,-71.6982031634796,
-71.5382433967428,-71.4322305051113,-71.292424008278,-71.0820984090018,
-70.9095934273694,-70.6889884263145,-70.5295921806519,-70.4237274826831,
-70.2838865719299,-70.0737103989504,-69.9012631469297,-69.6810805418431,
-69.5214303218753,-69.41550305007,-69.2756816129106,-69.0654273530361,-68.8929521476015,
-68.6726317279836,-68.5130705959056,-68.4071647676874,-68.2673383955658,
-68.0571217499896,-67.884661524328,-67.6645673682827,-67.5048663734266,
-67.3989249106178,-67.2591098422661,-67.0488598611346,-66.8763918770729,
-66.658651669558,-66.4974507682909,-66.3911002858384,-66.2513826672066,
-66.0408439496718,-65.8683060418149,-65.6401772541515,-65.4309829879885,
-65.3350553589436,-65.0929076908778,-64.8950377985158,-64.6972644760291,
-64.4491847467691,-64.4060739836119,-64.2986816063683,-64.0508943899226,
-63.8691274930506,-63.6561956981757,-63.4803176045911,-63.3700110952462,
-63.2379366317503,-63.0211171077155,-62.8470246104173,-62.6395444686835,
-62.4692160690279,-62.3603925705269,-62.2244718845535,-62.0105182173817,
-61.8371361301002,-61.6753285154585),.UNSPECIFIED.) ;
#266 = B_SPLINE_CURVE_WITH_KNOTS('',3,(#36317,#36318,#36319,#36320,#36321,
#36322,#36323,#36324,#36325,#36326,#36327,#36328,#36329,#36330,#36331,#36332,
#36333,#36334,#36335,#36336,#36337,#36338,#36339,#36340,#36341,#36342,#36343,
#36344,#36345,#36346,#36347,#36348,#36349,#36350,#36351,#36352,#36353,#36354,
#36355,#36356,#36357,#36358,#36359,#36360,#36361,#36362,#36363,#36364,#36365,
#36366,#36367,#36368,#36369,#36370,#36371,#36372,#36373,#36374,#36375,#36376,
#36377,#36378,#36379,#36380,#36381,#36382,#36383,#36384,#36385,#36386,#36387,
#36388,#36389,#36390,#36391,#36392,#36393,#36394,#36395,#36396,#36397,#36398,
#36399,#36400,#36401,#36402,#36403,#36404,#36405,#36406,#36407,#36408,#36409,
#36410,#36411,#36412,#36413,#36414,#36415,#36416,#36417,#36418,#36419,#36420,
#36421,#36422,#36423,#36424,#36425,#36426,#36427,#36428,#36429,#36430,#36431,
#36432,#36433,#36434,#36435,#36436,#36437,#36438,#36439,#36440,#36441,#36442,
#36443,#36444,#36445,#36446,#36447,#36448,#36449,#36450,#36451,#36452,#36453,
#36454,#36455,#36456,#36457,#36458,#36459,#36460,#36461,#36462,#36463,#36464),
 .UNSPECIFIED.,.F.,.F.,(4,2,2,2,2,2,2,2,2,2,2,2,2,2,2,2,2,2,2,2,2,2,2,2,
2,2,2,2,2,2,2,2,2,2,2,2,2,2,2,2,2,2,2,2,2,2,2,2,2,2,2,2,2,2,2,2,2,2,2,2,
2,2,2,2,2,2,2,2,2,2,2,2,2,4),(-34.1936391063407,-34.1526970834958,-34.0424813560459,
-33.8669170704365,-33.6539735846087,-33.4724917747383,-33.2253958642913,
-33.1173551327557,-32.9264081971104,-32.6582814268131,-32.483810603873,
-32.265402438362,-32.1277449105955,-32.0048155318769,-31.62374016017,-31.4308157047062,
-31.1934125312668,-31.0922100941797,-31.046804554797,-30.9172170606046,
-30.640647352708,-30.4656834280484,-30.2452703249294,-30.1184391905269,
-30.0066984351524,-29.825338795797,-29.6181078581474,-29.4345881974818,
-29.1783538943782,-29.0766484422157,-29.0314901472356,-28.903181133213,
-28.6240155892456,-28.4489244570544,-28.2279958106869,-28.101300372818,
-27.9885874062051,-27.8034838329686,-27.5977287160442,-27.4110695718176,
-27.1017882629211,-26.9978834700024,-26.8456153892239,-26.6132401534391,
-26.4406194907526,-26.2296982363399,-26.090141922616,-25.9832525168262,
-25.8200514725944,-25.6042957006854,-25.4313581532595,-25.2191616273762,
-25.0808395456631,-24.9728489461978,-24.8055916252599,-24.5939515075186,
-24.4200907745686,-24.2041691860031,-24.0709281545374,-23.9611090447325,
-23.7870453902097,-23.569558169572,-23.3864923558574,-23.2164704392175,
-23.0586180687099,-22.9436096408969,-22.7495001276715,-22.5483067922997,
-22.353543415325,-22.1142890470351,-22.0149792499618,-21.8292879644468,
-21.568999457946,-21.4112482236887),.UNSPECIFIED.) ;
#267 = B_SPLINE_CURVE_WITH_KNOTS('',3,(#36465,#36466,#36467,#36468,#36469,
#36470,#36471,#36472,#36473,#36474,#36475,#36476,#36477,#36478,#36479,#36480,
#36481,#36482,#36483,#36484,#36485,#36486,#36487,#36488,#36489,#36490,#36491,
#36492,#36493,#36494,#36495,#36496,#36497,#36498,#36499,#36500,#36501,#36502,
#36503,#36504,#36505,#36506,#36507,#36508,#36509,#36510,#36511,#36512,#36513,
#36514,#36515,#36516,#36517,#36518,#36519,#36520,#36521,#36522,#36523,#36524,
#36525,#36526,#36527,#36528,#36529,#36530,#36531,#36532,#36533,#36534,#36535,
#36536,#36537,#36538,#36539,#36540,#36541,#36542,#36543,#36544,#36545,#36546,
#36547,#36548,#36549,#36550,#36551,#36552,#36553,#36554,#36555,#36556,#36557,
#36558,#36559,#36560,#36561,#36562,#36563,#36564,#36565,#36566,#36567,#36568,
#36569,#36570,#36571,#36572,#36573,#36574,#36575,#36576,#36577,#36578,#36579,
#36580,#36581,#36582,#36583,#36584,#36585,#36586,#36587,#36588,#36589,#36590,
#36591,#36592,#36593,#36594,#36595,#36596,#36597,#36598,#36599,#36600,#36601,
#36602,#36603,#36604,#36605,#36606,#36607,#36608,#36609,#36610,#36611,#36612),
 .UNSPECIFIED.,.F.,.F.,(4,2,2,2,2,2,2,2,2,2,2,2,2,2,2,2,2,2,2,2,2,2,2,2,
2,2,2,2,2,2,2,2,2,2,2,2,2,2,2,2,2,2,2,2,2,2,2,2,2,2,2,2,2,2,2,2,2,2,2,2,
2,2,2,2,2,2,2,2,2,2,2,2,2,4),(-61.6753285154585,-61.6228359350141,-61.4580058246525,
-61.3506687888318,-61.2112613683406,-60.9999976335177,-60.82728245136,-60.6109254773445,
-60.4484481206533,-60.3417516253654,-60.202128704269,-59.9913443765748,
-59.8187492239848,-59.6021458502637,-59.4400166941392,-59.333415823976,
-59.1937688820631,-58.9830552850426,-58.8104791396269,-58.5801878127834,
-58.4266935186611,-58.3224509856121,-58.0123777319399,-57.8258717399889,
-57.6200037585776,-57.4350862756363,-57.3224177640415,-57.1958753725372,
-56.9748722836351,-56.7997560142291,-56.5202163191938,-56.3431495648183,
-56.2386178812058,-56.0039804817052,-55.8136681421047,-55.4363229335071,
-55.3126407866901,-55.1765513551912,-54.9570357797179,-54.7822842467627,
-54.5097109125687,-54.3222211715738,-54.2137989371203,-53.9671522627128,
-53.7857752745581,-53.5728020054108,-53.3973461293979,-53.2871555118113,
-53.1548254634903,-52.9382182238007,-52.7641853742159,-52.5549825616221,
-52.3858738418835,-52.2773823413023,-52.1405410142872,-51.9272766375091,
-51.7540723281387,-51.5071681601972,-51.3121195888342,-51.2138263409947,
-50.973471975645,-50.7775697538017,-50.5777247821068,-50.3307160871589,
-50.2881713296445,-50.1786052451498,-49.9333229491322,-49.7522852299641,
-49.5392844508873,-49.3641886634143,-49.2540937423335,-49.1215300736148,
-48.9050993610572,-48.8923243137223),.UNSPECIFIED.) ;
#268 = B_SPLINE_CURVE_WITH_KNOTS('',3,(#36617,#36618,#36619,#36620,#36621,
#36622,#36623,#36624,#36625,#36626,#36627,#36628,#36629,#36630,#36631,#36632,
#36633,#36634,#36635,#36636,#36637,#36638,#36639,#36640,#36641,#36642,#36643,
#36644,#36645,#36646,#36647,#36648,#36649,#36650,#36651,#36652,#36653,#36654,
#36655,#36656,#36657,#36658,#36659,#36660,#36661,#36662,#36663,#36664,#36665,
#36666,#36667,#36668,#36669,#36670,#36671,#36672,#36673,#36674,#36675,#36676,
#36677,#36678,#36679,#36680,#36681,#36682,#36683,#36684,#36685,#36686,#36687,
#36688,#36689,#36690,#36691,#36692,#36693,#36694,#36695,#36696,#36697,#36698,
#36699,#36700,#36701,#36702,#36703,#36704,#36705,#36706,#36707,#36708,#36709,
#36710,#36711,#36712,#36713,#36714,#36715,#36716,#36717,#36718,#36719,#36720,
#36721,#36722,#36723,#36724,#36725,#36726,#36727,#36728,#36729,#36730,#36731,
#36732,#36733,#36734,#36735,#36736,#36737,#36738,#36739,#36740,#36741,#36742,
#36743,#36744,#36745,#36746,#36747,#36748,#36749,#36750,#36751,#36752,#36753,
#36754,#36755,#36756),.UNSPECIFIED.,.F.,.F.,(4,2,2,2,2,2,2,2,2,2,2,2,2,
2,2,2,2,2,2,2,2,2,2,2,2,2,2,2,2,2,2,2,2,2,2,2,2,2,2,2,2,2,2,2,2,2,2,2,2,
2,2,2,2,2,2,2,2,2,2,2,2,2,2,2,2,2,2,2,2,4),(-46.9761112544596,-46.887959319714,
-46.7131715474143,-46.4396544303016,-46.2630271782697,-46.1624606952762,
-45.924487784234,-45.7310006255373,-45.3491627751212,-45.2263888687142,
-45.0883949216917,-44.8702369915205,-44.6958328063143,-44.4286423908784,
-44.2476883150171,-44.1477658417111,-43.9091656490518,-43.7150557229674,
-43.3323905629399,-43.2097750395941,-43.0714067915801,-42.8534998994136,
-42.6791555505541,-42.41295365977,-42.2267415181231,-42.1241220332522,-41.8879612904891,
-41.6962270516749,-41.3168066906816,-41.1935489113774,-41.0566066379994,
-40.8377084040195,-40.6631167026597,-40.3930248956316,-40.2602686457487,
-40.1614948136577,-39.9712357283276,-39.717589879487,-39.5440241228471,
-39.3292689229644,-39.1944821485798,-39.0852649836751,-38.9134417067484,
-38.7085802334176,-38.5346327441269,-38.3183406707748,-38.1856101147548,
-38.0755933914421,-37.9007777221915,-37.6877856691828,-37.507012703818,
-37.2627670479032,-37.1523202854762,-37.1099843269924,-36.8628889891071,
-36.6625531933715,-36.4670986898819,-36.2271740881804,-36.128511827087,
-35.9372096831459,-35.6850548715227,-35.5115749896293,-35.2971675371291,
-35.1619082853902,-35.0528651788837,-34.8816915200588,-34.6756393220112,
-34.5016007066658,-34.2849409728589,-34.1936391063407),.UNSPECIFIED.) ;
#269 = B_SPLINE_CURVE_WITH_KNOTS('',3,(#36757,#36758,#36759,#36760,#36761,
#36762,#36763,#36764,#36765,#36766,#36767,#36768,#36769,#36770,#36771,#36772,
#36773,#36774,#36775,#36776,#36777,#36778,#36779,#36780,#36781,#36782,#36783,
#36784,#36785,#36786,#36787,#36788,#36789,#36790,#36791,#36792,#36793,#36794,
#36795,#36796,#36797,#36798,#36799,#36800,#36801,#36802,#36803,#36804,#36805,
#36806,#36807,#36808,#36809,#36810,#36811,#36812,#36813,#36814,#36815,#36816,
#36817,#36818,#36819,#36820,#36821,#36822,#36823,#36824,#36825,#36826,#36827,
#36828,#36829,#36830,#36831,#36832,#36833,#36834,#36835,#36836,#36837,#36838,
#36839,#36840,#36841,#36842,#36843,#36844,#36845,#36846,#36847,#36848,#36849,
#36850,#36851,#36852,#36853,#36854,#36855,#36856,#36857,#36858,#36859,#36860,
#36861,#36862,#36863,#36864,#36865,#36866,#36867,#36868,#36869,#36870,#36871,
#36872,#36873,#36874,#36875,#36876,#36877,#36878,#36879,#36880,#36881,#36882,
#36883,#36884,#36885,#36886,#36887,#36888,#36889,#36890,#36891,#36892,#36893,
#36894,#36895,#36896,#36897,#36898,#36899,#36900,#36901,#36902),
 .UNSPECIFIED.,.F.,.F.,(4,2,2,2,2,2,2,2,2,2,2,2,2,2,2,2,2,2,2,2,2,2,2,2,
2,2,2,2,2,2,2,2,2,2,2,2,2,2,2,2,2,2,2,2,2,2,2,2,2,2,2,2,2,2,2,2,2,2,2,2,
2,2,2,2,2,2,2,2,2,2,2,2,4),(-48.8923243137223,-48.7311102437702,-48.4706971753778,
-48.2850805924847,-48.1857596435972,-47.9465181468345,-47.7517652195359,
-47.5505532007241,-47.3564530917116,-47.2414462242878,-47.0837073368052,
-46.9138544860948,-46.7306722642033,-46.518172647404,-46.3406619295693,
-46.2299276804503,-46.0988870050805,-45.881301830456,-45.7070281233357,
-45.4421203801134,-45.2492795993685,-45.1421281434426,-44.8938617393175,
-44.7121152693629,-44.4991963054057,-44.3233385544006,-44.2130416958794,
-44.0809711977412,-43.8641696370465,-43.6900895105923,-43.4824272948797,
-43.3122402199191,-43.2034588723095,-43.0674485332026,-42.8535811826038,
-42.680228459931,-42.3945193861139,-42.271790433139,-42.2277299954773,-42.1233538359875,
-41.8885949478744,-41.6981709741039,-41.3206583063989,-41.197009222143,
-41.060852538196,-40.8413838659923,-40.6666437124145,-40.3942671157565,
-40.2626060616138,-40.1640932887395,-39.9712757348543,-39.7212425122708,
-39.5478712057474,-39.3339324865582,-39.1980079905828,-39.0891951193058,
-38.918893231552,-38.711410109376,-38.5373264214066,-38.3205144570587,-38.1884461808277,
-38.0781473211432,-37.9022844381012,-37.6893683189646,-37.5076112921277,
-37.2597770807576,-37.1524168668946,-36.9755748468808,-36.6921066358992,
-36.5167312594253,-36.294688310285,-36.1710739584292,-36.1093811124386),
 .UNSPECIFIED.) ;
#270 = B_SPLINE_CURVE_WITH_KNOTS('',3,(#36907,#36908,#36909,#36910,#36911,
#36912,#36913,#36914,#36915,#36916,#36917,#36918,#36919,#36920,#36921,#36922,
#36923,#36924,#36925,#36926,#36927,#36928,#36929,#36930,#36931,#36932,#36933,
#36934,#36935,#36936,#36937,#36938,#36939,#36940,#36941,#36942,#36943,#36944,
#36945,#36946,#36947,#36948,#36949,#36950,#36951,#36952,#36953,#36954,#36955,
#36956,#36957,#36958,#36959,#36960,#36961,#36962,#36963,#36964,#36965,#36966,
#36967,#36968,#36969,#36970,#36971,#36972,#36973,#36974,#36975,#36976,#36977,
#36978,#36979,#36980,#36981,#36982,#36983,#36984,#36985,#36986,#36987,#36988,
#36989,#36990,#36991,#36992,#36993,#36994,#36995,#36996,#36997,#36998,#36999,
#37000,#37001,#37002,#37003,#37004,#37005,#37006,#37007,#37008,#37009,#37010,
#37011,#37012,#37013,#37014,#37015,#37016,#37017,#37018,#37019,#37020,#37021,
#37022,#37023,#37024,#37025,#37026,#37027,#37028,#37029,#37030,#37031,#37032,
#37033,#37034,#37035,#37036,#37037,#37038,#37039,#37040,#37041,#37042,#37043,
#37044,#37045,#37046,#37047,#37048,#37049,#37050,#37051,#37052,#37053,#37054,
#37055,#37056),.UNSPECIFIED.,.F.,.F.,(4,2,2,2,2,2,2,2,2,2,2,2,2,2,2,2,2,
2,2,2,2,2,2,2,2,2,2,2,2,2,2,2,2,2,2,2,2,2,2,2,2,2,2,2,2,2,2,2,2,2,2,2,2,
2,2,2,2,2,2,2,2,2,2,2,2,2,2,2,2,2,2,2,2,2,4),(-59.7576642542407,-59.5933744459689,
-59.4338184624438,-59.3279219508154,-59.188111664293,-58.9779089966092,
-58.8054641205551,-58.5851882669472,-58.4256344828241,-58.3197393690206,
-58.1799308625549,-57.9697309211142,-57.7972882660943,-57.577015372777,
-57.4174635456083,-57.3115697652949,-57.1717630540937,-56.9615657795836,
-56.7891253229855,-56.5688551907947,-56.4093054418243,-56.3034130257952,
-56.1636081016588,-55.9534135298879,-55.7809752851254,-55.5607079879421,
-55.4011602717046,-55.2952692091105,-55.1554660753708,-54.9452741896308,
-54.7728381505053,-54.5525736959291,-54.3930280076242,-54.2871382963303,
-54.1473369529504,-53.9371477560825,-53.7647139239242,-53.5444513981186,
-53.3849083145396,-53.279020112319,-53.1392205235918,-52.9290341279034,
-52.7566025303904,-52.5363804760838,-52.3768156488363,-52.2709223086606,
-52.1311259868732,-51.9209375912665,-51.7485070421084,-51.5295534196106,
-51.3691865786828,-51.2630751521756,-51.1233310020683,-50.9129874194926,
-50.7405200698919,-50.5147898879696,-50.3072521043426,-50.2112007438594,
-49.9432253358134,-49.7565323181416,-49.5508157270068,-49.3656601613506,
-49.2529377922316,-49.1261477278738,-48.9052897136255,-48.7302234356747,
-48.4513591565083,-48.2728065805656,-48.1675160513685,-47.9334953291543,
-47.7437434841282,-47.3672580888974,-47.2434274595821,-47.1076791434906,
-46.9761112544596),.UNSPECIFIED.) ;
#271 = B_SPLINE_CURVE_WITH_KNOTS('',3,(#37057,#37058,#37059,#37060,#37061,
#37062,#37063,#37064,#37065,#37066,#37067,#37068,#37069,#37070,#37071,#37072,
#37073,#37074,#37075,#37076,#37077,#37078,#37079,#37080,#37081,#37082,#37083,
#37084,#37085,#37086,#37087,#37088,#37089,#37090,#37091,#37092,#37093,#37094,
#37095,#37096,#37097,#37098,#37099,#37100,#37101,#37102,#37103,#37104,#37105,
#37106,#37107,#37108,#37109,#37110,#37111,#37112,#37113,#37114,#37115,#37116,
#37117,#37118,#37119,#37120,#37121,#37122,#37123,#37124,#37125,#37126,#37127,
#37128,#37129,#37130,#37131,#37132,#37133,#37134,#37135,#37136,#37137,#37138,
#37139,#37140,#37141,#37142,#37143,#37144,#37145,#37146,#37147,#37148,#37149,
#37150,#37151,#37152,#37153,#37154,#37155,#37156,#37157,#37158,#37159,#37160,
#37161,#37162,#37163,#37164,#37165,#37166,#37167,#37168,#37169,#37170,#37171,
#37172,#37173,#37174,#37175,#37176,#37177,#37178,#37179,#37180,#37181,#37182,
#37183,#37184,#37185,#37186,#37187,#37188,#37189,#37190,#37191,#37192,#37193,
#37194,#37195,#37196,#37197,#37198,#37199,#37200,#37201,#37202),
 .UNSPECIFIED.,.F.,.F.,(4,2,2,2,2,2,2,2,2,2,2,2,2,2,2,2,2,2,2,2,2,2,2,2,
2,2,2,2,2,2,2,2,2,2,2,2,2,2,2,2,2,2,2,2,2,2,2,2,2,2,2,2,2,2,2,2,2,2,2,2,
2,2,2,2,2,2,2,2,2,2,2,2,4),(-36.1093811124386,-36.059797019336,-35.8802277972535,
-35.6828168746143,-35.5069094314293,-35.2827111342303,-35.151117375553,
-35.0190731635707,-34.6470151800124,-34.4493600629226,-34.2073681631372,
-34.1113225917796,-33.9041369981001,-33.6734984391581,-33.5009153618648,
-33.2901659340044,-33.1505319122536,-33.0438858079697,-32.8815878157741,
-32.6651157479579,-32.492461697318,-32.2814314033653,-32.1419106931438,
-32.0348828588114,-31.8711850728226,-31.6558375621578,-31.4827493038765,
-31.2699695197905,-31.1324358815375,-31.0241753827991,-30.8559313620608,
-30.645560686355,-30.4715926842249,-30.2552634409984,-30.1225430663045,
-30.0125066105907,-29.8376391204446,-29.6246274794085,-29.4438028008348,
-29.1993945104597,-29.0890593822841,-28.8990471431737,-28.6273506283001,
-28.4526447571417,-28.2333306667098,-28.0969315775383,-27.9733961740721,
-27.5952916723206,-27.4044669019083,-27.1692706080269,-27.0654291954941,
-26.8759947765048,-26.6115868538986,-26.4373403468686,-26.2198756063967,
-26.088660565147,-25.9779984966219,-25.8007665613539,-25.5881753882271,
-25.4052207109607,-25.277012342567,-25.0908300755658,-24.9892704444479,
-24.845701269077,-24.5972924815534,-24.4240009379411,-24.2104076248183,
-24.0739894173798,-23.9653435726816,-23.7956737648866,-23.5872421169101,
-23.4131668872054,-23.3261135788128),.UNSPECIFIED.) ;
#272 = B_SPLINE_CURVE_WITH_KNOTS('',3,(#37207,#37208,#37209,#37210,#37211,
#37212,#37213,#37214,#37215,#37216,#37217,#37218,#37219,#37220,#37221,#37222,
#37223,#37224,#37225,#37226,#37227,#37228,#37229,#37230,#37231,#37232,#37233,
#37234,#37235,#37236,#37237,#37238,#37239,#37240,#37241,#37242,#37243,#37244,
#37245,#37246,#37247,#37248,#37249,#37250,#37251,#37252,#37253,#37254,#37255,
#37256,#37257,#37258,#37259,#37260,#37261,#37262,#37263,#37264,#37265,#37266,
#37267,#37268,#37269,#37270,#37271,#37272,#37273,#37274,#37275,#37276,#37277,
#37278,#37279,#37280,#37281,#37282,#37283,#37284,#37285,#37286,#37287,#37288,
#37289,#37290,#37291,#37292,#37293,#37294,#37295,#37296,#37297,#37298,#37299,
#37300,#37301,#37302,#37303,#37304,#37305,#37306,#37307,#37308,#37309,#37310,
#37311,#37312,#37313,#37314,#37315,#37316,#37317,#37318,#37319,#37320,#37321,
#37322,#37323,#37324,#37325,#37326,#37327,#37328,#37329,#37330,#37331,#37332,
#37333,#37334,#37335,#37336,#37337,#37338,#37339,#37340,#37341,#37342,#37343,
#37344,#37345,#37346,#37347,#37348,#37349,#37350,#37351,#37352,#37353,#37354,
#37355,#37356,#37357,#37358,#37359,#37360,#37361,#37362),.UNSPECIFIED.,
 .F.,.F.,(4,2,2,2,2,2,2,2,2,2,2,2,2,2,2,2,2,2,2,2,2,2,2,2,2,2,2,2,2,2,2,
2,2,2,2,2,2,2,2,2,2,2,2,2,2,2,2,2,2,2,2,2,2,2,2,2,2,2,2,2,2,2,2,2,2,2,2,
2,2,2,2,2,2,2,2,2,2,4),(-72.5408068653678,-72.4391534491535,-72.2954642163267,
-72.0853270421682,-71.9128932356433,-71.6931951744418,-71.5332421280119,
-71.4272305392111,-71.2874223100186,-71.077096347533,-70.9045903798868,
-70.6839783638239,-70.5245839584325,-70.4187192648185,-70.2788769277484,
-70.0686992119904,-69.8962505191355,-69.676056586719,-69.5164108517257,
-69.4104842553953,-69.2706612128027,-69.0604062046357,-68.8879298574234,
-68.6676033055693,-68.5080433944154,-68.4021373891409,-68.262309628792,
-68.05209139734,-67.8796297739851,-67.659319606616,-67.4997525201673,-67.393847081321,
-67.25402236401,-67.0437970512951,-66.8713341719612,-66.6510498184925,-66.4914713007699,
-66.3855629356491,-66.2457405650643,-66.0355178602222,-65.8630570459642,
-65.6427513883988,-65.4831893790932,-65.3772864117109,-65.2374650056748,
-65.0272476019066,-64.8547900216135,-64.6345028319881,-64.474933400994,
-64.3690292788099,-64.2292102574205,-64.0189932278641,-63.8465369725667,
-63.6262448370045,-63.4666821782468,-63.3607806131091,-63.2209630624664,
-63.0107501229198,-62.8382965998372,-62.6180101833715,-62.4584477843913,
-62.3525471496183,-62.2127315202632,-62.0025206188915,-61.8300690621381,
-61.6097848819375,-61.4502248961111,-61.3443256863569,-61.2045118116099,
-60.994303823011,-60.8218545537725,-60.6015729642054,-60.4420151511489,
-60.3361173450703,-60.1963052573786,-59.9860999300074,-59.8136528590843,
-59.7576642542407),.UNSPECIFIED.) ;
#273 = B_SPLINE_CURVE_WITH_KNOTS('',3,(#37363,#37364,#37365,#37366,#37367,
#37368,#37369,#37370,#37371,#37372,#37373,#37374,#37375,#37376,#37377,#37378,
#37379,#37380,#37381,#37382,#37383,#37384,#37385,#37386,#37387,#37388,#37389,
#37390,#37391,#37392,#37393,#37394,#37395,#37396,#37397,#37398,#37399,#37400,
#37401,#37402,#37403,#37404,#37405,#37406,#37407,#37408,#37409,#37410,#37411,
#37412,#37413,#37414,#37415,#37416,#37417,#37418,#37419,#37420,#37421,#37422,
#37423,#37424,#37425,#37426,#37427,#37428,#37429,#37430,#37431,#37432,#37433,
#37434,#37435,#37436,#37437,#37438,#37439,#37440,#37441,#37442,#37443,#37444,
#37445,#37446,#37447,#37448,#37449,#37450,#37451,#37452,#37453,#37454,#37455,
#37456,#37457,#37458,#37459,#37460,#37461,#37462,#37463,#37464,#37465,#37466,
#37467,#37468,#37469,#37470,#37471,#37472,#37473,#37474,#37475,#37476,#37477,
#37478,#37479,#37480,#37481,#37482,#37483,#37484,#37485,#37486,#37487,#37488,
#37489,#37490,#37491,#37492,#37493,#37494,#37495,#37496,#37497,#37498,#37499,
#37500,#37501,#37502,#37503,#37504,#37505,#37506,#37507,#37508),
 .UNSPECIFIED.,.F.,.F.,(4,2,2,2,2,2,2,2,2,2,2,2,2,2,2,2,2,2,2,2,2,2,2,2,
2,2,2,2,2,2,2,2,2,2,2,2,2,2,2,2,2,2,2,2,2,2,2,2,2,2,2,2,2,2,2,2,2,2,2,2,
2,2,2,2,2,2,2,2,2,2,2,2,4),(-23.3261135788128,-23.1964122101452,-23.0642484493351,
-22.9539813882199,-22.778249740813,-22.5653025552382,-22.3836641930565,
-22.1282235208404,-22.0242491936684,-21.8369835871211,-21.5698412106102,
-21.3954151573718,-21.1772412301014,-21.0391945576416,-20.9164167373402,
-20.5344605856882,-20.3408935159719,-20.1028309733555,-20.0023019437154,
-19.8253186808675,-19.5522518367965,-19.3774650802196,-19.1578223420381,
-19.0218904733213,-18.8981241350163,-18.5211803167825,-18.3311315652274,
-18.0967783795858,-17.9918572842245,-17.8015295407976,-17.5365947175085,
-17.3623149656535,-17.1447146028426,-17.0136779253518,-16.9029390390793,
-16.7254157304334,-16.5129199959725,-16.3297211405915,-16.1459749552859,
-16.0078912622961,-15.8998137655918,-15.7322476667436,-15.5209855844207,
-15.3470836956579,-15.1310224393778,-14.9979448674968,-14.8880515511446,
-14.7137223485656,-14.4976288883751,-14.3152746440806,-14.1883830381326,
-13.9980150996916,-13.8955256353688,-13.7484955119404,-13.5066310847622,
-13.3336531396858,-13.1213377043073,-12.9831420011226,-12.8750953885095,
-12.7076522530855,-12.4962138280885,-12.3223183804109,-12.1063015828812,
-11.9731491078745,-11.8632801018285,-11.6890507397833,-11.4723357756697,
-11.2896572000988,-11.1620685942577,-10.9738931175874,-10.8718966904332,
-10.7267076612704,-10.5425049368748),.UNSPECIFIED.) ;
#274 = B_SPLINE_CURVE_WITH_KNOTS('',3,(#37514,#37515,#37516,#37517,#37518,
#37519,#37520,#37521,#37522,#37523,#37524,#37525,#37526,#37527,#37528,#37529,
#37530,#37531,#37532,#37533,#37534,#37535,#37536,#37537,#37538,#37539,#37540,
#37541,#37542,#37543,#37544,#37545,#37546,#37547,#37548,#37549,#37550,#37551,
#37552,#37553,#37554,#37555,#37556,#37557,#37558,#37559,#37560,#37561,#37562,
#37563,#37564,#37565,#37566,#37567,#37568,#37569,#37570,#37571,#37572,#37573,
#37574,#37575,#37576,#37577,#37578,#37579,#37580,#37581,#37582,#37583,#37584,
#37585,#37586,#37587,#37588,#37589,#37590,#37591,#37592,#37593,#37594,#37595,
#37596,#37597,#37598,#37599,#37600,#37601,#37602,#37603,#37604,#37605,#37606,
#37607,#37608,#37609,#37610,#37611,#37612,#37613,#37614,#37615,#37616,#37617,
#37618,#37619,#37620,#37621,#37622,#37623,#37624,#37625,#37626,#37627,#37628,
#37629,#37630,#37631,#37632,#37633,#37634,#37635,#37636,#37637,#37638,#37639,
#37640,#37641,#37642,#37643,#37644,#37645,#37646,#37647,#37648,#37649,#37650,
#37651,#37652,#37653,#37654,#37655,#37656,#37657,#37658,#37659,#37660,#37661,
#37662,#37663,#37664,#37665,#37666,#37667,#37668,#37669,#37670,#37671,#37672,
#37673,#37674,#37675,#37676,#37677,#37678,#37679,#37680,#37681,#37682,#37683,
#37684,#37685,#37686,#37687,#37688,#37689,#37690,#37691,#37692,#37693,#37694,
#37695,#37696,#37697,#37698,#37699,#37700,#37701,#37702,#37703,#37704,#37705,
#37706,#37707,#37708,#37709,#37710,#37711,#37712,#37713,#37714,#37715,#37716,
#37717,#37718,#37719,#37720,#37721,#37722,#37723,#37724,#37725,#37726,#37727,
#37728,#37729,#37730,#37731,#37732,#37733,#37734,#37735,#37736,#37737,#37738,
#37739,#37740,#37741,#37742,#37743,#37744,#37745,#37746,#37747,#37748,#37749,
#37750,#37751,#37752,#37753),.UNSPECIFIED.,.F.,.F.,(4,2,2,2,2,2,2,2,2,2,
2,2,2,2,2,2,2,2,2,2,2,2,2,2,2,2,2,2,2,2,2,2,2,2,2,2,2,2,2,2,2,2,2,2,2,2,
2,2,2,2,2,2,2,2,2,2,2,2,2,2,2,2,2,2,2,2,2,2,2,2,2,2,2,2,2,2,2,2,2,2,2,2,
2,2,2,2,2,2,2,2,2,2,2,2,2,2,2,2,2,2,2,2,2,2,2,2,2,2,2,2,2,2,2,2,2,2,2,2,
2,4),(-7.07001074019559,-6.97214799296548,-6.86257413286767,-6.815076472517,
-6.77781127057839,-6.73435011765435,-6.64787909076555,-6.51661040762408,
-6.38274658248721,-6.34808760339101,-6.32936344415715,-6.30808846045213,
-6.27074207319299,-6.2211598558415,-6.07834832333788,-5.94288381481757,
-5.89779633375777,-5.85982903394297,-5.81931476283132,-5.75073449114823,
-5.70297785800585,-5.52925430061811,-5.44364308355816,-5.41803276265346,
-5.39792813650759,-5.37448251943844,-5.32533346674813,-5.17375247153273,
-5.01651467495703,-4.97144238528326,-4.9334755870355,-4.89294824119181,
-4.82430744727727,-4.77648907560603,-4.60228634462766,-4.51736172903062,
-4.49173201521265,-4.47162424844343,-4.44819645774043,-4.39913656527529,
-4.247686484259,-4.10327612770059,-4.04763579703826,-4.00973399465062,-3.96992400695954,
-3.9053390477792,-3.8233409502829,-3.71812616332203,-3.68973805571307,-3.59319124604815,
-3.56382019913162,-3.5439000307015,-3.51973495493247,-3.46614699626435,
-3.38120386675306,-3.16800726161808,-3.12137332113153,-3.08345076694654,
-3.04365603404235,-2.97918496125071,-2.89740332700571,-2.79191626716292,
-2.77546374061009,-2.67591475821705,-2.64203033053413,-2.62343344176577,
-2.60194884328964,-2.56356273770187,-2.51202638466183,-2.35598119717274,
-2.26681982957397,-2.20328757294974,-2.16365752688015,-2.12518099839849,
-2.06837297332616,-2.00026103662752,-1.83338532789489,-1.73975551249685,
-1.71080075654854,-1.69093948456169,-1.66657999711708,-1.61159897970373,
-1.52303217123091,-1.31734880043544,-1.26458886979624,-1.22676414386914,
-1.1914426910813,-1.13499811808568,-1.06156327628703,-0.855608151594484,
-0.801459131626637,-0.777206119362864,-0.758416903670133,-0.7559933625668,
-0.754383203189016,-0.753152784062996,-0.752131919506535,-0.751234637396342,
-0.750409970413967,-0.749623510843456,-0.748848986992787,-0.748063705107264,
-0.747245569367162,-0.746370635723716,-0.74541057345217,-0.744329492112801,
-0.743079473345434,-0.741593827743262,-0.739776504427147,-0.737485107454084,
-0.734503627617138,-0.730500059700828,-0.696818098040978,-0.627882540733976,
-0.390114315027872,-0.343393722788442,-0.305390732344919,-0.270426232424303,
-0.230894996292773,-1.96849127237957E-5),.UNSPECIFIED.) ;
#275 = B_SPLINE_CURVE_WITH_KNOTS('',3,(#37756,#37757,#37758,#37759,#37760,
#37761,#37762,#37763,#37764,#37765,#37766,#37767,#37768,#37769,#37770,#37771,
#37772,#37773,#37774,#37775,#37776,#37777,#37778,#37779,#37780,#37781,#37782,
#37783,#37784,#37785,#37786,#37787,#37788,#37789,#37790,#37791,#37792,#37793,
#37794,#37795,#37796,#37797,#37798,#37799,#37800,#37801,#37802,#37803,#37804,
#37805,#37806,#37807,#37808,#37809,#37810,#37811,#37812,#37813,#37814,#37815,
#37816,#37817,#37818,#37819,#37820,#37821,#37822,#37823,#37824,#37825,#37826,
#37827,#37828,#37829,#37830,#37831,#37832,#37833,#37834,#37835,#37836,#37837,
#37838,#37839,#37840,#37841,#37842,#37843,#37844,#37845,#37846,#37847,#37848,
#37849,#37850,#37851,#37852,#37853,#37854,#37855,#37856,#37857,#37858,#37859,
#37860,#37861,#37862,#37863,#37864,#37865,#37866,#37867,#37868,#37869,#37870,
#37871,#37872,#37873,#37874,#37875,#37876,#37877,#37878,#37879,#37880,#37881,
#37882,#37883,#37884,#37885,#37886,#37887,#37888,#37889,#37890,#37891,#37892,
#37893,#37894,#37895,#37896,#37897,#37898,#37899,#37900,#37901,#37902,#37903),
 .UNSPECIFIED.,.F.,.F.,(4,2,2,2,2,2,2,2,2,2,2,2,2,2,2,2,2,2,2,2,2,2,2,2,
2,2,2,2,2,2,2,2,2,2,2,2,2,2,2,2,2,2,2,2,2,2,2,2,2,2,2,2,2,2,2,2,2,2,2,2,
2,2,2,2,2,2,2,2,2,2,2,2,2,4),(-30.9360917508779,-30.9172686061639,-30.8923525799296,
-30.7520148786595,-30.5902087215969,-30.5487737722513,-30.5131684200696,
-30.4746533000097,-30.4207200076829,-30.1401595208009,-30.0752894875511,
-30.0431710704356,-30.034244148993,-30.030559360134,-30.0270253893342,-30.0247930648611,
-30.0234480796277,-30.0056381873835,-29.9849208811472,-29.9509450339346,
-29.8001616461514,-29.6825535715349,-29.6247809295708,-29.5852819125843,
-29.5503343290935,-29.5123662271205,-29.4565029910238,-29.2798001519611,
-29.127372093649,-29.0970176100024,-29.0770243913552,-29.0533768770667,
-29.0035447573524,-28.8098233148861,-28.7273054275376,-28.6623184632453,
-28.6221834204209,-28.5838750031023,-28.5273482769931,-28.4143021457096,
-28.2673071730302,-28.2170454955267,-28.1792760863907,-28.1577694941432,
-28.1390211672174,-28.1042164905962,-27.983621445643,-27.8440240607279,
-27.8013736683322,-27.7379011213654,-27.6984264085651,-27.6606470540911,
-27.6140179451516,-27.399599766512,-27.3142149514903,-27.2604789252421,
-27.2363937886926,-27.2165494279139,-27.1874346688687,-27.0921926598196,
-26.9605183436304,-26.8764532442066,-26.8107295661752,-26.7706516210622,
-26.7327487215632,-26.6864909734428,-26.4362394890791,-26.3900300566055,
-26.3353779971005,-26.3109960011018,-26.2910617730222,-26.2618384231154,
-26.1649960376261,-26.1634755787047),.UNSPECIFIED.) ;
#276 = B_SPLINE_CURVE_WITH_KNOTS('',3,(#37906,#37907,#37908,#37909,#37910,
#37911,#37912,#37913,#37914,#37915,#37916,#37917,#37918,#37919,#37920,#37921,
#37922,#37923,#37924,#37925,#37926,#37927,#37928,#37929,#37930,#37931,#37932,
#37933,#37934,#37935,#37936,#37937,#37938,#37939,#37940,#37941,#37942,#37943,
#37944,#37945,#37946,#37947,#37948,#37949,#37950,#37951,#37952,#37953,#37954,
#37955,#37956,#37957,#37958,#37959,#37960,#37961,#37962,#37963,#37964,#37965,
#37966,#37967,#37968,#37969,#37970,#37971,#37972,#37973,#37974,#37975,#37976,
#37977,#37978,#37979,#37980,#37981,#37982,#37983,#37984,#37985,#37986,#37987,
#37988,#37989,#37990,#37991,#37992,#37993,#37994,#37995,#37996,#37997,#37998,
#37999,#38000,#38001,#38002,#38003,#38004,#38005,#38006,#38007,#38008,#38009,
#38010,#38011,#38012,#38013,#38014,#38015,#38016,#38017,#38018,#38019,#38020,
#38021,#38022,#38023,#38024,#38025,#38026,#38027,#38028,#38029,#38030,#38031,
#38032,#38033,#38034,#38035,#38036,#38037,#38038,#38039,#38040,#38041,#38042,
#38043,#38044,#38045,#38046,#38047,#38048,#38049,#38050,#38051,#38052,#38053,
#38054,#38055,#38056,#38057,#38058,#38059,#38060,#38061,#38062,#38063,#38064,
#38065,#38066,#38067,#38068,#38069,#38070,#38071,#38072,#38073,#38074,#38075,
#38076,#38077,#38078,#38079,#38080,#38081,#38082,#38083,#38084,#38085,#38086,
#38087,#38088,#38089,#38090,#38091,#38092,#38093,#38094,#38095,#38096,#38097,
#38098,#38099,#38100,#38101,#38102,#38103,#38104,#38105,#38106,#38107,#38108,
#38109,#38110,#38111,#38112,#38113,#38114,#38115,#38116,#38117,#38118,#38119,
#38120,#38121,#38122,#38123,#38124,#38125,#38126,#38127,#38128,#38129,#38130,
#38131,#38132,#38133,#38134,#38135,#38136,#38137,#38138,#38139,#38140,#38141,
#38142,#38143,#38144,#38145,#38146,#38147,#38148,#38149,#38150,#38151,#38152,
#38153,#38154,#38155,#38156,#38157,#38158,#38159,#38160,#38161,#38162,#38163,
#38164,#38165,#38166,#38167,#38168,#38169,#38170,#38171,#38172,#38173,#38174,
#38175,#38176,#38177,#38178,#38179,#38180,#38181,#38182,#38183,#38184,#38185,
#38186,#38187,#38188,#38189,#38190,#38191,#38192,#38193,#38194,#38195,#38196,
#38197,#38198,#38199,#38200,#38201,#38202,#38203,#38204,#38205,#38206,#38207,
#38208,#38209,#38210,#38211,#38212,#38213,#38214,#38215,#38216,#38217,#38218,
#38219,#38220,#38221,#38222,#38223,#38224,#38225,#38226,#38227,#38228,#38229,
#38230,#38231,#38232,#38233,#38234,#38235,#38236,#38237,#38238,#38239,#38240,
#38241,#38242,#38243,#38244,#38245,#38246,#38247,#38248,#38249,#38250,#38251,
#38252,#38253),.UNSPECIFIED.,.F.,.F.,(4,2,2,2,2,2,2,2,2,2,2,2,2,2,2,2,2,
2,2,2,2,2,2,2,2,2,2,2,2,2,2,2,2,2,2,2,2,2,2,2,2,2,2,2,2,2,2,2,2,2,2,2,2,
2,2,2,2,2,2,2,2,2,2,2,2,2,2,2,2,2,2,2,2,2,2,2,2,2,2,2,2,2,2,2,2,2,2,2,2,
2,2,2,2,2,2,2,2,2,2,2,2,2,2,2,2,2,2,2,2,2,2,2,2,2,2,2,2,2,2,2,2,2,2,2,2,
2,2,2,2,2,2,2,2,2,2,2,2,2,2,2,2,2,2,2,2,2,2,2,2,2,2,2,2,2,2,2,2,2,2,2,2,
2,2,2,2,2,2,2,2,2,2,2,2,4),(-18.7375580075198,-18.4579862149391,-18.4189665915328,
-18.3950896458485,-18.3765503519507,-18.3564393637291,-18.3307942748687,
-18.2435404331931,-18.0711070497076,-18.002110175455,-17.9473726343971,
-17.9121469745524,-17.8746723335695,-17.8194209847092,-17.6491524721797,
-17.5408669391277,-17.4975238639656,-17.466216439978,-17.4657178120353,
-17.4652033870502,-17.4646735204379,-17.4644742782827,-17.4642379308623,
-17.4514439563287,-17.4315024961516,-17.4019551080055,-17.2981709672734,
-17.0915058608801,-17.026191244316,-16.9862503614574,-16.9484199348765,
-16.9021972840528,-16.6842688407334,-16.6016590989677,-16.5489939740601,
-16.5249748299567,-16.5050232052533,-16.4753921015072,-16.3941272611813,
-16.2192353158017,-16.1713310421565,-16.1026095418212,-16.0620700389661,
-16.0241128501855,-15.9790775254471,-15.8391124156287,-15.6996396583568,
-15.6505860584727,-15.6135237322754,-15.5923039017763,-15.5708356149652,
-15.5325076210353,-15.4716811480552,-15.2938771520068,-15.2456114567767,
-15.1765461579765,-15.1359465892385,-15.0980158784726,-15.0446834466261,
-14.7992645355587,-14.7361154894136,-14.6919246450575,-14.6693481043091,
-14.6491422861336,-14.6164600620795,-14.4200521381964,-14.2779941690264,
-14.2287347246425,-14.1913198099039,-14.1489593791614,-14.0718962488988,
-14.0157724419108,-13.8533561274452,-13.8155744269607,-13.7676372195694,
-13.7443988307045,-13.7244580450334,-13.6934549235393,-13.6155297746863,
-13.4402812588759,-13.3923320717822,-13.3235676473882,-13.2830204898403,
-13.245066420483,-13.200047091984,-13.0602747993704,-12.9206195344528,-12.8715365279665,
-12.8344583063442,-12.8132352961779,-12.7944728373515,-12.7595883915594,
-12.6220963203171,-12.4934358876886,-12.4079185211845,-12.364602993916,
-12.3273239633255,-12.279618745961,-12.1674567067921,-12.0015541338996,
-11.9633925239032,-11.9151355134899,-11.891842360134,-11.8719193134874,
-11.846229077102,-11.7583416989424,-11.5864570876021,-11.5389362017157,
-11.4705808491239,-11.4301052145122,-11.3921186562034,-11.3469414307865,
-11.2104010046782,-11.0686129972136,-11.0191911391835,-10.9819306659204,
-10.960671940907,-10.9419353528719,-10.9072032009569,-10.8388377710356,
-10.7140137820564,-10.6045049784185,-10.5405651203629,-10.5008659476202,
-10.4628881492575,-10.415995008236,-10.2045122278261,-10.1189250065178,
-10.0650866756129,-10.0408829515528,-10.0209694345372,-9.99166274633418,
-9.8932218354319,-9.85210782893539,-9.71760557152259,-9.67579407772946,
-9.61309082906137,-9.57360868241256,-9.53548183038103,-9.4784518693945,
-9.36876339638761,-9.24465830736443,-9.15053143643168,-9.12150471572193,
-9.10162210812889,-9.07725134688667,-9.02232972364714,-8.93392214376293,
-8.72837701308831,-8.67568573773897,-8.63784685011571,-8.59702284837532,
-8.52667079192331,-8.43341338631384,-8.23354100927888,-8.19988798492783,
-8.18133139913975,-8.15979651614854,-8.12112799589184,-8.06905216477359,
-7.90911878531789,-7.84122831140762,-7.76847067488092,-7.72723151293331,
-7.6895395441119,-7.63792504560375,-7.46602620876009,-7.3064207474548,-7.27316757229043,
-7.2546757637246,-7.23302751088149,-7.19377779746802,-7.1405877102439,-7.07001074019559),
 .UNSPECIFIED.) ;
#277 = B_SPLINE_CURVE_WITH_KNOTS('',3,(#38255,#38256,#38257,#38258,#38259,
#38260,#38261,#38262,#38263,#38264,#38265,#38266,#38267,#38268,#38269,#38270,
#38271,#38272,#38273,#38274,#38275,#38276,#38277,#38278,#38279,#38280,#38281,
#38282,#38283,#38284,#38285,#38286,#38287,#38288,#38289,#38290,#38291,#38292,
#38293,#38294,#38295,#38296,#38297,#38298,#38299,#38300,#38301,#38302,#38303,
#38304,#38305,#38306,#38307,#38308,#38309,#38310,#38311,#38312,#38313,#38314,
#38315,#38316,#38317,#38318,#38319,#38320,#38321,#38322,#38323,#38324,#38325,
#38326,#38327,#38328,#38329,#38330,#38331,#38332,#38333,#38334,#38335,#38336,
#38337,#38338,#38339,#38340,#38341,#38342,#38343,#38344,#38345,#38346,#38347,
#38348,#38349,#38350,#38351,#38352,#38353,#38354,#38355,#38356,#38357,#38358,
#38359,#38360,#38361,#38362,#38363,#38364,#38365,#38366,#38367,#38368,#38369,
#38370,#38371,#38372,#38373,#38374,#38375,#38376,#38377,#38378,#38379,#38380,
#38381,#38382,#38383,#38384,#38385,#38386,#38387,#38388,#38389,#38390,#38391,
#38392,#38393,#38394,#38395,#38396,#38397,#38398,#38399,#38400,#38401,#38402,
#38403,#38404,#38405,#38406,#38407,#38408,#38409,#38410,#38411,#38412,#38413,
#38414,#38415,#38416,#38417,#38418,#38419,#38420,#38421,#38422,#38423,#38424,
#38425,#38426,#38427,#38428,#38429,#38430,#38431,#38432,#38433,#38434,#38435,
#38436,#38437,#38438,#38439,#38440,#38441,#38442,#38443,#38444,#38445,#38446,
#38447,#38448,#38449,#38450,#38451,#38452,#38453,#38454,#38455,#38456,#38457,
#38458,#38459,#38460,#38461,#38462,#38463,#38464,#38465,#38466,#38467,#38468,
#38469,#38470,#38471,#38472,#38473,#38474,#38475,#38476,#38477,#38478,#38479,
#38480,#38481,#38482,#38483,#38484,#38485,#38486,#38487,#38488,#38489,#38490,
#38491,#38492,#38493,#38494,#38495,#38496,#38497,#38498,#38499,#38500,#38501,
#38502,#38503,#38504,#38505,#38506,#38507,#38508,#38509,#38510,#38511,#38512,
#38513,#38514,#38515,#38516,#38517,#38518,#38519,#38520,#38521,#38522,#38523,
#38524,#38525,#38526,#38527,#38528,#38529,#38530,#38531,#38532,#38533,#38534,
#38535,#38536,#38537,#38538,#38539,#38540,#38541,#38542,#38543,#38544,#38545,
#38546,#38547,#38548,#38549,#38550,#38551,#38552,#38553,#38554,#38555,#38556,
#38557,#38558,#38559,#38560,#38561,#38562,#38563,#38564,#38565,#38566,#38567,
#38568,#38569,#38570,#38571,#38572,#38573,#38574,#38575,#38576,#38577,#38578,
#38579,#38580,#38581,#38582,#38583,#38584,#38585,#38586,#38587,#38588,#38589,
#38590,#38591,#38592,#38593,#38594),.UNSPECIFIED.,.F.,.F.,(4,2,2,2,2,2,
2,2,2,2,2,2,2,2,2,2,2,2,2,2,2,2,2,2,2,2,2,2,2,2,2,2,2,2,2,2,2,2,2,2,2,2,
2,2,2,2,2,2,2,2,2,2,2,2,2,2,2,2,2,2,2,2,2,2,2,2,2,2,2,2,2,2,2,2,2,2,2,2,
2,2,2,2,2,2,2,2,2,2,2,2,2,2,2,2,2,2,2,2,2,2,2,2,2,2,2,2,2,2,2,2,2,2,2,2,
2,2,2,2,2,2,2,2,2,2,2,2,2,2,2,2,2,2,2,2,2,2,2,2,2,2,2,2,2,2,2,2,2,2,2,2,
2,2,2,2,2,2,2,2,2,2,2,2,2,2,2,2,2,2,2,4),(-26.1634755787047,-26.0334578101818,
-25.9504826045188,-25.8853926173577,-25.845512348684,-25.8076959446399,
-25.7524802596143,-25.5601565951091,-25.4664566749428,-25.4095722102639,
-25.3849267470747,-25.3651098408812,-25.3366010798324,-25.2524470344086,
-25.0778485204486,-25.0299764394409,-24.9612816156411,-24.9207429868624,
-24.8827774449592,-24.8377196036669,-24.680749271585,-24.5291081290318,
-24.47990017027,-24.4564407657557,-24.4363330047353,-24.4107237026037,-24.3247986950126,
-24.1513140492844,-24.1035878508508,-24.0350350372646,-23.994522228116,
-23.9565470107593,-23.9029335603355,-23.7800342326202,-23.7631464770853,
-23.6915944362003,-23.6082744927197,-23.5553254744775,-23.5312605194321,
-23.5113191418352,-23.4817705923174,-23.3784408919763,-23.2545749027527,
-23.1712797749366,-23.1060055837674,-23.0660737334587,-23.0282427254408,
-22.9820082805796,-22.7642624404873,-22.6815391212178,-22.6288287860635,
-22.6048036276971,-22.5848537202244,-22.5552366934647,-22.4549707926327,
-22.244644209188,-22.1794742414709,-22.139556268115,-22.1017069034204,-22.0554084880218,
-21.8389686594796,-21.7555482547361,-21.7025598368536,-21.6784878355756,
-21.6585458632077,-21.629002846757,-21.5254158127055,-21.4015473708483,
-21.3183763153513,-21.2531668134287,-21.2132443344753,-21.1754032963411,
-21.1291319650173,-20.9120770749062,-20.8289772122803,-20.7761163517607,
-20.7520663224401,-20.7321212779141,-20.7025461935975,-20.5982709956715,
-20.5751683037172,-20.4329515751015,-20.3427035642946,-20.2986821008092,
-20.2614593501161,-20.2147099154791,-20.1078032032136,-19.9354950561963,
-19.8818222480587,-19.84232239296,-19.82062539022,-19.8021596011287,-19.7690707945252,
-19.5746299471708,-19.4778269621961,-19.4437671476783,-19.3893374251967,
-19.3512414944441,-19.3109881599704,-19.2439038410166,-19.1628658358809,
-19.1298207123143,-19.0598117780832,-18.976431156369,-18.9234587075389,
-18.8993904387056,-18.8794487274373,-18.849903798898,-18.7464455849048,
-18.6225743880683,-18.5393385104102,-18.4740940557718,-18.4341644156287,
-18.3963251901799,-18.3500668533918,-18.1327488461618,-18.0498014893005,
-17.9970010415534,-17.972959813284,-17.9530120082177,-17.9234177827661,
-17.8188701633905,-17.6950080951325,-17.6123680686955,-17.5474392610172,
-17.5075650230533,-17.4696931585916,-17.4142691816239,-17.2224434605133,
-17.1290756929418,-17.0723115543148,-17.0476632564873,-17.0278239029684,
-16.9992329475797,-16.911219304383,-16.7396509046822,-16.6921700598255,
-16.6238522577736,-16.5833822121358,-16.5453911231349,-16.5001967572111,
-16.3595290896939,-16.2209117567024,-16.1719947945481,-16.1350056779493,
-16.1137995674763,-16.0950232893443,-16.0600606581171,-15.9220580798422,
-15.7938067505655,-15.7084393456323,-15.6651456164388,-15.6278626728261,
-15.5801212498485,-15.4682741747646,-15.3431173637202,-15.2403231128215,
-15.2062431753446,-15.1876157061126,-15.1661936280959,-15.128104445325,
-15.0771291151771,-14.9250567613349,-14.8138260063995,-14.7585515137222,
-14.7207029072916,-14.6807888986875,-14.6156342640823,-14.5325682072647,
-14.4958190039446),.UNSPECIFIED.) ;
#278 = B_SPLINE_CURVE_WITH_KNOTS('',3,(#38600,#38601,#38602,#38603,#38604,
#38605,#38606,#38607,#38608,#38609,#38610,#38611,#38612,#38613,#38614,#38615,
#38616,#38617,#38618,#38619,#38620,#38621,#38622,#38623,#38624,#38625,#38626,
#38627,#38628,#38629,#38630,#38631,#38632,#38633,#38634,#38635,#38636,#38637,
#38638,#38639,#38640,#38641,#38642,#38643,#38644,#38645,#38646,#38647,#38648,
#38649,#38650,#38651,#38652,#38653,#38654,#38655,#38656,#38657,#38658,#38659,
#38660,#38661,#38662,#38663,#38664,#38665,#38666,#38667,#38668,#38669,#38670,
#38671,#38672,#38673,#38674,#38675,#38676,#38677,#38678,#38679,#38680,#38681,
#38682,#38683,#38684,#38685,#38686,#38687,#38688,#38689,#38690,#38691,#38692,
#38693,#38694,#38695,#38696,#38697,#38698,#38699,#38700,#38701,#38702,#38703,
#38704,#38705,#38706,#38707,#38708,#38709,#38710,#38711,#38712,#38713,#38714,
#38715,#38716,#38717,#38718,#38719,#38720,#38721,#38722,#38723,#38724,#38725,
#38726,#38727,#38728,#38729,#38730,#38731,#38732,#38733,#38734,#38735,#38736,
#38737,#38738,#38739,#38740,#38741,#38742,#38743,#38744,#38745,#38746,#38747,
#38748,#38749,#38750,#38751,#38752,#38753,#38754,#38755,#38756,#38757,#38758,
#38759,#38760,#38761,#38762,#38763,#38764,#38765,#38766,#38767,#38768,#38769,
#38770,#38771,#38772,#38773,#38774,#38775,#38776,#38777,#38778,#38779,#38780,
#38781,#38782,#38783,#38784,#38785,#38786,#38787,#38788,#38789,#38790,#38791,
#38792,#38793,#38794,#38795,#38796,#38797,#38798,#38799,#38800,#38801,#38802,
#38803,#38804,#38805,#38806,#38807,#38808,#38809,#38810,#38811,#38812,#38813,
#38814,#38815,#38816,#38817,#38818,#38819,#38820,#38821,#38822,#38823,#38824,
#38825,#38826,#38827,#38828,#38829,#38830,#38831,#38832,#38833,#38834,#38835,
#38836,#38837,#38838,#38839,#38840,#38841,#38842,#38843,#38844,#38845,#38846,
#38847,#38848,#38849,#38850,#38851,#38852,#38853,#38854,#38855,#38856,#38857,
#38858,#38859,#38860,#38861,#38862,#38863,#38864,#38865,#38866,#38867,#38868,
#38869,#38870,#38871,#38872,#38873,#38874,#38875,#38876,#38877,#38878,#38879,
#38880,#38881,#38882,#38883,#38884,#38885,#38886,#38887,#38888,#38889,#38890,
#38891,#38892,#38893,#38894,#38895,#38896,#38897,#38898,#38899,#38900,#38901,
#38902,#38903,#38904,#38905,#38906,#38907,#38908,#38909,#38910,#38911,#38912,
#38913,#38914,#38915,#38916,#38917,#38918,#38919,#38920,#38921,#38922,#38923,
#38924,#38925,#38926,#38927,#38928,#38929,#38930,#38931,#38932,#38933,#38934,
#38935,#38936,#38937,#38938,#38939,#38940,#38941,#38942,#38943,#38944,#38945,
#38946,#38947,#38948,#38949,#38950,#38951,#38952,#38953,#38954,#38955,#38956,
#38957,#38958,#38959,#38960,#38961,#38962,#38963,#38964,#38965,#38966,#38967,
#38968,#38969,#38970,#38971,#38972,#38973,#38974,#38975,#38976,#38977,#38978,
#38979,#38980,#38981,#38982,#38983,#38984,#38985,#38986,#38987,#38988,#38989,
#38990,#38991,#38992,#38993,#38994,#38995,#38996,#38997,#38998,#38999,#39000,
#39001,#39002,#39003,#39004,#39005,#39006,#39007,#39008,#39009,#39010,#39011,
#39012,#39013,#39014,#39015,#39016,#39017,#39018,#39019,#39020,#39021,#39022,
#39023,#39024,#39025,#39026,#39027,#39028,#39029,#39030,#39031,#39032,#39033,
#39034,#39035,#39036,#39037,#39038,#39039,#39040,#39041,#39042,#39043,#39044,
#39045,#39046,#39047),.UNSPECIFIED.,.F.,.F.,(4,2,2,2,2,2,2,2,2,2,2,2,2,
2,2,2,2,2,2,2,2,2,2,2,2,2,2,2,2,2,2,2,2,2,2,2,2,2,2,2,2,2,2,2,2,2,2,2,2,
2,2,2,2,2,2,2,2,2,2,2,2,2,2,2,2,2,2,2,2,2,2,2,2,2,2,2,2,2,2,2,2,2,2,2,2,
2,2,2,2,2,2,2,2,2,2,2,2,2,2,2,2,2,2,2,2,2,2,2,2,2,2,2,2,2,2,2,2,2,2,2,2,
2,2,2,2,2,2,2,2,2,2,2,2,2,2,2,2,2,2,2,2,2,2,2,2,2,2,2,2,2,2,2,2,2,2,2,2,
2,2,2,2,2,2,2,2,2,2,2,2,2,2,2,2,2,2,2,2,2,2,2,2,2,2,2,2,2,2,2,2,2,2,2,2,
2,2,2,2,2,2,2,2,2,2,2,2,2,2,2,2,2,2,2,2,2,2,2,2,2,2,2,2,2,2,4),(-11.6673889993071,
-11.6414158400702,-11.574563813691,-11.4494678783821,-11.2996368794634,
-11.2457355278412,-11.2077198576758,-11.1673044897343,-11.09929592368,-11.0521367785433,
-10.883020098933,-10.791878724752,-10.7632000319207,-10.7433526304018,-10.7187624297976,
-10.6623875084877,-10.5700847614003,-10.3719797181445,-10.3186429934542,
-10.2807109571705,-10.2401114659179,-10.1710504826137,-10.122789864657,
-9.9450344115547,-9.88371728784024,-9.84562761555956,-9.8242057096389,-9.80294122763359,
-9.76565255217539,-9.71617859054154,-9.57406061285339,-9.43787150157558,
-9.39272212907696,-9.35474086781874,-9.31425176949696,-9.24582213852396,
-9.19822399215516,-9.02574538146354,-8.93853351698104,-8.91289018339228,
-8.89277914104077,-8.86935672527111,-8.82033933013097,-8.66896001451323,
-8.52441849268399,-8.46878038716984,-8.43087566782274,-8.39105849649317,
-8.32645040204664,-8.24441196995473,-8.1392464068676,-8.11095470271037,
-8.01427096839576,-7.98492889911764,-7.96501121266049,-7.94082773342848,
-7.88712014908426,-7.80186914220275,-7.58948821901505,-7.54273746537615,
-7.50479103653867,-7.46504181575087,-7.40081894061912,-7.35750887844528,
-7.21427302371124,-7.15529565952184,-7.08298489450034,-7.05847113541836,
-7.03856328301299,-7.01432999532432,-6.96030171930695,-6.87422518718765,
-6.66409589106449,-6.6118194202079,-6.57403825712675,-6.53306024102123,
-6.46182006489084,-6.26674497875347,-6.16208775740732,-6.13248527924259,
-6.11253694301691,-6.08850145365457,-6.03573443577002,-5.95286975655572,
-5.73593068717517,-5.6894879676015,-5.6516094364336,-5.61174994372923,-5.54689951350203,
-5.46440551573931,-5.34054763232634,-5.23575780896039,-5.20614345195109,
-5.18619375261828,-5.16216504835746,-5.10944035135405,-5.02668165853167,
-4.80903328253382,-4.76279440965888,-4.72496028014888,-4.68502512561532,
-4.61974424975641,-4.53643800115724,-4.41256755889412,-4.30927179621196,
-4.27972045625702,-4.25977844870596,-4.23571483789555,-4.18276914930895,
-4.09945442821063,-4.02775996688346,-4.01153331695854,-3.88734656622141,
-3.83408553643121,-3.79616515728329,-3.75554128637079,-3.68633732835755,
-3.63792546766863,-3.45892387997426,-3.40815982734118,-3.36473450414089,
-3.34229783286455,-3.32177272874948,-3.28841027202112,-3.24601785790036,
-3.14222177441733,-2.9664581223,-2.91075932621465,-2.87284554315337,-2.8330448517961,
-2.76852779212229,-2.68665930884086,-2.58127511655769,-2.51565062616614,
-2.4495181143703,-2.42337079637734,-2.4036443268204,-2.37743220141496,-2.30894087780662,
-2.17776609758675,-2.1262685594329,-2.01854812418162,-1.97167615226222,
-1.93444879885877,-1.89052670097352,-1.80095296929998,-1.6607640988575,
-1.61024194317157,-1.53271424601636,-1.50202682426316,-1.48193460790729,
-1.46682602892255,-1.46649107583697,-1.46615059335386,-1.46580418068822,
-1.46545142230802,-1.46509188656417,-1.46472512422194,-1.46435066697454,
-1.46396802583975,-1.4635766895023,-1.46317612256954,-1.46276576371511,
-1.46234502373877,-1.46191328348857,-1.46146989169033,-1.46101416264418,
-1.46054537374701,-1.46006276290185,-1.45956552574377,-1.45905281271588,
-1.45852372593188,-1.4579773158531,-1.45741257775742,-1.4568284479894,-1.45622379995191,
-1.45559743985673,-1.4549481021682,-1.45427444480741,-1.45357504398354,
-1.45335387401897,-1.45311011695992,-1.45284129123703,-1.45254461133786,
-1.45221694541013,-1.45185476635826,-1.45145409541343,-1.45101043684475,
-1.45051870253417,-1.44997312487016,-1.44936715631,-1.44869335374756,-1.44794324588435,
-1.44710718164647,-1.44617415778365,-1.44513162420742,-1.44396526597181,
-1.44265876160541,-1.44119351879905,-1.4395483901838,-1.43769937447867,
-1.43561931224237,-1.39307777380501,-1.28858811270789,-1.11266457863325,
-1.05749935428708,-1.02810363060601,-0.998871842682495,-0.951127935374367,
-0.896784254548924,-0.792829289920703,-0.614202334992856,-0.579506851910618,
-0.560776545599971,-0.542649433513584,-0.520930955994243,-0.438846879756886,
-0.435132429627941,-0.293457525354243,-0.170016495734836,-0.122152514992153,
-0.0863789722169139,-0.0514477278305473,-2.04088515964041E-6),
 .UNSPECIFIED.) ;
#279 = B_SPLINE_CURVE_WITH_KNOTS('',3,(#39048,#39049,#39050,#39051,#39052,
#39053,#39054,#39055,#39056,#39057,#39058,#39059,#39060,#39061,#39062,#39063,
#39064,#39065,#39066,#39067,#39068,#39069,#39070,#39071,#39072,#39073,#39074,
#39075,#39076,#39077,#39078,#39079,#39080,#39081,#39082,#39083,#39084,#39085,
#39086,#39087,#39088,#39089,#39090,#39091,#39092,#39093,#39094,#39095,#39096,
#39097,#39098,#39099,#39100,#39101,#39102,#39103,#39104,#39105,#39106,#39107,
#39108,#39109,#39110,#39111,#39112,#39113,#39114,#39115,#39116,#39117,#39118,
#39119,#39120,#39121,#39122,#39123,#39124,#39125,#39126,#39127,#39128,#39129,
#39130,#39131,#39132,#39133,#39134,#39135,#39136,#39137,#39138,#39139,#39140,
#39141,#39142,#39143,#39144,#39145,#39146,#39147,#39148,#39149,#39150,#39151,
#39152,#39153,#39154,#39155,#39156,#39157,#39158,#39159,#39160,#39161,#39162,
#39163,#39164,#39165,#39166,#39167,#39168,#39169,#39170,#39171,#39172,#39173,
#39174,#39175,#39176,#39177,#39178,#39179,#39180,#39181,#39182,#39183,#39184,
#39185,#39186,#39187,#39188,#39189,#39190,#39191,#39192,#39193,#39194,#39195,
#39196,#39197,#39198,#39199,#39200,#39201,#39202,#39203,#39204,#39205,#39206,
#39207,#39208,#39209,#39210,#39211,#39212,#39213,#39214,#39215,#39216,#39217,
#39218,#39219,#39220,#39221,#39222,#39223,#39224,#39225,#39226,#39227,#39228,
#39229,#39230,#39231,#39232,#39233,#39234,#39235,#39236,#39237,#39238,#39239,
#39240,#39241,#39242,#39243,#39244,#39245,#39246,#39247,#39248,#39249,#39250,
#39251,#39252,#39253,#39254,#39255,#39256,#39257,#39258,#39259,#39260,#39261,
#39262,#39263,#39264,#39265,#39266,#39267,#39268,#39269,#39270,#39271,#39272,
#39273,#39274,#39275,#39276,#39277,#39278,#39279,#39280,#39281,#39282,#39283,
#39284,#39285,#39286,#39287,#39288,#39289,#39290,#39291,#39292,#39293,#39294,
#39295,#39296,#39297,#39298,#39299,#39300,#39301,#39302,#39303,#39304,#39305,
#39306,#39307,#39308,#39309,#39310,#39311,#39312,#39313,#39314,#39315,#39316,
#39317,#39318,#39319,#39320,#39321,#39322,#39323,#39324,#39325,#39326,#39327,
#39328,#39329,#39330,#39331,#39332,#39333,#39334,#39335,#39336,#39337,#39338,
#39339,#39340,#39341,#39342,#39343,#39344,#39345,#39346,#39347,#39348,#39349,
#39350,#39351,#39352,#39353,#39354,#39355,#39356,#39357,#39358,#39359,#39360,
#39361,#39362,#39363,#39364,#39365,#39366,#39367,#39368,#39369,#39370,#39371,
#39372,#39373,#39374,#39375,#39376,#39377,#39378,#39379,#39380,#39381,#39382,
#39383),.UNSPECIFIED.,.F.,.F.,(4,2,2,2,2,2,2,2,2,2,2,2,2,2,2,2,2,2,2,2,
2,2,2,2,2,2,2,2,2,2,2,2,2,2,2,2,2,2,2,2,2,2,2,2,2,2,2,2,2,2,2,2,2,2,2,2,
2,2,2,2,2,2,2,2,2,2,2,2,2,2,2,2,2,2,2,2,2,2,2,2,2,2,2,2,2,2,2,2,2,2,2,2,
2,2,2,2,2,2,2,2,2,2,2,2,2,2,2,2,2,2,2,2,2,2,2,2,2,2,2,2,2,2,2,2,2,2,2,2,
2,2,2,2,2,2,2,2,2,2,2,2,2,2,2,2,2,2,2,2,2,2,2,2,2,2,2,2,2,2,2,2,2,2,2,2,
2,2,2,4),(-14.4958190039446,-14.3373580112747,-14.2892645766673,-14.2659988076896,
-14.2458353919106,-14.2146688434469,-14.0720874915304,-13.8858491284987,
-13.8312840022495,-13.7935440679781,-13.7534322144962,-13.6871543830497,
-13.6417767672902,-13.4853593191387,-13.3797252932852,-13.3495916421851,
-13.329575243453,-13.3058213253949,-13.2548079991878,-13.1762655815467,
-12.947765396533,-12.8986464350487,-12.8611514255218,-12.8191761917304,
-12.7420623141319,-12.4866696467823,-12.4371289540817,-12.4136182847426,
-12.3935337433925,-12.3629051488733,-12.3251885068873,-12.2413098127795,
-12.0256913649303,-11.9793452928128,-11.9414867355403,-11.9015893161373,
-11.836529715951,-11.7536432399417,-11.6297751182179,-11.5256561631738,
-11.4960899097444,-11.4761453995416,-11.4520883724604,-11.3991886383168,
-11.3159918858435,-11.0991258788283,-11.0528460253069,-11.015001960363,
-10.9750800429482,-10.9098805554953,-10.7432958967631,-10.6093683514663,
-10.5747075359722,-10.5559825690707,-10.5347057711346,-10.497355721679,
-10.4477677459395,-10.3049250258376,-10.1694961801413,-10.1244102830015,
-10.0864415013633,-10.0459224602998,-9.97732500005632,-9.92955173854313,
-9.75570691724357,-9.6702532905009,-9.64463908730002,-9.62453360736005,
-9.6010917422683,-9.55196070433939,-9.40040044806362,-9.24306493930806,
-9.19799743020723,-9.16003250290041,-9.11950526695179,-9.05086049031395,
-9.00303758733737,-8.82880065026865,-8.74391729420133,-8.7182856712044,
-8.69817673488079,-8.67474615810394,-8.62568187671633,-8.47422725134347,
-8.32983414661231,-8.27419096187223,-8.23628495157328,-8.19646817427363,
-8.13186505488578,-8.04983661421166,-7.9446543047438,-7.91632465043103,
-7.81973292762577,-7.79036065623526,-7.77043920706713,-7.74627248813241,
-7.69267397627321,-7.60770319538625,-7.39459142778028,-7.34794861107074,
-7.31002554400733,-7.27023713204597,-7.20579432265316,-7.12406588933853,
-7.01849447414561,-6.99301117600529,-6.89336047762903,-6.86398960192666,
-6.84406839667928,-6.81990107813924,-6.76629822444857,-6.68131607690297,
-6.46823527272909,-6.42158835331446,-6.38366452062368,-6.34387785454935,
-6.27944415674602,-6.1977325731074,-6.09214050287717,-6.06326256988111,
-5.96680599970245,-5.93752327798759,-5.91761225440428,-5.89339393817029,
-5.83946327651986,-5.75363919801492,-5.54280490221809,-5.49065808921857,
-5.4528943433869,-5.41186601331318,-5.34033653135174,-5.24465911125954,
-5.11984237775976,-5.05028395605779,-5.01609857056104,-4.99745380556073,
-4.97605956254654,-4.93811073441908,-4.88739977756039,-4.73713714189295,
-4.62715388854455,-4.57023292808584,-4.53212351801521,-4.49261641560508,
-4.42977225479692,-4.38782299203269,-4.25254437429793,-4.12492568549646,
-4.09021634206403,-4.07148342536188,-4.05021883608906,-4.01292952283937,
-3.96345434829835,-3.82132844087882,-3.68514808807925,-3.6399994745683,
-3.60201840653155,-3.56152904505586,-3.49309770319846,-3.44549773920924,
-3.27300476488007,-3.1858102547822,-3.1601679109962,-3.14005708743202,-3.11663409172876,
-3.06761314366686,-2.9162282990954,-2.82796833318193),.UNSPECIFIED.) ;
#280 = B_SPLINE_CURVE_WITH_KNOTS('',3,(#39388,#39389,#39390,#39391,#39392,
#39393,#39394,#39395,#39396,#39397,#39398,#39399,#39400,#39401,#39402,#39403,
#39404,#39405,#39406,#39407,#39408,#39409,#39410,#39411,#39412,#39413,#39414,
#39415,#39416,#39417,#39418,#39419,#39420,#39421,#39422,#39423,#39424,#39425,
#39426,#39427,#39428,#39429,#39430,#39431,#39432,#39433,#39434,#39435,#39436,
#39437,#39438,#39439,#39440,#39441,#39442,#39443,#39444,#39445,#39446,#39447,
#39448,#39449,#39450,#39451,#39452,#39453,#39454,#39455,#39456,#39457,#39458,
#39459,#39460,#39461,#39462,#39463,#39464,#39465,#39466,#39467,#39468,#39469,
#39470,#39471,#39472,#39473,#39474,#39475,#39476,#39477,#39478,#39479,#39480,
#39481,#39482,#39483,#39484,#39485,#39486,#39487,#39488,#39489,#39490,#39491,
#39492,#39493,#39494,#39495,#39496,#39497,#39498,#39499,#39500,#39501,#39502,
#39503,#39504,#39505,#39506,#39507,#39508,#39509,#39510,#39511,#39512,#39513,
#39514,#39515,#39516,#39517,#39518,#39519,#39520,#39521,#39522,#39523,#39524,
#39525,#39526,#39527,#39528,#39529,#39530,#39531,#39532,#39533,#39534,#39535,
#39536,#39537,#39538,#39539,#39540,#39541,#39542,#39543,#39544,#39545,#39546,
#39547,#39548,#39549,#39550,#39551,#39552,#39553,#39554,#39555,#39556,#39557,
#39558,#39559,#39560,#39561,#39562,#39563,#39564,#39565,#39566,#39567,#39568,
#39569,#39570,#39571,#39572,#39573,#39574,#39575,#39576,#39577,#39578,#39579,
#39580,#39581,#39582,#39583,#39584,#39585,#39586,#39587,#39588,#39589,#39590,
#39591,#39592,#39593,#39594,#39595,#39596,#39597,#39598,#39599,#39600,#39601,
#39602,#39603,#39604,#39605,#39606,#39607,#39608,#39609,#39610,#39611,#39612,
#39613,#39614,#39615,#39616,#39617,#39618,#39619,#39620,#39621,#39622,#39623,
#39624,#39625,#39626,#39627,#39628,#39629,#39630,#39631,#39632,#39633,#39634,
#39635,#39636,#39637,#39638,#39639,#39640,#39641,#39642,#39643,#39644,#39645,
#39646,#39647,#39648,#39649,#39650,#39651,#39652,#39653,#39654,#39655,#39656,
#39657,#39658,#39659,#39660,#39661,#39662,#39663,#39664,#39665,#39666,#39667,
#39668,#39669,#39670,#39671,#39672,#39673,#39674,#39675,#39676,#39677,#39678,
#39679,#39680,#39681,#39682,#39683,#39684,#39685,#39686,#39687,#39688,#39689,
#39690,#39691,#39692,#39693,#39694,#39695,#39696,#39697,#39698,#39699,#39700,
#39701,#39702,#39703,#39704,#39705,#39706,#39707,#39708,#39709,#39710,#39711,
#39712,#39713,#39714,#39715,#39716,#39717,#39718,#39719,#39720,#39721,#39722,
#39723,#39724,#39725,#39726,#39727,#39728,#39729,#39730,#39731,#39732,#39733,
#39734,#39735,#39736,#39737,#39738,#39739,#39740,#39741,#39742,#39743,#39744,
#39745,#39746,#39747,#39748,#39749,#39750,#39751,#39752,#39753,#39754,#39755,
#39756,#39757,#39758,#39759,#39760,#39761,#39762,#39763,#39764,#39765,#39766,
#39767,#39768,#39769,#39770,#39771,#39772,#39773,#39774,#39775,#39776,#39777,
#39778,#39779),.UNSPECIFIED.,.F.,.F.,(4,2,2,2,2,2,2,2,2,2,2,2,2,2,2,2,2,
2,2,2,2,2,2,2,2,2,2,2,2,2,2,2,2,2,2,2,2,2,2,2,2,2,2,2,2,2,2,2,2,2,2,2,2,
2,2,2,2,2,2,2,2,2,2,2,2,2,2,2,2,2,2,2,2,2,2,2,2,2,2,2,2,2,2,2,2,2,2,2,2,
2,2,2,2,2,2,2,2,2,2,2,2,2,2,2,2,2,2,2,2,2,2,2,2,2,2,2,2,2,2,2,2,2,2,2,2,
2,2,2,2,2,2,2,2,2,2,2,2,2,2,2,2,2,2,2,2,2,2,2,2,2,2,2,2,2,2,2,2,2,2,2,2,
2,2,2,2,2,2,2,2,2,2,2,2,2,2,2,2,2,2,2,2,2,2,2,2,2,2,2,2,2,2,2,2,2,2,4),
(-23.3348397112233,-23.2993172367671,-23.2669907699709,-23.2311740902177,
-23.1832226642003,-23.0578285182112,-22.9159484900769,-22.9124521050827,
-22.832303470825,-22.8106450701826,-22.7924825678868,-22.7737003328901,
-22.7387000238908,-22.5603221831332,-22.4565494278997,-22.4022565325379,
-22.3545258305532,-22.3249389228639,-22.2939916884548,-22.239021017315,
-22.0760469565898,-21.9637527372471,-21.9195901089961,-21.9178419690096,
-21.916568182451,-21.9156417127412,-21.9149686193334,-21.9130725270963,
-21.9113831215892,-21.9098767733616,-21.9085325006564,-21.907331728677,
-21.9062580508492,-21.9052969994771,-21.9044358303664,-21.9036633241023,
-21.9029696051567,-21.9023459790588,-21.901784787155,-21.9012792779261,
-21.9008234936442,-21.9004121709575,-21.9000406540205,-21.8997048187409,
-21.8802652480536,-21.8662520969433,-21.84749733324,-21.8126580356763,-21.6920591698447,
-21.5522998020584,-21.4628701923475,-21.418969195433,-21.3817404211713,
-21.3348411377723,-21.2317368614652,-21.027681516855,-20.9716590136785,
-20.9471217365161,-20.9272666823625,-20.898506883662,-20.8066224826225,
-20.7793855072209,-20.6303414366049,-20.5379163061973,-20.4935845081535,
-20.4563794804764,-20.4100153315694,-20.3116036153469,-20.2930191907013,
-20.247453441294,-20.1176861630082,-20.0702541324799,-20.0340718473344,
-20.0130228466001,-19.991360001033,-19.9520332253064,-19.833261044638,-19.6975645945741,
-19.6095239728515,-19.5658277971769,-19.5285838033317,-19.4814131870597,
-19.3728146795223,-19.2028458265398,-19.1494632485972,-19.1101139362712,
-19.0884467229887,-19.0699659367477,-19.0367806247737,-18.8736215107497,
-18.7334569860586,-18.6682795218591,-18.6283624779642,-18.5905177106118,
-18.5442301628618,-18.2966978568228,-18.2320920446824,-18.1872146957074,
-18.1645139264421,-18.1443653337862,-18.1120286163427,-18.0383448332831,
-17.8619196996226,-17.8138235638719,-17.7449190549555,-17.7043471740428,
-17.6664035806144,-17.6214367948851,-17.4824571593927,-17.3420832662042,
-17.2928852187869,-17.2557449801477,-17.2345097225891,-17.2157559516563,
-17.1809231758297,-17.0664081209725,-16.9604194089774,-16.8790235539479,
-16.8147590459264,-16.7750025587324,-16.7370608076141,-16.6903309771244,
-16.4778103087671,-16.3926109482357,-16.3389235630559,-16.3147432581902,
-16.2948249833002,-16.2654775656503,-16.1688107937782,-16.1405146486189,
-16.0353487870993,-15.9533129918301,-15.888706252311,-15.8488893784422,
-15.8109845857131,-15.7553457168384,-15.610746559667,-15.4593949970142,
-15.4103959631573,-15.3869766688053,-15.3668646835359,-15.3412165793642,
-15.2539205290033,-15.0815165746579,-15.0339283242457,-14.9655081608823,
-14.92502077795,-14.8870388222489,-14.8418858525222,-14.7056531737461,-14.5635732085539,
-14.5141050458567,-14.4768195612773,-14.4555557338694,-14.4368222866574,
-14.4021098083766,-14.2746835941915,-14.1392855571267,-14.097315329346,
-14.0344497216388,-13.9949388714451,-13.9568321545062,-13.8999278188513,
-13.7932230015052,-13.7663699859351,-13.6959834222626,-13.6125862230555,
-13.5596074619825,-13.5355383153788,-13.5155969994046,-13.4860541266841,
-13.3824732918141,-13.1755593667015,-13.1102575285974,-13.0703182074741,
-13.0324854227903,-12.9862549739649,-12.7684338779628,-12.6857621677955,
-12.6330718402318,-12.6090483168674,-12.5890970462745,-12.5594720934808,
-12.4594863109513,-12.2982877355796,-12.2311402042666,-12.1749026291894,
-12.1365217343892,-12.1015045217743,-12.0421914371924,-11.941913865857,
-11.7879382633651,-11.7139919945353,-11.6871599737912,-11.6674293422724,
-11.6673889993071),.UNSPECIFIED.) ;
#281 = B_SPLINE_CURVE_WITH_KNOTS('',3,(#39781,#39782,#39783,#39784,#39785,
#39786,#39787,#39788,#39789,#39790,#39791,#39792,#39793,#39794,#39795,#39796,
#39797,#39798,#39799,#39800,#39801,#39802,#39803,#39804,#39805,#39806,#39807,
#39808,#39809,#39810,#39811,#39812,#39813,#39814,#39815,#39816,#39817,#39818,
#39819,#39820,#39821,#39822,#39823,#39824,#39825,#39826,#39827,#39828,#39829,
#39830,#39831,#39832,#39833,#39834,#39835,#39836,#39837,#39838,#39839,#39840,
#39841,#39842,#39843,#39844,#39845,#39846,#39847,#39848,#39849,#39850,#39851,
#39852,#39853,#39854,#39855,#39856,#39857,#39858,#39859,#39860,#39861,#39862,
#39863,#39864,#39865,#39866,#39867,#39868,#39869,#39870,#39871,#39872,#39873,
#39874,#39875,#39876,#39877,#39878,#39879,#39880,#39881,#39882,#39883,#39884,
#39885,#39886,#39887,#39888,#39889,#39890,#39891,#39892,#39893,#39894,#39895,
#39896,#39897,#39898,#39899,#39900),.UNSPECIFIED.,.F.,.F.,(4,2,2,2,2,2,
2,2,2,2,2,2,2,2,2,2,2,2,2,2,2,2,2,2,2,2,2,2,2,2,2,2,2,2,2,2,2,2,2,2,2,2,
2,2,2,2,2,2,2,2,2,2,2,2,2,2,2,2,2,4),(-2.82796833318193,-2.77169818879921,
-2.71606011920696,-2.67815545324654,-2.63833836198687,-2.57373045869571,
-2.49169232342441,-2.38652668618395,-2.35823445383571,-2.26155274844925,
-2.23221005884666,-2.21229232822597,-2.18810927709837,-2.13440427339247,
-2.04915980214108,-1.83676235265293,-1.79001426271762,-1.75206846843233,
-1.71231840360563,-1.6480904686316,-1.60477534110728,-1.46150870661961,
-1.39838276334144,-1.32958338414609,-1.30533091289941,-1.28546182358305,
-1.27967754629077,-1.27910834204922,-1.27816310482052,-1.2773134432467,
-1.27655559111289,-1.27588483640795,-1.27529565715373,-1.27478190628782,
-1.27433702662791,-1.27395427410561,-1.27362692883975,-1.27334847788875,
-1.27311275978566,-1.27291406723207,-1.27238427551862,-1.2718699315524,
-1.27137139093596,-1.24006028294253,-1.19671105207008,-1.08839688598522,
-0.9181710735731,-0.862918002163598,-0.82544265927117,-0.790217316412342,
-0.735418657931634,-0.666372985295183,-0.49363333447154,-0.406738998577033,
-0.381111444865455,-0.3610037663698,-0.342461169469871,-0.318572664411245,
-0.279521614387501,-1.00000000635703E-6),.UNSPECIFIED.) ;
#282 = B_SPLINE_CURVE_WITH_KNOTS('',3,(#39901,#39902,#39903,#39904,#39905,
#39906,#39907,#39908,#39909,#39910,#39911,#39912,#39913,#39914,#39915,#39916,
#39917,#39918,#39919,#39920,#39921,#39922,#39923,#39924,#39925,#39926,#39927,
#39928,#39929,#39930,#39931,#39932,#39933,#39934,#39935,#39936,#39937,#39938,
#39939,#39940,#39941,#39942,#39943,#39944,#39945,#39946,#39947,#39948,#39949,
#39950,#39951,#39952,#39953,#39954,#39955,#39956,#39957,#39958,#39959,#39960,
#39961,#39962,#39963,#39964,#39965,#39966,#39967,#39968,#39969,#39970,#39971,
#39972,#39973,#39974,#39975,#39976,#39977,#39978,#39979,#39980,#39981,#39982,
#39983,#39984,#39985,#39986,#39987,#39988,#39989,#39990,#39991,#39992,#39993,
#39994,#39995,#39996,#39997,#39998,#39999,#40000,#40001,#40002,#40003,#40004,
#40005,#40006,#40007,#40008,#40009,#40010,#40011,#40012,#40013,#40014,#40015,
#40016,#40017,#40018,#40019,#40020,#40021,#40022,#40023,#40024,#40025,#40026,
#40027,#40028,#40029,#40030,#40031,#40032,#40033,#40034,#40035,#40036,#40037,
#40038,#40039,#40040,#40041,#40042,#40043,#40044,#40045,#40046,#40047,#40048,
#40049,#40050,#40051,#40052,#40053,#40054,#40055,#40056,#40057,#40058,#40059,
#40060,#40061,#40062,#40063,#40064,#40065,#40066,#40067,#40068,#40069,#40070,
#40071,#40072,#40073,#40074,#40075,#40076,#40077,#40078,#40079,#40080,#40081,
#40082,#40083,#40084,#40085,#40086,#40087,#40088,#40089,#40090,#40091,#40092,
#40093,#40094,#40095,#40096,#40097,#40098,#40099,#40100,#40101,#40102,#40103,
#40104,#40105,#40106,#40107,#40108,#40109,#40110,#40111,#40112,#40113,#40114,
#40115,#40116,#40117,#40118,#40119,#40120,#40121,#40122,#40123,#40124,#40125,
#40126,#40127,#40128,#40129,#40130,#40131,#40132,#40133,#40134,#40135,#40136,
#40137,#40138,#40139,#40140,#40141,#40142,#40143,#40144,#40145,#40146,#40147,
#40148,#40149,#40150,#40151,#40152,#40153,#40154,#40155,#40156,#40157,#40158,
#40159,#40160,#40161,#40162,#40163,#40164,#40165,#40166,#40167,#40168,#40169,
#40170,#40171,#40172,#40173,#40174,#40175,#40176,#40177,#40178),
 .UNSPECIFIED.,.F.,.F.,(4,2,2,2,2,2,2,2,2,2,2,2,2,2,2,2,2,2,2,2,2,2,2,2,
2,2,2,2,2,2,2,2,2,2,2,2,2,2,2,2,2,2,2,2,2,2,2,2,2,2,2,2,2,2,2,2,2,2,2,2,
2,2,2,2,2,2,2,2,2,2,2,2,2,2,2,2,2,2,2,2,2,2,2,2,2,2,2,2,2,2,2,2,2,2,2,2,
2,2,2,2,2,2,2,2,2,2,2,2,2,2,2,2,2,2,2,2,2,2,2,2,2,2,2,2,2,2,2,2,2,2,2,2,
2,2,2,2,2,2,4),(-32.1749139758755,-32.1234445413344,-32.0885145288793,-32.0527255510178,
-32.0048303950346,-31.8809426218388,-31.73887653435,-31.6556357235931,-31.6334812934669,
-31.6153322341368,-31.5968705120142,-31.5638047818036,-31.3835735070858,
-31.2787683039668,-31.224188226212,-31.1762912027275,-31.1470066806158,
-31.1176462889212,-31.0626692938337,-30.8843551462058,-30.7812177052451,
-30.7389675472676,-30.7383270818889,-30.7363538389313,-30.7345990938568,
-30.7330371366753,-30.7316452795556,-30.7304035535523,-30.7057319756753,
-30.685212448733,-30.6627650321193,-30.6192818218547,-30.5191256613385,
-30.3755827046354,-30.332222088579,-30.2679484579597,-30.2281904562499,
-30.1902498561424,-30.1435248321897,-29.9309741851585,-29.8457868201532,
-29.7921041792333,-29.7679246649735,-29.748006312417,-29.7186577589798,
-29.6194386270037,-29.4572657456978,-29.4110567724104,-29.3439672486347,
-29.3037135243254,-29.2660470162103,-29.2119652825699,-29.0973255522735,
-29.0661791079758,-28.9384104652755,-28.8708271839429,-28.8447243360711,
-28.8269503209363,-28.8015313391385,-28.7435801251643,-28.6577803337735,
-28.5200387815974,-28.4776591623938,-28.4143767406085,-28.3747929357461,
-28.3367378210081,-28.2801519650378,-28.1725772837586,-28.1419630000505,
-27.9883740115552,-27.9379552638988,-27.9142993004938,-27.8942574170918,
-27.8689675188123,-27.7847630684693,-27.6600735992862,-27.5654110630461,
-27.4943726339059,-27.4534293484341,-27.4156351513558,-27.363265706846,
-27.1536299428732,-27.0673719562485,-27.0132733568616,-26.9890290587264,
-26.9691231505486,-26.9398850335921,-26.837587846541,-26.8116286256321,
-26.6695201160768,-26.579308637423,-26.5352931941648,-26.5018233147707,
-26.4569760599015,-26.3608175362302,-26.3054806974993,-26.1639327835766,
-26.1145483933945,-26.0773078940499,-26.0560528918878,-26.0373131455154,
-26.0025634956857,-25.9342338034163,-25.7572472695213,-25.7090814967771,
-25.6401106156737,-25.5995269377324,-25.5615881301547,-25.5166458687692,
-25.2936575456301,-25.2120228240571,-25.1597480368229,-25.1357906865815,
-25.1158245435788,-25.086078834622,-24.9837408349233,-24.8598634940935,
-24.7762838607387,-24.7108580824416,-24.6708967913419,-24.6330761684987,
-24.5779795501058,-24.3858072049656,-24.2921967120047,-24.2353448226708,
-24.210683816046,-24.1908466327638,-24.1622760018495,-24.0727358870121,
-23.9022662937596,-23.8335777406837,-23.7764342289586,-23.7379050371185,
-23.7030382873186,-23.6447052194208,-23.5384870893744,-23.3875898346536,
-23.3511393588933,-23.3353514234518),.UNSPECIFIED.) ;
#283 = B_SPLINE_CURVE_WITH_KNOTS('',3,(#40183,#40184,#40185,#40186,#40187,
#40188,#40189,#40190,#40191,#40192,#40193,#40194,#40195,#40196,#40197,#40198,
#40199,#40200,#40201,#40202,#40203,#40204,#40205,#40206,#40207,#40208,#40209,
#40210,#40211,#40212,#40213,#40214,#40215,#40216,#40217,#40218,#40219,#40220,
#40221,#40222,#40223,#40224,#40225,#40226,#40227,#40228,#40229,#40230,#40231,
#40232,#40233,#40234,#40235,#40236,#40237,#40238,#40239,#40240,#40241,#40242,
#40243,#40244,#40245,#40246,#40247,#40248,#40249,#40250,#40251,#40252,#40253,
#40254,#40255,#40256,#40257,#40258,#40259,#40260,#40261,#40262,#40263,#40264,
#40265,#40266,#40267,#40268,#40269,#40270,#40271,#40272,#40273,#40274,#40275,
#40276,#40277,#40278,#40279,#40280,#40281,#40282,#40283,#40284,#40285,#40286,
#40287,#40288,#40289,#40290,#40291,#40292,#40293,#40294,#40295,#40296,#40297,
#40298,#40299,#40300,#40301,#40302,#40303,#40304,#40305,#40306,#40307,#40308,
#40309,#40310,#40311,#40312,#40313,#40314,#40315,#40316,#40317,#40318,#40319,
#40320,#40321,#40322,#40323,#40324,#40325,#40326,#40327,#40328,#40329,#40330,
#40331,#40332,#40333,#40334,#40335,#40336,#40337,#40338,#40339,#40340,#40341,
#40342,#40343,#40344,#40345,#40346,#40347,#40348,#40349,#40350,#40351,#40352,
#40353,#40354,#40355,#40356,#40357,#40358,#40359,#40360,#40361,#40362,#40363,
#40364,#40365,#40366,#40367,#40368,#40369,#40370,#40371,#40372,#40373,#40374,
#40375,#40376,#40377,#40378,#40379,#40380,#40381,#40382,#40383,#40384,#40385,
#40386,#40387,#40388,#40389,#40390,#40391,#40392,#40393,#40394,#40395,#40396,
#40397,#40398,#40399,#40400,#40401,#40402,#40403,#40404,#40405,#40406,#40407,
#40408,#40409,#40410,#40411,#40412,#40413,#40414,#40415,#40416,#40417,#40418,
#40419,#40420,#40421,#40422,#40423,#40424,#40425,#40426,#40427,#40428,#40429,
#40430,#40431,#40432,#40433,#40434,#40435,#40436,#40437,#40438,#40439,#40440,
#40441,#40442,#40443,#40444,#40445,#40446,#40447,#40448,#40449,#40450,#40451,
#40452,#40453,#40454,#40455,#40456,#40457,#40458,#40459,#40460,#40461,#40462,
#40463,#40464,#40465,#40466,#40467,#40468,#40469,#40470,#40471,#40472,#40473,
#40474,#40475,#40476,#40477,#40478,#40479,#40480,#40481,#40482,#40483,#40484,
#40485,#40486,#40487,#40488,#40489,#40490,#40491,#40492,#40493,#40494,#40495,
#40496,#40497,#40498,#40499,#40500,#40501,#40502,#40503,#40504,#40505,#40506,
#40507,#40508,#40509,#40510,#40511,#40512,#40513,#40514,#40515,#40516,#40517,
#40518,#40519,#40520,#40521,#40522,#40523,#40524,#40525,#40526,#40527,#40528),
 .UNSPECIFIED.,.F.,.F.,(4,2,2,2,2,2,2,2,2,2,2,2,2,2,2,2,2,2,2,2,2,2,2,2,
2,2,2,2,2,2,2,2,2,2,2,2,2,2,2,2,2,2,2,2,2,2,2,2,2,2,2,2,2,2,2,2,2,2,2,2,
2,2,2,2,2,2,2,2,2,2,2,2,2,2,2,2,2,2,2,2,2,2,2,2,2,2,2,2,2,2,2,2,2,2,2,2,
2,2,2,2,2,2,2,2,2,2,2,2,2,2,2,2,2,2,2,2,2,2,2,2,2,2,2,2,2,2,2,2,2,2,2,2,
2,2,2,2,2,2,2,2,2,2,2,2,2,2,2,2,2,2,2,2,2,2,2,2,2,2,2,2,2,2,2,2,2,2,2,2,
2,2,2,2,4),(-11.6678427707497,-11.6678175290612,-11.6336314550966,-11.5424990175251,
-11.51382078103,-11.4939730324175,-11.4693815468937,-11.4130004897398,-11.3206824183468,
-11.1225442412055,-11.0692274479373,-11.0312976302417,-10.990690078636,
-10.9215866936304,-10.8732819623636,-10.6951708379899,-10.6369369784023,
-10.5973211250985,-10.5756018451578,-10.5545975409668,-10.5186505341154,
-10.4716487990387,-10.3443355835049,-10.3295003766852,-10.1888194348089,
-10.1435413749685,-10.1055327949303,-10.065099664423,-9.99699344885882,
-9.94973323856204,-9.77985593358532,-9.68957805151048,-9.66097249826407,
-9.64113169951097,-9.61649282180796,-9.55979264937159,-9.46660102146701,
-9.2750055228268,-9.21935575517764,-9.181448484148,-9.14163298116555,-9.07703836113052,
-8.99502615575051,-8.88982093324299,-8.86143034680384,-8.76488264372093,
-8.73551216482047,-8.71559079382582,-8.69142271883687,-8.63781631608035,
-8.55282575248703,-8.33976089712768,-8.29311067467974,-8.25518576034033,
-8.21539954934082,-8.15097050509996,-8.06926811964727,-7.9636615432727,
-7.93259790083748,-7.83790849534589,-7.80881444329642,-7.78892414707992,
-7.76459316046365,-7.7099341459535,-7.66369143202974,-7.41212526762461,
-7.36593635765425,-7.32811219161243,-7.28815639564545,-7.22276304848743,
-7.13924501324903,-7.01536646221562,-6.9127043236503,-6.88305025245966,
-6.86309530871848,-6.8390875574717,-6.78649723896041,-6.70407638583837,
-6.48578017493408,-6.43957954906868,-6.40175299482887,-6.36180193944418,
-6.29643471577007,-6.21296597641834,-6.08908911960547,-5.98623839752679,
-5.95662722232766,-5.93667758970236,-5.91264633032177,-5.85990745317786,
-5.77711414845469,-5.55952252414827,-5.51327941410975,-5.47544382428296,
-5.4355091477315,-5.37023414558013,-5.32587148003723,-5.17610582780607,
-5.15702154995673,-5.05870275363856,-5.02963007660712,-5.00974236743992,
-4.9853991386362,-4.93065858616744,-4.88430622739851,-4.63289530046974,
-4.58673579424507,-4.54891841598725,-4.50895234253447,-4.44349799382778,
-4.35986365060906,-4.23598441835955,-4.13404710424258,-4.10416402675081,
-4.08418071905752,-4.06029746899842,-4.00848367057867,-3.92798804788365,
-3.70299751181169,-3.653736982684,-3.61622618653403,-3.5743260164386,-3.49765864507666,
-3.44097870517749,-3.33363210772645,-3.31887184001726,-3.21604777308864,
-3.18196655315214,-3.1633392903041,-3.14191851702691,-3.10383372051061,
-3.05286600650788,-2.90083989264133,-2.78937452912237,-2.73418605816945,
-2.69635170776026,-2.65641625503964,-2.59113472775737,-2.50782750601567,
-2.38395625577425,-2.28066084122462,-2.2511092441252,-2.23116709993902,
-2.20710337112163,-2.1541575766174,-2.07084291212987,-1.85420212691175,
-1.80791403531042,-1.77006921177343,-1.73015249992359,-1.66497661967465,
-1.46380943584966,-1.36307276819266,-1.32913323091078,-1.31052951300075,
-1.29228857727534,-1.27033953391371,-1.23657942584488,-1.16728479137407,
-0.927790949628409,-0.87737059778315,-0.840365950065773,-0.803100134060258,
-0.761758184915453,-0.621177597732689,-0.445029393994813,-0.406453413416984,
-0.384936587192776,-0.366763387244894,-0.345122971337476,-0.312200863253871,
-0.245779091502141,-1.00000000458067E-6),.UNSPECIFIED.) ;
#284 = B_SPLINE_CURVE_WITH_KNOTS('',3,(#40529,#40530,#40531,#40532,#40533,
#40534,#40535,#40536,#40537,#40538,#40539,#40540,#40541,#40542,#40543,#40544,
#40545,#40546,#40547,#40548,#40549,#40550,#40551,#40552,#40553,#40554,#40555,
#40556,#40557,#40558,#40559,#40560,#40561,#40562,#40563,#40564,#40565,#40566,
#40567,#40568,#40569,#40570,#40571,#40572,#40573,#40574,#40575,#40576,#40577,
#40578,#40579,#40580,#40581,#40582,#40583,#40584,#40585,#40586,#40587,#40588,
#40589,#40590,#40591,#40592,#40593,#40594,#40595,#40596,#40597,#40598,#40599,
#40600,#40601,#40602,#40603,#40604,#40605,#40606,#40607,#40608,#40609,#40610,
#40611,#40612,#40613,#40614,#40615,#40616,#40617,#40618,#40619,#40620,#40621,
#40622,#40623,#40624,#40625,#40626,#40627,#40628,#40629,#40630,#40631,#40632,
#40633,#40634,#40635,#40636,#40637,#40638,#40639,#40640,#40641,#40642,#40643,
#40644,#40645,#40646,#40647,#40648,#40649,#40650,#40651,#40652,#40653,#40654,
#40655,#40656,#40657,#40658,#40659,#40660,#40661,#40662,#40663,#40664,#40665,
#40666,#40667,#40668,#40669,#40670,#40671,#40672,#40673,#40674,#40675,#40676,
#40677,#40678,#40679,#40680,#40681,#40682,#40683,#40684,#40685,#40686,#40687,
#40688,#40689,#40690,#40691,#40692,#40693,#40694,#40695,#40696,#40697,#40698,
#40699,#40700,#40701,#40702,#40703,#40704,#40705,#40706,#40707,#40708,#40709,
#40710,#40711,#40712,#40713,#40714,#40715,#40716,#40717,#40718,#40719,#40720,
#40721,#40722,#40723,#40724,#40725,#40726,#40727,#40728,#40729,#40730,#40731,
#40732,#40733,#40734,#40735,#40736,#40737,#40738,#40739,#40740,#40741,#40742,
#40743,#40744,#40745,#40746,#40747,#40748,#40749,#40750,#40751,#40752,#40753,
#40754,#40755,#40756,#40757,#40758,#40759,#40760,#40761,#40762,#40763,#40764,
#40765,#40766,#40767,#40768,#40769,#40770,#40771,#40772,#40773,#40774,#40775,
#40776,#40777,#40778,#40779,#40780,#40781,#40782,#40783,#40784,#40785,#40786,
#40787,#40788,#40789,#40790,#40791,#40792,#40793,#40794,#40795,#40796,#40797,
#40798,#40799,#40800,#40801,#40802,#40803,#40804,#40805,#40806,#40807,#40808,
#40809,#40810,#40811,#40812,#40813,#40814,#40815,#40816,#40817,#40818,#40819,
#40820,#40821,#40822,#40823,#40824,#40825,#40826,#40827,#40828,#40829,#40830,
#40831,#40832,#40833,#40834,#40835,#40836,#40837,#40838,#40839,#40840,#40841,
#40842,#40843,#40844,#40845,#40846,#40847,#40848,#40849,#40850,#40851,#40852,
#40853,#40854,#40855,#40856,#40857,#40858,#40859,#40860,#40861,#40862,#40863,
#40864,#40865,#40866,#40867,#40868),.UNSPECIFIED.,.F.,.F.,(4,2,2,2,2,2,
2,2,2,2,2,2,2,2,2,2,2,2,2,2,2,2,2,2,2,2,2,2,2,2,2,2,2,2,2,2,2,2,2,2,2,2,
2,2,2,2,2,2,2,2,2,2,2,2,2,2,2,2,2,2,2,2,2,2,2,2,2,2,2,2,2,2,2,2,2,2,2,2,
2,2,2,2,2,2,2,2,2,2,2,2,2,2,2,2,2,2,2,2,2,2,2,2,2,2,2,2,2,2,2,2,2,2,2,2,
2,2,2,2,2,2,2,2,2,2,2,2,2,2,2,2,2,2,2,2,2,2,2,2,2,2,2,2,2,2,2,2,2,2,2,2,
2,2,2,2,2,2,2,2,2,2,2,2,2,2,2,2,2,2,2,4),(-23.3353514234518,-23.304336453575,
-23.281294079642,-23.2612840850882,-23.229821444945,-23.1541190155707,-22.977897528171,
-22.9298262389341,-22.8609449829051,-22.8203766943299,-22.7824305977091,
-22.7374538524634,-22.5983246910093,-22.4580803357955,-22.4089024897131,
-22.3717729443308,-22.3505395482959,-22.3317838523465,-22.2969410096231,
-22.1765810732244,-22.0366597186924,-21.9471746377961,-21.9032647347992,
-21.8660355302898,-21.8191451233293,-21.7164608524388,-21.5120261802275,
-21.4559473848375,-21.4314012607999,-21.4115469685829,-21.3827992814526,
-21.2992958957657,-21.0816728163509,-21.0101544844516,-20.9691278405556,
-20.9313630355502,-20.8792104609235,-20.6683991293658,-20.5825633677076,
-20.5286280051641,-20.5044088132735,-20.4844977395687,-20.4599653856239,
-20.3875328247002,-20.1441231857728,-20.0788220747043,-20.0388825825197,
-20.0010492585766,-19.9548176682012,-19.7370054663383,-19.6543268760753,
-19.6016335952436,-19.5776094383401,-19.5576580422244,-19.528033468963,
-19.4280228110715,-19.2668385347409,-19.2207690814492,-19.1538148733074,
-19.1135843371879,-19.0759052612154,-19.0304024690919,-18.9016097494586,
-18.7545389997685,-18.70430236801,-18.6666057156846,-18.6452608895655,-18.6239206275512,
-18.5862471877911,-18.5240761343268,-18.3464164134873,-18.2981674523852,
-18.2291172121456,-18.1885192579184,-18.1505858694052,-18.1056723658765,
-17.9675279960662,-17.8263953691815,-17.7553917397604,-17.7288856825717,
-17.709159565226,-17.6832971146946,-17.6343960574231,-17.5505491160553,
-17.4446689283901,-17.3631835310849,-17.2988705962436,-17.2591049536508,
-17.2211675349858,-17.1744600877133,-16.9617799636402,-16.8766381582123,
-16.8229727789355,-16.7987955566402,-16.7788761186885,-16.7495217937295,
-16.6502024839808,-16.4881035471758,-16.4419044104947,-16.3748238887758,
-16.3345710224327,-16.2969026386361,-16.2514521025166,-16.1203438919195,
-16.0873458892449,-15.9146317727454,-15.8826212314254,-15.8625251603367,
-15.8397009874527,-15.7941362623971,-15.7591093759334,-15.6194755139688,
-15.4796741021172,-15.4346514637233,-15.396695768019,-15.3561481123711,
-15.287386297156,-15.2394406118933,-15.0642288413577,-14.9858793657378,
-14.9550511939247,-14.9349380919672,-14.9115208804347,-14.8625356897023,
-14.7112061105873,-14.5665648564298,-14.5109240705266,-14.4730184917753,
-14.4332011979365,-14.3685948388047,-14.2865602505239,-14.181386408875,
-14.1530778828282,-14.0564409906452,-14.0270820511801,-14.0071621733911,
-13.9829878372708,-13.9293403680683,-13.8442441936181,-13.6314536771025,
-13.5847637994324,-13.5468304089743,-13.5070588478134,-13.4427114666762,
-13.3992777944032,-13.2552948477284,-13.228538501451,-13.1299692058251,
-13.1006549069615,-13.0807402262999,-13.0565401821588,-13.0027273818341,
-12.917206832101,-12.7055402023887,-12.6586759385115,-12.6207040346553,
-12.5809938094974,-12.5169942859756,-12.4071733459207,-12.2102847793757,
-12.1776937999183,-12.1575029135442,-12.1348934026794,-12.0905227261423,
-12.0269946598089,-11.8389652654348,-11.7544461169129,-11.711283458406,
-11.6743418796539,-11.6675240120961),.UNSPECIFIED.) ;
#285 = B_SPLINE_CURVE_WITH_KNOTS('',3,(#40873,#40874,#40875,#40876,#40877,
#40878,#40879,#40880,#40881,#40882,#40883,#40884,#40885,#40886,#40887,#40888,
#40889,#40890,#40891,#40892,#40893,#40894,#40895,#40896,#40897,#40898,#40899,
#40900,#40901,#40902,#40903,#40904,#40905,#40906,#40907,#40908,#40909,#40910,
#40911,#40912,#40913,#40914,#40915,#40916,#40917,#40918,#40919,#40920,#40921,
#40922,#40923,#40924,#40925,#40926,#40927,#40928,#40929,#40930,#40931,#40932,
#40933,#40934,#40935,#40936,#40937,#40938,#40939,#40940,#40941,#40942,#40943,
#40944,#40945,#40946,#40947,#40948,#40949,#40950,#40951,#40952,#40953,#40954,
#40955,#40956,#40957,#40958,#40959,#40960,#40961,#40962,#40963,#40964,#40965,
#40966,#40967,#40968,#40969,#40970,#40971,#40972,#40973,#40974,#40975,#40976,
#40977,#40978,#40979,#40980,#40981,#40982,#40983,#40984,#40985,#40986,#40987,
#40988,#40989,#40990,#40991,#40992,#40993,#40994,#40995,#40996,#40997,#40998,
#40999,#41000,#41001,#41002,#41003,#41004,#41005,#41006,#41007,#41008,#41009,
#41010,#41011,#41012,#41013,#41014,#41015,#41016,#41017,#41018,#41019,#41020,
#41021,#41022,#41023,#41024,#41025,#41026,#41027,#41028,#41029,#41030,#41031,
#41032,#41033,#41034,#41035,#41036,#41037,#41038,#41039,#41040,#41041,#41042,
#41043,#41044,#41045,#41046,#41047,#41048,#41049,#41050,#41051,#41052,#41053,
#41054,#41055,#41056,#41057,#41058,#41059,#41060,#41061,#41062,#41063,#41064,
#41065,#41066,#41067,#41068,#41069,#41070,#41071,#41072,#41073,#41074,#41075,
#41076,#41077,#41078,#41079,#41080,#41081,#41082,#41083,#41084,#41085,#41086,
#41087,#41088,#41089,#41090,#41091,#41092,#41093,#41094,#41095,#41096,#41097,
#41098,#41099,#41100,#41101,#41102,#41103,#41104,#41105,#41106,#41107,#41108,
#41109,#41110,#41111,#41112,#41113,#41114,#41115,#41116,#41117,#41118,#41119,
#41120,#41121,#41122,#41123,#41124,#41125,#41126,#41127,#41128,#41129,#41130,
#41131,#41132,#41133,#41134,#41135,#41136,#41137,#41138,#41139,#41140,#41141,
#41142,#41143,#41144,#41145,#41146,#41147,#41148,#41149,#41150,#41151,#41152,
#41153,#41154,#41155,#41156,#41157,#41158,#41159,#41160,#41161,#41162,#41163,
#41164,#41165,#41166,#41167,#41168,#41169,#41170,#41171,#41172,#41173,#41174,
#41175,#41176,#41177,#41178,#41179,#41180,#41181,#41182,#41183,#41184,#41185,
#41186,#41187,#41188,#41189,#41190,#41191,#41192,#41193,#41194,#41195,#41196,
#41197,#41198,#41199,#41200,#41201,#41202,#41203,#41204,#41205,#41206,#41207,
#41208,#41209,#41210,#41211,#41212,#41213,#41214,#41215,#41216,#41217,#41218,
#41219,#41220,#41221,#41222,#41223,#41224,#41225,#41226,#41227,#41228,#41229,
#41230,#41231,#41232,#41233,#41234,#41235,#41236,#41237,#41238,#41239,#41240),
 .UNSPECIFIED.,.F.,.F.,(4,2,2,2,2,2,2,2,2,2,2,2,2,2,2,2,2,2,2,2,2,2,2,2,
2,2,2,2,2,2,2,2,2,2,2,2,2,2,2,2,2,2,2,2,2,2,2,2,2,2,2,2,2,2,2,2,2,2,2,2,
2,2,2,2,2,2,2,2,2,2,2,2,2,2,2,2,2,2,2,2,2,2,2,2,2,2,2,2,2,2,2,2,2,2,2,2,
2,2,2,2,2,2,2,2,2,2,2,2,2,2,2,2,2,2,2,2,2,2,2,2,2,2,2,2,2,2,2,2,2,2,2,2,
2,2,2,2,2,2,2,2,2,2,2,2,2,2,2,2,2,2,2,2,2,2,2,2,2,2,2,2,2,2,2,2,2,2,2,2,
2,2,2,2,2,2,2,2,2,2,2,2,2,2,2,4),(-23.3356224284091,-23.1752910327308,-23.1316004967274,
-23.0963736709529,-23.0591486217279,-23.0123353436188,-22.9106695363059,
-22.8968366236876,-22.829460335953,-22.7154050385202,-22.6527838974531,
-22.6502910072541,-22.6483669204974,-22.6468396735258,-22.6455953700816,
-22.6445568376552,-22.6436704743946,-22.642898083557,-22.6422117177883,
-22.6415903506155,-22.641017669718,-22.6404805653369,-22.639968048979,-22.6233708392609,
-22.6034050406333,-22.5736620172565,-22.4681488137098,-22.3110706125266,
-22.2446510118568,-22.1924312768605,-22.1591672125633,-22.1214468788745,
-22.0757448693712,-21.852652184604,-21.7723994397085,-21.7206842785241,
-21.6968167216298,-21.676829288011,-21.6469156172914,-21.5411988871072,
-21.3371071938026,-21.2718599740503,-21.231930083881,-21.1940915042348,
-21.1478350896097,-20.9304875416017,-20.8475579134906,-20.7947646885645,
-20.7707247477425,-20.7507769061461,-20.7211810756207,-20.6166100158651,
-20.4927492977278,-20.4101241445086,-20.3452034357598,-20.305330903538,
-20.2674586402655,-20.2210476816895,-20.0061876026044,-19.9219374250095,
-19.8841264053389,-19.8534416545061,-19.8333493391444,-19.8098657015225,
-19.7604851009467,-19.5663838114834,-19.4837408746199,-19.4188107775557,
-19.3789366685353,-19.3410655011596,-19.2946592305909,-19.0797556479186,
-18.9955260509616,-18.9422183284378,-18.9180972046655,-18.8981665403129,
-18.8687148877574,-18.760886463944,-18.605002188652,-18.5597042151212,-18.4935048224512,
-18.4534071115013,-18.4156604272277,-18.3610485514088,-18.2479329730214,
-18.0961873250121,-18.0452593272866,-18.0071953634659,-17.9857783572679,
-17.9671479237223,-17.9330494845069,-17.8299930382376,-17.8155501407971,
-17.6727746622876,-17.6295407314629,-17.5653940078109,-17.5256576707772,
-17.4877019370155,-17.4409114754964,-17.3165702342082,-17.1449489384995,
-17.0901507259142,-17.0657984303569,-17.0459119808705,-17.0168532591001,
-16.9194146268465,-16.8913393696762,-16.7863228085223,-16.7041704285616,
-16.6395011227664,-16.5996726790366,-16.5617736885086,-16.5061754583293,
-16.3145305336669,-16.2212961331576,-16.1645805521732,-16.1399394985055,
-16.1200991742111,-16.0914974017609,-16.0012744793912,-15.9611054693506,
-15.8194922398149,-15.7764522341081,-15.7125007195857,-15.6727985114528,
-15.6348204659372,-15.58793050243,-15.3764110668331,-15.2510581494459,-15.2209530159252,
-15.2009404123223,-15.1771719402775,-15.1260692815802,-15.0897247834949,
-14.9087052186348,-14.8600504736467,-14.8272824585023,-14.7742974318444,
-14.7364157470234,-14.6956943939728,-14.6259378508564,-14.5511590725254,
-14.3925642374133,-14.3552103295018,-14.3076347380174,-14.2844580112734,
-14.2644954456196,-14.2333484987246,-14.1557598209334,-13.9804683780983,
-13.9325128277285,-13.8637414695466,-13.8231920245191,-13.7852368628706,
-13.7317466302716,-13.6121153731153,-13.4634711540442,-13.4272952331865,
-13.3807289011451,-13.3577277014064,-13.3377018792542,-13.306137865739,
-13.1288631944879,-13.0206247346011,-12.9433266888803,-12.9013208071003,
-12.8638324018811,-12.8147714037803,-12.6793344274383,-12.6665414627295,
-12.5937503995926,-12.5104432089797,-12.457499674592,-12.4334357262163,
-12.4134927114653,-12.3839388680023,-12.2800487751444,-12.1561803460734,
-12.0731681060141,-12.008041786093,-11.9681326365893,-11.9302809200484,
-11.8839663264008,-11.6678427707497),.UNSPECIFIED.) ;
#286 = B_SPLINE_CURVE_WITH_KNOTS('',3,(#41241,#41242,#41243,#41244,#41245,
#41246,#41247,#41248,#41249,#41250,#41251,#41252,#41253,#41254,#41255,#41256,
#41257,#41258,#41259,#41260,#41261,#41262,#41263,#41264,#41265,#41266,#41267,
#41268,#41269,#41270,#41271,#41272,#41273,#41274,#41275,#41276,#41277,#41278,
#41279,#41280,#41281,#41282,#41283,#41284,#41285,#41286,#41287,#41288,#41289,
#41290,#41291,#41292,#41293,#41294,#41295,#41296,#41297,#41298,#41299,#41300,
#41301,#41302,#41303,#41304,#41305,#41306,#41307,#41308,#41309,#41310,#41311,
#41312,#41313,#41314,#41315,#41316,#41317,#41318,#41319,#41320,#41321,#41322,
#41323,#41324,#41325,#41326,#41327,#41328,#41329,#41330,#41331,#41332,#41333,
#41334,#41335,#41336,#41337,#41338,#41339,#41340,#41341,#41342,#41343,#41344,
#41345,#41346,#41347,#41348,#41349,#41350,#41351,#41352,#41353,#41354,#41355,
#41356,#41357,#41358,#41359,#41360,#41361,#41362,#41363,#41364,#41365,#41366,
#41367,#41368,#41369,#41370,#41371,#41372,#41373,#41374,#41375,#41376,#41377,
#41378,#41379,#41380,#41381,#41382,#41383,#41384,#41385,#41386,#41387,#41388,
#41389,#41390,#41391,#41392,#41393,#41394,#41395,#41396,#41397,#41398,#41399,
#41400,#41401,#41402,#41403,#41404,#41405,#41406,#41407,#41408,#41409,#41410,
#41411,#41412,#41413,#41414,#41415,#41416,#41417,#41418,#41419,#41420,#41421,
#41422,#41423,#41424,#41425,#41426,#41427,#41428,#41429,#41430,#41431,#41432,
#41433,#41434,#41435,#41436,#41437,#41438,#41439,#41440,#41441,#41442,#41443,
#41444,#41445,#41446,#41447,#41448,#41449,#41450,#41451,#41452,#41453,#41454,
#41455,#41456,#41457,#41458,#41459,#41460,#41461,#41462,#41463,#41464,#41465,
#41466,#41467,#41468,#41469,#41470,#41471,#41472,#41473,#41474,#41475,#41476,
#41477,#41478,#41479,#41480,#41481,#41482,#41483,#41484,#41485,#41486,#41487,
#41488,#41489,#41490,#41491,#41492,#41493,#41494,#41495,#41496,#41497,#41498,
#41499,#41500,#41501,#41502,#41503,#41504,#41505,#41506,#41507,#41508,#41509,
#41510,#41511,#41512,#41513,#41514,#41515,#41516,#41517,#41518,#41519,#41520,
#41521,#41522,#41523,#41524,#41525,#41526,#41527,#41528,#41529,#41530,#41531,
#41532,#41533,#41534,#41535,#41536,#41537,#41538,#41539,#41540,#41541,#41542,
#41543,#41544,#41545,#41546,#41547,#41548,#41549,#41550,#41551,#41552,#41553,
#41554,#41555,#41556,#41557,#41558,#41559,#41560,#41561,#41562,#41563,#41564,
#41565,#41566,#41567,#41568,#41569,#41570,#41571,#41572,#41573,#41574,#41575,
#41576,#41577,#41578,#41579,#41580,#41581,#41582,#41583,#41584,#41585,#41586,
#41587,#41588,#41589,#41590,#41591,#41592,#41593,#41594,#41595,#41596,#41597,
#41598,#41599,#41600,#41601,#41602,#41603,#41604,#41605,#41606,#41607,#41608,
#41609,#41610,#41611,#41612,#41613,#41614,#41615,#41616),.UNSPECIFIED.,
 .F.,.F.,(4,2,2,2,2,2,2,2,2,2,2,2,2,2,2,2,2,2,2,2,2,2,2,2,2,2,2,2,2,2,2,
2,2,2,2,2,2,2,2,2,2,2,2,2,2,2,2,2,2,2,2,2,2,2,2,2,2,2,2,2,2,2,2,2,2,2,2,
2,2,2,2,2,2,2,2,2,2,2,2,2,2,2,2,2,2,2,2,2,2,2,2,2,2,2,2,2,2,2,2,2,2,2,2,
2,2,2,2,2,2,2,2,2,2,2,2,2,2,2,2,2,2,2,2,2,2,2,2,2,2,2,2,2,2,2,2,2,2,2,2,
2,2,2,2,2,2,2,2,2,2,2,2,2,2,2,2,2,2,2,2,2,2,2,2,2,2,2,2,2,2,2,2,2,2,2,2,
2,2,2,2,2,2,2,2,2,2,2,2,4),(-11.6675240120961,-11.626614261062,-11.5049066428377,
-11.3810336064293,-11.2777209614977,-11.2481698993271,-11.2282275661209,
-11.2041629116592,-11.1512127953789,-11.0678880142526,-10.9967659838497,
-10.977751297978,-10.8499086117722,-10.8041375398596,-10.7664026992862,
-10.7262834839868,-10.6599603784825,-10.6145361677103,-10.4578007729936,
-10.3520937954821,-10.3222118954192,-10.3022286112759,-10.2783444258485,
-10.2265255765459,-10.1460179022355,-9.92104580533755,-9.87178409363482,
-9.83427290890201,-9.79237281908231,-9.71570730203895,-9.65902977923404,
-9.55167974144845,-9.53689295720504,-9.43408751358441,-9.40000741883825,
-9.38138024151623,-9.35995893963465,-9.32187200628127,-9.27090042167162,
-9.11884914963252,-9.00752064757142,-8.95228302574212,-8.91444083486559,
-8.87451822236405,-8.80931087495381,-8.72614425572813,-8.60227479504981,
-8.49867645786069,-8.46913362584126,-8.44919240456902,-8.4251234477171,
-8.37214533693766,-8.28874956921323,-8.21836199001807,-8.19154616899052,
-8.08468912089318,-8.0278417951736,-7.98974446150653,-7.95022092751081,
-7.88728221260635,-7.84524019312781,-7.70943455738341,-7.64748291069781,
-7.60182199900407,-7.55571338915206,-7.53279313130586,-7.51249899088974,
-7.48049690347562,-7.45932726468103,-7.39645619054944,-7.14385659417263,
-7.09832078990359,-7.06063546462461,-7.02042004895647,-6.95354844654136,
-6.90756323880015,-6.7469677099623,-6.64607943621641,-6.61648311801943,
-6.59653550494772,-6.57249653672232,-6.51970770671173,-6.43678831565594,
-6.21987280606089,-6.17345337947077,-6.13557988886499,-6.09571174864011,
-6.03081244115732,-5.94822653317546,-5.8243673140553,-5.71973179984141,
-5.69013120920131,-5.67018315733077,-5.6461467582124,-5.59337366596395,
-5.51049356779011,-5.29429626749042,-5.24758346204922,-5.20964571598462,
-5.16988371332307,-5.10558650251306,-5.02412910350441,-4.91821717895962,
-4.82759925792647,-4.77828363620081,-4.75481130912595,-4.7347162726686,
-4.70400959377336,-4.66616154134513,-4.58176361132367,-4.36725077541677,
-4.32080295046152,-4.28292339972129,-4.24306597573255,-4.17822674347864,
-4.09575367539922,-3.97189645241117,-3.86707273230806,-3.83745510444977,
-3.81750506333563,-3.79347831068277,-3.74076558260037,-3.65803674921595,
-3.44033417820391,-3.39409851502524,-3.35626517413593,-3.3163290030225,
-3.25104180351796,-2.99795430518477,-2.93294312668903,-2.90697357423404,
-2.88724827418492,-2.86085582917944,-2.79083463512742,-2.65369318337073,
-2.51180083625297,-2.46635287345153,-2.42868599869819,-2.38843410048223,
-2.32135355339895,-2.27515356203339,-2.11304433646482,-2.01374467084728,
-1.98439211488226,-1.96447345391899,-1.94029662431368,-1.88663023856808,
-1.80148409268042,-1.58883537611954,-1.54212652776392,-1.50418975191282,
-1.46897020179996,-1.4667986765337,-1.46461856627264,-1.46239741478584,
-1.46010269786793,-1.45770010998939,-1.45515187655848,-1.45241493705354,
-1.44943886143034,-1.44616336709126,-1.44251530824729,-1.43840502985344,
-1.43372204246142,-1.42833013370374,-1.36985256116618,-1.25016199999906,
-1.09631907853567,-1.06253542577883,-1.04395749049124,-1.02997228115826,
-1.00120584322775,-0.965459138600484,-0.889063567284749,-0.669843809898982,
-0.614806598336588,-0.576995909451253,-0.542128550249746,-0.520825383229167,
-0.499904143437578,-0.449780354056626,-0.30945191890729,-0.171121419916737,
-0.136721806125387,-0.118041454839647,-0.0999484447591764,-0.0781695906212831,
-1.00000000660683E-6),.UNSPECIFIED.) ;
#287 = B_SPLINE_CURVE_WITH_KNOTS('',3,(#41621,#41622,#41623,#41624,#41625,
#41626,#41627,#41628,#41629,#41630,#41631,#41632,#41633,#41634,#41635,#41636,
#41637,#41638,#41639,#41640,#41641,#41642,#41643,#41644,#41645,#41646,#41647,
#41648,#41649,#41650,#41651,#41652,#41653,#41654,#41655,#41656,#41657,#41658,
#41659,#41660,#41661,#41662,#41663,#41664,#41665,#41666,#41667,#41668,#41669,
#41670,#41671,#41672,#41673,#41674,#41675,#41676,#41677,#41678,#41679,#41680,
#41681,#41682,#41683,#41684,#41685,#41686,#41687,#41688,#41689,#41690,#41691,
#41692,#41693,#41694,#41695,#41696,#41697,#41698,#41699,#41700,#41701,#41702,
#41703,#41704,#41705,#41706,#41707,#41708,#41709,#41710,#41711,#41712,#41713,
#41714,#41715,#41716,#41717,#41718,#41719,#41720,#41721,#41722,#41723,#41724,
#41725,#41726,#41727,#41728,#41729,#41730,#41731,#41732,#41733,#41734,#41735,
#41736,#41737,#41738,#41739,#41740,#41741,#41742,#41743,#41744,#41745,#41746,
#41747,#41748,#41749,#41750,#41751,#41752,#41753,#41754,#41755,#41756,#41757,
#41758,#41759,#41760,#41761,#41762,#41763,#41764,#41765,#41766,#41767,#41768,
#41769,#41770,#41771,#41772,#41773,#41774,#41775,#41776,#41777,#41778,#41779,
#41780,#41781,#41782,#41783,#41784,#41785,#41786,#41787,#41788,#41789,#41790,
#41791,#41792,#41793,#41794,#41795,#41796,#41797,#41798,#41799,#41800,#41801,
#41802,#41803,#41804,#41805,#41806,#41807,#41808,#41809,#41810,#41811,#41812,
#41813,#41814,#41815,#41816,#41817,#41818,#41819,#41820,#41821,#41822,#41823,
#41824,#41825,#41826,#41827,#41828,#41829,#41830,#41831,#41832,#41833,#41834,
#41835,#41836,#41837,#41838,#41839,#41840,#41841,#41842,#41843,#41844,#41845,
#41846,#41847,#41848,#41849,#41850,#41851,#41852,#41853,#41854,#41855,#41856,
#41857,#41858,#41859,#41860,#41861,#41862,#41863,#41864,#41865,#41866,#41867,
#41868,#41869,#41870,#41871,#41872,#41873,#41874,#41875,#41876,#41877,#41878,
#41879,#41880,#41881,#41882,#41883,#41884,#41885,#41886,#41887,#41888,#41889,
#41890,#41891,#41892,#41893,#41894,#41895,#41896,#41897,#41898,#41899,#41900,
#41901,#41902,#41903,#41904,#41905,#41906,#41907,#41908,#41909,#41910,#41911,
#41912,#41913,#41914,#41915,#41916,#41917,#41918,#41919,#41920,#41921,#41922,
#41923,#41924,#41925,#41926,#41927,#41928,#41929,#41930,#41931,#41932,#41933,
#41934,#41935,#41936,#41937,#41938,#41939,#41940,#41941,#41942,#41943,#41944,
#41945,#41946,#41947,#41948,#41949,#41950,#41951,#41952,#41953,#41954,#41955,
#41956,#41957,#41958,#41959,#41960,#41961,#41962,#41963,#41964,#41965,#41966,
#41967,#41968,#41969,#41970,#41971,#41972,#41973,#41974,#41975,#41976,#41977,
#41978,#41979,#41980,#41981,#41982),.UNSPECIFIED.,.F.,.F.,(4,2,2,2,2,2,
2,2,2,2,2,2,2,2,2,2,2,2,2,2,2,2,2,2,2,2,2,2,2,2,2,2,2,2,2,2,2,2,2,2,2,2,
2,2,2,2,2,2,2,2,2,2,2,2,2,2,2,2,2,2,2,2,2,2,2,2,2,2,2,2,2,2,2,2,2,2,2,2,
2,2,2,2,2,2,2,2,2,2,2,2,2,2,2,2,2,2,2,2,2,2,2,2,2,2,2,2,2,2,2,2,2,2,2,2,
2,2,2,2,2,2,2,2,2,2,2,2,2,2,2,2,2,2,2,2,2,2,2,2,2,2,2,2,2,2,2,2,2,2,2,2,
2,2,2,2,2,2,2,2,2,2,2,2,2,2,2,2,2,2,2,2,2,2,2,2,2,2,2,2,2,2,4),(-11.6674812185143,
-11.6250639341939,-11.452758614136,-11.3653419798497,-11.3396861835031,
-11.3195725537615,-11.2961578970493,-11.2471869236146,-11.095880570994,
-10.9512030144633,-10.8955607672905,-10.8576552586143,-10.8178388970075,
-10.7532361748559,-10.6712080015292,-10.5660279602421,-10.537701199713,
-10.4411061122323,-10.4117353694135,-10.3918142977727,-10.3676471955674,
-10.3140450010698,-10.2290641620888,-10.0159831768752,-9.96933684787503,
-9.93141334317261,-9.89162686979631,-9.82719310907355,-9.74548112754296,
-9.639891111604,-9.61122440863084,-9.51459368712576,-9.48529475573627,-9.46538200855945,
-9.44117345798131,-9.38730488311043,-9.30164030901264,-9.09037053895614,
-9.04344259947757,-9.00545681747296,-8.96576913842449,-8.90189602246303,
-8.8212285645194,-8.7144919510522,-8.63680863312446,-8.5790685732414,-8.55368028483248,
-8.53590456504855,-8.50976772224468,-8.44190412092377,-8.31309460352719,
-8.24729796672785,-8.14809719214093,-8.10212655204483,-8.06493335961516,
-8.02026032297791,-7.92538306037018,-7.76812338690922,-7.66276767904412,
-7.63307051890696,-7.61311055057693,-7.58912712131054,-7.53668797455304,
-7.45464381966607,-7.2356073071504,-7.18946333331688,-7.15164944554759,
-7.11167773561874,-7.04619051473791,-6.96249359454973,-6.83861351932384,
-6.73740638782467,-6.70723702141564,-6.68721641940793,-6.66348203429672,
-6.61258501742843,-6.5343218996708,-6.30532873394259,-6.25623282981488,
-6.21874160611061,-6.1767566613799,-6.09957817794074,-5.85038241694493,
-5.79732852069243,-5.77292106510181,-5.75323374648202,-5.72442534241997,
-5.62743568691826,-5.44413721835684,-5.35988754664747,-5.31676700650914,
-5.27982100499634,-5.23203175716964,-5.1096397012042,-4.98575863720367,
-4.88561384303071,-4.85496873549817,-4.83488243151526,-4.81138097380995,
-4.76189196102184,-4.6097691271684,-4.60131147568333,-4.58685289213873,
-4.45118108351957,-4.4026239527585,-4.36519316845768,-4.32291588513274,
-4.24396160179546,-4.13187072449056,-3.9664113497804,-3.93213211999609,
-3.91347183275484,-3.89210188443545,-3.85427577016492,-3.80379554769993,
-3.65509167807215,-3.53585953630813,-3.48223661083977,-3.44426288449034,
-3.40375899392297,-3.33524257144796,-3.28755332486283,-3.11436112041818,
-3.02803584316149,-3.00242473939964,-2.98232038937175,-2.9588778863584,
-2.90973999638714,-2.75817144637901,-2.60087707652758,-2.55580768467391,
-2.51784334726336,-2.47731904322722,-2.40868548786738,-2.36087352344309,
-2.18671604919849,-2.10172654422203,-2.07610002701691,-2.05599262562791,
-2.0325601309602,-1.98348140961611,-1.83200650639649,-1.68767487707398,
-1.63203041603379,-1.594125196244,-1.55431058712312,-1.55222433781072,-1.55008167205715,
-1.54785282433669,-1.54550542370535,-1.54300298035776,-1.54030315603164,
-1.53735569514967,-1.53409988425154,-1.48470822882833,-1.39749447046565,
-1.29950401058437,-1.24933120713727,-1.20159772880599,-1.159153294331,-1.13689806285749,
-1.1237037002735,-1.12331886021745,-1.12242255779361,-1.12160855836381,
-1.09513478026533,-1.01999273177026,-0.853056510683363,-0.742518967345985,
-0.694690698631797,-0.65740269551631,-0.618224087802075,-0.605760054832675,
-0.511200275098992,-0.345374345319041,-0.250657363238717,-0.221560729498369,
-0.201670745750975,-0.182879237196195,-0.158118805160595,-1.00000000458067E-6),
 .UNSPECIFIED.) ;
#288 = B_SPLINE_CURVE_WITH_KNOTS('',3,(#41983,#41984,#41985,#41986,#41987,
#41988,#41989,#41990,#41991,#41992,#41993,#41994,#41995,#41996,#41997,#41998,
#41999,#42000,#42001,#42002,#42003,#42004,#42005,#42006,#42007,#42008,#42009,
#42010,#42011,#42012,#42013,#42014,#42015,#42016,#42017,#42018,#42019,#42020,
#42021,#42022,#42023,#42024,#42025,#42026,#42027,#42028,#42029,#42030,#42031,
#42032,#42033,#42034,#42035,#42036,#42037,#42038,#42039,#42040,#42041,#42042,
#42043,#42044,#42045,#42046,#42047,#42048,#42049,#42050,#42051,#42052,#42053,
#42054,#42055,#42056,#42057,#42058,#42059,#42060,#42061,#42062,#42063,#42064,
#42065,#42066,#42067,#42068,#42069,#42070,#42071,#42072,#42073,#42074,#42075,
#42076,#42077,#42078,#42079,#42080,#42081,#42082,#42083,#42084,#42085,#42086,
#42087,#42088,#42089,#42090,#42091,#42092,#42093,#42094,#42095,#42096,#42097,
#42098,#42099,#42100,#42101,#42102,#42103,#42104,#42105,#42106,#42107,#42108,
#42109,#42110,#42111,#42112,#42113,#42114,#42115,#42116,#42117,#42118,#42119,
#42120,#42121,#42122,#42123,#42124,#42125,#42126,#42127,#42128,#42129,#42130,
#42131,#42132,#42133,#42134,#42135,#42136,#42137,#42138,#42139,#42140,#42141,
#42142,#42143,#42144,#42145,#42146,#42147,#42148,#42149,#42150,#42151,#42152,
#42153,#42154,#42155,#42156,#42157,#42158,#42159,#42160,#42161,#42162,#42163,
#42164,#42165,#42166,#42167,#42168,#42169,#42170,#42171,#42172,#42173,#42174,
#42175,#42176,#42177,#42178,#42179,#42180,#42181,#42182,#42183,#42184,#42185,
#42186,#42187,#42188,#42189,#42190,#42191,#42192,#42193,#42194,#42195,#42196,
#42197,#42198,#42199,#42200,#42201,#42202,#42203,#42204,#42205,#42206,#42207,
#42208,#42209,#42210,#42211,#42212,#42213,#42214,#42215,#42216,#42217,#42218,
#42219,#42220,#42221,#42222,#42223,#42224,#42225,#42226,#42227,#42228,#42229,
#42230,#42231,#42232,#42233,#42234,#42235,#42236,#42237,#42238,#42239,#42240,
#42241,#42242,#42243,#42244,#42245,#42246,#42247,#42248,#42249,#42250,#42251,
#42252,#42253,#42254,#42255,#42256,#42257,#42258,#42259,#42260,#42261,#42262,
#42263,#42264,#42265,#42266,#42267,#42268,#42269,#42270,#42271,#42272,#42273,
#42274,#42275,#42276,#42277,#42278,#42279,#42280,#42281,#42282,#42283,#42284,
#42285,#42286,#42287,#42288,#42289,#42290,#42291,#42292,#42293,#42294,#42295,
#42296,#42297,#42298,#42299,#42300,#42301,#42302,#42303,#42304,#42305,#42306,
#42307,#42308,#42309,#42310,#42311,#42312,#42313,#42314,#42315,#42316,#42317,
#42318,#42319,#42320,#42321,#42322,#42323,#42324,#42325,#42326,#42327,#42328,
#42329,#42330,#42331,#42332),.UNSPECIFIED.,.F.,.F.,(4,2,2,2,2,2,2,2,2,2,
2,2,2,2,2,2,2,2,2,2,2,2,2,2,2,2,2,2,2,2,2,2,2,2,2,2,2,2,2,2,2,2,2,2,2,2,
2,2,2,2,2,2,2,2,2,2,2,2,2,2,2,2,2,2,2,2,2,2,2,2,2,2,2,2,2,2,2,2,2,2,2,2,
2,2,2,2,2,2,2,2,2,2,2,2,2,2,2,2,2,2,2,2,2,2,2,2,2,2,2,2,2,2,2,2,2,2,2,2,
2,2,2,2,2,2,2,2,2,2,2,2,2,2,2,2,2,2,2,2,2,2,2,2,2,2,2,2,2,2,2,2,2,2,2,2,
2,2,2,2,2,2,2,2,2,2,2,2,2,2,2,2,2,2,2,2,4),(-26.1634555927762,-25.9005456295573,
-25.8600838083982,-25.8252427581716,-25.7873788085081,-25.734512258233,
-25.6130482706574,-25.4647201032695,-25.4142954645128,-25.3864213717277,
-25.3844024290128,-25.382774964513,-25.3814232611875,-25.3802679922519,
-25.3792529907394,-25.3783368821727,-25.3774876173322,-25.3766786756518,
-25.375886125169,-25.3750858987278,-25.354804803248,-25.3360605959684,-25.3012841550326,
-25.1873106731379,-25.0430099848548,-24.9790256235431,-24.9278006216719,
-24.8952378510719,-24.8572941145254,-24.8105553531357,-24.5980929156349,
-24.512871195488,-24.459175077678,-24.4349934041492,-24.4150753922217,-24.3857303139356,
-24.2865798222306,-24.1243511429391,-24.0781342201265,-24.0110368873529,
-23.9707816888126,-23.9331156938107,-23.8876737258095,-23.7461806934493,
-23.668699420783,-23.5854307848718,-23.5325030712123,-23.5084420375879,
-23.4884990609389,-23.4589419283742,-23.3549762451747,-23.1965191409114,
-23.1298531155164,-23.0739005284528,-23.0355657586829,-22.9957331307228,
-22.9310370363089,-22.8442856845235,-22.6879151558265,-22.6134544937361,
-22.5865674439942,-22.5668355786942,-22.5413199412167,-22.4834442323932,
-22.2836432920101,-22.2329477168704,-22.1616080174331,-22.1206126392663,
-22.0828374267399,-22.0306056096125,-21.8202292630448,-21.7342388213413,
-21.6802437786536,-21.6560155463226,-21.636106571774,-21.6068411676604,
-21.5040598381009,-21.306447110696,-21.2351700303235,-21.1941854110295,
-21.1564062027908,-21.1041457964309,-20.8939220934962,-20.8078762863678,
-20.7538597494541,-20.7296281461066,-20.709719764947,-20.6804599451628,
-20.5842388264993,-20.5474181173527,-20.4085456092294,-20.3194142234463,
-20.2755563358497,-20.2383237952918,-20.1913663274925,-20.08337294593,-19.9124234870151,
-19.8589183604534,-19.8195054100113,-19.7978256430033,-19.7793512276182,
-19.746207064751,-19.5520249341974,-19.4410474997005,-19.376799582891,-19.3370457439736,
-19.2991017312293,-19.25236286487,-19.0398963674548,-18.9546746733153,-18.9009783782314,
-18.8767965322115,-18.8568783280013,-18.8275328959924,-18.7283798655883,
-18.6993466763047,-18.5573457725992,-18.4671694667898,-18.4231589409445,
-18.3859362788938,-18.3391750213158,-18.2318737943291,-18.0295479009915,
-17.9749827787363,-17.9506663174477,-17.9307735668863,-17.9016559045358,
-17.8034618068912,-17.7844372269668,-17.6346122604599,-17.5902402468478,
-17.5249557153422,-17.4850191029655,-17.4471840492026,-17.4009446318418,
-17.1832689341992,-17.1005167582596,-17.0477941075134,-17.0237652693973,
-17.0038148665442,-16.9741986450779,-16.8739082490558,-16.8555838522135,
-16.7074615332913,-16.6153215954891,-16.5710292439237,-16.5338213263505,
-16.4874071327477,-16.3886563685478,-16.3255127177209,-16.1953454964747,
-16.1271189396966,-16.1009379292865,-16.0831595837025,-16.0578098398817,
-16.0010039944814,-15.7581977319401,-15.6809418056191,-15.6389432856571,
-15.601453866195,-15.5523805409929,-15.4168210638147,-15.404303705419,-15.2702466876122,
-15.2010056304652,-15.1747039748708,-15.1569190219069,-15.1316758310669,
-15.0770469074865,-14.8110317928371,-14.745738297446,-14.7058003368894,
-14.6679665446841,-14.6217319227932,-14.4955868793316),.UNSPECIFIED.) ;
#289 = B_SPLINE_CURVE_WITH_KNOTS('',3,(#42337,#42338,#42339,#42340,#42341,
#42342,#42343,#42344,#42345,#42346,#42347,#42348,#42349,#42350,#42351,#42352,
#42353,#42354,#42355,#42356,#42357,#42358,#42359,#42360,#42361,#42362,#42363,
#42364,#42365,#42366,#42367,#42368,#42369,#42370,#42371,#42372,#42373,#42374,
#42375,#42376,#42377,#42378,#42379,#42380,#42381,#42382,#42383,#42384,#42385,
#42386,#42387,#42388,#42389,#42390,#42391,#42392,#42393,#42394,#42395,#42396,
#42397,#42398,#42399,#42400,#42401,#42402,#42403,#42404,#42405,#42406,#42407,
#42408,#42409,#42410,#42411,#42412,#42413,#42414,#42415,#42416,#42417,#42418,
#42419,#42420,#42421,#42422,#42423,#42424,#42425,#42426,#42427,#42428,#42429,
#42430,#42431,#42432,#42433,#42434,#42435,#42436,#42437,#42438,#42439,#42440,
#42441,#42442,#42443,#42444,#42445,#42446,#42447,#42448,#42449,#42450,#42451,
#42452,#42453,#42454,#42455,#42456,#42457,#42458,#42459,#42460,#42461,#42462,
#42463,#42464,#42465,#42466,#42467,#42468,#42469,#42470,#42471,#42472,#42473,
#42474,#42475,#42476,#42477,#42478,#42479,#42480,#42481,#42482,#42483,#42484,
#42485,#42486,#42487,#42488,#42489,#42490,#42491,#42492,#42493,#42494,#42495,
#42496,#42497,#42498,#42499,#42500,#42501,#42502,#42503,#42504,#42505,#42506,
#42507,#42508,#42509,#42510,#42511,#42512,#42513,#42514,#42515,#42516,#42517,
#42518,#42519,#42520,#42521,#42522,#42523,#42524,#42525,#42526,#42527,#42528,
#42529,#42530,#42531,#42532,#42533,#42534,#42535,#42536,#42537,#42538,#42539,
#42540,#42541,#42542,#42543,#42544,#42545,#42546,#42547,#42548,#42549,#42550,
#42551,#42552,#42553,#42554,#42555,#42556,#42557,#42558,#42559,#42560,#42561,
#42562,#42563,#42564,#42565,#42566,#42567,#42568,#42569,#42570,#42571,#42572,
#42573,#42574,#42575,#42576,#42577,#42578,#42579,#42580,#42581,#42582,#42583,
#42584,#42585,#42586,#42587,#42588,#42589,#42590,#42591,#42592,#42593,#42594,
#42595,#42596,#42597,#42598,#42599,#42600,#42601,#42602,#42603,#42604,#42605,
#42606,#42607,#42608,#42609,#42610,#42611,#42612,#42613,#42614,#42615,#42616,
#42617,#42618,#42619,#42620,#42621,#42622,#42623,#42624,#42625,#42626,#42627,
#42628,#42629,#42630,#42631,#42632,#42633,#42634,#42635,#42636,#42637,#42638,
#42639,#42640,#42641,#42642,#42643,#42644,#42645,#42646,#42647,#42648,#42649,
#42650,#42651,#42652,#42653,#42654,#42655,#42656,#42657,#42658,#42659,#42660,
#42661,#42662,#42663,#42664,#42665,#42666,#42667,#42668,#42669,#42670,#42671,
#42672,#42673,#42674,#42675,#42676,#42677,#42678,#42679,#42680,#42681,#42682),
 .UNSPECIFIED.,.F.,.F.,(4,2,2,2,2,2,2,2,2,2,2,2,2,2,2,2,2,2,2,2,2,2,2,2,
2,2,2,2,2,2,2,2,2,2,2,2,2,2,2,2,2,2,2,2,2,2,2,2,2,2,2,2,2,2,2,2,2,2,2,2,
2,2,2,2,2,2,2,2,2,2,2,2,2,2,2,2,2,2,2,2,2,2,2,2,2,2,2,2,2,2,2,2,2,2,2,2,
2,2,2,2,2,2,2,2,2,2,2,2,2,2,2,2,2,2,2,2,2,2,2,2,2,2,2,2,2,2,2,2,2,2,2,2,
2,2,2,2,2,2,2,2,2,2,2,2,2,2,2,2,2,2,2,2,2,2,2,2,2,2,2,2,2,2,2,2,2,2,2,2,
2,2,2,2,4),(-23.3349707992079,-23.3239989922033,-23.2274410553899,-23.1990240476791,
-23.0938151116522,-23.0118143646992,-22.9472266039377,-22.9074134561651,
-22.8695072376447,-22.8138567655311,-22.6695990338205,-22.5180893204448,
-22.468989507289,-22.4455534313055,-22.4254471005389,-22.3998260719168,
-22.314678798683,-22.1406314632797,-22.0928336449136,-22.0242135104071,
-21.9836915128912,-21.945726031682,-21.900651319766,-21.7434025499433,-21.5918145040618,
-21.5426652260224,-21.5192207757426,-21.4991169770238,-21.4735087958048,
-21.3876212384794,-21.2141006998859,-21.1663697481116,-21.097813392588,
-21.0573024673435,-21.0193318152379,-20.9742323342496,-20.8337931661458,
-20.7542881292985,-20.6710366417479,-20.6181158670165,-20.5940560346243,
-20.5741129661683,-20.5445541653208,-20.440554184855,-20.3166909204677,
-20.2337443427625,-20.1686535080152,-20.1287515477145,-20.0908976740466,
-20.0355839580884,-19.8425220773191,-19.7498203057522,-19.6932995032669,
-19.668687742462,-19.6488437458234,-19.6201988448173,-19.5294090246976,
-19.49350484282,-19.3879702952107,-19.3062179237801,-19.241762545288,-19.2019723597133,
-19.1640513280577,-19.1174158592369,-18.9042572573285,-18.8193055305962,
-18.765714794811,-18.7415495247288,-18.7216281558883,-18.6922544503117,
-18.5957102482914,-18.5673310201109,-18.4621333355221,-18.3801212151583,
-18.3155270288677,-18.2757122615612,-18.2378059618934,-18.1821581645104,
-18.0378488734775,-17.886357665714,-17.8372703761585,-17.8138361492038,
-17.7937287675624,-17.7681037877475,-17.683060504112,-17.50893803918,-17.4611302574943,
-17.3925002185211,-17.3519759984953,-17.3140105524144,-17.268938417913,
-17.1116537719647,-16.9600753526623,-16.9109329760767,-16.8874894267804,
-16.8673848764319,-16.8417742281581,-16.7555044665352,-16.5822678654633,
-16.5345726919139,-16.4660501272825,-16.4255446265172,-16.3875705491433,
-16.3424567945677,-16.2019590351409,-16.1225479323325,-16.0392939849133,
-15.986371892441,-15.9623115821687,-15.9423681850436,-15.9128089919985,
-15.809603313635,-15.6857304891592,-15.6023847873357,-15.5370824006422,
-15.4971426973787,-15.4593095220977,-15.413078559313,-15.1952561319728,
-15.1125831345607,-15.0598920956018,-15.0358683020998,-15.0159168375672,
-14.9862916396495,-14.8863030501742,-14.7251040700319,-14.6790325390657,
-14.6120763189037,-14.5718454426768,-14.5341665611389,-14.4800057606724,
-14.362322645614,-14.3349578000564,-14.2067675568506,-14.1390697175955,
-14.1129525875296,-14.0951775335738,-14.0697704865219,-14.0119037940393,
-13.7703337862915,-13.6930624711711,-13.6510614580554,-13.6135726811405,
-13.5645043561546,-13.428992268934,-13.2853742085968,-13.2137761940229,
-13.1872028594267,-13.1674763559152,-13.1416772799711,-13.0814214710313,
-12.9726925023648,-12.9299558829238,-12.7905693845878,-12.7455763520613,
-12.7076269340837,-12.6670661609092,-12.5982279800385,-12.5502019133739,
-12.3743456840732,-12.295004629071,-12.2650674026273,-12.2450769181647,
-12.2212217132812,-12.1695832220456,-12.0140833218758,-11.9835391163372,
-11.8922817073756,-11.8294225786088,-11.7899126742753,-11.7513554355678,
-11.6940425261241,-11.6674812185143),.UNSPECIFIED.) ;
#290 = B_SPLINE_CURVE_WITH_KNOTS('',3,(#42683,#42684,#42685,#42686,#42687,
#42688,#42689,#42690,#42691,#42692,#42693,#42694,#42695,#42696,#42697,#42698,
#42699,#42700,#42701,#42702,#42703,#42704,#42705,#42706,#42707,#42708,#42709,
#42710,#42711,#42712,#42713,#42714,#42715,#42716,#42717,#42718,#42719,#42720,
#42721,#42722,#42723,#42724,#42725,#42726,#42727,#42728,#42729,#42730,#42731,
#42732,#42733,#42734,#42735,#42736,#42737,#42738,#42739,#42740,#42741,#42742,
#42743,#42744,#42745,#42746,#42747,#42748,#42749,#42750,#42751,#42752,#42753,
#42754,#42755,#42756,#42757,#42758,#42759,#42760,#42761,#42762,#42763,#42764,
#42765,#42766,#42767,#42768,#42769,#42770,#42771,#42772,#42773,#42774,#42775,
#42776,#42777,#42778,#42779,#42780,#42781,#42782,#42783,#42784,#42785,#42786,
#42787,#42788,#42789,#42790,#42791,#42792,#42793,#42794,#42795,#42796,#42797,
#42798,#42799,#42800,#42801,#42802,#42803,#42804,#42805,#42806,#42807,#42808,
#42809,#42810,#42811,#42812,#42813,#42814,#42815,#42816,#42817,#42818,#42819,
#42820,#42821,#42822,#42823,#42824,#42825,#42826,#42827,#42828,#42829,#42830,
#42831,#42832,#42833,#42834,#42835,#42836,#42837,#42838,#42839,#42840,#42841,
#42842,#42843,#42844,#42845,#42846,#42847,#42848,#42849,#42850,#42851,#42852,
#42853,#42854,#42855,#42856,#42857,#42858,#42859,#42860,#42861,#42862,#42863,
#42864,#42865,#42866,#42867,#42868,#42869,#42870,#42871,#42872,#42873,#42874,
#42875,#42876,#42877,#42878,#42879,#42880,#42881,#42882,#42883,#42884,#42885,
#42886,#42887,#42888,#42889,#42890,#42891,#42892,#42893,#42894,#42895,#42896,
#42897,#42898,#42899,#42900,#42901,#42902,#42903,#42904,#42905,#42906,#42907,
#42908,#42909,#42910,#42911,#42912,#42913,#42914,#42915,#42916,#42917,#42918,
#42919,#42920,#42921,#42922,#42923,#42924,#42925,#42926,#42927,#42928,#42929,
#42930,#42931,#42932,#42933,#42934,#42935,#42936,#42937,#42938,#42939,#42940,
#42941,#42942,#42943,#42944,#42945,#42946,#42947,#42948,#42949,#42950,#42951,
#42952,#42953,#42954,#42955,#42956,#42957,#42958,#42959,#42960,#42961,#42962,
#42963,#42964,#42965,#42966,#42967,#42968,#42969,#42970,#42971,#42972,#42973,
#42974,#42975,#42976,#42977,#42978,#42979,#42980,#42981,#42982,#42983,#42984,
#42985,#42986,#42987,#42988,#42989,#42990,#42991,#42992,#42993,#42994,#42995,
#42996,#42997,#42998,#42999,#43000,#43001,#43002,#43003,#43004,#43005,#43006,
#43007,#43008,#43009,#43010,#43011,#43012,#43013,#43014,#43015,#43016,#43017,
#43018,#43019,#43020,#43021,#43022,#43023,#43024),.UNSPECIFIED.,.F.,.F.,
(4,2,2,2,2,2,2,2,2,2,2,2,2,2,2,2,2,2,2,2,2,2,2,2,2,2,2,2,2,2,2,2,2,2,2,
2,2,2,2,2,2,2,2,2,2,2,2,2,2,2,2,2,2,2,2,2,2,2,2,2,2,2,2,2,2,2,2,2,2,2,2,
2,2,2,2,2,2,2,2,2,2,2,2,2,2,2,2,2,2,2,2,2,2,2,2,2,2,2,2,2,2,2,2,2,2,2,2,
2,2,2,2,2,2,2,2,2,2,2,2,2,2,2,2,2,2,2,2,2,2,2,2,2,2,2,2,2,2,2,2,2,2,2,2,
2,2,2,2,2,2,2,2,2,2,2,2,2,2,2,2,2,2,2,2,2,2,2,2,2,2,2,4),(-14.4955868793316,
-14.4039793170469,-14.3212701233793,-14.2685647675828,-14.2445387984084,
-14.2245879677227,-14.1949671515612,-14.0901164688323,-13.9662581554151,
-13.8837995239049,-13.818967367714,-13.7791105038954,-13.7412291128518,
-13.6857417290152,-13.4454965581512,-13.3821441933305,-13.3378565835037,
-13.3152620374607,-13.29506387067,-13.2624299488094,-13.0815402128621,-13.0552579637053,
-12.9287762164095,-12.8826137696698,-12.8447955346388,-12.8048301231133,
-12.7393808313133,-12.6557564066087,-12.5318764198995,-12.4298476854656,
-12.3999971117681,-12.3800178084561,-12.3561169356853,-12.3041943909403,
-12.2234313772468,-12.0125505313966,-11.9569134908243,-11.9190089599369,
-11.8791915540792,-11.8145820097614,-11.732540833122,-11.6273789954797,
-11.599096028804,-11.502381473842,-11.4730505829374,-11.453134192005,-11.4289442618914,
-11.3751952309114,-11.2898378643987,-11.0777384421734,-11.0309439647207,
-10.9929878708533,-10.9532540167676,-10.8891183497146,-10.8458949680382,
-10.7031814765845,-10.6882010948926,-10.5855391011472,-10.5514693862968,
-10.5328439803766,-10.5114200871932,-10.4733196929336,-10.4223226058006,
-10.2700942582674,-10.1597890125376,-10.104188150797,-10.066289455147,-10.0264629941703,
-9.96180111446944,-9.87966156226488,-9.77463037878878,-9.74654599323164,
-9.65616965373775,-9.62368751845823,-9.60351496148271,-9.58086708463561,
-9.53628310367461,-9.5023622158865,-9.37083921768833,-9.32767411642239,
-9.30812174256324,-9.21036054192749,-9.16409192863681,-9.12689018779048,
-9.08247743215429,-8.98947772570046,-8.83856297365265,-8.82205571155216,
-8.7233601673296,-8.69403940962128,-8.67412430492512,-8.64992880103779,
-8.59614322763526,-8.51069163470255,-8.2988475014797,-8.25201322898575,
-8.2140485133544,-8.17432895057607,-8.11027328158569,-8.06712919649685,
-7.92489080825616,-7.90248048993045,-7.79764620296472,-7.76802746102402,
-7.7480772430249,-7.72405100507957,-7.67134177166229,-7.5886218284831,-7.37090178651196,
-7.32466695889884,-7.28683372805554,-7.24689709566393,-7.18160768543455,
-6.92363123316017,-6.86309710298538,-6.83729101113456,-6.81756499659706,
-6.79100033675199,-6.71947556664963,-6.5761623686038,-6.44034623790568,
-6.39124741547667,-6.3537557613976,-6.3117721511883,-6.2346022165538,-5.98462798559819,
-5.93147205349662,-5.90737507205986,-5.8894540419988,-5.86162268850463,
-5.77741720675405,-5.56334169413312,-5.48980431784596,-5.44806685953881,
-5.41051656611965,-5.36003403345945,-5.18444949296384,-5.02599200081779,
-4.99261966705988,-4.97410867131996,-4.95249508261339,-4.91342284446691,
-4.86057417999203,-4.69480579808704,-4.58240258557219,-4.53472468081932,
-4.49744729924692,-4.45411235710466,-4.36846993305474,-4.23947159206005,
-4.10239999887364,-4.06756899516444,-4.04881551835389,-4.02757981635413,
-3.990437399122,-3.94123543379691,-3.80083578355941,-3.66188827416622,-3.61692358349515,
-3.5789803919992,-3.53840749432713,-3.46949737322776,-3.42139531978016,
-3.24492466024322,-3.17165719730139,-3.13913700231706,-3.11895810454882,
-3.09632383325239,-3.05181526940531,-2.98799466372576,-2.82792612848063),
 .UNSPECIFIED.) ;
#291 = B_SPLINE_CURVE_WITH_KNOTS('',3,(#43030,#43031,#43032,#43033,#43034,
#43035,#43036,#43037,#43038,#43039,#43040,#43041,#43042,#43043,#43044,#43045,
#43046,#43047,#43048,#43049,#43050,#43051,#43052,#43053,#43054,#43055,#43056,
#43057,#43058,#43059,#43060,#43061,#43062,#43063,#43064,#43065,#43066,#43067,
#43068,#43069,#43070,#43071,#43072,#43073,#43074,#43075,#43076,#43077,#43078,
#43079,#43080,#43081,#43082,#43083,#43084,#43085,#43086,#43087,#43088,#43089,
#43090,#43091,#43092,#43093,#43094,#43095,#43096,#43097,#43098,#43099,#43100,
#43101,#43102,#43103,#43104,#43105,#43106,#43107,#43108,#43109,#43110,#43111,
#43112,#43113,#43114,#43115,#43116,#43117,#43118,#43119,#43120,#43121,#43122,
#43123,#43124,#43125,#43126,#43127,#43128,#43129,#43130,#43131,#43132,#43133,
#43134,#43135,#43136,#43137,#43138,#43139,#43140,#43141,#43142,#43143,#43144,
#43145,#43146,#43147,#43148,#43149,#43150,#43151,#43152,#43153,#43154,#43155,
#43156,#43157,#43158,#43159,#43160,#43161,#43162,#43163,#43164,#43165,#43166,
#43167,#43168,#43169,#43170,#43171,#43172,#43173,#43174,#43175,#43176,#43177,
#43178,#43179,#43180,#43181,#43182,#43183,#43184,#43185,#43186,#43187,#43188,
#43189,#43190,#43191,#43192,#43193,#43194,#43195,#43196,#43197,#43198,#43199,
#43200,#43201,#43202,#43203,#43204,#43205,#43206,#43207,#43208,#43209,#43210,
#43211,#43212,#43213,#43214,#43215,#43216,#43217,#43218,#43219,#43220,#43221,
#43222,#43223,#43224,#43225,#43226,#43227,#43228,#43229,#43230,#43231,#43232,
#43233,#43234,#43235,#43236,#43237,#43238,#43239,#43240,#43241,#43242,#43243,
#43244,#43245,#43246,#43247,#43248,#43249,#43250,#43251,#43252,#43253,#43254,
#43255,#43256,#43257,#43258,#43259,#43260,#43261,#43262,#43263,#43264,#43265,
#43266,#43267,#43268,#43269,#43270,#43271,#43272,#43273,#43274,#43275,#43276,
#43277,#43278,#43279,#43280,#43281,#43282,#43283,#43284,#43285,#43286,#43287,
#43288,#43289,#43290,#43291,#43292,#43293,#43294,#43295,#43296,#43297),
 .UNSPECIFIED.,.F.,.F.,(4,2,2,2,2,2,2,2,2,2,2,2,2,2,2,2,2,2,2,2,2,2,2,2,
2,2,2,2,2,2,2,2,2,2,2,2,2,2,2,2,2,2,2,2,2,2,2,2,2,2,2,2,2,2,2,2,2,2,2,2,
2,2,2,2,2,2,2,2,2,2,2,2,2,2,2,2,2,2,2,2,2,2,2,2,2,2,2,2,2,2,2,2,2,2,2,2,
2,2,2,2,2,2,2,2,2,2,2,2,2,2,2,2,2,2,2,2,2,2,2,2,2,2,2,2,2,2,2,2,2,2,2,2,
2,4),(-8.83945532408071,-8.81772296497787,-8.77981688992475,-8.74000136067843,
-8.67540352300486,-8.59338454410489,-8.48819223953054,-8.45983298970468,
-8.36327884080695,-8.3339011300318,-8.313979235886,-8.28981610975072,-8.23623945405055,
-8.15132397785674,-7.93807746110587,-7.89145490121599,-7.8535366028422,
-7.81374158039737,-7.74925940985965,-7.66745688941652,-7.5619835882094,
-7.53134212096736,-7.43637551815251,-7.40724975211934,-7.38735631909881,
-7.36304522409823,-7.30851372638641,-7.22113035751957,-7.01406654748622,
-6.96134665866414,-6.92350346431488,-6.88268928374934,-6.81239518505327,
-6.71925619475584,-6.5947381301372,-6.50834087970517,-6.48272835949858,
-6.46262363412635,-6.43918179811748,-6.39004842026468,-6.23848654365196,
-6.08117096506745,-6.03610325029695,-5.99813908142674,-5.95761364055599,
-5.88897458095356,-5.84115699579456,-5.66695637310105,-5.58202864716916,
-5.55639960356666,-5.53629160286888,-5.51286048360273,-5.46379047419234,
-5.3123288773162,-5.16796451107701,-5.11232159130715,-5.07441643550708,
-5.03460109859423,-4.97000165847179,-4.88797902381774,-4.78279506124984,
-4.75445410765858,-4.65788350880418,-4.62850800295046,-4.60858663971583,
-4.58442292871877,-4.53084084653061,-4.44591062717666,-4.23270834965547,
-4.18608074271722,-4.14816179496332,-4.10836952055798,-4.04390026569526,
-3.96212126842258,-3.8566210513172,-3.73523163742586,-3.7040891185304,-3.68412781972634,
-3.66095061508918,-3.61336883076644,-3.57600692301453,-3.41733343367493,
-3.34301308077549,-3.27306337647489,-3.23230953181443,-3.19444318982108,
-3.14155708152949,-3.07998366293311,-2.94707990393144,-2.89773104151819,
-2.80428847398365,-2.77534451285491,-2.75547084430239,-2.73104971675999,
-2.67579621070942,-2.5865098677734,-2.38291387507709,-2.32996762224583,
-2.29209281180773,-2.25136043184919,-2.18153343131242,-2.13246145383143,
-1.94786327624138,-1.93470102807542,-1.87124632747421,-1.84545302553626,
-1.82572708541858,-1.7991492386095,-1.72750584998882,-1.58369019303517,
-1.44839253437952,-1.39934788487226,-1.36186284374058,-1.32694073848364,
-1.28519128592769,-1.1525946536019,-0.961623155505617,-0.928367322517469,
-0.907931625399414,-0.889741860057858,-0.875874959638054,-0.814163079981681,
-0.706304858487514,-0.667332989671791,-0.524217272788026,-0.478765902264634,
-0.441098484134846,-0.406249494706772,-0.366330681831491,-0.307347671505237,
-0.167385808365722,-0.0429957109239202,-0.0182555783699187,-1.00000000173572E-6),
 .UNSPECIFIED.) ;
#292 = B_SPLINE_CURVE_WITH_KNOTS('',3,(#43298,#43299,#43300,#43301,#43302,
#43303,#43304,#43305,#43306,#43307,#43308,#43309,#43310,#43311,#43312,#43313,
#43314,#43315,#43316,#43317,#43318,#43319,#43320,#43321,#43322,#43323,#43324,
#43325,#43326,#43327,#43328,#43329,#43330,#43331,#43332,#43333,#43334,#43335,
#43336,#43337,#43338,#43339,#43340,#43341,#43342,#43343,#43344,#43345,#43346,
#43347,#43348,#43349,#43350,#43351,#43352,#43353,#43354,#43355,#43356,#43357,
#43358,#43359,#43360,#43361,#43362,#43363,#43364,#43365,#43366,#43367,#43368,
#43369,#43370,#43371,#43372,#43373,#43374,#43375,#43376,#43377,#43378,#43379,
#43380,#43381,#43382,#43383,#43384,#43385,#43386,#43387,#43388,#43389,#43390,
#43391,#43392,#43393,#43394,#43395,#43396,#43397,#43398,#43399,#43400,#43401,
#43402,#43403,#43404,#43405,#43406,#43407,#43408,#43409),.UNSPECIFIED.,
 .F.,.F.,(4,2,2,2,2,2,2,2,2,2,2,2,2,2,2,2,2,2,2,2,2,2,2,2,2,2,2,2,2,2,2,
2,2,2,2,2,2,2,2,2,2,2,2,2,2,2,2,2,2,2,2,2,2,2,2,4),(-26.1629118607084,-26.1454935044846,
-26.1261207928679,-26.0917122142876,-25.9628614800202,-25.8273404683811,
-25.7414593988453,-25.7054475674227,-25.6681895085004,-25.6246522692977,
-25.537676959584,-25.3506240911098,-25.2886646959746,-25.2450408134631,
-25.2262511845348,-25.2115733057507,-25.187046031042,-25.1337856122842,
-24.9286494438691,-24.8552799980706,-24.8509574230423,-24.8387277361866,
-24.83388082635,-24.8255983766822,-24.8199213669822,-24.8160452575958,-24.813395492473,
-24.8115785832224,-24.8103287015693,-24.8064810097528,-24.803093528574,
-24.8000903033327,-24.7974062205088,-24.7949856496721,-24.7601013428692,
-24.7221954241647,-24.6665495485182,-24.489860052902,-24.3389903115827,
-24.3083751113904,-24.2882932115933,-24.2647779655738,-24.2152056292869,
-24.1249752275425,-24.0190672851008,-23.9376097197101,-23.8733124310856,
-23.8335505595953,-23.7956130296214,-23.748900607415,-23.5362722260045,
-23.4511164813559,-23.397446393384,-23.3732690015012,-23.3533504815712,
-23.3349707992079),.UNSPECIFIED.) ;
#293 = B_SPLINE_CURVE_WITH_KNOTS('',3,(#43411,#43412,#43413,#43414,#43415,
#43416,#43417,#43418,#43419,#43420,#43421,#43422,#43423,#43424,#43425,#43426,
#43427,#43428,#43429,#43430,#43431,#43432,#43433,#43434,#43435,#43436,#43437,
#43438,#43439,#43440,#43441,#43442,#43443,#43444,#43445,#43446,#43447,#43448,
#43449,#43450,#43451,#43452,#43453,#43454,#43455,#43456,#43457,#43458,#43459,
#43460,#43461,#43462,#43463,#43464,#43465,#43466,#43467,#43468,#43469,#43470,
#43471,#43472,#43473,#43474,#43475,#43476,#43477,#43478,#43479,#43480,#43481,
#43482,#43483,#43484,#43485,#43486,#43487,#43488,#43489,#43490,#43491,#43492,
#43493,#43494,#43495,#43496,#43497,#43498,#43499,#43500,#43501,#43502,#43503,
#43504,#43505,#43506,#43507,#43508,#43509,#43510,#43511,#43512,#43513,#43514,
#43515,#43516,#43517,#43518),.UNSPECIFIED.,.F.,.F.,(4,2,2,2,2,2,2,2,2,2,
2,2,2,2,2,2,2,2,2,2,2,2,2,2,2,2,2,2,2,2,2,2,2,2,2,2,2,2,2,2,2,2,2,2,2,2,
2,2,2,2,2,2,2,4),(-2.82792612848063,-2.8041603327855,-2.71722452840601,
-2.67369354603614,-2.63643530107694,-2.58903728134093,-2.4708245315289,
-2.36446470976795,-2.24363929252875,-2.21196612827096,-2.19192388812018,
-2.16896819323943,-2.12265796130199,-2.08677713582502,-1.94050254230746,
-1.80722666065535,-1.75862839639159,-1.72119316882715,-1.67893897308388,
-1.6001259222878,-1.48836799577483,-1.32226757322654,-1.28803156524166,
-1.26937851219505,-1.25378343596525,-1.25321556649319,-1.25271179604491,
-1.25226639635086,-1.25187384333195,-1.25152887399879,-1.25122653042299,
-1.25096219051075,-1.25073158616506,-1.25053081021818,-1.2500027044565,
-1.2494860725939,-1.24898097171239,-1.21745789151553,-1.17423099090844,
-1.06650389790476,-0.89558294968666,-0.840263873650828,-0.802778320537367,
-0.766902826466558,-0.716509180206056,-0.650490717393987,-0.495617729964171,
-0.395330090035875,-0.361413339863902,-0.342813367365246,-0.324703471960157,
-0.302795572703682,-0.269147194228328,-9.99999989481637E-7),
 .UNSPECIFIED.) ;
#294 = B_SPLINE_CURVE_WITH_KNOTS('',3,(#43519,#43520,#43521,#43522,#43523,
#43524,#43525,#43526,#43527,#43528,#43529,#43530,#43531,#43532,#43533,#43534,
#43535,#43536,#43537,#43538,#43539,#43540,#43541,#43542,#43543,#43544,#43545,
#43546,#43547,#43548,#43549,#43550,#43551,#43552,#43553,#43554,#43555,#43556,
#43557,#43558,#43559,#43560,#43561,#43562,#43563,#43564,#43565,#43566,#43567,
#43568,#43569,#43570,#43571,#43572,#43573,#43574,#43575,#43576,#43577,#43578,
#43579,#43580,#43581,#43582,#43583,#43584,#43585,#43586,#43587,#43588,#43589,
#43590,#43591,#43592,#43593,#43594,#43595,#43596,#43597,#43598,#43599,#43600,
#43601,#43602,#43603,#43604,#43605,#43606,#43607,#43608,#43609,#43610,#43611,
#43612,#43613,#43614,#43615,#43616,#43617,#43618,#43619,#43620,#43621,#43622,
#43623,#43624,#43625,#43626,#43627,#43628,#43629,#43630,#43631,#43632,#43633,
#43634,#43635,#43636,#43637,#43638,#43639,#43640,#43641,#43642,#43643,#43644,
#43645,#43646,#43647,#43648,#43649,#43650,#43651,#43652,#43653,#43654,#43655,
#43656,#43657,#43658,#43659,#43660,#43661,#43662,#43663,#43664,#43665,#43666,
#43667,#43668,#43669,#43670,#43671,#43672,#43673,#43674,#43675,#43676,#43677,
#43678,#43679,#43680,#43681,#43682,#43683,#43684,#43685,#43686,#43687,#43688,
#43689,#43690,#43691,#43692,#43693,#43694,#43695,#43696,#43697,#43698,#43699,
#43700,#43701,#43702,#43703,#43704,#43705,#43706,#43707,#43708,#43709,#43710,
#43711,#43712,#43713,#43714,#43715,#43716,#43717,#43718,#43719,#43720,#43721,
#43722,#43723,#43724,#43725,#43726,#43727,#43728,#43729,#43730,#43731,#43732,
#43733,#43734,#43735,#43736,#43737,#43738,#43739,#43740,#43741,#43742,#43743,
#43744,#43745,#43746,#43747,#43748,#43749,#43750,#43751,#43752,#43753,#43754,
#43755,#43756,#43757,#43758,#43759,#43760,#43761,#43762,#43763,#43764,#43765,
#43766,#43767,#43768,#43769,#43770,#43771,#43772,#43773,#43774,#43775,#43776,
#43777,#43778,#43779,#43780,#43781,#43782,#43783,#43784,#43785,#43786,#43787,
#43788,#43789,#43790,#43791,#43792,#43793,#43794,#43795,#43796,#43797,#43798,
#43799,#43800,#43801,#43802,#43803,#43804,#43805,#43806,#43807,#43808,#43809,
#43810,#43811,#43812,#43813,#43814,#43815,#43816,#43817,#43818,#43819,#43820,
#43821,#43822,#43823,#43824,#43825,#43826,#43827,#43828,#43829,#43830,#43831,
#43832,#43833,#43834,#43835,#43836,#43837,#43838,#43839,#43840,#43841,#43842,
#43843,#43844,#43845,#43846,#43847,#43848,#43849,#43850,#43851,#43852,#43853,
#43854,#43855,#43856,#43857,#43858,#43859,#43860,#43861,#43862,#43863,#43864,
#43865,#43866,#43867,#43868,#43869,#43870,#43871,#43872,#43873,#43874,#43875,
#43876,#43877,#43878,#43879,#43880,#43881,#43882,#43883,#43884),
 .UNSPECIFIED.,.F.,.F.,(4,2,2,2,2,2,2,2,2,2,2,2,2,2,2,2,2,2,2,2,2,2,2,2,
2,2,2,2,2,2,2,2,2,2,2,2,2,2,2,2,2,2,2,2,2,2,2,2,2,2,2,2,2,2,2,2,2,2,2,2,
2,2,2,2,2,2,2,2,2,2,2,2,2,2,2,2,2,2,2,2,2,2,2,2,2,2,2,2,2,2,2,2,2,2,2,2,
2,2,2,2,2,2,2,2,2,2,2,2,2,2,2,2,2,2,2,2,2,2,2,2,2,2,2,2,2,2,2,2,2,2,2,2,
2,2,2,2,2,2,2,2,2,2,2,2,2,2,2,2,2,2,2,2,2,2,2,2,2,2,2,2,2,2,2,2,2,2,2,2,
2,2,2,2,2,2,2,2,2,2,2,2,2,2,4),(-23.3351463080753,-23.294167951005,-23.2607234492997,
-23.2258029543077,-23.1899174225933,-23.1418265154115,-23.0158784775917,
-22.8703830766604,-22.8097257526394,-22.7771067645078,-22.7583306858827,
-22.7384307415802,-22.7092439655656,-22.6137266913003,-22.5914715742371,
-22.4421401846129,-22.3771646348096,-22.3258402204451,-22.292806562641,
-22.2554008546556,-22.2005981424254,-22.0148262787654,-21.9165041602218,
-21.8753201060059,-21.8735469715915,-21.8719714444937,-21.8705696836065,
-21.8693208279231,-21.868206647997,-21.8672112252402,-21.8663206615595,
-21.8655228197381,-21.8648070935743,-21.8641642059376,-21.8635860324511,
-21.8630654482073,-21.8625961950523,-21.8621727669429,-21.8617903110256,
-21.8614445424995,-21.8611316712138,-21.860848338432,-21.8605915624252,
-21.8603586914862,-21.8601473633363,-21.8594299393724,-21.8587391921259,
-21.8580736184432,-21.857431804381,-21.8568124193287,-21.8562142105715,
-21.8556359981386,-21.8550766700135,-21.8545351776685,-21.8540105318744,
-21.8535017987687,-21.853008096188,-21.8525285902435,-21.852062492069,-21.8516090548073,
-21.8511675708174,-21.850737368974,-21.8503178121519,-21.8499082949377,
-21.8495082413861,-21.8491171029318,-21.848734356484,-21.8483595025164,
-21.8479920633295,-21.8476315814089,-21.8472776178631,-21.8469297508675,
-21.8465875743004,-21.8462506963629,-21.8459187382141,-21.8455913327549,
-21.8452681233537,-21.8449487627008,-21.8303501039131,-21.8102318170827,
-21.7845517460689,-21.6967912768393,-21.5247930905553,-21.4772574380689,
-21.4088878749417,-21.3684096724222,-21.3304241416761,-21.2852522741711,
-21.1487804911606,-21.0069275054717,-20.9574953331976,-20.9202292887279,
-20.8989694292156,-20.8802335287785,-20.8455057344452,-20.7096122929139,
-20.5797387920721,-20.4937753602065,-20.4503916108007,-20.4131193577101,
-20.3655125350636,-20.2554343035864,-20.0433495689906,-19.9987394987869,
-19.9760868720848,-19.9559164124966,-19.9234472134472,-19.7259266535772,
-19.6301546078995,-19.5585797029641,-19.5175438020412,-19.4797831953867,
-19.4276574179106,-19.1811606293551,-19.117013450659,-19.0955400340761,
-19.063208342075,-19.0428600036321,-19.0200649975175,-18.9746619643204,
-18.7771066036361,-18.6931403601937,-18.6275112187552,-18.587514481014,
-18.5497144507524,-18.4947491724804,-18.3120770146737,-18.2118982483161,
-18.1702979781377,-18.137390627667,-18.1169448064465,-18.0943557802202,
-18.0500968134275,-18.0009297486148,-17.8217266458526,-17.7517048340439,
-17.693785196244,-17.6551273509583,-17.6203792254955,-17.5628254584511,
-17.4578846589815,-17.3047234125667,-17.2535919136577,-17.2154205256659,
-17.1939827757626,-17.1753663220772,-17.1413502110518,-17.0394372067765,
-17.011667863475,-16.8769013833938,-16.7891854527113,-16.7455375226847,
-16.7082894285267,-16.6610528831851,-16.5522755775284,-16.3825985754233,
-16.3292523611245,-16.2899218375541,-16.2682582040096,-16.2497753201483,
-16.2165772725303,-16.0237724688728,-15.9111734778208,-15.8471138037135,
-15.8073934530403,-15.7694290347796,-15.7225965045835,-15.5107357727681,
-15.4252878551299,-15.3715036616736,-15.3473083162426,-15.3273930978448,
-15.2980718425089,-15.2014729188486,-15.1730243944334,-15.0678042440994,
-14.9858103705424,-14.9212260620675,-14.8814132303399,-14.8435061826619,
-14.787852332879,-14.6436272489799,-14.4955154817265),.UNSPECIFIED.) ;
#295 = B_SPLINE_CURVE_WITH_KNOTS('',3,(#43889,#43890,#43891,#43892,#43893,
#43894,#43895,#43896,#43897,#43898,#43899,#43900,#43901,#43902,#43903,#43904,
#43905,#43906,#43907,#43908,#43909,#43910,#43911,#43912,#43913,#43914,#43915,
#43916,#43917,#43918,#43919,#43920,#43921,#43922,#43923,#43924,#43925,#43926,
#43927,#43928,#43929,#43930,#43931,#43932,#43933,#43934,#43935,#43936,#43937,
#43938,#43939,#43940,#43941,#43942,#43943,#43944,#43945,#43946,#43947,#43948,
#43949,#43950,#43951,#43952,#43953,#43954,#43955,#43956,#43957,#43958,#43959,
#43960,#43961,#43962,#43963,#43964,#43965,#43966,#43967,#43968,#43969,#43970,
#43971,#43972,#43973,#43974,#43975,#43976,#43977,#43978,#43979,#43980,#43981,
#43982,#43983,#43984,#43985,#43986,#43987,#43988,#43989,#43990,#43991,#43992,
#43993,#43994,#43995,#43996,#43997,#43998,#43999,#44000,#44001,#44002,#44003,
#44004,#44005,#44006,#44007,#44008,#44009,#44010,#44011,#44012,#44013,#44014,
#44015,#44016,#44017,#44018,#44019,#44020,#44021,#44022,#44023,#44024,#44025,
#44026,#44027,#44028,#44029,#44030,#44031,#44032,#44033,#44034,#44035,#44036,
#44037,#44038,#44039,#44040,#44041,#44042,#44043,#44044,#44045,#44046,#44047,
#44048,#44049,#44050,#44051,#44052,#44053,#44054,#44055,#44056,#44057,#44058,
#44059,#44060,#44061,#44062,#44063,#44064,#44065,#44066,#44067,#44068,#44069,
#44070,#44071,#44072,#44073,#44074,#44075,#44076,#44077,#44078,#44079,#44080,
#44081,#44082,#44083,#44084,#44085,#44086,#44087,#44088,#44089,#44090,#44091,
#44092,#44093,#44094,#44095,#44096,#44097,#44098,#44099,#44100,#44101,#44102,
#44103,#44104,#44105,#44106,#44107,#44108,#44109,#44110,#44111,#44112,#44113,
#44114,#44115,#44116,#44117,#44118,#44119,#44120,#44121,#44122,#44123,#44124,
#44125,#44126,#44127,#44128,#44129,#44130,#44131,#44132,#44133,#44134,#44135,
#44136,#44137,#44138,#44139,#44140,#44141,#44142,#44143,#44144,#44145,#44146,
#44147,#44148,#44149,#44150,#44151,#44152,#44153,#44154,#44155,#44156,#44157,
#44158,#44159,#44160,#44161,#44162,#44163,#44164,#44165,#44166,#44167,#44168,
#44169,#44170,#44171,#44172,#44173,#44174,#44175,#44176,#44177,#44178,#44179,
#44180,#44181,#44182,#44183,#44184,#44185,#44186,#44187,#44188,#44189,#44190,
#44191,#44192,#44193,#44194,#44195,#44196,#44197,#44198,#44199,#44200,#44201,
#44202,#44203,#44204,#44205,#44206,#44207,#44208,#44209,#44210,#44211,#44212,
#44213,#44214,#44215,#44216,#44217,#44218,#44219,#44220,#44221,#44222,#44223,
#44224,#44225,#44226,#44227,#44228,#44229,#44230),.UNSPECIFIED.,.F.,.F.,
(4,2,2,2,2,2,2,2,2,2,2,2,2,2,2,2,2,2,2,2,2,2,2,2,2,2,2,2,2,2,2,2,2,2,2,
2,2,2,2,2,2,2,2,2,2,2,2,2,2,2,2,2,2,2,2,2,2,2,2,2,2,2,2,2,2,2,2,2,2,2,2,
2,2,2,2,2,2,2,2,2,2,2,2,2,2,2,2,2,2,2,2,2,2,2,2,2,2,2,2,2,2,2,2,2,2,2,2,
2,2,2,2,2,2,2,2,2,2,2,2,2,2,2,2,2,2,2,2,2,2,2,2,2,2,2,2,2,2,2,2,2,2,2,2,
2,2,2,2,2,2,2,2,2,2,2,2,2,2,2,2,2,2,2,2,2,2,2,2,2,2,2,4),(-20.507299559048,
-20.4750081423604,-20.423427616719,-20.3850189726539,-20.3635343236376,
-20.3423278927266,-20.3053371938717,-20.2417535837765,-20.0642492426348,
-20.0160191618219,-19.9469866841915,-19.9063916276704,-19.8684565790793,
-19.8235359106753,-19.5998889145673,-19.480904253598,-19.4509981832004,
-19.4310114714177,-19.4071392645321,-19.3553967726712,-19.1033233011638,
-19.026174929525,-18.9841940818035,-18.9467004710437,-18.897592665659,-18.7616985398062,
-18.7499181832599,-18.5964517061827,-18.5413589484032,-18.5169616415103,
-18.4970829854371,-18.4680977629777,-18.3863969883353,-18.2107771347324,
-18.1412880234492,-18.0836772949979,-18.0450702467323,-18.0102751325587,
-17.9524152039754,-17.8482896755343,-17.6949818457012,-17.6438285025493,
-17.6056452472752,-17.5842047694776,-17.5655891152944,-17.5315800762635,
-17.4616337607536,-17.2848149921297,-17.2366694582687,-17.167717391648,
-17.1271364794953,-17.089195442148,-17.0358005384335,-16.912419010596,-16.7665123516105,
-16.6943773689444,-16.6677436538751,-16.6480163172177,-16.6222726702742,
-16.5628157894647,-16.5459300492343,-16.5166574195152,-16.3535473228537,
-16.2860706759758,-16.2296386412465,-16.1912257849105,-16.1515111531045,
-16.0874885728065,-15.9778210838673,-15.7807494027894,-15.7481927004737,
-15.7280073419323,-15.705385210704,-15.6609458650914,-15.5972727980809,
-15.4113448369261,-15.3256133611883,-15.2822641229311,-15.2449872097988,
-15.1973274194708,-15.0763627005395,-14.8817611245948,-14.8329607746095,
-14.8095747422674,-14.7894515705858,-14.7585549201691,-14.7203883996381,
-14.634731627884,-14.4234290614924,-14.3765044069543,-14.3385186501703,
-14.2988284107755,-14.2349448942323,-14.123153347139,-13.9286985245183,
-13.8957537749415,-13.8773108952936,-13.8555713510835,-13.8158501977611,
-13.7617482839575,-13.5858872438347,-13.4836610011631,-13.436795019513,
-13.3995666614531,-13.3556368965417,-13.2660186282788,-13.1257014179184,
-13.0792665967161,-12.9928456922186,-12.967232109516,-12.9471267977523,
-12.9236846494042,-12.8745516636906,-12.7229885612288,-12.5656622906149,
-12.5205940942157,-12.4826291101795,-12.4421023657926,-12.3734599204552,
-12.3256393886276,-12.1514205649339,-12.0665113087927,-12.0408808137782,
-12.0207721481933,-11.9973409647251,-11.9482728184068,-11.7968123188526,
-11.6524335746977,-11.5967898492279,-11.5588838394353,-11.5190673594432,
-11.4544654554578,-11.3724391764939,-11.2672546875182,-11.2389185811808,
-11.1423377633651,-11.11296308292,-11.0930414032415,-11.0688761918549,-11.0152870292955,
-10.9303400032328,-10.7171694674061,-10.6705353715052,-10.6326143056607,
-10.5928229432139,-10.5283628987424,-10.4466021050839,-10.3410730945386,
-10.3372134355085,-10.2264782260157,-10.191829022171,-10.1731062028581,
-10.1518270378394,-10.1144639207663,-10.0648512839366,-9.92184798585374,
-9.78659161028094,-9.74152124345755,-9.70355605191445,-9.66303080138468,
-9.59439554852061,-9.5465823544125,-9.37241980257034,-9.28743000167747,
-9.26180284009967,-9.24169496852961,-9.21826197903713,-9.16918237066026,
-9.01770438184618,-8.87336864188202,-8.83945532408071),.UNSPECIFIED.) ;
#296 = B_SPLINE_CURVE_WITH_KNOTS('',3,(#44231,#44232,#44233,#44234,#44235,
#44236,#44237,#44238,#44239,#44240,#44241,#44242,#44243,#44244,#44245,#44246,
#44247,#44248,#44249,#44250,#44251,#44252,#44253,#44254,#44255,#44256,#44257,
#44258,#44259,#44260,#44261,#44262,#44263,#44264,#44265,#44266,#44267,#44268,
#44269,#44270,#44271,#44272,#44273,#44274,#44275,#44276,#44277,#44278,#44279,
#44280,#44281,#44282,#44283,#44284,#44285,#44286,#44287,#44288,#44289,#44290,
#44291,#44292,#44293,#44294,#44295,#44296,#44297,#44298,#44299,#44300,#44301,
#44302,#44303,#44304,#44305,#44306,#44307,#44308,#44309,#44310,#44311,#44312,
#44313,#44314,#44315,#44316,#44317,#44318,#44319,#44320,#44321,#44322,#44323,
#44324,#44325,#44326,#44327,#44328,#44329,#44330,#44331,#44332,#44333,#44334,
#44335,#44336,#44337,#44338,#44339,#44340,#44341,#44342,#44343,#44344,#44345,
#44346,#44347,#44348,#44349,#44350,#44351,#44352,#44353,#44354,#44355,#44356,
#44357,#44358,#44359,#44360,#44361,#44362,#44363,#44364,#44365,#44366,#44367,
#44368,#44369,#44370,#44371,#44372,#44373,#44374,#44375,#44376,#44377,#44378,
#44379,#44380,#44381,#44382,#44383,#44384,#44385,#44386,#44387,#44388,#44389,
#44390,#44391,#44392,#44393,#44394,#44395,#44396,#44397,#44398,#44399,#44400,
#44401,#44402,#44403,#44404,#44405,#44406,#44407,#44408,#44409,#44410,#44411,
#44412,#44413,#44414,#44415,#44416,#44417,#44418,#44419,#44420,#44421,#44422,
#44423,#44424,#44425,#44426,#44427,#44428,#44429,#44430,#44431,#44432,#44433,
#44434,#44435,#44436,#44437,#44438,#44439,#44440,#44441,#44442,#44443,#44444,
#44445,#44446,#44447,#44448,#44449,#44450,#44451,#44452,#44453,#44454,#44455,
#44456,#44457,#44458,#44459,#44460,#44461,#44462,#44463,#44464,#44465,#44466,
#44467,#44468,#44469,#44470,#44471,#44472,#44473,#44474,#44475,#44476,#44477,
#44478,#44479,#44480,#44481,#44482,#44483,#44484,#44485,#44486,#44487,#44488,
#44489,#44490,#44491,#44492,#44493,#44494,#44495,#44496,#44497,#44498,#44499,
#44500,#44501,#44502,#44503,#44504,#44505,#44506,#44507,#44508,#44509,#44510,
#44511,#44512,#44513,#44514,#44515,#44516,#44517,#44518,#44519,#44520,#44521,
#44522,#44523,#44524,#44525,#44526,#44527,#44528,#44529,#44530,#44531,#44532,
#44533,#44534,#44535,#44536,#44537,#44538,#44539,#44540,#44541,#44542,#44543,
#44544,#44545,#44546,#44547,#44548,#44549,#44550,#44551,#44552,#44553,#44554,
#44555,#44556,#44557,#44558,#44559,#44560,#44561,#44562,#44563,#44564,#44565,
#44566,#44567,#44568),.UNSPECIFIED.,.F.,.F.,(4,2,2,2,2,2,2,2,2,2,2,2,2,
2,2,2,2,2,2,2,2,2,2,2,2,2,2,2,2,2,2,2,2,2,2,2,2,2,2,2,2,2,2,2,2,2,2,2,2,
2,2,2,2,2,2,2,2,2,2,2,2,2,2,2,2,2,2,2,2,2,2,2,2,2,2,2,2,2,2,2,2,2,2,2,2,
2,2,2,2,2,2,2,2,2,2,2,2,2,2,2,2,2,2,2,2,2,2,2,2,2,2,2,2,2,2,2,2,2,2,2,2,
2,2,2,2,2,2,2,2,2,2,2,2,2,2,2,2,2,2,2,2,2,2,2,2,2,2,2,2,2,2,2,2,2,2,2,2,
2,2,2,2,2,2,2,2,2,2,2,4),(-14.4955154817265,-14.4921015805046,-14.4429921461233,
-14.4195542924433,-14.3994482342011,-14.3738293341153,-14.288601347128,
-14.1640202039879,-14.0702953232699,-13.9997138545117,-13.9588497000149,
-13.9210256786476,-13.8684426683958,-13.6625403707464,-13.5428991907983,
-13.5076878109589,-13.4868239037886,-13.4677532750718,-13.431095049103,
-13.3668216546039,-13.1893972668873,-13.1411775992524,-13.0721555325839,
-13.031562936377,-12.9936280679082,-12.9402713709789,-12.7403375790634,
-12.6172144382479,-12.5816262233561,-12.5606908888506,-12.5416892169662,
-12.5054232410481,-12.4403274337214,-12.2629929906486,-12.214784389061,
-12.1457728406979,-12.1051820907638,-12.0672464351001,-12.0138842923567,
-11.8137937063797,-11.72283332356,-11.6669536294428,-11.6424376059487,-11.622578985395,
-11.5937850759278,-11.4970168396412,-11.3138423765389,-11.2293454773349,
-11.1861864978242,-11.1492448225963,-11.1015126039201,-10.9797513977014,
-10.8558786437209,-10.7526483369395,-10.7230915832855,-10.7031486968195,
-10.6790875506406,-10.6261588459311,-10.5428876384062,-10.4659573371001,
-10.3239452887559,-10.2784953828644,-10.2408278191866,-10.2005761398127,
-10.1334984835463,-10.0873016961473,-9.92521685684855,-9.82588359837368,
-9.79652907563537,-9.7766100200221,-9.75243390964364,-9.69877316019389,
-9.6136419842748,-9.40095006549675,-9.35424691911125,-9.31631112205278,
-9.27654532718786,-9.21222764979518,-9.00669827909516,-8.90102697631658,
-8.870950534164,-8.85094220246908,-8.8271601757043,-8.77597140710462,-8.69700263764407,
-8.46928380234722,-8.42013382164952,-8.38263617210211,-8.34067919193864,
-8.26366977592732,-8.15608774708344,-7.97944719429653,-7.94700264990251,
-7.92683636024456,-7.90417502294572,-7.85951623847511,-7.79537636151634,
-7.54889819588217,-7.49676299144869,-7.45900141417797,-7.4179697725824,
-7.34641793604392,-7.25069311358847,-7.12587250001796,-7.05699974038036,
-7.02250120812312,-7.00380417152983,-6.98248919080206,-6.94494191718322,
-6.8949846511611,-6.74974558110172,-6.62506639957466,-6.57186842119787,
-6.53395716584005,-6.49331174479136,-6.42398451921839,-6.37544251481086,
-6.19536113237998,-6.15273948416572,-6.10950881197842,-6.08472608306475,
-6.06490585258803,-6.0365181463832,-5.94548206320116,-5.69430151266495,
-5.64802322418462,-5.61018064190618,-5.57026049271225,-5.50506440693273,
-5.46078067688279,-5.31151435228598,-5.28830411326515,-5.19347775773949,
-5.16436847469594,-5.1444771683531,-5.12015698276449,-5.06556431195823,
-4.97801994561764,-4.77113274387754,-4.71844772505787,-4.68061005017704,
-4.6397844335495,-4.56942128337941,-4.47614069820228,-4.27632410469421,
-4.24266710881524,-4.2241099891639,-4.20257635055,-4.16391381474872,-4.11184919599735,
-3.95199560771034,-3.88371022260167,-3.811129721386,-3.76992120239732,-3.73221979722566,
-3.68053162209566,-3.50682596208475,-3.34957756713854,-3.31613220568713,
-3.29760956654551,-3.27601709180426,-3.23705248412017,-3.18441010424254,
-3.02022349162204,-3.00028739678404,-2.95464433693914,-2.88364754025106,
-2.8427119762498,-2.82789765027506),.UNSPECIFIED.) ;
#297 = B_SPLINE_CURVE_WITH_KNOTS('',3,(#44573,#44574,#44575,#44576,#44577,
#44578,#44579,#44580,#44581,#44582,#44583,#44584,#44585,#44586,#44587,#44588,
#44589,#44590,#44591,#44592,#44593,#44594,#44595,#44596,#44597,#44598,#44599,
#44600,#44601,#44602,#44603,#44604,#44605,#44606,#44607,#44608,#44609,#44610,
#44611,#44612,#44613,#44614,#44615,#44616,#44617,#44618,#44619,#44620,#44621,
#44622,#44623,#44624,#44625,#44626,#44627,#44628,#44629,#44630,#44631,#44632,
#44633,#44634,#44635,#44636,#44637,#44638,#44639,#44640,#44641,#44642,#44643,
#44644,#44645,#44646,#44647,#44648,#44649,#44650,#44651,#44652,#44653,#44654,
#44655,#44656,#44657,#44658,#44659,#44660,#44661,#44662,#44663,#44664,#44665,
#44666,#44667,#44668,#44669,#44670,#44671,#44672,#44673,#44674,#44675,#44676,
#44677,#44678,#44679,#44680,#44681,#44682,#44683,#44684,#44685,#44686,#44687,
#44688,#44689,#44690,#44691,#44692,#44693,#44694,#44695,#44696,#44697,#44698,
#44699,#44700,#44701,#44702,#44703,#44704,#44705,#44706,#44707,#44708,#44709,
#44710,#44711,#44712,#44713,#44714,#44715,#44716,#44717,#44718,#44719,#44720,
#44721,#44722,#44723,#44724,#44725,#44726,#44727,#44728,#44729,#44730,#44731,
#44732,#44733,#44734,#44735,#44736,#44737,#44738,#44739,#44740,#44741,#44742,
#44743,#44744,#44745,#44746,#44747,#44748,#44749,#44750,#44751,#44752,#44753,
#44754,#44755,#44756,#44757,#44758,#44759,#44760,#44761,#44762,#44763,#44764,
#44765,#44766,#44767,#44768,#44769,#44770,#44771,#44772,#44773,#44774,#44775,
#44776,#44777,#44778,#44779,#44780,#44781,#44782,#44783,#44784,#44785,#44786,
#44787,#44788,#44789,#44790,#44791,#44792,#44793,#44794,#44795,#44796,#44797,
#44798,#44799,#44800,#44801,#44802,#44803,#44804,#44805,#44806,#44807,#44808,
#44809,#44810,#44811,#44812,#44813,#44814,#44815,#44816,#44817,#44818,#44819,
#44820,#44821,#44822,#44823,#44824,#44825,#44826,#44827,#44828,#44829,#44830,
#44831,#44832,#44833,#44834,#44835,#44836,#44837,#44838,#44839,#44840,#44841,
#44842,#44843,#44844,#44845,#44846,#44847,#44848,#44849,#44850,#44851,#44852,
#44853,#44854,#44855,#44856,#44857,#44858,#44859,#44860,#44861,#44862,#44863,
#44864,#44865,#44866,#44867,#44868,#44869,#44870,#44871,#44872,#44873,#44874,
#44875,#44876,#44877,#44878,#44879,#44880,#44881,#44882,#44883,#44884,#44885,
#44886,#44887,#44888,#44889,#44890,#44891,#44892,#44893,#44894,#44895,#44896,
#44897,#44898,#44899,#44900,#44901,#44902,#44903,#44904,#44905,#44906,#44907,
#44908,#44909,#44910,#44911,#44912,#44913,#44914,#44915,#44916,#44917,#44918),
 .UNSPECIFIED.,.F.,.F.,(4,2,2,2,2,2,2,2,2,2,2,2,2,2,2,2,2,2,2,2,2,2,2,2,
2,2,2,2,2,2,2,2,2,2,2,2,2,2,2,2,2,2,2,2,2,2,2,2,2,2,2,2,2,2,2,2,2,2,2,2,
2,2,2,2,2,2,2,2,2,2,2,2,2,2,2,2,2,2,2,2,2,2,2,2,2,2,2,2,2,2,2,2,2,2,2,2,
2,2,2,2,2,2,2,2,2,2,2,2,2,2,2,2,2,2,2,2,2,2,2,2,2,2,2,2,2,2,2,2,2,2,2,2,
2,2,2,2,2,2,2,2,2,2,2,2,2,2,2,2,2,2,2,2,2,2,2,2,2,2,2,2,2,2,2,2,2,2,2,2,
2,2,2,2,4),(-32.1750764478982,-32.0207553169334,-31.9813013241376,-31.9464178057449,
-31.908516085165,-31.8528969676883,-31.7086263720659,-31.528646642724,-31.50065638766,
-31.4844759542813,-31.4643647427817,-31.4387206369914,-31.3514941384981,
-31.311554194876,-31.1674620938463,-31.1035194047997,-31.0526466261229,
-31.0202426277755,-30.982368352764,-30.9359472703877,-30.7210857662802,
-30.6368557993027,-30.583548018481,-30.5594269537457,-30.5394963850721,
-30.5100449398096,-30.4022393723395,-30.1991173198759,-30.1339423933532,
-30.0940252284562,-30.0561793152143,-30.0098890417771,-29.7932611781259,
-29.7099323537193,-29.6569805222344,-29.6329154869372,-29.6129730635167,
-29.5834221965595,-29.4801056572308,-29.3562335811888,-29.2345293742903,
-29.1868019031081,-29.1495203415574,-29.1062179339575,-29.0207918920525,
-28.8343326620093,-28.7706960958894,-28.7262741198875,-28.7036552199766,
-28.6834685260311,-28.6509033227743,-28.5777361234241,-28.401253769229,
-28.353149973984,-28.2842376816045,-28.2436638265746,-28.2057199008725,
-28.1607545267688,-28.0218099534825,-27.8813989465371,-27.8321944101105,
-27.7950504506345,-27.7738141644002,-27.7550604070396,-27.7202293332302,
-27.6058088560617,-27.4618746577715,-27.4184490615059,-27.3541096608302,
-27.3143393972536,-27.2764049412821,-27.2205804084513,-27.0290266593841,
-26.93605909713,-26.8794407852576,-26.854814205345,-26.8349718752996,-26.8063482614371,
-26.7158171125605,-26.5461617183768,-26.4776028718446,-26.4205351055321,
-26.3820181525979,-26.342452768001,-26.2792789873513,-26.1887963941779,
-26.0330924962666,-25.9815993865763,-25.943236842607,-25.9217612811732,
-25.9031676436787,-25.8692915243263,-25.7699242773961,-25.7507713551287,
-25.741627264221,-25.7347998279155,-25.6029889384459,-25.541658071247,-25.4889197060988,
-25.4510732424879,-25.4102644316514,-25.3400047891248,-25.2663898578329,
-25.10757207869,-25.0556471834723,-25.0170575511103,-24.9955375930234,-24.9769710303939,
-24.9432595549775,-24.872657806435,-24.6959079620363,-24.6477709588806,
-24.578827011004,-24.5382475283352,-24.500305885695,-24.4553522124513,-24.2326711685105,
-24.1128746462818,-24.0829405635136,-24.0629503166061,-24.0390930462161,
-23.9874427598014,-23.7352330484433,-23.6580864573933,-23.6161060135417,
-23.5786124867964,-23.5295043894913,-23.3936060694109,-23.3818356569591,
-23.2308869698538,-23.1740059759665,-23.1493405565464,-23.1295038312328,
-23.1009394119394,-23.0118351682198,-22.9703946806594,-22.96247501611,-22.8261832729238,
-22.7840556958983,-22.7210293050245,-22.6814898249792,-22.6434024408258,
-22.5866202859186,-22.4795778109928,-22.4528044631825,-22.3823183919003,
-22.2989789741983,-22.2460228294659,-22.2219570243986,-22.2020146247,-22.1724647241394,
-22.0691279808191,-21.9452553811855,-21.8619640131505,-21.7966901863892,
-21.7567553066748,-21.7189189361172,-21.6726741164618,-21.4550916503824,
-21.3722880192855,-21.3195447577275,-21.2955125674727,-21.275562763714,
-21.2459521953679,-21.1430964664194,-20.9839239494493,-20.9171302953464,
-20.8611017335229,-20.8227540765982,-20.7829394768408,-20.7183494474712,
-20.6313350432498,-20.507299559048),.UNSPECIFIED.) ;
#298 = B_SPLINE_CURVE_WITH_KNOTS('',3,(#44920,#44921,#44922,#44923,#44924,
#44925,#44926,#44927,#44928,#44929,#44930,#44931,#44932,#44933,#44934,#44935,
#44936,#44937,#44938,#44939,#44940,#44941,#44942,#44943,#44944,#44945,#44946,
#44947,#44948,#44949,#44950,#44951,#44952,#44953,#44954,#44955,#44956,#44957,
#44958,#44959,#44960,#44961,#44962,#44963,#44964,#44965,#44966,#44967,#44968,
#44969,#44970,#44971,#44972,#44973,#44974,#44975,#44976,#44977,#44978,#44979,
#44980,#44981,#44982,#44983,#44984,#44985,#44986,#44987,#44988,#44989,#44990,
#44991,#44992,#44993,#44994,#44995,#44996,#44997,#44998,#44999,#45000,#45001,
#45002,#45003,#45004,#45005,#45006,#45007,#45008,#45009,#45010,#45011,#45012,
#45013,#45014,#45015,#45016,#45017,#45018,#45019,#45020,#45021,#45022,#45023,
#45024,#45025,#45026,#45027,#45028,#45029,#45030,#45031,#45032,#45033,#45034,
#45035,#45036,#45037,#45038,#45039,#45040,#45041,#45042,#45043,#45044,#45045),
 .UNSPECIFIED.,.F.,.F.,(4,2,2,2,2,2,2,2,2,2,2,2,2,2,2,2,2,2,2,2,2,2,2,2,
2,2,2,2,2,2,2,2,2,2,2,2,2,2,2,2,2,2,2,2,2,2,2,2,2,2,2,2,2,2,2,2,2,2,2,2,
2,2,4),(-2.82789765027506,-2.80491587923842,-2.75252875979998,-2.69176955209418,
-2.56248106626684,-2.4257920012106,-2.39100182663586,-2.37225547168151,
-2.3510106267097,-2.31382050770316,-2.26452956679996,-2.12356759474721,
-1.98524905487421,-1.94032515680157,-1.9023906560633,-1.86179967690516,
-1.79278379025566,-1.7445701196702,-1.56719242407696,-1.50250281169606,
-1.46604416157332,-1.44700891037799,-1.43290375683057,-1.41340814401782,
-1.41297209775783,-1.41248755497472,-1.4119487288995,-1.41134908705566,
-1.41068125200755,-1.4099368906042,-1.40910659127049,-1.408179729461,-1.40714432181633,
-1.40598687042924,-1.40469219953839,-1.40324328826263,-1.40162110455089,
-1.399804447703,-1.39898693511867,-1.39786866932377,-1.39634240263808,-1.39426620597236,
-1.39145600046461,-1.38768037979173,-1.33858895621796,-1.19887936310669,
-1.05917041085551,-1.01013404551959,-0.978758906063135,-0.939967697712623,
-0.899290885858743,-0.731746744846582,-0.569941484339615,-0.536828717737774,
-0.518359610198079,-0.500213170638933,-0.478073369992099,-0.395171047276128,
-0.210481860352328,-0.118823237187442,-0.0747521515350052,-0.040571949127146,
-1.0000000096877E-6),.UNSPECIFIED.) ;
#299 = B_SPLINE_CURVE_WITH_KNOTS('',3,(#45046,#45047,#45048,#45049,#45050,
#45051,#45052,#45053,#45054,#45055,#45056,#45057,#45058,#45059,#45060,#45061,
#45062,#45063,#45064,#45065,#45066,#45067,#45068,#45069,#45070,#45071,#45072,
#45073,#45074,#45075,#45076,#45077,#45078,#45079,#45080,#45081,#45082,#45083,
#45084,#45085,#45086,#45087,#45088,#45089,#45090,#45091,#45092,#45093,#45094,
#45095,#45096,#45097,#45098,#45099,#45100,#45101,#45102,#45103,#45104,#45105,
#45106,#45107,#45108,#45109,#45110,#45111,#45112,#45113,#45114,#45115,#45116,
#45117,#45118,#45119,#45120,#45121,#45122,#45123,#45124,#45125,#45126,#45127,
#45128,#45129,#45130,#45131,#45132,#45133,#45134,#45135,#45136,#45137,#45138,
#45139,#45140,#45141,#45142,#45143,#45144,#45145,#45146,#45147,#45148,#45149,
#45150,#45151,#45152,#45153,#45154,#45155,#45156,#45157,#45158,#45159,#45160,
#45161,#45162,#45163,#45164,#45165,#45166,#45167,#45168,#45169,#45170,#45171,
#45172,#45173,#45174,#45175,#45176,#45177,#45178,#45179,#45180,#45181,#45182,
#45183,#45184,#45185,#45186,#45187,#45188,#45189,#45190,#45191,#45192,#45193,
#45194,#45195,#45196,#45197,#45198,#45199,#45200,#45201,#45202,#45203,#45204,
#45205,#45206,#45207,#45208,#45209,#45210,#45211,#45212,#45213,#45214,#45215,
#45216,#45217,#45218,#45219,#45220,#45221,#45222,#45223,#45224,#45225,#45226,
#45227,#45228,#45229,#45230,#45231,#45232,#45233,#45234,#45235,#45236,#45237,
#45238,#45239,#45240,#45241,#45242,#45243,#45244,#45245,#45246,#45247,#45248,
#45249,#45250,#45251,#45252,#45253,#45254,#45255,#45256,#45257,#45258,#45259,
#45260,#45261,#45262,#45263,#45264,#45265,#45266,#45267,#45268,#45269,#45270,
#45271,#45272,#45273,#45274,#45275,#45276,#45277,#45278,#45279,#45280,#45281,
#45282,#45283,#45284,#45285,#45286,#45287,#45288,#45289,#45290,#45291,#45292,
#45293,#45294,#45295,#45296,#45297,#45298,#45299,#45300,#45301,#45302,#45303,
#45304,#45305,#45306,#45307,#45308,#45309,#45310,#45311,#45312,#45313,#45314,
#45315,#45316,#45317),.UNSPECIFIED.,.F.,.F.,(4,2,2,2,2,2,2,2,2,2,2,2,2,
2,2,2,2,2,2,2,2,2,2,2,2,2,2,2,2,2,2,2,2,2,2,2,2,2,2,2,2,2,2,2,2,2,2,2,2,
2,2,2,2,2,2,2,2,2,2,2,2,2,2,2,2,2,2,2,2,2,2,2,2,2,2,2,2,2,2,2,2,2,2,2,2,
2,2,2,2,2,2,2,2,2,2,2,2,2,2,2,2,2,2,2,2,2,2,2,2,2,2,2,2,2,2,2,2,2,2,2,2,
2,2,2,2,2,2,2,2,2,2,2,2,2,2,4),(-32.1748014029942,-32.1217728507451,-31.9110886571694,
-31.8419207857683,-31.8081973307716,-31.7862618783361,-31.768148047931,
-31.7495648135089,-31.7157486512336,-31.5633091967486,-31.38845875213,-31.3476096594065,
-31.3108449372146,-31.2737290336029,-31.2225437870683,-30.988005450012,
-30.9168700971781,-30.8825836466127,-30.8604407612231,-30.8462404556041,
-30.826136254408,-30.800525326171,-30.7149601337697,-30.5412074560776,-30.493447215244,
-30.4248631121917,-30.3843476135401,-30.3463795865153,-30.3012915074843,
-30.1658223922661,-30.0230260151101,-29.9734461993299,-29.9361010365137,
-29.914825787547,-29.8961011411747,-29.8614390598299,-29.7273293862152,
-29.7224373879445,-29.5944797563901,-29.5092229360122,-29.4659474170641,
-29.4286642699448,-29.3809007063307,-29.26930398573,-29.1030759131334,-29.0648794349637,
-29.0165932222484,-28.9932951386548,-28.9733737771776,-28.9476916629009,
-28.8599036583143,-28.6879315104497,-28.6403993924543,-28.5720333676748,
-28.5315559770895,-28.4935704548857,-28.4483976917787,-28.3119117671141,
-28.1700738139059,-28.120644190398,-28.0833795867322,-28.0621201037945,
-28.0433841629174,-28.0086556193548,-27.9402827661942,-27.7633040379646,
-27.7151396875567,-27.6461705627761,-27.6055876893548,-27.5676495011915,
-27.5142667021209,-27.3138048905067,-27.2231239297503,-27.1673484243307,
-27.142848279012,-27.122987437994,-27.0941693815941,-27.001789726951,-26.9644116148836,
-26.8227021794838,-26.7796467122456,-26.7156803233494,-26.6759764936705,
-26.6380017183422,-26.5911221199755,-26.3795562256849,-26.2939997356236,
-26.2401733721356,-26.2159715214406,-26.1960576758965,-26.1667478737976,
-26.0682502219196,-26.0515086166581,-26.0468111029761,-25.8991525652874,
-25.8345017653895,-25.7797511522522,-25.7416064300295,-25.7063078392734,
-25.6451885867517,-25.5495665681602,-25.3947774519404,-25.3434140562006,
-25.3051201934907,-25.2836584378892,-25.2650570506229,-25.2311319733638,
-25.1306762208981,-24.9504184135711,-24.8730075399343,-24.8309839665196,
-24.793501035518,-24.7444780002106,-24.6093877280885,-24.4653617847604,
-24.3936680835194,-24.3670843235507,-24.3473580894345,-24.321569669536,
-24.2581952288189,-24.2460425931659,-24.0605977208903,-23.9896890169054,
-23.9312566816054,-23.8925125734221,-23.8578371470493,-23.8007681670583,
-23.694515025,-23.6675550360273,-23.5971764338513,-23.5137804818024,-23.4608024520918,
-23.4367336088587,-23.4167925289507,-23.3872499858046,-23.3353232287531),
 .UNSPECIFIED.) ;
#300 = B_SPLINE_CURVE_WITH_KNOTS('',3,(#45322,#45323,#45324,#45325,#45326,
#45327,#45328,#45329,#45330,#45331,#45332,#45333,#45334,#45335,#45336,#45337,
#45338,#45339,#45340,#45341,#45342,#45343,#45344,#45345,#45346,#45347,#45348,
#45349,#45350,#45351,#45352,#45353,#45354,#45355,#45356,#45357,#45358,#45359,
#45360,#45361,#45362,#45363,#45364,#45365,#45366,#45367,#45368,#45369,#45370,
#45371,#45372,#45373,#45374,#45375,#45376,#45377,#45378,#45379,#45380,#45381,
#45382,#45383,#45384,#45385,#45386,#45387,#45388,#45389,#45390,#45391,#45392,
#45393,#45394,#45395,#45396,#45397,#45398,#45399,#45400,#45401,#45402,#45403,
#45404,#45405,#45406,#45407,#45408,#45409,#45410,#45411,#45412,#45413,#45414,
#45415,#45416,#45417,#45418,#45419,#45420,#45421,#45422,#45423,#45424,#45425,
#45426,#45427,#45428,#45429,#45430,#45431,#45432,#45433,#45434,#45435,#45436,
#45437,#45438,#45439,#45440,#45441,#45442,#45443,#45444,#45445,#45446,#45447,
#45448,#45449,#45450,#45451,#45452,#45453,#45454,#45455,#45456,#45457,#45458,
#45459,#45460,#45461,#45462,#45463,#45464,#45465,#45466,#45467,#45468,#45469,
#45470,#45471,#45472,#45473,#45474,#45475,#45476,#45477,#45478,#45479,#45480,
#45481,#45482,#45483,#45484,#45485,#45486,#45487,#45488,#45489,#45490,#45491,
#45492,#45493,#45494,#45495,#45496,#45497,#45498,#45499,#45500,#45501,#45502,
#45503,#45504,#45505,#45506,#45507,#45508,#45509,#45510,#45511,#45512,#45513,
#45514,#45515,#45516,#45517,#45518,#45519,#45520,#45521,#45522,#45523,#45524,
#45525,#45526,#45527,#45528,#45529,#45530,#45531,#45532,#45533,#45534,#45535,
#45536,#45537,#45538,#45539,#45540,#45541,#45542,#45543,#45544,#45545,#45546,
#45547,#45548,#45549,#45550,#45551,#45552,#45553,#45554,#45555,#45556,#45557,
#45558,#45559,#45560,#45561,#45562,#45563,#45564,#45565,#45566,#45567,#45568,
#45569,#45570,#45571,#45572,#45573,#45574,#45575,#45576,#45577,#45578,#45579,
#45580,#45581,#45582,#45583,#45584,#45585,#45586,#45587,#45588,#45589,#45590,
#45591,#45592,#45593,#45594,#45595,#45596,#45597,#45598,#45599,#45600,#45601,
#45602,#45603,#45604,#45605,#45606,#45607,#45608,#45609,#45610,#45611,#45612,
#45613,#45614,#45615,#45616,#45617,#45618,#45619,#45620,#45621,#45622,#45623,
#45624,#45625,#45626,#45627,#45628,#45629,#45630,#45631,#45632,#45633,#45634,
#45635,#45636,#45637,#45638,#45639,#45640,#45641,#45642,#45643,#45644,#45645,
#45646,#45647,#45648,#45649,#45650,#45651,#45652,#45653,#45654,#45655,#45656,
#45657,#45658,#45659,#45660,#45661,#45662,#45663,#45664,#45665,#45666,#45667,
#45668,#45669,#45670,#45671,#45672,#45673,#45674,#45675,#45676,#45677,#45678,
#45679,#45680,#45681,#45682,#45683,#45684,#45685),.UNSPECIFIED.,.F.,.F.,
(4,2,2,2,2,2,2,2,2,2,2,2,2,2,2,2,2,2,2,2,2,2,2,2,2,2,2,2,2,2,2,2,2,2,2,
2,2,2,2,2,2,2,2,2,2,2,2,2,2,2,2,2,2,2,2,2,2,2,2,2,2,2,2,2,2,2,2,2,2,2,2,
2,2,2,2,2,2,2,2,2,2,2,2,2,2,2,2,2,2,2,2,2,2,2,2,2,2,2,2,2,2,2,2,2,2,2,2,
2,2,2,2,2,2,2,2,2,2,2,2,2,2,2,2,2,2,2,2,2,2,2,2,2,2,2,2,2,2,2,2,2,2,2,2,
2,2,2,2,2,2,2,2,2,2,2,2,2,2,2,2,2,2,2,2,2,2,2,2,2,2,2,2,2,2,2,2,2,2,2,2,
2,2,4),(-11.667685703203,-11.5974316070097,-11.4728113815751,-11.388239375587,
-11.3625934376122,-11.3424815815118,-11.319060060456,-11.2700497058543,
-11.1186800799611,-10.9741112869419,-10.9184720436934,-10.8805665823937,
-10.8407486584663,-10.7761394093138,-10.6940995674359,-10.5889317420429,
-10.560638938262,-10.4639551648775,-10.434611881157,-10.4146937354645,-10.3905101640877,
-10.3368039476596,-10.2515574620737,-10.0391562301076,-9.99240706610917,
-9.95446045546595,-9.91470958945891,-9.85048049035179,-9.80716463512985,
-9.66389607316894,-9.60090983144109,-9.53199958485302,-9.50773402142319,
-9.48786273237982,-9.46342260346886,-9.40804740665859,-9.31843932378605,
-9.11610453475213,-9.06281925821977,-9.02489446901323,-8.98427710712707,
-8.91511519644477,-8.86674841066104,-8.68812478378421,-8.634248218679,-8.59242807224055,
-8.57028917102263,-8.54958726553916,-8.51524638483093,-8.49188971516608,
-8.45358188185071,-8.28631500837497,-8.1761112626246,-8.12830621713902,
-8.09101892603745,-8.04776902200252,-7.96268558383584,-7.83519696495176,
-7.8234755887839,-7.69552189760284,-7.6608178807833,-7.64208571903125,-7.6208195215608,
-7.58352282643212,-7.534034126159,-7.39182402862126,-7.25572991788653,-7.21058800169032,
-7.17260798260029,-7.13211490016285,-7.06366418059457,-7.01604423487268,
-6.84339802489378,-6.75638356189347,-6.73075018124856,-6.71064099122271,
-6.68721180492634,-6.63815517092944,-6.48671312983415,-6.34229597796817,
-6.28665432214012,-6.24874874692571,-6.20893193690682,-6.14432754988181,
-6.06229646880678,-5.95711908004927,-5.92880045397095,-5.83218829117392,
-5.80282200565116,-5.78290135902911,-5.75873146098656,-5.70511192280679,
-5.62008699319999,-5.40711588233199,-5.36045309394554,-5.32252581126531,
-5.28274489541692,-5.218343590184,-5.13669251266178,-5.03102307268413,-4.99997135019261,
-4.90524538946022,-4.8761473308443,-4.85625684222584,-4.83192888097718,
-4.77728807338461,-4.73106933108943,-4.47938065706351,-4.43322146343006,
-4.39540410139643,-4.35543780296601,-4.28998247231869,-4.20634634088272,
-4.08246684328929,-3.98054395488003,-3.95065546503768,-3.93067143708637,
-3.90679098702943,-3.85499474867049,-3.77454239226924,-3.54947440591486,
-3.50021681022972,-3.46270630537767,-3.42080451150579,-3.34412770873095,
-3.28743684411569,-3.18009978881906,-3.16543813015873,-3.0625413429593,
-3.02845485427676,-3.00982669158184,-2.9884072310827,-2.9503292557538,-2.8993744629628,
-2.74743795751088,-2.63545496828495,-2.58044893052033,-2.54264267093298,
-2.50265725830496,-2.43709231660903,-2.23104960744161,-2.12711269220111,
-2.09755713542059,-2.077614443664,-2.05355275275202,-2.0006202909316,-1.91733945460583,
-1.70063633900036,-1.6543508588316,-1.6165064788147,-1.57658853522894,-1.51140636916261,
-1.42828700664986,-1.32457658289954,-1.28695820099813,-1.1986314477956,
-1.17005474682505,-1.15021734082862,-1.14858911206641,-1.14728987946515,
-1.14654805879147,-1.14612909829587,-1.14522873617732,-1.14441150981607,
-1.14366947301655,-1.1429954656423,-1.1156623398666,-1.02845255432607,-0.776871849066619,
-0.724417052628229,-0.686611486371154,-0.649544161006118,-0.63311295881949,
-0.607229325938222,-0.455355961206685,-0.278739403615303,-0.247060802035675,
-0.227017815742242,-0.208598596012939,-0.185182493756475,-0.147428453795999,
-1.00000001260203E-6),.UNSPECIFIED.) ;
#301 = B_SPLINE_CURVE_WITH_KNOTS('',3,(#45686,#45687,#45688,#45689,#45690,
#45691,#45692,#45693,#45694,#45695,#45696,#45697,#45698,#45699,#45700,#45701,
#45702,#45703,#45704,#45705,#45706,#45707,#45708,#45709,#45710,#45711,#45712,
#45713,#45714,#45715,#45716,#45717,#45718,#45719,#45720,#45721,#45722,#45723,
#45724,#45725,#45726,#45727,#45728,#45729,#45730,#45731,#45732,#45733,#45734,
#45735,#45736,#45737,#45738,#45739,#45740,#45741,#45742,#45743,#45744,#45745,
#45746,#45747,#45748,#45749,#45750,#45751,#45752,#45753,#45754,#45755,#45756,
#45757,#45758,#45759,#45760,#45761,#45762,#45763,#45764,#45765,#45766,#45767,
#45768,#45769,#45770,#45771,#45772,#45773,#45774,#45775,#45776,#45777,#45778,
#45779,#45780,#45781,#45782,#45783,#45784,#45785,#45786,#45787,#45788,#45789,
#45790,#45791,#45792,#45793,#45794,#45795,#45796,#45797,#45798,#45799,#45800,
#45801,#45802,#45803,#45804,#45805,#45806,#45807,#45808,#45809,#45810,#45811,
#45812,#45813,#45814,#45815,#45816,#45817,#45818,#45819,#45820,#45821,#45822,
#45823,#45824,#45825,#45826,#45827,#45828,#45829,#45830,#45831,#45832,#45833,
#45834,#45835,#45836,#45837,#45838,#45839,#45840,#45841,#45842,#45843,#45844,
#45845,#45846,#45847,#45848,#45849,#45850,#45851,#45852,#45853,#45854,#45855,
#45856,#45857,#45858,#45859,#45860,#45861,#45862,#45863,#45864,#45865,#45866,
#45867,#45868,#45869,#45870,#45871,#45872,#45873,#45874,#45875,#45876,#45877,
#45878,#45879,#45880,#45881,#45882,#45883,#45884,#45885,#45886,#45887,#45888,
#45889,#45890,#45891,#45892,#45893,#45894,#45895,#45896,#45897,#45898,#45899,
#45900,#45901,#45902,#45903,#45904,#45905,#45906,#45907,#45908,#45909,#45910,
#45911,#45912,#45913,#45914,#45915,#45916,#45917,#45918,#45919,#45920,#45921,
#45922,#45923,#45924,#45925,#45926,#45927,#45928,#45929,#45930,#45931,#45932,
#45933,#45934,#45935,#45936,#45937,#45938,#45939,#45940,#45941,#45942,#45943,
#45944,#45945,#45946,#45947,#45948,#45949,#45950,#45951,#45952,#45953,#45954,
#45955,#45956,#45957,#45958,#45959,#45960,#45961,#45962,#45963,#45964,#45965,
#45966,#45967,#45968,#45969,#45970,#45971,#45972,#45973,#45974,#45975,#45976,
#45977,#45978,#45979,#45980,#45981,#45982,#45983,#45984,#45985,#45986,#45987,
#45988,#45989,#45990,#45991,#45992,#45993,#45994,#45995,#45996,#45997,#45998,
#45999,#46000,#46001,#46002,#46003,#46004,#46005,#46006,#46007,#46008,#46009,
#46010,#46011,#46012,#46013,#46014,#46015,#46016,#46017,#46018,#46019,#46020,
#46021),.UNSPECIFIED.,.F.,.F.,(4,2,2,2,2,2,2,2,2,2,2,2,2,2,2,2,2,2,2,2,
2,2,2,2,2,2,2,2,2,2,2,2,2,2,2,2,2,2,2,2,2,2,2,2,2,2,2,2,2,2,2,2,2,2,2,2,
2,2,2,2,2,2,2,2,2,2,2,2,2,2,2,2,2,2,2,2,2,2,2,2,2,2,2,2,2,2,2,2,2,2,2,2,
2,2,2,2,2,2,2,2,2,2,2,2,2,2,2,2,2,2,2,2,2,2,2,2,2,2,2,2,2,2,2,2,2,2,2,2,
2,2,2,2,2,2,2,2,2,2,2,2,2,2,2,2,2,2,2,2,2,2,2,2,2,2,2,2,2,2,2,2,2,2,2,2,
2,2,2,4),(-23.3353232287531,-23.2836336843603,-23.1597669879378,-23.0766117993692,
-23.011410553683,-22.9714892140942,-22.9336466929956,-22.8873700048232,
-22.670465504122,-22.5872940294445,-22.5344049672141,-22.5103501075281,
-22.4904059026293,-22.4608380148715,-22.3566770690333,-22.2328149271518,
-22.1499579392554,-22.0849145359343,-22.0450208533294,-22.0071619949999,
-21.960810602154,-21.7436000868795,-21.6607478120452,-21.6079856022095,
-21.5839507497518,-21.5640020783355,-21.5343979004054,-21.4297222106453,
-21.2718411334518,-21.226248649101,-21.1597606128989,-21.1196124854158,
-21.0818928015084,-21.0274569293033,-20.84005715869,-20.6974413726604,-20.6667214742891,
-20.6466243023904,-20.6231575702143,-20.5738766568391,-20.4832057966711,
-20.3393116945671,-20.2958929918039,-20.231560821376,-20.1917922543951,
-20.1538576769389,-20.1071610683738,-19.8944172125292,-19.8093027510303,
-19.7556483783176,-19.7314731302676,-19.7115536997074,-19.6821971135982,
-19.5828258142415,-19.4207723138667,-19.3745799675933,-19.3075064088695,
-19.26725522758,-19.2295869505261,-19.1841347141394,-19.0419469538013,-18.9050282021086,
-18.8350619139842,-18.8086754926488,-18.7908855514234,-18.7657158095996,
-18.7086357071888,-18.6297396143924,-18.5230143732836,-18.442334207463,
-18.3784539759465,-18.3387648031809,-18.3007794290804,-18.253854408906,
-18.0382158373008,-17.9553268138185,-17.9025498101062,-17.8785124860334,
-17.8585641498629,-17.8289638313947,-17.7260579793596,-17.6021830902463,
-17.5187317541391,-17.4533736063989,-17.4134241267227,-17.3755966089807,
-17.3204559828818,-17.128328726292,-17.034751643352,-16.9779117914376,-16.95325250703,
-16.933414999532,-16.9048415322082,-16.8163979931498,-16.6451222197646,
-16.5976796631281,-16.5293988090945,-16.4889355510299,-16.4509419474887,
-16.3971896204609,-16.1482849279925,-16.0876403506079,-16.0446502676035,
-16.0222933193482,-16.001722798788,-15.9681072300132,-15.9252723255546,
-15.8194108553877,-15.7788843401984,-15.6343652298015,-15.5889389460784,
-15.5512756036654,-15.5110125094001,-15.4438736671729,-15.3976144736802,
-15.2350904277882,-15.1362980871434,-15.1069714197455,-15.0870551794142,
-15.0628619666166,-15.0090939145782,-14.9236887794412,-14.7117078992256,
-14.6648931206517,-14.6269319683612,-14.587204069174,-14.5231055020978,
-14.4799193883562,-14.3374321834459,-14.320088167473,-14.2192161202029,
-14.1852686149023,-14.1666632176757,-14.1452066779954,-14.1069411468773,
-14.055632052595,-13.9012291566851,-13.8033983278317,-13.7431414538368,
-13.7079773708991,-13.6697247418832,-13.6142897791556,-13.4062335559749,
-13.3797718028052,-13.2834220783063,-13.2541494193847,-13.2342393781621,
-13.2100147758301,-13.1560446141659,-13.0701192042578,-12.8595611044772,
-12.8073623837127,-12.7695912504969,-12.7285822922506,-12.6571665694385,
-12.4489214808299,-12.3561288309886,-12.3272611370388,-12.3073947818981,
-12.2829247002842,-12.227351545166,-12.0267256243128,-11.9192684382317,
-11.8724689891664,-11.8352443755935,-11.7912636631108,-11.7012933700652,
-11.6675653273102),.UNSPECIFIED.) ;
#302 = B_SPLINE_CURVE_WITH_KNOTS('',3,(#46026,#46027,#46028,#46029,#46030,
#46031,#46032,#46033,#46034,#46035,#46036,#46037,#46038,#46039,#46040,#46041,
#46042,#46043,#46044,#46045,#46046,#46047,#46048,#46049,#46050,#46051,#46052,
#46053,#46054,#46055,#46056,#46057,#46058,#46059,#46060,#46061,#46062,#46063,
#46064,#46065,#46066,#46067,#46068,#46069,#46070,#46071,#46072,#46073,#46074,
#46075,#46076,#46077,#46078,#46079,#46080,#46081,#46082,#46083,#46084,#46085,
#46086,#46087,#46088,#46089,#46090,#46091,#46092,#46093,#46094,#46095,#46096,
#46097,#46098,#46099,#46100,#46101,#46102,#46103,#46104,#46105,#46106,#46107,
#46108,#46109,#46110,#46111,#46112,#46113,#46114,#46115,#46116,#46117,#46118,
#46119,#46120,#46121,#46122,#46123,#46124,#46125,#46126,#46127,#46128,#46129,
#46130,#46131,#46132,#46133,#46134,#46135,#46136,#46137,#46138,#46139,#46140,
#46141,#46142,#46143,#46144,#46145,#46146,#46147,#46148,#46149,#46150,#46151,
#46152,#46153,#46154,#46155,#46156,#46157,#46158,#46159,#46160,#46161,#46162,
#46163,#46164,#46165,#46166,#46167,#46168,#46169,#46170,#46171,#46172,#46173,
#46174,#46175,#46176,#46177,#46178,#46179,#46180,#46181,#46182,#46183,#46184,
#46185,#46186,#46187,#46188,#46189,#46190,#46191,#46192,#46193,#46194,#46195,
#46196,#46197,#46198,#46199,#46200,#46201,#46202,#46203,#46204,#46205,#46206,
#46207,#46208,#46209,#46210,#46211,#46212,#46213,#46214,#46215,#46216,#46217,
#46218,#46219,#46220,#46221,#46222,#46223,#46224,#46225,#46226,#46227,#46228,
#46229,#46230,#46231,#46232,#46233,#46234,#46235,#46236,#46237,#46238,#46239,
#46240,#46241,#46242,#46243,#46244,#46245,#46246,#46247,#46248,#46249,#46250,
#46251,#46252,#46253,#46254,#46255,#46256,#46257,#46258,#46259,#46260,#46261,
#46262,#46263,#46264,#46265,#46266,#46267,#46268,#46269,#46270,#46271,#46272,
#46273,#46274,#46275,#46276,#46277,#46278,#46279,#46280,#46281,#46282,#46283,
#46284,#46285,#46286,#46287,#46288,#46289,#46290,#46291,#46292,#46293,#46294,
#46295,#46296,#46297,#46298,#46299,#46300,#46301,#46302,#46303,#46304,#46305,
#46306,#46307,#46308,#46309,#46310,#46311,#46312,#46313,#46314,#46315,#46316,
#46317,#46318,#46319,#46320,#46321,#46322,#46323,#46324,#46325,#46326,#46327,
#46328,#46329,#46330,#46331,#46332,#46333,#46334,#46335,#46336,#46337,#46338,
#46339,#46340,#46341,#46342,#46343,#46344,#46345,#46346,#46347,#46348,#46349,
#46350,#46351,#46352,#46353,#46354,#46355,#46356,#46357,#46358,#46359,#46360,
#46361),.UNSPECIFIED.,.F.,.F.,(4,2,2,2,2,2,2,2,2,2,2,2,2,2,2,2,2,2,2,2,
2,2,2,2,2,2,2,2,2,2,2,2,2,2,2,2,2,2,2,2,2,2,2,2,2,2,2,2,2,2,2,2,2,2,2,2,
2,2,2,2,2,2,2,2,2,2,2,2,2,2,2,2,2,2,2,2,2,2,2,2,2,2,2,2,2,2,2,2,2,2,2,2,
2,2,2,2,2,2,2,2,2,2,2,2,2,2,2,2,2,2,2,2,2,2,2,2,2,2,2,2,2,2,2,2,2,2,2,2,
2,2,2,2,2,2,2,2,2,2,2,2,2,2,2,2,2,2,2,2,2,2,2,2,2,2,2,2,2,2,2,2,2,2,2,2,
2,2,2,4),(-23.3355609284769,-23.2597287932774,-23.222225214567,-23.1167937467186,
-23.0349671579936,-22.970471448011,-22.9306716603284,-22.8927506184788,
-22.8461267646939,-22.6328417921701,-22.5479273841423,-22.4943501547635,
-22.4701863473356,-22.4502652883526,-22.4208902220894,-22.324326615371,
-22.295965597956,-22.190758663422,-22.1087525408583,-22.0441626782366,-22.0043511077128,
-21.9664486753242,-21.9108091228529,-21.7661909080502,-21.6148359855681,
-21.5658384152302,-21.542420742005,-21.5223090739911,-21.4966619460148,
-21.4093946091982,-21.3656175211198,-21.2241436401028,-21.1341396575724,
-21.0901521948904,-21.0529251825028,-21.0061266185742,-20.900500509744,
-20.6979596889977,-20.6424521270335,-20.6179906439059,-20.5981217166481,
-20.569235622051,-20.4762894630837,-20.3088312370607,-20.2406290264233,
-20.1837707184177,-20.1452890794756,-20.1056772895833,-20.0422349775556,
-19.9524022454156,-19.7965777892175,-19.7450676412924,-19.7066963236677,
-19.6852196704393,-19.666627582009,-19.6327603484839,-19.5625011539637,
-19.3857148475227,-19.3375731352389,-19.268624464095,-19.2280438247443,
-19.1901019842602,-19.1451490323796,-18.9224525442309,-18.8406516377513,
-18.7883096075161,-18.7643409489732,-18.7443765958703,-18.7146490032512,
-18.6091820724899,-18.4028767473322,-18.3384652674937,-18.2986821920745,
-18.2607554267598,-18.2140966586248,-18.0010833329753,-17.9160690783646,
-17.8624534034883,-17.8382839374336,-17.8183629236402,-17.7889951995181,
-17.692386261373,-17.6640648724364,-17.5588847300649,-17.4768551992637,
-17.4122512188597,-17.3724340540874,-17.3345277451068,-17.2788842798252,
-17.1344789791574,-16.9830255971562,-16.9339633145125,-16.9105329295557,
-16.8904236533959,-16.8647911132839,-16.7799269527606,-16.6056779782297,
-16.557853550413,-16.4892070546307,-16.4486792379562,-16.4107139895469,
-16.3656463550079,-16.2304299890274,-16.0873796485533,-16.0377588955467,
-16.0003912625658,-15.9791109182628,-15.9603882297376,-15.9257413546584,
-15.8150473175076,-15.6683381522635,-15.5766415197884,-15.5324117847278,
-15.4952004255303,-15.448709384268,-15.3687398273464,-15.1734945703925,
-15.091969191924,-15.064378514863,-15.0464838897029,-15.0222268448732,-14.9680489709915,
-14.9374316069859,-14.7666760261359,-14.6585565290365,-14.6115564470379,
-14.5743207148758,-14.5304932832417,-14.4415745340718,-14.3033318174456,
-14.2657208310757,-14.1693589954677,-14.1400849184509,-14.1201745068449,
-14.0959502124043,-14.0419832792392,-13.9560668426929,-13.7454784744436,
-13.6932842652118,-13.6555133797642,-13.6145019552021,-13.5430739617164,
-13.3338533275426,-13.2418465028581,-13.2130717535092,-13.1932145700271,
-13.1686851991473,-13.1127194909873,-13.02152844155,-12.821763904206,-12.7684100370052,
-12.7304748610735,-12.6898799021145,-12.6208483030156,-12.5726191450503,
-12.3951246716236,-12.3314273615835,-12.2944906744239,-12.2753705715818,
-12.2545542479143,-12.2195978170628,-12.1022591009582,-11.8934143193826,
-11.8408999442353,-11.8030847950654,-11.7621939182167,-11.6914624396032,
-11.667685703203),.UNSPECIFIED.) ;
#303 = B_SPLINE_CURVE_WITH_KNOTS('',3,(#46362,#46363,#46364,#46365,#46366,
#46367,#46368,#46369,#46370,#46371,#46372,#46373,#46374,#46375,#46376,#46377,
#46378,#46379,#46380,#46381,#46382,#46383,#46384,#46385,#46386,#46387,#46388,
#46389,#46390,#46391,#46392,#46393,#46394,#46395,#46396,#46397,#46398,#46399,
#46400,#46401,#46402,#46403,#46404,#46405,#46406,#46407,#46408,#46409,#46410,
#46411,#46412,#46413,#46414,#46415,#46416,#46417,#46418,#46419,#46420,#46421,
#46422,#46423,#46424,#46425,#46426,#46427,#46428,#46429,#46430,#46431,#46432,
#46433,#46434,#46435,#46436,#46437,#46438,#46439,#46440,#46441,#46442,#46443,
#46444,#46445,#46446,#46447,#46448,#46449,#46450,#46451,#46452,#46453,#46454,
#46455,#46456,#46457,#46458,#46459,#46460,#46461,#46462,#46463,#46464,#46465,
#46466,#46467,#46468,#46469,#46470,#46471,#46472,#46473,#46474,#46475,#46476,
#46477,#46478,#46479,#46480,#46481,#46482,#46483,#46484,#46485,#46486,#46487,
#46488,#46489,#46490,#46491,#46492,#46493,#46494,#46495,#46496,#46497,#46498,
#46499,#46500,#46501,#46502,#46503,#46504,#46505,#46506,#46507,#46508,#46509,
#46510,#46511,#46512,#46513,#46514,#46515,#46516,#46517,#46518,#46519,#46520,
#46521,#46522,#46523,#46524,#46525,#46526,#46527,#46528,#46529,#46530,#46531,
#46532,#46533,#46534,#46535,#46536,#46537,#46538,#46539,#46540,#46541,#46542,
#46543,#46544,#46545,#46546,#46547,#46548,#46549,#46550,#46551,#46552,#46553,
#46554,#46555,#46556,#46557,#46558,#46559,#46560,#46561,#46562,#46563,#46564,
#46565,#46566,#46567,#46568,#46569,#46570,#46571,#46572,#46573,#46574,#46575,
#46576,#46577,#46578,#46579,#46580,#46581,#46582,#46583,#46584,#46585,#46586,
#46587,#46588,#46589,#46590,#46591,#46592,#46593,#46594,#46595,#46596,#46597,
#46598,#46599,#46600,#46601,#46602,#46603,#46604,#46605,#46606,#46607,#46608,
#46609,#46610,#46611,#46612,#46613,#46614,#46615,#46616,#46617,#46618,#46619,
#46620,#46621,#46622,#46623,#46624,#46625,#46626,#46627,#46628,#46629,#46630,
#46631,#46632,#46633,#46634,#46635,#46636,#46637,#46638,#46639,#46640,#46641,
#46642,#46643,#46644,#46645,#46646,#46647,#46648,#46649,#46650,#46651,#46652,
#46653,#46654,#46655,#46656,#46657,#46658,#46659,#46660,#46661,#46662,#46663,
#46664,#46665,#46666,#46667,#46668,#46669,#46670,#46671,#46672,#46673,#46674,
#46675,#46676,#46677,#46678,#46679,#46680,#46681,#46682,#46683,#46684,#46685,
#46686,#46687,#46688,#46689,#46690,#46691,#46692,#46693,#46694,#46695,#46696,
#46697,#46698,#46699,#46700,#46701,#46702,#46703,#46704,#46705),
 .UNSPECIFIED.,.F.,.F.,(4,2,2,2,2,2,2,2,2,2,2,2,2,2,2,2,2,2,2,2,2,2,2,2,
2,2,2,2,2,2,2,2,2,2,2,2,2,2,2,2,2,2,2,2,2,2,2,2,2,2,2,2,2,2,2,2,2,2,2,2,
2,2,2,2,2,2,2,2,2,2,2,2,2,2,2,2,2,2,2,2,2,2,2,2,2,2,2,2,2,2,2,2,2,2,2,2,
2,2,2,2,2,2,2,2,2,2,2,2,2,2,2,2,2,2,2,2,2,2,2,2,2,2,2,2,2,2,2,2,2,2,2,2,
2,2,2,2,2,2,2,2,2,2,2,2,2,2,2,2,2,2,2,2,2,2,2,2,2,2,2,2,2,2,2,2,2,2,2,2,
2,2,2,4),(-11.6675653273102,-11.5599168418434,-11.5138978859093,-11.4286591377124,
-11.4030401139979,-11.3829338798932,-11.3594956788994,-11.3103851182522,
-11.158858251161,-11.0146362717321,-10.9589821415689,-10.9210747439862,
-10.88126140232,-10.8166759692942,-10.7346802388235,-10.6294574700789,-10.6010083746183,
-10.5044076668633,-10.4750857885122,-10.4551703247593,-10.4309748975263,
-10.3771912316371,-10.2917452730081,-10.0798798522952,-10.033047849607,
-9.99508325386252,-9.95536212172787,-9.89129978676861,-9.77864771153884,
-9.58591803710041,-9.55270602054035,-9.53422075328706,-9.51256083029925,
-9.47325028766468,-9.41994299387689,-9.25057680579537,-9.14160855047381,
-9.09430226539542,-9.05704949204078,-9.01345156463859,-8.92607244779549,
-8.79226385861574,-8.76997211879241,-8.7398532298263,-8.65004988525598,
-8.62147046078619,-8.60163258060766,-8.57697768547286,-8.52016631170477,
-8.42666703187411,-8.23465175162409,-8.17941132443611,-8.1415686792487,
-8.10164678549299,-8.03644362733608,-7.99361729264837,-7.84751934126576,
-7.8132801927561,-7.72368356416008,-7.69511152101925,-7.67527438556438,
-7.65061475848494,-7.59377101735208,-7.50018232480575,-7.30804148474877,
-7.25291997497611,-7.21509581752658,-7.17514188290794,-7.10975626871894,
-7.02625217938331,-6.90237607585637,-6.79966350634897,-6.77002270784409,
-6.7500696742293,-6.72605531614973,-6.6734216888468,-6.59089159087684,-6.37281143620365,
-6.32659770885665,-6.28876881795864,-6.2488237484525,-6.18348767917299,
-6.10007723808647,-5.9762037781576,-5.87317433023502,-5.84359489475306,
-5.82364939269744,-5.79960120016814,-5.74675369433131,-5.66368658126237,
-5.44660058565869,-5.40033301199408,-5.36249261974491,-5.3225681743427,
-5.25734844163975,-5.05044538559886,-4.94670944706507,-4.91716409227892,
-4.89722272587147,-4.87315557143905,-4.82018792259332,-4.73681806161008,
-4.66686438021753,-4.63281709456112,-4.55575940012506,-4.48698750433858,
-4.44643899776407,-4.40848544550055,-4.35499874965015,-4.29244025956197,
-4.15501239002384,-4.02572471520113,-3.9935906114256,-3.97347515068028,
-3.95069921434655,-3.90540206240404,-3.87067828988611,-3.73331562450593,
-3.59170345279729,-3.54625997369065,-3.5085940574052,-3.46834032614663,
-3.40124916719926,-3.3550382379002,-3.19285128415213,-3.09364913210538,
-3.06430162556963,-3.0443835577571,-3.02020382675209,-2.96651880486555,
-2.88132485994284,-2.66880115808774,-2.62207346237968,-2.58413253698623,
-2.54437601617899,-2.48010929894564,-2.37234582510119,-2.18914481939562,
-2.14803908722876,-2.12603539898619,-2.10524481282176,-2.07042276007788,
-1.94444877599146,-1.74586073057188,-1.69255191172432,-1.65462457524464,
-1.61401689884784,-1.54490566428976,-1.45415188442675,-1.24868373760917,
-1.2155060805417,-1.19702656937367,-1.18210690130692,-1.18162985498578,
-1.1811982453945,-1.1523101414957,-1.11465893813669,-1.03103382139579,-0.816009129807846,
-0.769297196591649,-0.731359689374574,-0.695161004090526,-0.665273959345048,
-0.612753371120607,-0.515190768148353,-0.322330617910769,-0.289141854711983,
-0.270660559861515,-0.252517933370279,-0.23040098625164,-0.196185058895016,
-1.00000001085343E-6),.UNSPECIFIED.) ;
#304 = B_SPLINE_CURVE_WITH_KNOTS('',3,(#46708,#46709,#46710,#46711,#46712,
#46713,#46714,#46715,#46716,#46717,#46718,#46719,#46720,#46721,#46722,#46723,
#46724,#46725,#46726,#46727,#46728,#46729,#46730,#46731,#46732,#46733,#46734,
#46735,#46736,#46737,#46738,#46739,#46740,#46741,#46742,#46743,#46744,#46745,
#46746,#46747,#46748,#46749,#46750,#46751,#46752,#46753,#46754,#46755,#46756,
#46757,#46758,#46759,#46760,#46761,#46762,#46763,#46764,#46765,#46766,#46767,
#46768,#46769,#46770,#46771,#46772,#46773,#46774,#46775,#46776,#46777,#46778,
#46779,#46780,#46781,#46782,#46783,#46784,#46785,#46786,#46787,#46788,#46789,
#46790,#46791,#46792,#46793,#46794,#46795,#46796,#46797,#46798,#46799,#46800,
#46801,#46802,#46803,#46804,#46805,#46806,#46807,#46808,#46809,#46810,#46811,
#46812,#46813,#46814,#46815,#46816,#46817,#46818,#46819,#46820,#46821,#46822,
#46823,#46824,#46825,#46826,#46827,#46828,#46829,#46830,#46831,#46832,#46833,
#46834,#46835,#46836,#46837,#46838,#46839,#46840,#46841,#46842,#46843,#46844,
#46845,#46846,#46847,#46848,#46849,#46850,#46851,#46852,#46853,#46854,#46855,
#46856,#46857,#46858,#46859,#46860,#46861,#46862,#46863,#46864,#46865,#46866,
#46867,#46868,#46869,#46870,#46871,#46872,#46873,#46874,#46875,#46876,#46877,
#46878,#46879,#46880,#46881,#46882,#46883,#46884,#46885,#46886,#46887,#46888,
#46889,#46890,#46891,#46892,#46893,#46894,#46895,#46896,#46897,#46898,#46899,
#46900,#46901,#46902,#46903,#46904,#46905,#46906,#46907,#46908,#46909,#46910,
#46911,#46912,#46913,#46914,#46915,#46916,#46917,#46918,#46919,#46920,#46921,
#46922,#46923,#46924,#46925,#46926,#46927,#46928,#46929,#46930,#46931,#46932,
#46933,#46934,#46935,#46936,#46937,#46938,#46939,#46940,#46941,#46942,#46943,
#46944,#46945,#46946,#46947,#46948,#46949,#46950,#46951,#46952,#46953,#46954,
#46955,#46956,#46957,#46958,#46959,#46960,#46961,#46962,#46963,#46964,#46965,
#46966,#46967,#46968,#46969,#46970,#46971,#46972,#46973,#46974,#46975,#46976,
#46977,#46978,#46979,#46980,#46981,#46982,#46983,#46984,#46985,#46986,#46987,
#46988,#46989,#46990,#46991,#46992,#46993,#46994,#46995,#46996,#46997,#46998,
#46999,#47000,#47001,#47002,#47003,#47004,#47005,#47006,#47007,#47008,#47009,
#47010,#47011,#47012,#47013,#47014,#47015,#47016,#47017,#47018,#47019,#47020,
#47021,#47022,#47023,#47024,#47025,#47026,#47027,#47028,#47029,#47030,#47031,
#47032,#47033,#47034,#47035,#47036,#47037,#47038,#47039,#47040,#47041,#47042,
#47043,#47044,#47045,#47046,#47047),.UNSPECIFIED.,.F.,.F.,(4,2,2,2,2,2,
2,2,2,2,2,2,2,2,2,2,2,2,2,2,2,2,2,2,2,2,2,2,2,2,2,2,2,2,2,2,2,2,2,2,2,2,
2,2,2,2,2,2,2,2,2,2,2,2,2,2,2,2,2,2,2,2,2,2,2,2,2,2,2,2,2,2,2,2,2,2,2,2,
2,2,2,2,2,2,2,2,2,2,2,2,2,2,2,2,2,2,2,2,2,2,2,2,2,2,2,2,2,2,2,2,2,2,2,2,
2,2,2,2,2,2,2,2,2,2,2,2,2,2,2,2,2,2,2,2,2,2,2,2,2,2,2,2,2,2,2,2,2,2,2,2,
2,2,2,2,2,2,2,2,2,2,2,2,2,2,2,2,2,2,2,4),(-8.83672325566634,-8.72339974280114,
-8.68386166002427,-8.64898714110386,-8.61113228183851,-8.55580942003574,
-8.41502260358477,-8.24221691069678,-8.2075784098526,-8.18873874032175,
-8.16887711629528,-8.14004990527668,-8.04759292469131,-8.02017856555552,
-7.87175350041695,-7.80695344124842,-7.75554249950216,-7.72279298257082,
-7.68495941869026,-7.63872276554454,-7.39884911134843,-7.32969916943655,
-7.29598074784733,-7.2955179103999,-7.29510143853705,-7.29472630908798,
-7.29438810083793,-7.29408291437532,-7.293807303533,-7.2935582167102,-7.29277562897946,
-7.29202378623707,-7.29130089086543,-7.29060525972034,-7.28993531600412,
-7.28928958179882,-7.2886666710752,-7.28806528324593,-7.28748419720352,
-7.28692226574861,-7.28637841042325,-7.28585161673894,-7.28534092970952,
-7.28484544971679,-7.28436432868456,-7.28389676647281,-7.28344200755974,
-7.28299933792181,-7.28256808213522,-7.28214760070153,-7.28173728752033,
-7.28133656751879,-7.25871267664155,-7.2385286762415,-7.20597878339026,
-7.13277680018572,-6.95631015395828,-6.90820931273134,-6.83930044602996,
-6.7987276617651,-6.76078407611064,-6.7158182518756,-6.57685725872102,-6.56230945149741,
-6.43287466606539,-6.36484382465875,-6.33868687537384,-6.3209106907098,
-6.29554250608781,-6.24019703235213,-6.15517165334181,-6.01508567695931,
-5.92554561400664,-5.88162904051464,-5.84440243176646,-5.79752642833198,
-5.69330620821936,-5.48953004821778,-5.43405628175592,-5.40960168586134,
-5.38973203905418,-5.36083768558537,-5.26782049869653,-5.10044717430939,
-5.03225969114084,-4.9754096148371,-4.93692739785334,-4.90201110844253,
-4.84336205128404,-4.74133357887729,-4.58766642049797,-4.5364620580424,
-4.49825191469023,-4.47680613613605,-4.45556687016721,-4.41839852922431,
-4.27942759244415,-4.10338407788865,-4.0476993631982,-4.00979041154072,
-3.96999151060022,-3.90547052297783,-3.82359252103421,-3.71821960242769,
-3.60344920293334,-3.56894117433974,-3.55024320585233,-3.5289305704546,
-3.49139794606272,-3.44146906294306,-3.29642535072114,-3.18159511238375,
-3.12376680441117,-3.08897503512535,-3.0503597725156,-2.9927092509224,-2.92315179708276,
-2.74707523567595,-2.6700207679134,-2.63913558248495,-2.61920824042201,
-2.59590213134742,-2.54759846309893,-2.5093829502471,-2.34293671861362,
-2.23190743042217,-2.1841018291998,-2.14681130373033,-2.10355330181405,
-2.01843491008466,-1.89086859611604,-1.88015634021239,-1.8415520780261,
-1.74116925266082,-1.71156202771834,-1.6916255070351,-1.66764616256745,
-1.61510573303749,-1.53280351586751,-1.31373289219991,-1.26755185166437,
-1.22975151575445,-1.19703210946525,-1.1456923152463,-1.08096298290102,
-0.932797394368955,-0.815064462429085,-0.785120838675239,-0.765424231108012,
-0.750109886792035,-0.749330846664115,-0.748554575935521,-0.747758918081246,
-0.746921327833159,-0.746016452447542,-0.745013409506678,-0.743872194103966,
-0.742538455551737,-0.740935468372936,-0.738951391871269,-0.736418772801353,
-0.733081877396021,-0.701181541314413,-0.638260302490662,-0.386295812752923,
-0.340986276786363,-0.302905898673403,-0.267984339448119,-0.227731199758877,
-1.96846129342848E-5),.UNSPECIFIED.) ;
#305 = B_SPLINE_CURVE_WITH_KNOTS('',3,(#47050,#47051,#47052,#47053,#47054,
#47055,#47056,#47057,#47058,#47059,#47060,#47061,#47062,#47063,#47064,#47065,
#47066,#47067,#47068,#47069,#47070,#47071,#47072,#47073,#47074,#47075,#47076,
#47077,#47078,#47079,#47080,#47081,#47082,#47083,#47084,#47085,#47086,#47087,
#47088,#47089,#47090,#47091,#47092,#47093,#47094,#47095,#47096,#47097,#47098,
#47099,#47100,#47101,#47102,#47103,#47104,#47105,#47106,#47107,#47108,#47109,
#47110,#47111,#47112,#47113,#47114,#47115,#47116,#47117,#47118,#47119,#47120,
#47121,#47122,#47123,#47124,#47125,#47126,#47127,#47128,#47129,#47130,#47131,
#47132,#47133,#47134,#47135,#47136,#47137,#47138,#47139,#47140,#47141,#47142,
#47143,#47144,#47145,#47146,#47147,#47148,#47149,#47150,#47151,#47152,#47153,
#47154,#47155,#47156,#47157,#47158,#47159,#47160,#47161,#47162,#47163,#47164,
#47165,#47166,#47167,#47168,#47169,#47170,#47171,#47172,#47173,#47174,#47175,
#47176,#47177,#47178,#47179,#47180,#47181,#47182,#47183,#47184,#47185,#47186,
#47187,#47188,#47189,#47190,#47191,#47192,#47193,#47194,#47195,#47196,#47197,
#47198,#47199,#47200,#47201,#47202,#47203,#47204,#47205,#47206,#47207,#47208,
#47209,#47210,#47211,#47212,#47213,#47214,#47215,#47216,#47217,#47218,#47219,
#47220,#47221,#47222,#47223,#47224,#47225,#47226,#47227,#47228,#47229,#47230,
#47231,#47232,#47233,#47234,#47235,#47236,#47237,#47238,#47239,#47240,#47241,
#47242,#47243,#47244,#47245,#47246,#47247,#47248,#47249,#47250,#47251),
 .UNSPECIFIED.,.F.,.F.,(4,2,2,2,2,2,2,2,2,2,2,2,2,2,2,2,2,2,2,2,2,2,2,2,
2,2,2,2,2,2,2,2,2,2,2,2,2,2,2,2,2,2,2,2,2,2,2,2,2,2,2,2,2,2,2,2,2,2,2,2,
2,2,2,2,2,2,2,2,2,2,2,2,2,2,2,2,2,2,2,2,2,2,2,2,2,2,2,2,2,2,2,2,2,2,2,2,
2,2,2,2,4),(-29.8748049370787,-29.8559623263054,-29.8310093407934,-29.6893565955101,
-29.5245377048083,-29.4841327566667,-29.4484770034037,-29.4099263933365,
-29.3532477761587,-29.1334555528409,-29.0344403123814,-28.9931722782713,
-28.9806683328654,-28.9750709988028,-28.9701189579125,-28.9663087516873,
-28.9638773537707,-28.9624017958589,-28.9446163187811,-28.9239575025797,
-28.8902752588268,-28.7426392944441,-28.622747079501,-28.5644150487242,
-28.5247241046179,-28.4897947109261,-28.4519297175056,-28.4056792359559,
-28.1853058710086,-28.1031483881522,-28.0507279668659,-28.0268697609116,
-28.0068883743685,-27.9771754794791,-27.8770101891862,-27.716092888132,
-27.6488512352504,-27.5924426658416,-27.5537667007694,-27.5135072819418,
-27.447781589121,-27.3257844177079,-27.174462736726,-27.1251475022996,-27.1015241115852,
-27.0813434574031,-27.0555673010956,-26.965667719789,-26.7956413031322,
-26.7484167986561,-26.6804349480034,-26.6401647951043,-26.6023882827539,
-26.5575180680391,-26.3319888718872,-26.2506379027527,-26.1985035135455,
-26.1746709129656,-26.154771559656,-26.1252144797171,-26.0217843114692,
-25.8978541335425,-25.8144945360647,-25.749142711359,-25.709129919641,-25.6711894328127,
-25.6157535961383,-25.4236732396369,-25.3312904716796,-25.274881413357,
-25.2502336066244,-25.2303427726501,-25.2015490711106,-25.109484335517,
-24.9413172978235,-24.8730218149808,-24.8161221980946,-24.7776560442992,
-24.7427880945695,-24.6843187969317,-24.5809851745903,-24.4276278117773,
-24.3764628207489,-24.3382797304737,-24.3168593827777,-24.2982644115716,
-24.2643468836702,-24.1640124207224,-24.0091390279228,-23.9639888264052,
-23.8979316861805,-23.8578560675221,-23.820091020739,-23.7653775833646,
-23.5729497659355,-23.4790726889548,-23.4221257040589,-23.3974458025519,
-23.3776043580981,-23.3490370914111,-23.3355609284769),.UNSPECIFIED.) ;
#306 = B_SPLINE_CURVE_WITH_KNOTS('',3,(#47254,#47255,#47256,#47257,#47258,
#47259,#47260,#47261,#47262,#47263,#47264,#47265,#47266,#47267,#47268,#47269,
#47270,#47271,#47272,#47273,#47274,#47275,#47276,#47277,#47278,#47279,#47280,
#47281,#47282,#47283,#47284,#47285,#47286,#47287,#47288,#47289,#47290,#47291,
#47292,#47293,#47294,#47295,#47296,#47297,#47298,#47299,#47300,#47301,#47302,
#47303,#47304,#47305,#47306,#47307,#47308,#47309,#47310,#47311,#47312,#47313,
#47314,#47315,#47316,#47317,#47318,#47319,#47320,#47321,#47322,#47323,#47324,
#47325,#47326,#47327,#47328,#47329,#47330,#47331,#47332,#47333,#47334,#47335,
#47336,#47337,#47338,#47339,#47340,#47341,#47342,#47343,#47344,#47345,#47346,
#47347,#47348,#47349,#47350,#47351,#47352,#47353,#47354,#47355,#47356,#47357,
#47358,#47359,#47360,#47361,#47362,#47363,#47364,#47365),.UNSPECIFIED.,
 .F.,.F.,(4,2,2,2,2,2,2,2,2,2,2,2,2,2,2,2,2,2,2,2,2,2,2,2,2,2,2,2,2,2,2,
2,2,2,2,2,2,2,2,2,2,2,2,2,2,2,2,2,2,2,2,2,2,2,2,4),(-10.5425049368748,-10.4813665573713,
-10.3082210802619,-10.0952472441292,-9.95794965199355,-9.84959651696192,
-9.68102697606107,-9.47105758716311,-9.29704804786971,-9.08058762674709,
-8.94801017752495,-8.83790843595371,-8.66281179722811,-8.44979106049249,
-8.26875026576761,-8.02350533146686,-7.91386747822455,-7.72464433932807,
-7.45273652713729,-7.27799612001064,-7.05859100547209,-6.92228575466226,
-6.79872465568987,-6.4206733771102,-6.2299195775176,-5.99481772115077,-5.89085098224896,
-5.70306580415755,-5.43654325973892,-5.26211479592577,-5.04399855157591,
-4.90583377233716,-4.78312363312272,-4.40082965711161,-4.20706485434783,
-3.96876887000412,-3.86847375874845,-3.69017410085091,-3.41895959388069,
-3.24427481755454,-3.02508335598879,-2.8884582034516,-2.76461624729456,
-2.3882303819844,-2.19831894215256,-1.96368955992695,-1.85875788984718,
-1.66529088291307,-1.403256505249,-1.22966469894533,-1.01422844467065,-0.880428165090804,
-0.769524651617117,-0.411353224294561,-0.250713762539928,-2.85710713469914E-5),
 .UNSPECIFIED.) ;
#307 = B_SPLINE_CURVE_WITH_KNOTS('',3,(#47368,#47369,#47370,#47371,#47372,
#47373,#47374,#47375,#47376,#47377,#47378,#47379,#47380,#47381,#47382,#47383,
#47384,#47385,#47386,#47387,#47388,#47389,#47390,#47391,#47392,#47393,#47394,
#47395,#47396,#47397,#47398,#47399,#47400,#47401,#47402,#47403,#47404,#47405,
#47406,#47407,#47408,#47409,#47410,#47411,#47412,#47413,#47414,#47415,#47416,
#47417,#47418,#47419,#47420,#47421,#47422,#47423,#47424,#47425,#47426,#47427,
#47428,#47429,#47430,#47431,#47432,#47433,#47434,#47435,#47436,#47437,#47438,
#47439,#47440,#47441,#47442,#47443,#47444,#47445,#47446,#47447,#47448,#47449,
#47450,#47451,#47452,#47453,#47454,#47455,#47456,#47457),.UNSPECIFIED.,
 .F.,.F.,(4,2,2,2,2,2,2,2,2,2,2,2,2,2,2,2,2,2,2,2,2,2,2,2,2,2,2,2,2,2,2,
2,2,2,2,2,2,2,2,2,2,2,2,2,4),(-80.5199172564641,-80.1644944208614,-80.0041939643627,
-79.6847223829998,-79.5240762293956,-79.4233443519087,-79.1836115690117,
-78.9943596077749,-78.65284703493,-78.5470907958417,-78.4516464435982,-78.2020394547879,
-77.9993526461617,-77.8038656449858,-77.6033858547518,-77.4865313444434,
-77.3320976775467,-77.1260689513558,-76.9553817713464,-76.6803092179975,
-76.49669658309,-76.385784272223,-76.150948460969,-75.9660559062757,-75.753224074914,
-75.575790872784,-75.4649445913754,-75.3309730714214,-75.1156319162072,
-74.9420481818352,-74.7355520721864,-74.5645322172805,-74.4555737217011,
-74.3216560757955,-74.1061821600071,-73.9323706298221,-73.7296741777522,
-73.5568647574461,-73.4473510989502,-73.3126234791358,-73.0977447422244,
-72.9241171079032,-72.7216571734284,-72.548688145428,-72.5408068653678),
 .UNSPECIFIED.) ;
#308 = B_SPLINE_CURVE_WITH_KNOTS('',3,(#47460,#47461,#47462,#47463,#47464,
#47465,#47466,#47467,#47468,#47469,#47470,#47471,#47472,#47473,#47474,#47475,
#47476,#47477,#47478,#47479,#47480,#47481,#47482,#47483,#47484,#47485,#47486,
#47487,#47488,#47489,#47490,#47491,#47492,#47493,#47494,#47495,#47496,#47497,
#47498,#47499),.UNSPECIFIED.,.F.,.F.,(4,3,3,3,3,3,3,3,3,3,3,3,3,4),(38.8091570539889,
38.8694027977159,38.9296461683401,38.989896014336,39.0501473311069,39.1104107652207,
39.1514960580706,39.2116081997616,39.27171086176,39.3318070729702,39.3936353160341,
39.4537320202377,39.5164260327317,39.5791200452257),.UNSPECIFIED.) ;
#309 = B_SPLINE_CURVE_WITH_KNOTS('',3,(#47503,#47504,#47505,#47506,#47507,
#47508,#47509,#47510,#47511,#47512,#47513,#47514,#47515,#47516,#47517,#47518,
#47519,#47520,#47521,#47522,#47523,#47524,#47525,#47526,#47527,#47528,#47529,
#47530,#47531,#47532,#47533,#47534,#47535,#47536,#47537,#47538,#47539,#47540,
#47541,#47542,#47543,#47544,#47545,#47546,#47547,#47548,#47549,#47550,#47551,
#47552,#47553,#47554,#47555,#47556,#47557,#47558,#47559,#47560,#47561,#47562,
#47563,#47564,#47565,#47566,#47567,#47568,#47569,#47570,#47571,#47572,#47573,
#47574,#47575,#47576,#47577,#47578,#47579,#47580,#47581,#47582,#47583,#47584,
#47585,#47586,#47587,#47588,#47589,#47590,#47591,#47592,#47593,#47594,#47595,
#47596,#47597,#47598,#47599,#47600,#47601,#47602,#47603,#47604,#47605,#47606,
#47607,#47608,#47609,#47610,#47611,#47612,#47613,#47614,#47615,#47616,#47617,
#47618,#47619,#47620,#47621,#47622,#47623,#47624,#47625,#47626,#47627,#47628,
#47629,#47630,#47631,#47632,#47633,#47634,#47635,#47636,#47637,#47638,#47639,
#47640,#47641,#47642,#47643,#47644,#47645,#47646,#47647,#47648,#47649,#47650,
#47651,#47652,#47653,#47654,#47655,#47656,#47657,#47658,#47659,#47660,#47661,
#47662,#47663,#47664,#47665,#47666,#47667,#47668,#47669,#47670,#47671,#47672,
#47673,#47674,#47675,#47676,#47677,#47678,#47679,#47680,#47681,#47682,#47683,
#47684,#47685,#47686,#47687,#47688,#47689,#47690,#47691,#47692,#47693,#47694,
#47695,#47696,#47697,#47698,#47699,#47700,#47701,#47702,#47703,#47704,#47705,
#47706,#47707,#47708,#47709,#47710,#47711,#47712,#47713,#47714,#47715,#47716,
#47717,#47718,#47719,#47720,#47721,#47722,#47723,#47724,#47725,#47726,#47727,
#47728,#47729,#47730,#47731,#47732,#47733,#47734,#47735,#47736,#47737,#47738,
#47739,#47740,#47741,#47742,#47743,#47744,#47745,#47746,#47747,#47748,#47749,
#47750,#47751,#47752,#47753,#47754,#47755,#47756,#47757,#47758,#47759,#47760,
#47761,#47762,#47763,#47764,#47765,#47766,#47767,#47768,#47769,#47770,#47771,
#47772,#47773,#47774,#47775,#47776,#47777,#47778,#47779,#47780,#47781,#47782,
#47783,#47784,#47785,#47786,#47787,#47788,#47789,#47790,#47791,#47792,#47793,
#47794,#47795,#47796,#47797,#47798,#47799,#47800,#47801,#47802,#47803,#47804,
#47805,#47806,#47807,#47808,#47809,#47810,#47811,#47812,#47813,#47814,#47815,
#47816,#47817,#47818,#47819,#47820,#47821,#47822,#47823,#47824,#47825,#47826,
#47827,#47828,#47829,#47830,#47831,#47832,#47833,#47834,#47835,#47836,#47837,
#47838,#47839,#47840,#47841,#47842,#47843,#47844,#47845,#47846,#47847,#47848,
#47849,#47850,#47851,#47852,#47853,#47854,#47855,#47856,#47857,#47858,#47859,
#47860,#47861,#47862,#47863,#47864,#47865,#47866,#47867,#47868,#47869,#47870,
#47871,#47872,#47873,#47874,#47875,#47876),.UNSPECIFIED.,.F.,.F.,(4,2,2,
2,2,2,2,2,2,2,2,2,2,2,2,2,2,2,2,2,2,2,2,2,2,2,2,2,2,2,2,2,2,2,2,2,2,2,2,
2,2,2,2,2,2,2,2,2,2,2,2,2,2,2,2,2,2,2,2,2,2,2,2,2,2,2,2,2,2,2,2,2,2,2,2,
2,2,2,2,2,2,2,2,2,2,2,2,2,2,2,2,2,2,2,2,2,2,2,2,2,2,2,2,2,2,2,2,2,2,2,2,
2,2,2,2,2,2,2,2,2,2,2,2,2,2,2,2,2,2,2,2,2,2,2,2,2,2,2,2,2,2,2,2,2,2,2,2,
2,2,2,2,2,2,2,2,2,2,2,2,2,2,2,2,2,2,2,2,2,2,2,2,2,2,2,2,2,2,2,2,2,2,2,2,
2,2,2,4),(12.2072423730149,12.2352191971208,12.2826569185805,12.3199218461975,
12.3632367703069,12.4476936178893,12.570959081202,12.736960751213,12.7712185243792,
12.7899046594911,12.8110958594259,12.8477758062442,12.9775498472711,13.186850273024,
13.2414042611081,13.2791719333704,13.3191621616987,13.3843445062427,13.4283106072689,
13.571818250311,13.703077921244,13.7390148797864,13.7579955084812,13.7788333307434,
13.8137096799704,13.9274501747456,14.1649810223736,14.2107354896485,14.2484923886513,
14.2885024925577,14.3537950693201,14.3978697781285,14.5420032459383,14.6763405085586,
14.7101190497473,14.7287234735031,14.7500338458174,14.7873103976802,14.8364313854618,
14.9720349776009,14.9951544653213,15.1331017759202,15.1792500957851,15.2170924865626,
15.2569504404925,15.3213987389577,15.3646448623818,15.504077960292,15.5393575172787,
15.6436449362394,15.6784198201109,15.6971953543804,15.7182674144656,15.7543468588177,
15.8785479367335,16.0957546475812,16.1497574669088,16.1874404271184,16.2275915897599,
16.2936677418344,16.3385182845485,16.4872119182997,16.5225488814497,16.6229804370995,
16.6526714130605,16.6726354756428,16.6963210792083,16.7464171669615,16.7864055409356,
16.962630390052,16.9924079593312,17.088306000914,17.1333446489689,17.1705248555486,
17.2158728626694,17.3139913778747,17.4768169480921,17.5819524092582,17.6167855591192,
17.6355711590667,17.6566292337011,17.6926408650967,17.8162330412686,18.0343992755267,
18.0883065109779,18.1259740276626,18.1661521329659,18.2323828326118,18.2773877277253,
18.4270102994341,18.4414035791782,18.4691306508678,18.5619445513156,18.5913834403182,
18.6113154546221,18.6351376173856,18.6860428603105,18.8442137203142,19.0099584586975,
19.0560936002452,19.093934576838,19.1338008765076,19.1982873848837,19.2415700475714,
19.3812049082807,19.4103466456513,19.4394988404435,19.5313524466272,19.5606807983543,
19.5805980985628,19.6044755801851,19.6557311127837,19.8144735380744,19.9772665517165,
20.0241117669603,20.0621065620635,20.10170899509,20.164753729605,20.206640131746,
20.3387062130429,20.3770288819941,20.4046552093695,20.4998778235861,20.5295201131088,
20.5494768264847,20.5731859404254,20.623421447614,20.6635769726289,20.8413927447492,
20.9555215426404,21.0034034723294,21.0407764988915,21.0832855070926,21.1628107718385,
21.347842788525,21.3712421860454,21.4688546884355,21.4986088990629,21.5185848426185,
21.5422513859962,21.5922080050725,21.6320278687749,21.8067026296436,21.8713843789855,
21.9449867583524,21.9868524349962,22.024353265849,22.0742603937447,22.2173877193162,
22.3441788131783,22.4383303184236,22.4678730112234,22.4878055784151,22.5115165527441,
22.561887359572,22.7206260368362,22.8857575036312,22.9324261795403,22.970362556157,
23.0028103026188,23.0530709333166,23.1155220944091,23.2491008063794,23.395836497707,
23.4315490522561,23.4504940804626,23.4704160773139,23.4722676083633,23.4741530752907,
23.4761135314339,23.4781910345803,23.4804314105348,23.4828868373316,23.4836044905581,
23.484530463745,23.4857418875848,23.4873529350992,23.4895365131139,23.5211848320784,
23.5827324207832,23.8242118109602,23.8900513082125,23.9302202891897,23.965754532381,
24.0033012563355,24.0582608056696,24.2611810843085),.UNSPECIFIED.) ;
#310 = B_SPLINE_CURVE_WITH_KNOTS('',3,(#47879,#47880,#47881,#47882,#47883,
#47884,#47885,#47886,#47887,#47888,#47889,#47890,#47891,#47892,#47893,#47894,
#47895,#47896,#47897,#47898,#47899,#47900,#47901,#47902,#47903,#47904,#47905,
#47906,#47907,#47908,#47909,#47910,#47911,#47912,#47913,#47914,#47915,#47916,
#47917,#47918,#47919,#47920,#47921,#47922,#47923,#47924,#47925,#47926,#47927,
#47928,#47929,#47930,#47931,#47932,#47933,#47934,#47935,#47936,#47937,#47938,
#47939,#47940,#47941,#47942,#47943,#47944,#47945,#47946,#47947,#47948,#47949,
#47950,#47951,#47952,#47953,#47954,#47955,#47956,#47957,#47958,#47959,#47960,
#47961,#47962,#47963,#47964,#47965,#47966,#47967,#47968,#47969,#47970,#47971,
#47972,#47973,#47974,#47975,#47976,#47977,#47978,#47979,#47980,#47981,#47982,
#47983,#47984,#47985,#47986,#47987,#47988,#47989,#47990,#47991,#47992,#47993,
#47994,#47995,#47996,#47997,#47998,#47999,#48000,#48001,#48002,#48003,#48004,
#48005,#48006,#48007,#48008,#48009,#48010,#48011,#48012,#48013,#48014,#48015,
#48016,#48017,#48018,#48019,#48020,#48021,#48022,#48023,#48024,#48025,#48026,
#48027,#48028,#48029,#48030,#48031,#48032,#48033,#48034,#48035,#48036,#48037,
#48038,#48039,#48040,#48041,#48042,#48043,#48044,#48045,#48046,#48047,#48048,
#48049,#48050,#48051,#48052,#48053,#48054,#48055,#48056,#48057,#48058,#48059,
#48060,#48061,#48062,#48063,#48064,#48065,#48066,#48067,#48068,#48069,#48070,
#48071,#48072,#48073,#48074,#48075,#48076,#48077,#48078,#48079,#48080,#48081,
#48082,#48083,#48084,#48085,#48086,#48087,#48088,#48089,#48090,#48091,#48092,
#48093,#48094,#48095,#48096,#48097,#48098,#48099,#48100,#48101,#48102,#48103,
#48104,#48105,#48106,#48107,#48108,#48109,#48110,#48111,#48112,#48113,#48114,
#48115,#48116,#48117,#48118,#48119,#48120,#48121,#48122,#48123,#48124,#48125,
#48126,#48127,#48128,#48129,#48130,#48131,#48132,#48133,#48134,#48135,#48136,
#48137),.UNSPECIFIED.,.F.,.F.,(4,3,3,3,3,3,3,3,3,3,3,3,3,3,3,3,3,3,3,3,
3,3,3,3,3,3,3,3,3,3,3,3,3,3,3,3,3,3,3,3,3,3,3,3,3,3,3,3,3,3,3,3,3,3,3,3,
3,3,3,3,3,3,3,3,3,3,3,3,3,3,3,3,3,3,3,3,3,3,3,3,3,3,3,3,3,3,4),(-84.8061323363251,
-84.7434695854549,-84.6808110755322,-84.6181547160668,-84.5554984169936,
-84.4928322445765,-84.4301641985852,-84.3674819098806,-84.3072727343469,
-84.2449152840996,-84.1827586433676,-84.1206101572369,-84.0584666053991,
-83.9959532371414,-83.9338046160016,-83.8711088741851,-83.8084131323685,
-83.7460214897466,-83.6836387031221,-83.6212620261393,-83.5588887142844,
-83.4965090091967,-83.4341289979585,-83.3717356186068,-83.3095535303901,
-83.2471960801428,-83.1849129227894,-83.1226366457664,-83.0603642914639,
-82.9979467007009,-82.9356680248854,-82.8731809766486,-82.8106939284118,
-82.7483364781645,-82.6860202553423,-82.6237106902526,-82.5614048951035,
-82.499012252936,-82.4367000854348,-82.3742672059341,-82.3118343264334,
-82.2494768761861,-82.1871654863429,-82.1248607634951,-82.062559809642,
-82.0001635383452,-81.9378561629617,-81.8754154437083,-81.812974724455,
-81.7506172742077,-81.6883094565925,-81.6260083494707,-81.5637110472351,
-81.5013120660455,-81.4390083946495,-81.376561758563,-81.3141151224766,
-81.2517576722293,-81.189445700161,-81.1271403995358,-81.0648388735713,
-81.002443035303,-80.9401351071849,-80.8776953138415,-80.8152555204982,
-80.7528980702509,-80.6905887871496,-80.628286198462,-80.5659874016961,
-80.503589530902,-80.4412843477519,-80.3788401331359,-80.3163959185198,
-80.2540384682725,-80.1917278738116,-80.1294239633962,-80.0671238373162,
-80.0047269571225,-79.9424204389808,-79.8799783777611,-79.8175363165415,
-79.7551789658218,-79.6928320409426,-79.6304912444782,-79.5681557198953,
-79.5058202388051,-79.4912145662646),.UNSPECIFIED.) ;
#311 = B_SPLINE_CURVE_WITH_KNOTS('',3,(#48179,#48180,#48181,#48182,#48183,
#48184,#48185,#48186,#48187,#48188,#48189,#48190,#48191,#48192,#48193,#48194,
#48195,#48196),.UNSPECIFIED.,.F.,.F.,(4,2,2,2,2,2,2,2,4),(-3.02737420106107,
-2.83815008504339,-2.64892596902571,-2.45972830991075,-2.2705306507958,
-2.08133299168085,-1.8921353325659,-1.70291121654822,-1.51368710053054),
 .UNSPECIFIED.) ;
#312 = B_SPLINE_CURVE_WITH_KNOTS('',3,(#48199,#48200,#48201,#48202,#48203,
#48204,#48205,#48206,#48207,#48208,#48209,#48210,#48211,#48212,#48213,#48214,
#48215,#48216),.UNSPECIFIED.,.F.,.F.,(4,2,2,2,2,2,2,2,4),(-1.51368710053053,
-1.32446298451285,-1.13523886849517,-0.946041209380219,-0.756843550265268,
-0.567645891150316,-0.378448232035365,-0.189224116017682,0.),
 .UNSPECIFIED.) ;
#313 = B_SPLINE_CURVE_WITH_KNOTS('',3,(#48271,#48272,#48273,#48274,#48275,
#48276,#48277,#48278,#48279,#48280,#48281,#48282,#48283,#48284),
 .UNSPECIFIED.,.F.,.F.,(4,2,2,2,2,2,4),(-2.86271597092642,-2.47550138268059,
-2.09247759219639,-1.63307121855681,-1.1818186467659,-0.689259812314864,
-1.00000004810141E-6),.UNSPECIFIED.) ;
#314 = B_SPLINE_CURVE_WITH_KNOTS('',3,(#48285,#48286,#48287,#48288,#48289,
#48290,#48291,#48292,#48293,#48294,#48295,#48296,#48297,#48298,#48299,#48300,
#48301,#48302,#48303,#48304,#48305,#48306,#48307,#48308,#48309,#48310,#48311,
#48312,#48313,#48314,#48315,#48316,#48317,#48318,#48319,#48320,#48321,#48322,
#48323,#48324,#48325,#48326,#48327,#48328,#48329,#48330,#48331,#48332,#48333,
#48334,#48335,#48336,#48337,#48338,#48339,#48340,#48341,#48342,#48343,#48344,
#48345,#48346,#48347,#48348,#48349,#48350,#48351,#48352,#48353,#48354,#48355,
#48356,#48357,#48358,#48359,#48360,#48361,#48362,#48363,#48364,#48365,#48366,
#48367,#48368,#48369,#48370,#48371,#48372,#48373,#48374,#48375,#48376,#48377,
#48378,#48379,#48380,#48381,#48382,#48383,#48384,#48385,#48386,#48387,#48388,
#48389,#48390,#48391,#48392,#48393,#48394,#48395,#48396,#48397,#48398,#48399,
#48400,#48401,#48402,#48403,#48404,#48405,#48406,#48407,#48408,#48409,#48410,
#48411,#48412,#48413,#48414),.UNSPECIFIED.,.F.,.F.,(4,3,3,3,3,3,3,3,3,3,
3,3,3,3,3,3,3,3,3,3,3,3,3,3,3,3,3,3,3,3,3,3,3,3,3,3,3,3,3,3,3,3,3,4),(0.,
0.134956132691862,0.150548210071358,0.284576496872476,0.42651189256128,
0.561684253595667,0.696272635973996,0.82933537653257,0.852318079627691,
0.867571174403126,1.00107306380577,1.13432953696973,1.23838937708017,1.37208338021623,
1.50558528557567,1.60554221520874,1.69300452863768,1.71195887004486,1.8435302488514,
1.97562049759594,2.10733784413285,2.23767920145199,2.30524072264026,2.43707975007448,
2.52155729666941,2.54226292029336,2.67187769228001,2.80231319807097,2.93934656128157,
3.06892063981614,3.19735578614655,3.32372079372745,3.35044665091336,3.38443065417707,
3.51315247311986,3.64233608971587,3.75232450310687,3.82177124080331,3.86231291649787,
3.87975886711596,4.00788164525527,4.13559019490866,4.26173696563685,4.37270046381608),
 .UNSPECIFIED.) ;
#315 = B_SPLINE_CURVE_WITH_KNOTS('',3,(#48430,#48431,#48432,#48433,#48434,
#48435,#48436,#48437,#48438,#48439,#48440,#48441,#48442,#48443,#48444,#48445,
#48446,#48447,#48448,#48449,#48450,#48451,#48452,#48453,#48454,#48455,#48456,
#48457,#48458,#48459,#48460,#48461,#48462,#48463),.UNSPECIFIED.,.T.,.F.,
(4,2,2,2,2,2,2,2,2,2,2,2,2,2,2,2,4),(0.,0.131943994423176,0.263887988846351,
0.395831447701094,0.527774906555838,0.659718365410582,0.791661824265325,
0.9236058186885,1.05554981311168,1.18749380753485,1.31943780195803,1.45138126081277,
1.58332471966751,1.71526817852226,1.847211637377,1.97915563180018,2.11109962622335),
 .UNSPECIFIED.) ;
#316 = B_SPLINE_CURVE_WITH_KNOTS('',3,(#48465,#48466,#48467,#48468,#48469,
#48470,#48471,#48472,#48473,#48474,#48475,#48476,#48477,#48478,#48479,#48480,
#48481,#48482,#48483,#48484,#48485,#48486,#48487,#48488,#48489,#48490,#48491,
#48492,#48493,#48494,#48495,#48496,#48497,#48498),.UNSPECIFIED.,.T.,.F.,
(4,2,2,2,2,2,2,2,2,2,2,2,2,2,2,2,4),(0.,0.131943994423175,0.263887988846351,
0.395831447701094,0.527774906555838,0.659718365410582,0.791661824265325,
0.923605818688501,1.05554981311168,1.18749380753485,1.31943780195803,1.45138126081277,
1.58332471966751,1.71526817852226,1.847211637377,1.97915563180018,2.11109962622335),
 .UNSPECIFIED.) ;
#317 = B_SPLINE_CURVE_WITH_KNOTS('',3,(#48500,#48501,#48502,#48503,#48504,
#48505,#48506,#48507,#48508,#48509,#48510,#48511,#48512,#48513,#48514,#48515,
#48516,#48517,#48518,#48519,#48520,#48521,#48522,#48523,#48524,#48525,#48526,
#48527,#48528,#48529,#48530,#48531,#48532,#48533),.UNSPECIFIED.,.T.,.F.,
(4,2,2,2,2,2,2,2,2,2,2,2,2,2,2,2,4),(0.,0.131943994423175,0.26388798884635,
0.395831447701094,0.527774906555837,0.659718365410581,0.791661824265324,
0.9236058186885,1.05554981311168,1.18749380753485,1.31943780195803,1.45138126081277,
1.58332471966751,1.71526817852226,1.847211637377,1.97915563180018,2.11109962622335),
 .UNSPECIFIED.) ;
#318 = B_SPLINE_CURVE_WITH_KNOTS('',1,(#48613,#48614),.UNSPECIFIED.,.F.,.F.,
(2,2),(0.,1.00000015726815),.UNSPECIFIED.) ;
#319 = B_SPLINE_CURVE_WITH_KNOTS('',3,(#48615,#48616,#48617,#48618,#48619,
#48620,#48621,#48622,#48623,#48624,#48625,#48626,#48627,#48628,#48629,#48630,
#48631,#48632,#48633,#48634,#48635,#48636,#48637,#48638,#48639,#48640,#48641,
#48642,#48643,#48644,#48645,#48646,#48647,#48648,#48649,#48650,#48651,#48652,
#48653,#48654,#48655,#48656,#48657,#48658,#48659,#48660,#48661,#48662,#48663,
#48664,#48665,#48666,#48667,#48668,#48669),.UNSPECIFIED.,.T.,.F.,(4,2,2,
2,2,2,2,2,2,2,2,3,2,2,2,2,2,2,2,2,2,2,2,2,2,2,4),(0.630282646728311,0.638093074049646,
0.647002723099591,0.666366138141934,0.696779929267916,0.740656076798668,
0.804443699294602,0.892545576433704,1.02104051551844,1.06836668156106,1.13376734398064,
1.19519452402957,1.25836937632244,1.38453630464938,1.44224028136641,1.49447273220586,
1.54567596360975,1.59097946229049,1.63573830290034,1.67109818487044,1.70152973349188,
1.72897522297272,1.75594681875993,1.77754167411064,1.80981305883969,1.82286183962224,
1.82547717075788),.UNSPECIFIED.) ;
#320 = B_SPLINE_CURVE_WITH_KNOTS('',1,(#48740,#48741),.UNSPECIFIED.,.F.,.F.,
(2,2),(0.,1.00000015726814),.UNSPECIFIED.) ;
#321 = B_SPLINE_CURVE_WITH_KNOTS('',3,(#48742,#48743,#48744,#48745,#48746,
#48747,#48748,#48749,#48750,#48751,#48752,#48753,#48754,#48755,#48756,#48757,
#48758,#48759,#48760,#48761,#48762,#48763,#48764,#48765,#48766,#48767,#48768,
#48769,#48770,#48771,#48772,#48773,#48774,#48775,#48776,#48777,#48778,#48779,
#48780,#48781,#48782,#48783,#48784,#48785,#48786,#48787,#48788,#48789,#48790,
#48791,#48792,#48793,#48794,#48795,#48796),.UNSPECIFIED.,.T.,.F.,(4,2,2,
2,2,2,2,2,2,2,2,3,2,2,2,2,2,2,2,2,2,2,2,2,2,2,4),(0.630282646727731,0.638093074049046,
0.647002723098976,0.666366138141306,0.696779929267319,0.74065607679813,
0.804443699294194,0.892545576433443,1.02104051551834,1.06836668156095,1.13376734398052,
1.19519452402944,1.25836937632229,1.38453630464921,1.44224028136624,1.49447273220568,
1.54567596360952,1.59097946229014,1.63573830289993,1.67109818486996,1.70152973349133,
1.72897522297213,1.7559468187593,1.77754167410999,1.80981305883899,1.82286183962152,
1.82547717075717),.UNSPECIFIED.) ;
#322 = B_SPLINE_CURVE_WITH_KNOTS('',1,(#48867,#48868),.UNSPECIFIED.,.F.,.F.,
(2,2),(0.,1.00000015726815),.UNSPECIFIED.) ;
#323 = B_SPLINE_CURVE_WITH_KNOTS('',3,(#48869,#48870,#48871,#48872,#48873,
#48874,#48875,#48876,#48877,#48878,#48879,#48880,#48881,#48882,#48883,#48884,
#48885,#48886,#48887,#48888,#48889,#48890,#48891,#48892,#48893,#48894,#48895,
#48896,#48897,#48898,#48899,#48900,#48901,#48902,#48903,#48904,#48905,#48906,
#48907,#48908,#48909,#48910,#48911,#48912,#48913,#48914,#48915,#48916,#48917,
#48918,#48919,#48920,#48921,#48922,#48923),.UNSPECIFIED.,.T.,.F.,(4,2,2,
2,2,2,2,2,2,2,2,3,2,2,2,2,2,2,2,2,2,2,2,2,2,2,4),(0.630282646727811,0.638093074049133,
0.647002723099068,0.66636613814141,0.696779929267413,0.740656076798171,
0.804443699294128,0.892545576433259,1.02104051551798,1.06836668156057,1.13376734398012,
1.19519452402904,1.25836937632187,1.38453630464876,1.44224028136575,1.49447273220515,
1.545675963609,1.5909794622897,1.63573830289951,1.67109818486956,1.70152973349097,
1.72897522297177,1.75594681875897,1.77754167410966,1.80981305883867,1.82286183962121,
1.82547717075685),.UNSPECIFIED.) ;
#324 = B_SPLINE_CURVE_WITH_KNOTS('',3,(#49617,#49618,#49619,#49620,#49621,
#49622,#49623,#49624,#49625,#49626,#49627,#49628,#49629,#49630,#49631,#49632,
#49633,#49634,#49635,#49636,#49637,#49638,#49639,#49640,#49641,#49642,#49643,
#49644,#49645,#49646,#49647,#49648,#49649,#49650,#49651,#49652,#49653,#49654,
#49655,#49656,#49657,#49658,#49659,#49660,#49661,#49662,#49663,#49664,#49665,
#49666,#49667,#49668,#49669,#49670,#49671,#49672,#49673,#49674,#49675,#49676,
#49677,#49678,#49679,#49680,#49681,#49682,#49683,#49684,#49685,#49686,#49687,
#49688,#49689,#49690,#49691,#49692,#49693,#49694,#49695,#49696,#49697,#49698,
#49699,#49700,#49701,#49702,#49703,#49704,#49705,#49706,#49707,#49708,#49709,
#49710,#49711,#49712,#49713,#49714,#49715,#49716,#49717,#49718,#49719,#49720,
#49721,#49722,#49723,#49724,#49725,#49726,#49727,#49728,#49729,#49730,#49731,
#49732,#49733,#49734,#49735,#49736,#49737,#49738,#49739,#49740,#49741,#49742,
#49743,#49744,#49745,#49746,#49747,#49748,#49749,#49750,#49751,#49752),
 .UNSPECIFIED.,.F.,.F.,(4,3,3,3,3,3,3,3,3,3,3,3,3,3,3,3,3,3,3,3,3,3,3,3,
3,3,3,3,3,3,3,3,3,3,3,3,3,3,3,3,3,3,3,3,3,4),(2.18408295184663E-6,0.123020428160983,
0.15963065273004,0.281586707028109,0.404758111867876,0.527955343315918,
0.650212475416643,0.73717114933423,0.753380162546799,0.767542900869677,
0.772752757916178,0.895020990109926,1.01719177953705,1.12547299608439,1.2478361314004,
1.37486418901594,1.50189224663149,1.51295714877596,1.63388146162191,1.75558436713017,
1.8770599821172,1.99728332804384,2.08122088405351,2.1937412593632,2.22090947074412,
2.24234748900313,2.25711688775144,2.31417322948663,2.43433900312252,2.55521631537028,
2.67592273084785,2.79589111461474,2.91402806997879,2.98138388653104,2.99369222579519,
3.02628757255141,3.14563906826117,3.26562493318584,3.38565980391277,3.45762068722671,
3.4747197256305,3.48565352718463,3.60526986962867,3.72467353676032,3.84274714773479,
3.95993145615853),.UNSPECIFIED.) ;
#325 = B_SPLINE_CURVE_WITH_KNOTS('',3,(#49754,#49755,#49756,#49757,#49758,
#49759,#49760,#49761,#49762,#49763,#49764,#49765,#49766,#49767,#49768,#49769,
#49770,#49771,#49772,#49773,#49774,#49775,#49776,#49777,#49778,#49779,#49780,
#49781,#49782,#49783,#49784,#49785,#49786,#49787,#49788,#49789,#49790,#49791,
#49792,#49793,#49794,#49795,#49796,#49797,#49798,#49799,#49800,#49801,#49802,
#49803,#49804,#49805,#49806,#49807,#49808,#49809,#49810,#49811,#49812,#49813,
#49814,#49815,#49816,#49817,#49818,#49819,#49820,#49821,#49822,#49823,#49824,
#49825,#49826,#49827,#49828,#49829,#49830,#49831,#49832,#49833,#49834,#49835,
#49836,#49837,#49838,#49839,#49840,#49841,#49842,#49843,#49844,#49845,#49846,
#49847,#49848,#49849,#49850,#49851,#49852,#49853,#49854,#49855,#49856,#49857,
#49858,#49859,#49860,#49861,#49862,#49863,#49864,#49865,#49866,#49867,#49868,
#49869,#49870,#49871,#49872,#49873,#49874,#49875,#49876,#49877,#49878,#49879,
#49880,#49881,#49882,#49883,#49884,#49885,#49886,#49887,#49888,#49889,#49890,
#49891,#49892),.UNSPECIFIED.,.F.,.F.,(4,3,3,3,3,3,3,3,3,3,3,3,3,3,3,3,3,
3,3,3,3,3,3,3,3,3,3,3,3,3,3,3,3,3,3,3,3,3,3,3,3,3,3,3,3,3,4),(0.,0.119588194315636,
0.152837981974594,0.271317579881898,0.390765157706876,0.510593513266912,
0.630145691521126,0.687516409369078,0.712777341230908,0.729146013580884,
0.746103307941794,0.866247064092426,0.986797445428536,1.08911143430474,
1.20940114144625,1.32989963245365,1.41810059920495,1.44370363426542,1.46133334350923,
1.47491872658128,1.59493286517016,1.71620190524513,1.83753914921351,1.9580232347556,
2.03550736646401,2.15666423324517,2.18484158143669,2.20157601869575,2.21395295588132,
2.33405734051309,2.45539974153245,2.57743148373137,2.69927308058649,2.82035616630182,
2.90588765281033,2.94463079271265,2.95935015045668,2.99141913931883,3.11252755730056,
3.23451829514276,3.35702313311209,3.44804384530054,3.4621411140443,3.58565221622721,
3.70869195186839,3.83243873732217,3.95618552277594),.UNSPECIFIED.) ;
#326 = B_SPLINE_CURVE_WITH_KNOTS('',3,(#49893,#49894,#49895,#49896),
 .UNSPECIFIED.,.F.,.F.,(4,4),(-0.00157738977958374,0.),.UNSPECIFIED.) ;
#327 = B_SPLINE_CURVE_WITH_KNOTS('',3,(#50590,#50591,#50592,#50593,#50594,
#50595,#50596,#50597,#50598,#50599,#50600,#50601,#50602,#50603,#50604,#50605,
#50606,#50607,#50608,#50609,#50610,#50611,#50612,#50613,#50614,#50615,#50616,
#50617,#50618,#50619,#50620,#50621,#50622,#50623,#50624,#50625,#50626,#50627,
#50628,#50629,#50630,#50631,#50632,#50633,#50634,#50635,#50636,#50637,#50638,
#50639,#50640,#50641,#50642,#50643,#50644,#50645,#50646,#50647,#50648,#50649,
#50650,#50651,#50652,#50653,#50654,#50655,#50656,#50657,#50658,#50659,#50660,
#50661,#50662,#50663,#50664,#50665,#50666,#50667,#50668,#50669,#50670,#50671,
#50672,#50673,#50674,#50675,#50676,#50677,#50678,#50679,#50680,#50681,#50682,
#50683,#50684,#50685,#50686,#50687,#50688,#50689,#50690,#50691,#50692,#50693,
#50694,#50695,#50696,#50697,#50698,#50699,#50700,#50701,#50702,#50703,#50704,
#50705,#50706,#50707,#50708,#50709,#50710,#50711,#50712,#50713,#50714,#50715,
#50716,#50717,#50718,#50719,#50720,#50721,#50722,#50723,#50724,#50725),
 .UNSPECIFIED.,.F.,.F.,(4,3,3,3,3,3,3,3,3,3,3,3,3,3,3,3,3,3,3,3,3,3,3,3,
3,3,3,3,3,3,3,3,3,3,3,3,3,3,3,3,3,3,3,3,3,4),(0.,0.119588186287281,0.152837981974752,
0.27074719741009,0.390267991763342,0.510094677789097,0.61965267305727,0.674431670691357,
0.708278729033239,0.729210668325444,0.735267875681489,0.855351785448358,
0.975909365301059,1.08911143430487,1.20925610650812,1.33411169372933,1.45896728095053,
1.47047783077841,1.59044520192017,1.71170224358119,1.8330458276188,1.95355177499451,
2.03550736646409,2.15666422985477,2.18484158150908,2.20157601759723,2.21395295550005,
2.33397535245444,2.45526219673935,2.57760433999465,2.69951082281856,2.82207079628956,
2.94463076976056,2.95773533199481,2.99141913931887,3.11248092205803,3.23444145233754,
3.35694954126384,3.43211505332396,3.45237084951486,3.46204675189966,3.4646398157526,
3.58757479015538,3.7106123337395,3.83339892825768,3.95618552277586),
 .UNSPECIFIED.) ;
#328 = B_SPLINE_CURVE_WITH_KNOTS('',3,(#50726,#50727,#50728,#50729),
 .UNSPECIFIED.,.F.,.F.,(4,4),(0.,0.00157736468337877),.UNSPECIFIED.) ;
#329 = B_SPLINE_CURVE_WITH_KNOTS('',3,(#50730,#50731,#50732,#50733,#50734,
#50735,#50736,#50737,#50738,#50739,#50740,#50741,#50742,#50743,#50744,#50745,
#50746,#50747,#50748,#50749,#50750,#50751,#50752,#50753,#50754,#50755,#50756,
#50757,#50758,#50759,#50760,#50761,#50762,#50763,#50764,#50765,#50766,#50767,
#50768,#50769,#50770,#50771,#50772,#50773,#50774,#50775,#50776,#50777,#50778,
#50779,#50780,#50781,#50782,#50783,#50784,#50785,#50786,#50787,#50788,#50789,
#50790,#50791,#50792,#50793,#50794,#50795,#50796,#50797,#50798,#50799,#50800,
#50801,#50802,#50803,#50804,#50805,#50806,#50807,#50808,#50809,#50810,#50811,
#50812,#50813,#50814,#50815,#50816,#50817,#50818,#50819,#50820,#50821,#50822,
#50823,#50824,#50825,#50826,#50827,#50828,#50829,#50830,#50831,#50832,#50833,
#50834,#50835,#50836,#50837,#50838,#50839,#50840,#50841,#50842,#50843,#50844,
#50845,#50846,#50847,#50848,#50849,#50850,#50851,#50852,#50853,#50854,#50855,
#50856,#50857,#50858,#50859),.UNSPECIFIED.,.F.,.F.,(4,3,3,3,3,3,3,3,3,3,
3,3,3,3,3,3,3,3,3,3,3,3,3,3,3,3,3,3,3,3,3,3,3,3,3,3,3,3,3,3,3,3,3,4),(0.,
0.123018240977632,0.159630652729786,0.281611310473703,0.404794365344837,
0.527980108221235,0.650146381112849,0.754308226515199,0.766561817559909,
0.888812162564381,1.01099748544193,1.12547299608417,1.24783613177185,1.37486419163187,
1.50189225149189,1.51295715334221,1.63388146506136,1.75558437158114,1.87705998894425,
1.99728334001246,2.08122088405321,2.20269423912377,2.24766412561392,2.25939910057906,
2.37910849227707,2.49977219254656,2.62076457057125,2.74102482887587,2.86028037404055,
2.94328397329584,2.97018145502892,2.98651707444645,3.00353032282715,3.02628757255113,
3.14563905790358,3.26562491787666,3.38565979382963,3.45762067936319,3.48901510291289,
3.55710178412575,3.67664845340404,3.79570446790245,3.91331257842532,3.95993145615846),
 .UNSPECIFIED.) ;
#330 = B_SPLINE_CURVE_WITH_KNOTS('',3,(#51209,#51210,#51211,#51212,#51213,
#51214,#51215,#51216,#51217,#51218,#51219,#51220,#51221,#51222,#51223,#51224,
#51225,#51226,#51227,#51228,#51229,#51230,#51231,#51232,#51233,#51234,#51235,
#51236,#51237,#51238,#51239,#51240,#51241,#51242,#51243,#51244,#51245,#51246,
#51247,#51248,#51249,#51250,#51251,#51252,#51253,#51254,#51255,#51256,#51257,
#51258,#51259,#51260,#51261,#51262,#51263,#51264,#51265,#51266,#51267,#51268,
#51269,#51270,#51271,#51272,#51273,#51274,#51275,#51276,#51277,#51278,#51279,
#51280,#51281,#51282,#51283,#51284,#51285,#51286,#51287,#51288,#51289,#51290,
#51291,#51292,#51293,#51294,#51295,#51296,#51297,#51298,#51299,#51300,#51301,
#51302,#51303,#51304,#51305,#51306,#51307,#51308,#51309,#51310,#51311,#51312,
#51313,#51314,#51315,#51316,#51317,#51318,#51319,#51320,#51321,#51322,#51323,
#51324,#51325,#51326,#51327,#51328,#51329,#51330,#51331,#51332,#51333,#51334,
#51335),.UNSPECIFIED.,.F.,.F.,(4,3,3,3,3,3,3,3,3,3,3,3,3,3,3,3,3,3,3,3,
3,3,3,3,3,3,3,3,3,3,3,3,3,3,3,3,3,3,3,3,3,3,4),(6.28075782615231E-6,0.134962417714373,
0.150548210071363,0.284576510029121,0.4265119018776,0.561684260662624,0.696272643598151,
0.829335384069975,0.852318077423036,0.865259157588972,0.998756784143564,
1.13201928919157,1.2383893770802,1.37204896176997,1.50568859332497,1.63839311050962,
1.69300451064955,1.709972305995,1.84153084943448,1.97362301373667,2.10534945672862,
2.23570269565275,2.30524072264028,2.43707979046566,2.52155729901495,2.53397976802391,
2.66352086058859,2.79392303702358,2.92452377215859,3.05420467689459,3.18278646002985,
3.30927444084533,3.35044665091337,3.38440368336101,3.51310617758439,3.64228386708091,
3.77121409589701,3.85162416869255,3.8665988626213,3.99473725549904,4.12250938678091,
4.2487399621133,4.37270046381604),.UNSPECIFIED.) ;
#331 = B_SPLINE_CURVE_WITH_KNOTS('',3,(#51685,#51686,#51687,#51688,#51689,
#51690,#51691,#51692,#51693,#51694,#51695,#51696,#51697,#51698,#51699,#51700,
#51701,#51702,#51703,#51704,#51705,#51706,#51707,#51708,#51709,#51710,#51711,
#51712,#51713,#51714,#51715,#51716,#51717,#51718,#51719,#51720,#51721,#51722,
#51723,#51724,#51725,#51726,#51727,#51728,#51729,#51730,#51731,#51732,#51733,
#51734,#51735,#51736,#51737,#51738,#51739,#51740,#51741,#51742,#51743,#51744,
#51745,#51746,#51747,#51748,#51749,#51750,#51751,#51752,#51753,#51754,#51755,
#51756,#51757,#51758,#51759,#51760,#51761,#51762,#51763,#51764,#51765,#51766,
#51767,#51768,#51769,#51770,#51771,#51772,#51773,#51774,#51775,#51776,#51777,
#51778,#51779,#51780,#51781,#51782,#51783,#51784,#51785,#51786,#51787,#51788,
#51789,#51790,#51791,#51792,#51793,#51794,#51795,#51796,#51797,#51798,#51799,
#51800,#51801,#51802,#51803,#51804,#51805,#51806,#51807,#51808,#51809,#51810,
#51811,#51812,#51813,#51814),.UNSPECIFIED.,.F.,.F.,(4,3,3,3,3,3,3,3,3,3,
3,3,3,3,3,3,3,3,3,3,3,3,3,3,3,3,3,3,3,3,3,3,3,3,3,3,3,3,3,3,3,3,3,4),(0.,
0.127950841635321,0.138734436835898,0.266927318078744,0.39452245359627,
0.522788716549364,0.651083437735894,0.779381949996588,0.799252792649835,
0.815195110372998,0.944426122570075,1.07435921574577,1.16427748677867,1.29343658906208,
1.42315651822206,1.55284275525532,1.60917412077767,1.62373987619339,1.7535153835574,
1.88480435100334,2.01633375694167,2.14727531103612,2.21103030364097,2.34228118872861,
2.43432232649351,2.44667434785096,2.57724334887867,2.70921236615828,2.84205677072627,
2.97499463641324,3.1073063974138,3.237949250727,3.27831317758158,3.29127088822594,
3.4254816777589,3.55892260811963,3.69298599227836,3.77698239380477,3.8058365140531,
3.83035997939428,3.96532060706772,4.10051008302849,4.23496370739636,4.36495720448964),
 .UNSPECIFIED.) ;
#332 = B_SPLINE_CURVE_WITH_KNOTS('',3,(#51815,#51816,#51817,#51818),
 .UNSPECIFIED.,.F.,.F.,(4,4),(0.,0.00110748569343258),.UNSPECIFIED.) ;
#333 = B_SPLINE_CURVE_WITH_KNOTS('',3,(#53886,#53887,#53888,#53889,#53890,
#53891,#53892,#53893,#53894,#53895,#53896,#53897,#53898,#53899,#53900,#53901,
#53902,#53903,#53904,#53905,#53906,#53907,#53908,#53909,#53910,#53911,#53912,
#53913,#53914,#53915,#53916,#53917,#53918,#53919,#53920,#53921,#53922,#53923,
#53924,#53925),.UNSPECIFIED.,.F.,.F.,(4,3,3,3,3,3,3,3,3,3,3,3,3,4),(1.39920553665769,
1.60174184009255,1.6712576734102,1.86788901812265,2.06612241242195,2.22834356454693,
2.4268269574145,2.62368336398366,2.78544130230508,2.98797174735918,3.19010175291755,
3.34253904006323,3.55341784507492,3.76429664997047),.UNSPECIFIED.) ;
#334 = B_SPLINE_CURVE_WITH_KNOTS('',2,(#53927,#53928,#53929),
 .UNSPECIFIED.,.F.,.F.,(3,3),(0.,1.505093859451),.UNSPECIFIED.) ;
#335 = B_SPLINE_CURVE_WITH_KNOTS('',2,(#53933,#53934,#53935),
 .UNSPECIFIED.,.F.,.F.,(3,3),(0.0815875964935672,1.58668145590164),
 .UNSPECIFIED.) ;
#336 = B_SPLINE_CURVE_WITH_KNOTS('',3,(#53937,#53938,#53939,#53940,#53941,
#53942,#53943,#53944,#53945,#53946,#53947,#53948,#53949,#53950,#53951,#53952,
#53953,#53954,#53955,#53956,#53957,#53958,#53959,#53960,#53961,#53962,#53963,
#53964,#53965,#53966,#53967,#53968,#53969,#53970,#53971,#53972,#53973,#53974,
#53975,#53976),.UNSPECIFIED.,.F.,.F.,(4,3,3,3,3,3,3,3,3,3,3,3,3,4),(5.14917238118853,
5.36005118608411,5.57092999109581,5.77298643029957,5.97546031432194,6.12802772885396,
6.32462027006988,6.52281590231075,6.68512546661211,6.88364627198794,7.08054113574276,
7.24221135774884,7.44474766118475,7.51426349450141),.UNSPECIFIED.) ;
#337 = B_SPLINE_CURVE_WITH_KNOTS('',3,(#53980,#53981,#53982,#53983,#53984,
#53985,#53986,#53987,#53988,#53989,#53990,#53991,#53992,#53993,#53994,#53995,
#53996,#53997,#53998,#53999,#54000,#54001,#54002,#54003,#54004,#54005,#54006,
#54007,#54008,#54009,#54010,#54011,#54012,#54013,#54014,#54015,#54016,#54017,
#54018,#54019),.UNSPECIFIED.,.F.,.F.,(4,3,3,3,3,3,3,3,3,3,3,3,3,4),(1.3992055473476,
1.60174185079187,1.6712576734102,1.86788901812146,2.06612241241944,2.22834356454693,
2.42682695741341,2.62368336398125,2.78544130230507,2.98797174735946,3.19010175291812,
3.34253904006322,3.55341784507436,3.76429664996946),.UNSPECIFIED.) ;
#338 = B_SPLINE_CURVE_WITH_KNOTS('',2,(#54021,#54022,#54023),
 .UNSPECIFIED.,.F.,.F.,(3,3),(0.,1.50509385964352),.UNSPECIFIED.) ;
#339 = B_SPLINE_CURVE_WITH_KNOTS('',2,(#54027,#54028,#54029),
 .UNSPECIFIED.,.F.,.F.,(3,3),(0.0815875959280614,1.58668145590161),
 .UNSPECIFIED.) ;
#340 = B_SPLINE_CURVE_WITH_KNOTS('',3,(#54031,#54032,#54033,#54034,#54035,
#54036,#54037,#54038,#54039,#54040,#54041,#54042,#54043,#54044,#54045,#54046,
#54047,#54048,#54049,#54050,#54051,#54052,#54053,#54054,#54055,#54056,#54057,
#54058,#54059,#54060,#54061,#54062,#54063,#54064,#54065,#54066,#54067,#54068,
#54069,#54070),.UNSPECIFIED.,.F.,.F.,(4,3,3,3,3,3,3,3,3,3,3,3,3,4),(5.14917238118934,
5.36005118608456,5.57092999109581,5.77298643030027,5.97546031432337,6.12802772885396,
6.32462027007005,6.52281590231107,6.6851254666121,6.88364627198753,7.08054113574224,
7.24221135774884,7.44474766119323,7.51426348381142),.UNSPECIFIED.) ;
#341 = B_SPLINE_CURVE_WITH_KNOTS('',3,(#54074,#54075,#54076,#54077,#54078,
#54079,#54080,#54081,#54082,#54083,#54084,#54085,#54086,#54087,#54088,#54089,
#54090,#54091,#54092,#54093,#54094,#54095,#54096,#54097,#54098,#54099,#54100,
#54101,#54102,#54103,#54104,#54105,#54106,#54107,#54108,#54109,#54110,#54111,
#54112,#54113),.UNSPECIFIED.,.F.,.F.,(4,3,3,3,3,3,3,3,3,3,3,3,3,4),(1.39920580594633,
1.60174210962102,1.6712576734102,1.86788901812167,2.06612241242011,2.22834356454693,
2.42682695741379,2.62368336398277,2.78544130230507,2.9879717473613,3.19010175292116,
3.34253904006322,3.55341784507367,3.76429664996785),.UNSPECIFIED.) ;
#342 = B_SPLINE_CURVE_WITH_KNOTS('',2,(#54115,#54116,#54117),
 .UNSPECIFIED.,.F.,.F.,(3,3),(0.,1.50509385929303),.UNSPECIFIED.) ;
#343 = B_SPLINE_CURVE_WITH_KNOTS('',2,(#54121,#54122,#54123),
 .UNSPECIFIED.,.F.,.F.,(3,3),(0.0815875965016897,1.5866814559016),
 .UNSPECIFIED.) ;
#344 = B_SPLINE_CURVE_WITH_KNOTS('',3,(#54125,#54126,#54127,#54128,#54129,
#54130,#54131,#54132,#54133,#54134,#54135,#54136,#54137,#54138,#54139,#54140,
#54141,#54142,#54143,#54144,#54145,#54146,#54147,#54148,#54149,#54150,#54151,
#54152,#54153,#54154,#54155,#54156,#54157,#54158,#54159,#54160,#54161,#54162,
#54163,#54164),.UNSPECIFIED.,.F.,.F.,(4,3,3,3,3,3,3,3,3,3,3,3,3,4),(5.14917238119121,
5.36005118608542,5.57092999109581,5.77298643029801,5.97546031431876,6.12802772885396,
6.32462027007008,6.52281590231108,6.6851254666121,6.8836462719899,7.08054113574684,
7.24221135774884,7.44474766142535,7.51426322521267),.UNSPECIFIED.) ;
#345 = B_SPLINE_CURVE_WITH_KNOTS('',3,(#54168,#54169,#54170,#54171,#54172,
#54173,#54174,#54175,#54176,#54177,#54178,#54179,#54180,#54181,#54182,#54183,
#54184,#54185,#54186,#54187,#54188,#54189,#54190,#54191,#54192,#54193,#54194,
#54195,#54196,#54197,#54198,#54199,#54200,#54201,#54202,#54203,#54204,#54205,
#54206,#54207),.UNSPECIFIED.,.F.,.F.,(4,3,3,3,3,3,3,3,3,3,3,3,3,4),(1.39920578163106,
1.60174208528522,1.67125767341019,1.86788901812004,2.06612241241701,2.22834356454693,
2.42682695741272,2.62368336398046,2.78544130230507,2.98797174735873,3.19010175291722,
3.34253904006322,3.55341784507366,3.76429664996792),.UNSPECIFIED.) ;
#346 = B_SPLINE_CURVE_WITH_KNOTS('',2,(#54209,#54210,#54211),
 .UNSPECIFIED.,.F.,.F.,(3,3),(0.,1.50509385916676),.UNSPECIFIED.) ;
#347 = B_SPLINE_CURVE_WITH_KNOTS('',2,(#54215,#54216,#54217),
 .UNSPECIFIED.,.F.,.F.,(3,3),(0.0815875966396183,1.58668145590158),
 .UNSPECIFIED.) ;
#348 = B_SPLINE_CURVE_WITH_KNOTS('',3,(#54219,#54220,#54221,#54222,#54223,
#54224,#54225,#54226,#54227,#54228,#54229,#54230,#54231,#54232,#54233,#54234,
#54235,#54236,#54237,#54238,#54239,#54240,#54241,#54242,#54243,#54244,#54245,
#54246,#54247,#54248,#54249,#54250,#54251,#54252,#54253,#54254,#54255,#54256,
#54257,#54258),.UNSPECIFIED.,.F.,.F.,(4,3,3,3,3,3,3,3,3,3,3,3,3,4),(5.14917238119099,
5.36005118608529,5.57092999109581,5.77298643030054,5.97546031432383,6.12802772885395,
6.32462027006874,6.52281590230857,6.6851254666121,6.883646271988,7.08054113574284,
7.24221135774883,7.44474766140413,7.51426324952797),.UNSPECIFIED.) ;
#349 = B_SPLINE_CURVE_WITH_KNOTS('',3,(#54262,#54263,#54264,#54265,#54266,
#54267,#54268,#54269,#54270,#54271,#54272,#54273,#54274,#54275,#54276,#54277,
#54278,#54279,#54280,#54281,#54282,#54283,#54284,#54285,#54286,#54287,#54288,
#54289,#54290,#54291,#54292,#54293,#54294,#54295,#54296,#54297,#54298,#54299,
#54300,#54301),.UNSPECIFIED.,.F.,.F.,(4,3,3,3,3,3,3,3,3,3,3,3,3,4),(1.39920580297369,
1.60174210664721,1.6712576734102,1.86788901812216,2.06612241242095,2.22834356454693,
2.42682695741258,2.62368336398087,2.78544130230508,2.98797174735879,3.19010175291683,
3.34253904006322,3.55341784507441,3.76429664996957),.UNSPECIFIED.) ;
#350 = B_SPLINE_CURVE_WITH_KNOTS('',2,(#54303,#54304,#54305),
 .UNSPECIFIED.,.F.,.F.,(3,3),(0.,1.50509385957502),.UNSPECIFIED.) ;
#351 = B_SPLINE_CURVE_WITH_KNOTS('',2,(#54309,#54310,#54311),
 .UNSPECIFIED.,.F.,.F.,(3,3),(0.0815875964292831,1.58668145590159),
 .UNSPECIFIED.) ;
#352 = B_SPLINE_CURVE_WITH_KNOTS('',3,(#54313,#54314,#54315,#54316,#54317,
#54318,#54319,#54320,#54321,#54322,#54323,#54324,#54325,#54326,#54327,#54328,
#54329,#54330,#54331,#54332,#54333,#54334,#54335,#54336,#54337,#54338,#54339,
#54340,#54341,#54342,#54343,#54344,#54345,#54346,#54347,#54348,#54349,#54350,
#54351,#54352),.UNSPECIFIED.,.F.,.F.,(4,3,3,3,3,3,3,3,3,3,3,3,3,4),(5.14917238118972,
5.36005118608478,5.57092999109581,5.77298643029918,5.97546031432131,6.12802772885395,
6.32462027006936,6.52281590230965,6.6851254666121,6.88364627198904,7.08054113574454,
7.24221135774883,7.44474766142377,7.51426322818532),.UNSPECIFIED.) ;
#353 = B_SPLINE_CURVE_WITH_KNOTS('',3,(#54356,#54357,#54358,#54359,#54360,
#54361,#54362,#54363,#54364,#54365,#54366,#54367,#54368,#54369,#54370,#54371,
#54372,#54373,#54374,#54375,#54376,#54377,#54378,#54379,#54380,#54381,#54382,
#54383,#54384,#54385,#54386,#54387,#54388,#54389,#54390,#54391,#54392,#54393,
#54394,#54395),.UNSPECIFIED.,.F.,.F.,(4,3,3,3,3,3,3,3,3,3,3,3,3,4),(1.39920556389945,
1.60174186735948,1.67125767341019,1.86788901812192,2.06612241242117,2.22834356454693,
2.426826957414,2.62368336398261,2.78544130230507,2.98797174735794,3.1901017529155,
3.34253904006322,3.55341784507408,3.76429664996891),.UNSPECIFIED.) ;
#354 = B_SPLINE_CURVE_WITH_KNOTS('',2,(#54397,#54398,#54399),
 .UNSPECIFIED.,.F.,.F.,(3,3),(0.,1.50509385942592),.UNSPECIFIED.) ;
#355 = B_SPLINE_CURVE_WITH_KNOTS('',2,(#54403,#54404,#54405),
 .UNSPECIFIED.,.F.,.F.,(3,3),(0.0815875963862985,1.5866814559016),
 .UNSPECIFIED.) ;
#356 = B_SPLINE_CURVE_WITH_KNOTS('',3,(#54407,#54408,#54409,#54410,#54411,
#54412,#54413,#54414,#54415,#54416,#54417,#54418,#54419,#54420,#54421,#54422,
#54423,#54424,#54425,#54426,#54427,#54428,#54429,#54430,#54431,#54432,#54433,
#54434,#54435,#54436,#54437,#54438,#54439,#54440,#54441,#54442,#54443,#54444,
#54445,#54446),.UNSPECIFIED.,.F.,.F.,(4,3,3,3,3,3,3,3,3,3,3,3,3,4),(5.14917238118991,
5.36005118608483,5.57092999109581,5.77298643030024,5.97546031432328,6.12802772885395,
6.32462027006993,6.52281590231083,6.6851254666121,6.88364627199045,7.0805411357475,
7.24221135774883,7.44474766121079,7.51426346725949),.UNSPECIFIED.) ;
#357 = B_SPLINE_CURVE_WITH_KNOTS('',3,(#54450,#54451,#54452,#54453,#54454,
#54455,#54456,#54457,#54458,#54459,#54460,#54461,#54462,#54463,#54464,#54465,
#54466,#54467,#54468,#54469,#54470,#54471,#54472,#54473,#54474,#54475,#54476,
#54477,#54478,#54479,#54480,#54481,#54482,#54483,#54484,#54485,#54486,#54487,
#54488,#54489),.UNSPECIFIED.,.F.,.F.,(4,3,3,3,3,3,3,3,3,3,3,3,3,4),(1.39920553665765,
1.60174184009286,1.6712576734102,1.86788901812204,2.06612241242079,2.22834356454693,
2.42682695741453,2.62368336398352,2.78544130230508,2.98797174736053,3.19010175291979,
3.34253904006323,3.55341784507441,3.76429664996951),.UNSPECIFIED.) ;
#358 = B_SPLINE_CURVE_WITH_KNOTS('',2,(#54491,#54492,#54493),
 .UNSPECIFIED.,.F.,.F.,(3,3),(0.,1.50509385956687),.UNSPECIFIED.) ;
#359 = B_SPLINE_CURVE_WITH_KNOTS('',2,(#54497,#54498,#54499),
 .UNSPECIFIED.,.F.,.F.,(3,3),(0.0815875965308134,1.58668145590159),
 .UNSPECIFIED.) ;
#360 = B_SPLINE_CURVE_WITH_KNOTS('',3,(#54501,#54502,#54503,#54504,#54505,
#54506,#54507,#54508,#54509,#54510,#54511,#54512,#54513,#54514,#54515,#54516,
#54517,#54518,#54519,#54520,#54521,#54522,#54523,#54524,#54525,#54526,#54527,
#54528,#54529,#54530,#54531,#54532,#54533,#54534,#54535,#54536,#54537,#54538,
#54539,#54540),.UNSPECIFIED.,.F.,.F.,(4,3,3,3,3,3,3,3,3,3,3,3,3,4),(5.14917238118966,
5.36005118608471,5.57092999109581,5.77298643029994,5.9754603143227,6.12802772885396,
6.32462027006873,6.5228159023084,6.6851254666121,6.88364627198617,7.0805411357391,
7.24221135774884,7.44474766118404,7.51426349450139),.UNSPECIFIED.) ;
#361 = B_SPLINE_CURVE_WITH_KNOTS('',3,(#54544,#54545,#54546,#54547,#54548,
#54549,#54550,#54551,#54552,#54553,#54554,#54555,#54556,#54557,#54558,#54559,
#54560,#54561,#54562,#54563,#54564,#54565,#54566,#54567,#54568,#54569,#54570,
#54571,#54572,#54573,#54574,#54575,#54576,#54577,#54578,#54579,#54580,#54581,
#54582,#54583),.UNSPECIFIED.,.F.,.F.,(4,3,3,3,3,3,3,3,3,3,3,3,3,4),(1.39920553665761,
1.60174184009247,1.6712576734102,1.86788901812121,2.06612241241882,2.22834356454693,
2.42682695741519,2.62368336398565,2.78544130230508,2.98797174735976,3.1901017529189,
3.34253904006323,3.55341784507426,3.76429664996931),.UNSPECIFIED.) ;
#362 = B_SPLINE_CURVE_WITH_KNOTS('',2,(#54585,#54586,#54587),
 .UNSPECIFIED.,.F.,.F.,(3,3),(0.,1.50509385941839),.UNSPECIFIED.) ;
#363 = B_SPLINE_CURVE_WITH_KNOTS('',2,(#54591,#54592,#54593),
 .UNSPECIFIED.,.F.,.F.,(3,3),(0.081587596231324,1.5866814559016),
 .UNSPECIFIED.) ;
#364 = B_SPLINE_CURVE_WITH_KNOTS('',3,(#54595,#54596,#54597,#54598,#54599,
#54600,#54601,#54602,#54603,#54604,#54605,#54606,#54607,#54608,#54609,#54610,
#54611,#54612,#54613,#54614,#54615,#54616,#54617,#54618,#54619,#54620,#54621,
#54622,#54623,#54624,#54625,#54626,#54627,#54628,#54629,#54630,#54631,#54632,
#54633,#54634),.UNSPECIFIED.,.F.,.F.,(4,3,3,3,3,3,3,3,3,3,3,3,3,4),(5.14917238118963,
5.36005118608472,5.57092999109581,5.77298643030019,5.97546031432334,6.12802772885396,
6.32462027006835,6.52281590230765,6.68512546661211,6.88364627198795,7.08054113574254,
7.24221135774884,7.4447476611839,7.51426349450141),.UNSPECIFIED.) ;
#365 = B_SPLINE_CURVE_WITH_KNOTS('',3,(#54638,#54639,#54640,#54641,#54642,
#54643,#54644,#54645,#54646,#54647,#54648,#54649,#54650,#54651,#54652,#54653,
#54654,#54655,#54656,#54657,#54658,#54659,#54660,#54661,#54662,#54663,#54664,
#54665,#54666,#54667,#54668,#54669,#54670,#54671,#54672,#54673,#54674,#54675,
#54676,#54677),.UNSPECIFIED.,.F.,.F.,(4,3,3,3,3,3,3,3,3,3,3,3,3,4),(1.39920577957092,
1.60174208322376,1.6712576734102,1.86788901812092,2.06612241241852,2.22834356454693,
2.42682695741545,2.62368336398506,2.78544130230508,2.98797174736192,3.19010175292271,
3.34253904006322,3.55341784507434,3.76429664996941),.UNSPECIFIED.) ;
#366 = B_SPLINE_CURVE_WITH_KNOTS('',2,(#54679,#54680,#54681),
 .UNSPECIFIED.,.F.,.F.,(3,3),(0.,1.50509385951517),.UNSPECIFIED.) ;
#367 = B_SPLINE_CURVE_WITH_KNOTS('',2,(#54685,#54686,#54687),
 .UNSPECIFIED.,.F.,.F.,(3,3),(0.0815875965974276,1.58668145590159),
 .UNSPECIFIED.) ;
#368 = B_SPLINE_CURVE_WITH_KNOTS('',3,(#54689,#54690,#54691,#54692,#54693,
#54694,#54695,#54696,#54697,#54698,#54699,#54700,#54701,#54702,#54703,#54704,
#54705,#54706,#54707,#54708,#54709,#54710,#54711,#54712,#54713,#54714,#54715,
#54716,#54717,#54718,#54719,#54720,#54721,#54722,#54723,#54724,#54725,#54726,
#54727,#54728),.UNSPECIFIED.,.F.,.F.,(4,3,3,3,3,3,3,3,3,3,3,3,3,4),(5.14917238118954,
5.36005118608465,5.57092999109581,5.77298643029922,5.9754603143212,6.12802772885395,
6.32462027006964,6.52281590231008,6.6851254666121,6.88364627198796,7.0805411357427,
7.24221135774883,7.44474766140348,7.51426325158808),.UNSPECIFIED.) ;
#369 = B_SPLINE_CURVE_WITH_KNOTS('',3,(#54732,#54733,#54734,#54735,#54736,
#54737,#54738,#54739,#54740,#54741,#54742,#54743,#54744,#54745,#54746,#54747,
#54748,#54749,#54750,#54751,#54752,#54753,#54754,#54755,#54756,#54757,#54758,
#54759,#54760,#54761,#54762,#54763,#54764,#54765,#54766,#54767,#54768,#54769,
#54770,#54771),.UNSPECIFIED.,.F.,.F.,(4,3,3,3,3,3,3,3,3,3,3,3,3,4),(1.39920575510034,
1.60174205873101,1.6712576734102,1.86788901812208,2.06612241242132,2.22834356454693,
2.42682695741398,2.623683363982,2.78544130230508,2.98797174735979,3.19010175291888,
3.34253904006322,3.55341784507434,3.76429664996953),.UNSPECIFIED.) ;
#370 = B_SPLINE_CURVE_WITH_KNOTS('',2,(#54773,#54774,#54775),
 .UNSPECIFIED.,.F.,.F.,(3,3),(0.,1.50509385978829),.UNSPECIFIED.) ;
#371 = B_SPLINE_CURVE_WITH_KNOTS('',2,(#54779,#54780,#54781),
 .UNSPECIFIED.,.F.,.F.,(3,3),(0.0815875962064005,1.58668145590161),
 .UNSPECIFIED.) ;
#372 = B_SPLINE_CURVE_WITH_KNOTS('',3,(#54783,#54784,#54785,#54786,#54787,
#54788,#54789,#54790,#54791,#54792,#54793,#54794,#54795,#54796,#54797,#54798,
#54799,#54800,#54801,#54802,#54803,#54804,#54805,#54806,#54807,#54808,#54809,
#54810,#54811,#54812,#54813,#54814,#54815,#54816,#54817,#54818,#54819,#54820,
#54821,#54822),.UNSPECIFIED.,.F.,.F.,(4,3,3,3,3,3,3,3,3,3,3,3,3,4),(5.14917238118977,
5.36005118608484,5.57092999109581,5.77298643029907,5.97546031432088,6.12802772885396,
6.32462027006765,6.52281590230627,6.68512546661211,6.88364627198604,7.08054113573874,
7.24221135774884,7.44474766137677,7.51426327605873),.UNSPECIFIED.) ;
#373 = B_SPLINE_CURVE_WITH_KNOTS('',3,(#54826,#54827,#54828,#54829,#54830,
#54831,#54832,#54833,#54834,#54835,#54836,#54837,#54838,#54839,#54840,#54841,
#54842,#54843,#54844,#54845,#54846,#54847,#54848,#54849,#54850,#54851,#54852,
#54853,#54854,#54855,#54856,#54857,#54858,#54859,#54860,#54861,#54862,#54863,
#54864,#54865),.UNSPECIFIED.,.F.,.F.,(4,3,3,3,3,3,3,3,3,3,3,3,3,4),(1.39920578522048,
1.60174208887688,1.6712576734102,1.86788901812355,2.06612241242382,2.22834356454693,
2.42682695741664,2.62368336398744,2.78544130230508,2.98797174736012,3.19010175291939,
3.34253904006323,3.55341784507339,3.76429664996726),.UNSPECIFIED.) ;
#374 = B_SPLINE_CURVE_WITH_KNOTS('',2,(#54867,#54868,#54869),
 .UNSPECIFIED.,.F.,.F.,(3,3),(0.,1.50509385946946),.UNSPECIFIED.) ;
#375 = B_SPLINE_CURVE_WITH_KNOTS('',2,(#54873,#54874,#54875),
 .UNSPECIFIED.,.F.,.F.,(3,3),(0.0815875967998225,1.58668145590156),
 .UNSPECIFIED.) ;
#376 = B_SPLINE_CURVE_WITH_KNOTS('',3,(#54877,#54878,#54879,#54880,#54881,
#54882,#54883,#54884,#54885,#54886,#54887,#54888,#54889,#54890,#54891,#54892,
#54893,#54894,#54895,#54896,#54897,#54898,#54899,#54900,#54901,#54902,#54903,
#54904,#54905,#54906,#54907,#54908,#54909,#54910,#54911,#54912,#54913,#54914,
#54915,#54916),.UNSPECIFIED.,.F.,.F.,(4,3,3,3,3,3,3,3,3,3,3,3,3,4),(5.14917238119203,
5.36005118608581,5.57092999109581,5.77298643029689,5.97546031431666,6.12802772885396,
6.32462027006706,6.52281590230514,6.6851254666121,6.88364627198659,7.08054113574006,
7.24221135774884,7.44474766140431,7.51426324593851),.UNSPECIFIED.) ;
#377 = B_SPLINE_CURVE_WITH_KNOTS('',3,(#54920,#54921,#54922,#54923,#54924,
#54925,#54926,#54927,#54928,#54929,#54930,#54931,#54932,#54933,#54934,#54935,
#54936,#54937,#54938,#54939,#54940,#54941,#54942,#54943,#54944,#54945,#54946,
#54947,#54948,#54949,#54950,#54951,#54952,#54953,#54954,#54955,#54956,#54957,
#54958,#54959),.UNSPECIFIED.,.F.,.F.,(4,3,3,3,3,3,3,3,3,3,3,3,3,4),(1.39920579236041,
1.6017420960232,1.6712576734102,1.86788901812226,2.06612241242125,2.22834356454693,
2.42682695741395,2.62368336398385,2.78544130230508,2.98797174735984,3.19010175291892,
3.34253904006322,3.55341784507403,3.76429664996856),.UNSPECIFIED.) ;
#378 = B_SPLINE_CURVE_WITH_KNOTS('',2,(#54961,#54962,#54963),
 .UNSPECIFIED.,.F.,.F.,(3,3),(0.,1.50509385922266),.UNSPECIFIED.) ;
#379 = B_SPLINE_CURVE_WITH_KNOTS('',2,(#54967,#54968,#54969),
 .UNSPECIFIED.,.F.,.F.,(3,3),(0.0815875968142298,1.58668145590157),
 .UNSPECIFIED.) ;
#380 = B_SPLINE_CURVE_WITH_KNOTS('',3,(#54971,#54972,#54973,#54974,#54975,
#54976,#54977,#54978,#54979,#54980,#54981,#54982,#54983,#54984,#54985,#54986,
#54987,#54988,#54989,#54990,#54991,#54992,#54993,#54994,#54995,#54996,#54997,
#54998,#54999,#55000,#55001,#55002,#55003,#55004,#55005,#55006,#55007,#55008,
#55009,#55010),.UNSPECIFIED.,.F.,.F.,(4,3,3,3,3,3,3,3,3,3,3,3,3,4),(5.14917238119063,
5.36005118608513,5.57092999109581,5.77298643030012,5.97546031432292,6.12802772885395,
6.32462027007051,6.52281590231203,6.6851254666121,6.8836462719894,7.08054113574546,
7.24221135774883,7.44474766141017,7.51426323879855),.UNSPECIFIED.) ;
#381 = B_SPLINE_CURVE_WITH_KNOTS('',3,(#55014,#55015,#55016,#55017,#55018,
#55019,#55020,#55021,#55022,#55023,#55024,#55025,#55026,#55027,#55028,#55029,
#55030,#55031,#55032,#55033,#55034,#55035,#55036,#55037,#55038,#55039,#55040,
#55041,#55042,#55043,#55044,#55045,#55046,#55047,#55048,#55049,#55050,#55051,
#55052,#55053),.UNSPECIFIED.,.F.,.F.,(4,3,3,3,3,3,3,3,3,3,3,3,3,4),(1.39920565780197,
1.6017419613437,1.6712576734102,1.86788901812192,2.06612241242043,2.22834356454693,
2.42682695741329,2.62368336398141,2.78544130230508,2.98797174735931,3.19010175291749,
3.34253904006323,3.5534178450742,3.76429664996896),.UNSPECIFIED.) ;
#382 = B_SPLINE_CURVE_WITH_KNOTS('',2,(#55055,#55056,#55057),
 .UNSPECIFIED.,.F.,.F.,(3,3),(0.,1.50509385918315),.UNSPECIFIED.) ;
#383 = B_SPLINE_CURVE_WITH_KNOTS('',2,(#55061,#55062,#55063),
 .UNSPECIFIED.,.F.,.F.,(3,3),(0.0815875963175643,1.58668145590161),
 .UNSPECIFIED.) ;
#384 = B_SPLINE_CURVE_WITH_KNOTS('',3,(#55065,#55066,#55067,#55068,#55069,
#55070,#55071,#55072,#55073,#55074,#55075,#55076,#55077,#55078,#55079,#55080,
#55081,#55082,#55083,#55084,#55085,#55086,#55087,#55088,#55089,#55090,#55091,
#55092,#55093,#55094,#55095,#55096,#55097,#55098,#55099,#55100,#55101,#55102,
#55103,#55104),.UNSPECIFIED.,.F.,.F.,(4,3,3,3,3,3,3,3,3,3,3,3,3,4),(5.14917238118996,
5.36005118608481,5.57092999109581,5.77298643029938,5.97546031432158,6.12802772885396,
6.32462027006706,6.52281590230528,6.68512546661211,6.88364627198969,7.08054113574575,
7.24221135774884,7.44474766128961,7.51426337335708),.UNSPECIFIED.) ;
#385 = B_SPLINE_CURVE_WITH_KNOTS('',3,(#55108,#55109,#55110,#55111,#55112,
#55113,#55114,#55115,#55116,#55117,#55118,#55119,#55120,#55121,#55122,#55123,
#55124,#55125,#55126,#55127,#55128,#55129,#55130,#55131,#55132,#55133,#55134,
#55135,#55136,#55137,#55138,#55139,#55140,#55141,#55142,#55143,#55144,#55145,
#55146,#55147),.UNSPECIFIED.,.F.,.F.,(4,3,3,3,3,3,3,3,3,3,3,3,3,4),(1.39920626730384,
1.60174256547371,1.6712576734102,1.86788901812253,2.06612241242136,2.22834356454693,
2.42682695741533,2.62368336398524,2.78544130230508,2.9879717473591,3.19010175291799,
3.34253904006322,3.55341784507403,3.76429664996862),.UNSPECIFIED.) ;
#386 = B_SPLINE_CURVE_WITH_KNOTS('',2,(#55149,#55150,#55151),
 .UNSPECIFIED.,.F.,.F.,(3,3),(0.,1.50509385974731),.UNSPECIFIED.) ;
#387 = B_SPLINE_CURVE_WITH_KNOTS('',2,(#55155,#55156,#55157),
 .UNSPECIFIED.,.F.,.F.,(3,3),(0.081587596220629,1.58668145590162),
 .UNSPECIFIED.) ;
#388 = B_SPLINE_CURVE_WITH_KNOTS('',3,(#55159,#55160,#55161,#55162,#55163,
#55164,#55165,#55166,#55167,#55168,#55169,#55170,#55171,#55172,#55173,#55174,
#55175,#55176,#55177,#55178,#55179,#55180,#55181,#55182,#55183,#55184,#55185,
#55186,#55187,#55188,#55189,#55190,#55191,#55192,#55193,#55194,#55195,#55196,
#55197,#55198),.UNSPECIFIED.,.F.,.F.,(4,3,3,3,3,3,3,3,3,3,3,3,3,4),(5.14917238119046,
5.36005118608503,5.57092999109581,5.77298643030045,5.97546031432374,6.12802772885396,
6.32462027006966,6.52281590231019,6.6851254666121,6.88364627198813,7.08054113574297,
7.24221135774884,7.44474766183158,7.51426276518474),.UNSPECIFIED.) ;
#389 = B_SPLINE_CURVE_WITH_KNOTS('',3,(#55202,#55203,#55204,#55205,#55206,
#55207,#55208,#55209,#55210,#55211,#55212,#55213,#55214,#55215,#55216,#55217,
#55218,#55219,#55220,#55221,#55222,#55223,#55224,#55225,#55226,#55227,#55228,
#55229,#55230,#55231,#55232,#55233,#55234,#55235,#55236,#55237,#55238,#55239,
#55240,#55241),.UNSPECIFIED.,.F.,.F.,(4,3,3,3,3,3,3,3,3,3,3,3,3,4),(1.39920553665763,
1.60174184009342,1.6712576734102,1.86788901812086,2.06612241241843,2.22834356454693,
2.42682695741443,2.62368336398377,2.78544130230508,2.98797174735924,3.19010175291802,
3.34253904006322,3.55341784507355,3.76429664996775),.UNSPECIFIED.) ;
#390 = B_SPLINE_CURVE_WITH_KNOTS('',2,(#55243,#55244,#55245),
 .UNSPECIFIED.,.F.,.F.,(3,3),(0.,1.50509385940246),.UNSPECIFIED.) ;
#391 = B_SPLINE_CURVE_WITH_KNOTS('',2,(#55249,#55250,#55251),
 .UNSPECIFIED.,.F.,.F.,(3,3),(0.0815875964990715,1.58668145590159),
 .UNSPECIFIED.) ;
#392 = B_SPLINE_CURVE_WITH_KNOTS('',3,(#55253,#55254,#55255,#55256,#55257,
#55258,#55259,#55260,#55261,#55262,#55263,#55264,#55265,#55266,#55267,#55268,
#55269,#55270,#55271,#55272,#55273,#55274,#55275,#55276,#55277,#55278,#55279,
#55280,#55281,#55282,#55283,#55284,#55285,#55286,#55287,#55288,#55289,#55290,
#55291,#55292),.UNSPECIFIED.,.F.,.F.,(4,3,3,3,3,3,3,3,3,3,3,3,3,4),(5.14917238119122,
5.36005118608543,5.57092999109581,5.77298643029924,5.97546031432136,6.12802772885395,
6.32462027006939,6.52281590230979,6.6851254666121,6.88364627198772,7.08054113574227,
7.24221135774883,7.44474766118609,7.5142634945014),.UNSPECIFIED.) ;
#393 = B_SPLINE_CURVE_WITH_KNOTS('',3,(#55296,#55297,#55298,#55299,#55300,
#55301,#55302,#55303,#55304,#55305,#55306,#55307,#55308,#55309,#55310,#55311,
#55312,#55313,#55314,#55315,#55316,#55317,#55318,#55319,#55320,#55321,#55322,
#55323,#55324,#55325,#55326,#55327,#55328,#55329,#55330,#55331,#55332,#55333,
#55334,#55335),.UNSPECIFIED.,.F.,.F.,(4,3,3,3,3,3,3,3,3,3,3,3,3,4),(1.39920626597427,
1.60174256547503,1.6712576734102,1.86788901812092,2.06612241241852,2.22834356454693,
2.4268269574154,2.62368336398519,2.78544130230508,2.98797174735909,3.19010175291677,
3.34253904006322,3.55341784507445,3.76429664996961),.UNSPECIFIED.) ;
#394 = B_SPLINE_CURVE_WITH_KNOTS('',2,(#55337,#55338,#55339),
 .UNSPECIFIED.,.F.,.F.,(3,3),(0.,1.50509385919341),.UNSPECIFIED.) ;
#395 = B_SPLINE_CURVE_WITH_KNOTS('',2,(#55343,#55344,#55345),
 .UNSPECIFIED.,.F.,.F.,(3,3),(0.0815875964645715,1.58668145590163),
 .UNSPECIFIED.) ;
#396 = B_SPLINE_CURVE_WITH_KNOTS('',3,(#55347,#55348,#55349,#55350,#55351,
#55352,#55353,#55354,#55355,#55356,#55357,#55358,#55359,#55360,#55361,#55362,
#55363,#55364,#55365,#55366,#55367,#55368,#55369,#55370,#55371,#55372,#55373,
#55374,#55375,#55376,#55377,#55378,#55379,#55380,#55381,#55382,#55383,#55384,
#55385,#55386),.UNSPECIFIED.,.F.,.F.,(4,3,3,3,3,3,3,3,3,3,3,3,3,4),(5.14917238118938,
5.36005118608458,5.57092999109581,5.77298643029965,5.97546031432214,6.12802772885396,
6.32462027006888,6.5228159023088,6.6851254666121,6.88364627198861,7.0805411357444,
7.24221135774884,7.44474766183236,7.51426276385522),.UNSPECIFIED.) ;
#397 = B_SPLINE_CURVE_WITH_KNOTS('',3,(#55390,#55391,#55392,#55393,#55394,
#55395,#55396,#55397,#55398,#55399,#55400,#55401,#55402,#55403,#55404,#55405,
#55406,#55407,#55408,#55409,#55410,#55411,#55412,#55413,#55414,#55415,#55416,
#55417,#55418,#55419,#55420,#55421,#55422,#55423,#55424,#55425,#55426,#55427,
#55428,#55429),.UNSPECIFIED.,.F.,.F.,(4,3,3,3,3,3,3,3,3,3,3,3,3,4),(1.39920565780197,
1.60174196134636,1.6712576734102,1.86788901812062,2.06612241241771,2.22834356454693,
2.42682695741333,2.62368336398205,2.78544130230508,2.98797174735987,3.19010175291831,
3.34253904006323,3.55341784507432,3.76429664996955),.UNSPECIFIED.) ;
#398 = B_SPLINE_CURVE_WITH_KNOTS('',2,(#55431,#55432,#55433),
 .UNSPECIFIED.,.F.,.F.,(3,3),(0.,1.50509385959389),.UNSPECIFIED.) ;
#399 = B_SPLINE_CURVE_WITH_KNOTS('',2,(#55437,#55438,#55439),
 .UNSPECIFIED.,.F.,.F.,(3,3),(0.0815875963589051,1.58668145590161),
 .UNSPECIFIED.) ;
#400 = B_SPLINE_CURVE_WITH_KNOTS('',3,(#55441,#55442,#55443,#55444,#55445,
#55446,#55447,#55448,#55449,#55450,#55451,#55452,#55453,#55454,#55455,#55456,
#55457,#55458,#55459,#55460,#55461,#55462,#55463,#55464,#55465,#55466,#55467,
#55468,#55469,#55470,#55471,#55472,#55473,#55474,#55475,#55476,#55477,#55478,
#55479,#55480),.UNSPECIFIED.,.F.,.F.,(4,3,3,3,3,3,3,3,3,3,3,3,3,4),(5.1491723811898,
5.36005118608492,5.57092999109581,5.77298643029963,5.97546031432211,6.12802772885396,
6.32462027007047,6.52281590231188,6.6851254666121,6.88364627198989,7.08054113574668,
7.24221135774884,7.44474766129325,7.51426337335708),.UNSPECIFIED.) ;
#401 = B_SPLINE_CURVE_WITH_KNOTS('',3,(#55484,#55485,#55486,#55487,#55488,
#55489,#55490,#55491,#55492,#55493,#55494,#55495,#55496,#55497,#55498,#55499,
#55500,#55501,#55502,#55503,#55504,#55505,#55506,#55507,#55508,#55509,#55510,
#55511,#55512,#55513,#55514,#55515,#55516,#55517,#55518,#55519,#55520,#55521,
#55522,#55523),.UNSPECIFIED.,.F.,.F.,(4,3,3,3,3,3,3,3,3,3,3,3,3,4),(1.39920579236047,
1.60174209602461,1.6712576734102,1.86788901812178,2.06612241242039,2.22834356454693,
2.42682695741637,2.6236833639871,2.78544130230507,2.98797174736062,3.1901017529202,
3.34253904006322,3.55341784507431,3.76429664996928),.UNSPECIFIED.) ;
#402 = B_SPLINE_CURVE_WITH_KNOTS('',2,(#55525,#55526,#55527),
 .UNSPECIFIED.,.F.,.F.,(3,3),(0.,1.50509385958745),.UNSPECIFIED.) ;
#403 = B_SPLINE_CURVE_WITH_KNOTS('',2,(#55531,#55532,#55533),
 .UNSPECIFIED.,.F.,.F.,(3,3),(0.081587596555011,1.58668145590161),
 .UNSPECIFIED.) ;
#404 = B_SPLINE_CURVE_WITH_KNOTS('',3,(#55535,#55536,#55537,#55538,#55539,
#55540,#55541,#55542,#55543,#55544,#55545,#55546,#55547,#55548,#55549,#55550,
#55551,#55552,#55553,#55554,#55555,#55556,#55557,#55558,#55559,#55560,#55561,
#55562,#55563,#55564,#55565,#55566,#55567,#55568,#55569,#55570,#55571,#55572,
#55573,#55574),.UNSPECIFIED.,.F.,.F.,(4,3,3,3,3,3,3,3,3,3,3,3,3,4),(5.14917238118991,
5.36005118608479,5.5709299910958,5.77298643029917,5.9754603143211,6.12802772885395,
6.32462027006938,6.5228159023099,6.68512546661209,6.88364627198928,7.08054113574494,
7.24221135774883,7.44474766141436,7.51426323879859),.UNSPECIFIED.) ;
#405 = B_SPLINE_CURVE_WITH_KNOTS('',3,(#55578,#55579,#55580,#55581,#55582,
#55583,#55584,#55585,#55586,#55587,#55588,#55589,#55590,#55591,#55592,#55593,
#55594,#55595,#55596,#55597,#55598,#55599,#55600,#55601,#55602,#55603,#55604,
#55605,#55606,#55607,#55608,#55609,#55610,#55611,#55612,#55613,#55614,#55615,
#55616,#55617),.UNSPECIFIED.,.F.,.F.,(4,3,3,3,3,3,3,3,3,3,3,3,3,4),(1.39920578522049,
1.60174208887845,1.6712576734102,1.86788901812191,2.0661224124205,2.22834356454693,
2.42682695741374,2.62368336398196,2.78544130230508,2.98797174736077,3.19010175292072,
3.34253904006322,3.55341784507369,3.76429664996809),.UNSPECIFIED.) ;
#406 = B_SPLINE_CURVE_WITH_KNOTS('',2,(#55619,#55620,#55621),
 .UNSPECIFIED.,.F.,.F.,(3,3),(0.,1.50509385994802),.UNSPECIFIED.) ;
#407 = B_SPLINE_CURVE_WITH_KNOTS('',2,(#55625,#55626,#55627),
 .UNSPECIFIED.,.F.,.F.,(3,3),(0.0815875960578148,1.58668145590161),
 .UNSPECIFIED.) ;
#408 = B_SPLINE_CURVE_WITH_KNOTS('',3,(#55629,#55630,#55631,#55632,#55633,
#55634,#55635,#55636,#55637,#55638,#55639,#55640,#55641,#55642,#55643,#55644,
#55645,#55646,#55647,#55648,#55649,#55650,#55651,#55652,#55653,#55654,#55655,
#55656,#55657,#55658,#55659,#55660,#55661,#55662,#55663,#55664,#55665,#55666,
#55667,#55668),.UNSPECIFIED.,.F.,.F.,(4,3,3,3,3,3,3,3,3,3,3,3,3,4),(5.14917238119084,
5.36005118608529,5.57092999109581,5.7729864302989,5.97546031432077,6.12802772885396,
6.32462027007018,6.52281590231123,6.6851254666121,6.8836462719878,7.08054113574219,
7.24221135774883,7.44474766140652,7.5142632459385),.UNSPECIFIED.) ;
#409 = B_SPLINE_CURVE_WITH_KNOTS('',3,(#55672,#55673,#55674,#55675,#55676,
#55677,#55678,#55679,#55680,#55681,#55682,#55683,#55684,#55685,#55686,#55687,
#55688,#55689,#55690,#55691,#55692,#55693,#55694,#55695,#55696,#55697,#55698,
#55699,#55700,#55701,#55702,#55703,#55704,#55705,#55706,#55707,#55708,#55709,
#55710,#55711),.UNSPECIFIED.,.F.,.F.,(4,3,3,3,3,3,3,3,3,3,3,3,3,4),(1.39920575510034,
1.60174205873404,1.6712576734102,1.86788901812231,2.06612241242113,2.22834356454693,
2.42682695741377,2.62368336398224,2.78544130230507,2.98797174735987,3.1901017529183,
3.34253904006322,3.5534178450742,3.76429664996902),.UNSPECIFIED.) ;
#410 = B_SPLINE_CURVE_WITH_KNOTS('',2,(#55713,#55714,#55715),
 .UNSPECIFIED.,.F.,.F.,(3,3),(0.,1.50509385928664),.UNSPECIFIED.) ;
#411 = B_SPLINE_CURVE_WITH_KNOTS('',2,(#55719,#55720,#55721),
 .UNSPECIFIED.,.F.,.F.,(3,3),(0.081587596588401,1.58668145590163),
 .UNSPECIFIED.) ;
#412 = B_SPLINE_CURVE_WITH_KNOTS('',3,(#55723,#55724,#55725,#55726,#55727,
#55728,#55729,#55730,#55731,#55732,#55733,#55734,#55735,#55736,#55737,#55738,
#55739,#55740,#55741,#55742,#55743,#55744,#55745,#55746,#55747,#55748,#55749,
#55750,#55751,#55752,#55753,#55754,#55755,#55756,#55757,#55758,#55759,#55760,
#55761,#55762),.UNSPECIFIED.,.F.,.F.,(4,3,3,3,3,3,3,3,3,3,3,3,3,4),(5.14917238118993,
5.36005118608476,5.57092999109581,5.77298643029968,5.97546031432223,6.12802772885395,
6.32462027006896,6.52281590230873,6.6851254666121,6.88364627198979,7.08054113574599,
7.24221135774883,7.44474766138134,7.51426327605874),.UNSPECIFIED.) ;
#413 = B_SPLINE_CURVE_WITH_KNOTS('',3,(#55766,#55767,#55768,#55769,#55770,
#55771,#55772,#55773,#55774,#55775,#55776,#55777,#55778,#55779,#55780,#55781,
#55782,#55783,#55784,#55785,#55786,#55787,#55788,#55789,#55790,#55791,#55792,
#55793,#55794,#55795,#55796,#55797,#55798,#55799,#55800,#55801,#55802,#55803,
#55804,#55805),.UNSPECIFIED.,.F.,.F.,(4,3,3,3,3,3,3,3,3,3,3,3,3,4),(1.39920577957096,
1.60174208322522,1.6712576734102,1.86788901812319,2.06612241242312,2.22834356454693,
2.42682695741511,2.62368336398486,2.78544130230508,2.98797174736008,3.19010175291886,
3.34253904006322,3.5534178450743,3.76429664996913),.UNSPECIFIED.) ;
#414 = B_SPLINE_CURVE_WITH_KNOTS('',2,(#55807,#55808,#55809),
 .UNSPECIFIED.,.F.,.F.,(3,3),(0.,1.50509385929993),.UNSPECIFIED.) ;
#415 = B_SPLINE_CURVE_WITH_KNOTS('',2,(#55813,#55814,#55815),
 .UNSPECIFIED.,.F.,.F.,(3,3),(0.0815875966725096,1.58668145590163),
 .UNSPECIFIED.) ;
#416 = B_SPLINE_CURVE_WITH_KNOTS('',3,(#55817,#55818,#55819,#55820,#55821,
#55822,#55823,#55824,#55825,#55826,#55827,#55828,#55829,#55830,#55831,#55832,
#55833,#55834,#55835,#55836,#55837,#55838,#55839,#55840,#55841,#55842,#55843,
#55844,#55845,#55846,#55847,#55848,#55849,#55850,#55851,#55852,#55853,#55854,
#55855,#55856),.UNSPECIFIED.,.F.,.F.,(4,3,3,3,3,3,3,3,3,3,3,3,3,4),(5.14917238118991,
5.36005118608476,5.57092999109581,5.77298643029882,5.97546031432058,6.12802772885396,
6.32462027006761,6.52281590230618,6.6851254666121,6.88364627199035,7.08054113574733,
7.24221135774884,7.44474766140251,7.51426325158811),.UNSPECIFIED.) ;
#417 = B_SPLINE_CURVE_WITH_KNOTS('',3,(#55860,#55861,#55862,#55863,#55864,
#55865,#55866,#55867,#55868,#55869,#55870,#55871,#55872,#55873,#55874,#55875,
#55876,#55877,#55878,#55879,#55880,#55881,#55882,#55883,#55884,#55885,#55886,
#55887,#55888,#55889,#55890,#55891,#55892,#55893,#55894,#55895,#55896,#55897,
#55898,#55899),.UNSPECIFIED.,.F.,.F.,(4,3,3,3,3,3,3,3,3,3,3,3,3,4),(1.39920553665765,
1.60174184009056,1.6712576734102,1.86788901812072,2.06612241241829,2.22834356454694,
2.42682695741387,2.62368336398203,2.78544130230508,2.98797174735976,3.19010175291811,
3.34253904006323,3.55341784507432,3.76429664996928),.UNSPECIFIED.) ;
#418 = B_SPLINE_CURVE_WITH_KNOTS('',2,(#55901,#55902,#55903),
 .UNSPECIFIED.,.F.,.F.,(3,3),(0.,1.5050938596919),.UNSPECIFIED.) ;
#419 = B_SPLINE_CURVE_WITH_KNOTS('',2,(#55907,#55908,#55909),
 .UNSPECIFIED.,.F.,.F.,(3,3),(0.0815875961098428,1.58668145590164),
 .UNSPECIFIED.) ;
#420 = B_SPLINE_CURVE_WITH_KNOTS('',3,(#55911,#55912,#55913,#55914,#55915,
#55916,#55917,#55918,#55919,#55920,#55921,#55922,#55923,#55924,#55925,#55926,
#55927,#55928,#55929,#55930,#55931,#55932,#55933,#55934,#55935,#55936,#55937,
#55938,#55939,#55940,#55941,#55942,#55943,#55944,#55945,#55946,#55947,#55948,
#55949,#55950),.UNSPECIFIED.,.F.,.F.,(4,3,3,3,3,3,3,3,3,3,3,3,3,4),(5.14917238118964,
5.36005118608463,5.57092999109582,5.77298643029978,5.97546031432238,6.12802772885397,
6.32462027006883,6.52281590230841,6.68512546661211,6.88364627198785,7.0805411357423,
7.24221135774884,7.44474766118272,7.51426349450143),.UNSPECIFIED.) ;
#421 = B_SPLINE_CURVE_WITH_KNOTS('',3,(#55954,#55955,#55956,#55957,#55958,
#55959,#55960,#55961,#55962,#55963,#55964,#55965,#55966,#55967,#55968,#55969,
#55970,#55971,#55972,#55973,#55974,#55975,#55976,#55977,#55978,#55979,#55980,
#55981,#55982,#55983,#55984,#55985,#55986,#55987,#55988,#55989,#55990,#55991,
#55992,#55993),.UNSPECIFIED.,.F.,.F.,(4,3,3,3,3,3,3,3,3,3,3,3,3,4),(1.39920553665765,
1.60174184009242,1.6712576734102,1.86788901812178,2.0661224124197,2.22834356454693,
2.42682695741288,2.62368336398156,2.78544130230508,2.98797174735984,3.19010175291886,
3.34253904006323,3.55341784507438,3.76429664996941),.UNSPECIFIED.) ;
#422 = B_SPLINE_CURVE_WITH_KNOTS('',2,(#55995,#55996,#55997),
 .UNSPECIFIED.,.F.,.F.,(3,3),(0.,1.50509385942888),.UNSPECIFIED.) ;
#423 = B_SPLINE_CURVE_WITH_KNOTS('',2,(#56001,#56002,#56003),
 .UNSPECIFIED.,.F.,.F.,(3,3),(0.0815875966181519,1.58668145590164),
 .UNSPECIFIED.) ;
#424 = B_SPLINE_CURVE_WITH_KNOTS('',3,(#56005,#56006,#56007,#56008,#56009,
#56010,#56011,#56012,#56013,#56014,#56015,#56016,#56017,#56018,#56019,#56020,
#56021,#56022,#56023,#56024,#56025,#56026,#56027,#56028,#56029,#56030,#56031,
#56032,#56033,#56034,#56035,#56036,#56037,#56038,#56039,#56040,#56041,#56042,
#56043,#56044),.UNSPECIFIED.,.F.,.F.,(4,3,3,3,3,3,3,3,3,3,3,3,3,4),(5.1491723811896,
5.36005118608465,5.57092999109581,5.77298643029993,5.9754603143227,6.12802772885395,
6.32462027006869,6.52281590230835,6.6851254666121,6.88364627198907,7.08054113574468,
7.24221135774883,7.44474766118646,7.51426349450139),.UNSPECIFIED.) ;
#425 = B_SPLINE_CURVE_WITH_KNOTS('',3,(#56048,#56049,#56050,#56051,#56052,
#56053,#56054,#56055,#56056,#56057,#56058,#56059,#56060,#56061,#56062,#56063,
#56064,#56065,#56066,#56067,#56068,#56069,#56070,#56071,#56072,#56073,#56074,
#56075,#56076,#56077,#56078,#56079,#56080,#56081,#56082,#56083,#56084,#56085,
#56086,#56087),.UNSPECIFIED.,.F.,.F.,(4,3,3,3,3,3,3,3,3,3,3,3,3,4),(1.39920556389953,
1.60174186736169,1.6712576734102,1.86788901812329,2.06612241242289,2.22834356454693,
2.42682695741632,2.62368336398626,2.78544130230508,2.98797174736086,3.19010175292064,
3.34253904006322,3.55341784507414,3.76429664996872),.UNSPECIFIED.) ;
#426 = B_SPLINE_CURVE_WITH_KNOTS('',2,(#56089,#56090,#56091),
 .UNSPECIFIED.,.F.,.F.,(3,3),(0.,1.50509385902892),.UNSPECIFIED.) ;
#427 = B_SPLINE_CURVE_WITH_KNOTS('',2,(#56095,#56096,#56097),
 .UNSPECIFIED.,.F.,.F.,(3,3),(0.0815875968459406,1.58668145590164),
 .UNSPECIFIED.) ;
#428 = B_SPLINE_CURVE_WITH_KNOTS('',3,(#56099,#56100,#56101,#56102,#56103,
#56104,#56105,#56106,#56107,#56108,#56109,#56110,#56111,#56112,#56113,#56114,
#56115,#56116,#56117,#56118,#56119,#56120,#56121,#56122,#56123,#56124,#56125,
#56126,#56127,#56128,#56129,#56130,#56131,#56132,#56133,#56134,#56135,#56136,
#56137,#56138),.UNSPECIFIED.,.F.,.F.,(4,3,3,3,3,3,3,3,3,3,3,3,3,4),(5.14917238119049,
5.360051186085,5.57092999109581,5.77298643030171,5.97546031432617,6.12802772885396,
6.32462027007144,6.5228159023139,6.6851254666121,6.88364627198961,7.08054113574615,
7.24221135774884,7.44474766120728,7.51426346725953),.UNSPECIFIED.) ;
#429 = B_SPLINE_CURVE_WITH_KNOTS('',3,(#56142,#56143,#56144,#56145,#56146,
#56147,#56148,#56149,#56150,#56151,#56152,#56153,#56154,#56155,#56156,#56157,
#56158,#56159,#56160,#56161,#56162,#56163,#56164,#56165,#56166,#56167,#56168,
#56169,#56170,#56171,#56172,#56173,#56174,#56175,#56176,#56177,#56178,#56179,
#56180,#56181),.UNSPECIFIED.,.F.,.F.,(4,3,3,3,3,3,3,3,3,3,3,3,3,4),(1.39920580297372,
1.60174210665031,1.6712576734102,1.86788901812242,2.06612241242141,2.22834356454693,
2.42682695741471,2.6236833639841,2.78544130230508,2.98797174736084,3.19010175292033,
3.34253904006322,3.55341784507415,3.76429664996889),.UNSPECIFIED.) ;
#430 = B_SPLINE_CURVE_WITH_KNOTS('',2,(#56183,#56184,#56185),
 .UNSPECIFIED.,.F.,.F.,(3,3),(0.,1.50509385917405),.UNSPECIFIED.) ;
#431 = B_SPLINE_CURVE_WITH_KNOTS('',2,(#56189,#56190,#56191),
 .UNSPECIFIED.,.F.,.F.,(3,3),(0.0815875970104741,1.58668145590163),
 .UNSPECIFIED.) ;
#432 = B_SPLINE_CURVE_WITH_KNOTS('',3,(#56193,#56194,#56195,#56196,#56197,
#56198,#56199,#56200,#56201,#56202,#56203,#56204,#56205,#56206,#56207,#56208,
#56209,#56210,#56211,#56212,#56213,#56214,#56215,#56216,#56217,#56218,#56219,
#56220,#56221,#56222,#56223,#56224,#56225,#56226,#56227,#56228,#56229,#56230,
#56231,#56232),.UNSPECIFIED.,.F.,.F.,(4,3,3,3,3,3,3,3,3,3,3,3,3,4),(5.14917238118975,
5.36005118608465,5.57092999109581,5.77298643029957,5.97546031432202,6.12802772885396,
6.32462027006847,6.52281590230783,6.6851254666121,6.88364627198963,7.0805411357456,
7.24221135774883,7.44474766142264,7.51426322818531),.UNSPECIFIED.) ;
#433 = B_SPLINE_CURVE_WITH_KNOTS('',3,(#56236,#56237,#56238,#56239,#56240,
#56241,#56242,#56243,#56244,#56245,#56246,#56247,#56248,#56249,#56250,#56251,
#56252,#56253,#56254,#56255,#56256,#56257,#56258,#56259,#56260,#56261,#56262,
#56263,#56264,#56265,#56266,#56267,#56268,#56269,#56270,#56271,#56272,#56273,
#56274,#56275),.UNSPECIFIED.,.F.,.F.,(4,3,3,3,3,3,3,3,3,3,3,3,3,4),(1.39920578163109,
1.60174208528961,1.67125767341019,1.86788901812345,2.06612241242393,2.22834356454692,
2.42682695741443,2.62368336398346,2.78544130230507,2.98797174735876,3.1901017529163,
3.34253904006322,3.55341784507393,3.76429664996861),.UNSPECIFIED.) ;
#434 = B_SPLINE_CURVE_WITH_KNOTS('',2,(#56277,#56278,#56279),
 .UNSPECIFIED.,.F.,.F.,(3,3),(0.,1.50509385977447),.UNSPECIFIED.) ;
#435 = B_SPLINE_CURVE_WITH_KNOTS('',2,(#56283,#56284,#56285),
 .UNSPECIFIED.,.F.,.F.,(3,3),(0.0815875964822538,1.58668145590165),
 .UNSPECIFIED.) ;
#436 = B_SPLINE_CURVE_WITH_KNOTS('',3,(#56287,#56288,#56289,#56290,#56291,
#56292,#56293,#56294,#56295,#56296,#56297,#56298,#56299,#56300,#56301,#56302,
#56303,#56304,#56305,#56306,#56307,#56308,#56309,#56310,#56311,#56312,#56313,
#56314,#56315,#56316,#56317,#56318,#56319,#56320,#56321,#56322,#56323,#56324,
#56325,#56326),.UNSPECIFIED.,.F.,.F.,(4,3,3,3,3,3,3,3,3,3,3,3,3,4),(5.14917238119043,
5.36005118608505,5.5709299910958,5.77298643029934,5.97546031432166,6.12802772885395,
6.32462027006776,6.52281590230651,6.6851254666121,6.88364627199062,7.08054113574748,
7.24221135774883,7.44474766140304,7.51426324952791),.UNSPECIFIED.) ;
#437 = B_SPLINE_CURVE_WITH_KNOTS('',3,(#56330,#56331,#56332,#56333,#56334,
#56335,#56336,#56337,#56338,#56339,#56340,#56341,#56342,#56343,#56344,#56345,
#56346,#56347,#56348,#56349,#56350,#56351,#56352,#56353,#56354,#56355,#56356,
#56357,#56358,#56359,#56360,#56361,#56362,#56363,#56364,#56365,#56366,#56367,
#56368,#56369),.UNSPECIFIED.,.F.,.F.,(4,3,3,3,3,3,3,3,3,3,3,3,3,4),(1.39920580594635,
1.60174210962213,1.67125767341019,1.86788901812036,2.06612241241732,2.22834356454693,
2.42682695741494,2.62368336398253,2.78544130230507,2.98797174736146,3.1901017529218,
3.34253904006322,3.55341784507419,3.76429664996922),.UNSPECIFIED.) ;
#438 = B_SPLINE_CURVE_WITH_KNOTS('',2,(#56371,#56372,#56373),
 .UNSPECIFIED.,.F.,.F.,(3,3),(0.,1.50509385953119),.UNSPECIFIED.) ;
#439 = B_SPLINE_CURVE_WITH_KNOTS('',2,(#56377,#56378,#56379),
 .UNSPECIFIED.,.F.,.F.,(3,3),(0.0815875961704467,1.58668145590162),
 .UNSPECIFIED.) ;
#440 = B_SPLINE_CURVE_WITH_KNOTS('',3,(#56381,#56382,#56383,#56384,#56385,
#56386,#56387,#56388,#56389,#56390,#56391,#56392,#56393,#56394,#56395,#56396,
#56397,#56398,#56399,#56400,#56401,#56402,#56403,#56404,#56405,#56406,#56407,
#56408,#56409,#56410,#56411,#56412,#56413,#56414,#56415,#56416,#56417,#56418,
#56419,#56420),.UNSPECIFIED.,.F.,.F.,(4,3,3,3,3,3,3,3,3,3,3,3,3,4),(5.14917238118979,
5.3600511860848,5.57092999109581,5.77298643029889,5.97546031432064,6.12802772885396,
6.32462027006939,6.52281590230972,6.6851254666121,6.88364627198858,7.08054113574403,
7.24221135774883,7.44474766142492,7.51426322521266),.UNSPECIFIED.) ;
#441 = B_SPLINE_CURVE_WITH_KNOTS('',3,(#56424,#56425,#56426,#56427,#56428,
#56429,#56430,#56431,#56432,#56433,#56434,#56435,#56436,#56437,#56438,#56439,
#56440,#56441,#56442,#56443,#56444,#56445,#56446,#56447,#56448,#56449,#56450,
#56451,#56452,#56453,#56454,#56455,#56456,#56457,#56458,#56459,#56460,#56461,
#56462,#56463),.UNSPECIFIED.,.F.,.F.,(4,3,3,3,3,3,3,3,3,3,3,3,3,4),(1.39920554734762,
1.60174185079261,1.6712576734102,1.86788901812075,2.06612241241815,2.22834356454693,
2.42682695741446,2.62368336398269,2.78544130230508,2.9879717473577,3.19010175291388,
3.34253904006322,3.5534178450744,3.76429664996949),.UNSPECIFIED.) ;
#442 = B_SPLINE_CURVE_WITH_KNOTS('',2,(#56465,#56466,#56467),
 .UNSPECIFIED.,.F.,.F.,(3,3),(0.,1.50509385944905),.UNSPECIFIED.) ;
#443 = B_SPLINE_CURVE_WITH_KNOTS('',2,(#56471,#56472,#56473),
 .UNSPECIFIED.,.F.,.F.,(3,3),(0.0815875965531534,1.58668145590162),
 .UNSPECIFIED.) ;
#444 = B_SPLINE_CURVE_WITH_KNOTS('',3,(#56475,#56476,#56477,#56478,#56479,
#56480,#56481,#56482,#56483,#56484,#56485,#56486,#56487,#56488,#56489,#56490,
#56491,#56492,#56493,#56494,#56495,#56496,#56497,#56498,#56499,#56500,#56501,
#56502,#56503,#56504,#56505,#56506,#56507,#56508,#56509,#56510,#56511,#56512,
#56513,#56514),.UNSPECIFIED.,.F.,.F.,(4,3,3,3,3,3,3,3,3,3,3,3,3,4),(5.14917238118972,
5.36005118608473,5.57092999109581,5.77298643029944,5.97546031432173,6.12802772885396,
6.32462027006809,6.52281590230707,6.6851254666121,6.88364627198843,7.08054113574374,
7.24221135774884,7.44474766119369,7.51426348381143),.UNSPECIFIED.) ;
#445 = B_SPLINE_CURVE_WITH_KNOTS('',3,(#56518,#56519,#56520,#56521,#56522,
#56523,#56524,#56525,#56526,#56527,#56528,#56529,#56530,#56531,#56532,#56533,
#56534,#56535,#56536,#56537,#56538,#56539,#56540,#56541,#56542,#56543,#56544,
#56545,#56546,#56547,#56548,#56549,#56550,#56551,#56552,#56553,#56554,#56555,
#56556,#56557),.UNSPECIFIED.,.F.,.F.,(4,3,3,3,3,3,3,3,3,3,3,3,3,4),(1.39920553665764,
1.60174184009116,1.6712576734102,1.86788901812116,2.06612241241911,2.22834356454693,
2.42682695741597,2.62368336398584,2.78544130230508,2.98797174735932,3.19010175291758,
3.34253904006323,3.55341784507458,3.76429664996967),.UNSPECIFIED.) ;
#446 = B_SPLINE_CURVE_WITH_KNOTS('',2,(#56559,#56560,#56561),
 .UNSPECIFIED.,.F.,.F.,(3,3),(0.,1.50509385946355),.UNSPECIFIED.) ;
#447 = B_SPLINE_CURVE_WITH_KNOTS('',2,(#56565,#56566,#56567),
 .UNSPECIFIED.,.F.,.F.,(3,3),(0.0815875966540559,1.58668145590163),
 .UNSPECIFIED.) ;
#448 = B_SPLINE_CURVE_WITH_KNOTS('',3,(#56569,#56570,#56571,#56572,#56573,
#56574,#56575,#56576,#56577,#56578,#56579,#56580,#56581,#56582,#56583,#56584,
#56585,#56586,#56587,#56588,#56589,#56590,#56591,#56592,#56593,#56594,#56595,
#56596,#56597,#56598,#56599,#56600,#56601,#56602,#56603,#56604,#56605,#56606,
#56607,#56608),.UNSPECIFIED.,.F.,.F.,(4,3,3,3,3,3,3,3,3,3,3,3,3,4),(5.14917238118944,
5.36005118608449,5.57092999109581,5.77298643029889,5.97546031432065,6.12802772885396,
6.32462027006934,6.52281590230941,6.68512546661211,6.88364627198978,7.08054113574635,
7.24221135774884,7.4447476611834,7.51426349450135),.UNSPECIFIED.) ;
#449 = B_SPLINE_CURVE_WITH_KNOTS('',3,(#56616,#56617,#56618,#56619,#56620,
#56621,#56622,#56623,#56624,#56625,#56626,#56627,#56628,#56629,#56630,#56631,
#56632,#56633,#56634,#56635,#56636,#56637),.UNSPECIFIED.,.F.,.F.,(4,2,2,
2,2,2,2,2,2,2,4),(5.27191149550306E-6,0.0527078513361115,6.45340679863479,
7.10706620105005,7.54824310354326,7.76072560346531,7.78191476646708,7.79349134258084,
7.79962401028583,7.80184798817142,7.80203371562736),.UNSPECIFIED.) ;
#450 = B_SPLINE_CURVE_WITH_KNOTS('',3,(#56640,#56641,#56642,#56643,#56644,
#56645,#56646,#56647,#56648,#56649),.UNSPECIFIED.,.F.,.F.,(4,2,2,2,4),(7.80221259693202,
7.80241711061396,7.80965893536248,8.08890869992909,13.8149316250846),
 .UNSPECIFIED.) ;
#451 = B_SPLINE_CURVE_WITH_KNOTS('',3,(#56653,#56654,#56655,#56656,#56657,
#56658,#56659,#56660,#56661,#56662,#56663,#56664,#56665,#56666,#56667,#56668,
#56669,#56670,#56671,#56672,#56673,#56674),.UNSPECIFIED.,.F.,.F.,(4,2,2,
2,2,2,2,2,2,2,4),(5.27191148509523E-6,0.0465537949478901,6.44830136700651,
7.10264046407999,7.54412371933544,7.75697956115347,7.7781894765911,7.78977015010294,
7.79592806966615,7.79819769958458,7.79836756459383),.UNSPECIFIED.) ;
#452 = B_SPLINE_CURVE_WITH_KNOTS('',3,(#56677,#56678,#56679,#56680,#56681,
#56682,#56683,#56684,#56685,#56686,#56687,#56688),.UNSPECIFIED.,.F.,.F.,
(4,2,2,2,2,4),(7.79863737329538,7.79879895211581,7.811727333517,8.2183177167418,
17.3378811428621,58.4300224110889),.UNSPECIFIED.) ;
#453 = B_SPLINE_CURVE_WITH_KNOTS('',3,(#56692,#56693,#56694,#56695,#56696,
#56697,#56698,#56699,#56700,#56701,#56702,#56703,#56704,#56705,#56706,#56707,
#56708,#56709,#56710,#56711,#56712,#56713),.UNSPECIFIED.,.F.,.F.,(4,2,2,
2,2,2,2,2,2,2,4),(5.27191158905907E-6,0.0396446874731099,6.43885097308755,
7.09357142809069,7.53514148843079,7.74829188309382,7.76951301811614,7.78108926141565,
7.78727446991383,7.78888160161461,7.78890865002446),.UNSPECIFIED.) ;
#454 = B_SPLINE_CURVE_WITH_KNOTS('',3,(#56716,#56717,#56718,#56719,#56720,
#56721,#56722,#56723,#56724,#56725),.UNSPECIFIED.,.F.,.F.,(4,2,2,2,4),(7.78895653301216,
7.78900494242095,7.79222894606557,7.8726852687626,8.96203806139483),
 .UNSPECIFIED.) ;
#455 = B_SPLINE_CURVE_WITH_KNOTS('',3,(#56729,#56730,#56731,#56732,#56733,
#56734,#56735,#56736,#56737,#56738,#56739,#56740,#56741,#56742,#56743,#56744,
#56745,#56746,#56747,#56748,#56749,#56750),.UNSPECIFIED.,.F.,.F.,(4,2,2,
2,2,2,2,2,2,2,4),(5.27191189062319E-6,0.0355022021223558,6.44121530656163,
7.0969892443639,7.53916678802634,7.75276318216616,7.77401784522417,7.78560516000671,
7.79181523099173,7.79344311532259,7.79346999485175),.UNSPECIFIED.) ;
#456 = B_SPLINE_CURVE_WITH_KNOTS('',3,(#56753,#56754,#56755,#56756,#56757,
#56758,#56759,#56760,#56761,#56762,#56763,#56764),.UNSPECIFIED.,.F.,.F.,
(4,2,2,2,2,4),(7.79352661259234,7.79358342104345,7.80166819041049,7.90391945213033,
10.5115157415884,22.7185743110134),.UNSPECIFIED.) ;
#457 = B_SPLINE_CURVE_WITH_KNOTS('',3,(#56768,#56769,#56770,#56771,#56772,
#56773,#56774,#56775,#56776,#56777,#56778,#56779,#56780,#56781,#56782,#56783,
#56784,#56785,#56786,#56787,#56788,#56789),.UNSPECIFIED.,.F.,.F.,(4,2,2,
2,2,2,2,2,2,2,4),(5.27191147638787E-6,0.0377827332366595,6.43903319305708,
7.0941366968806,7.5359188939874,7.74924020070412,7.77047347261814,7.78205309254291,
7.78824859694197,7.78986477823942,7.78989191787037),.UNSPECIFIED.) ;
#458 = B_SPLINE_CURVE_WITH_KNOTS('',3,(#56792,#56793,#56794,#56795,#56796,
#56797,#56798,#56799,#56800,#56801),.UNSPECIFIED.,.F.,.F.,(4,2,2,2,4),(7.78996291674499,
7.7900243542677,7.79393765773531,7.88810518975087,9.08002513845262),
 .UNSPECIFIED.) ;
#459 = B_SPLINE_CURVE_WITH_KNOTS('',3,(#56805,#56806,#56807,#56808,#56809,
#56810,#56811,#56812,#56813,#56814,#56815,#56816,#56817,#56818,#56819,#56820,
#56821,#56822,#56823,#56824,#56825,#56826),.UNSPECIFIED.,.F.,.F.,(4,2,2,
2,2,2,2,2,2,2,4),(5.27191138067076E-6,0.0449461593234226,6.44633404502776,
7.1007856663008,7.54230514096117,7.75523728757385,7.77645054559184,7.78803083691326,
7.79419520281166,7.79647958901679,7.79664367287054),.UNSPECIFIED.) ;
#460 = B_SPLINE_CURVE_WITH_KNOTS('',3,(#56829,#56830,#56831,#56832,#56833,
#56834,#56835,#56836,#56837,#56838,#56839,#56840,#56841,#56842,#56843,#56844,
#56845,#56846,#56847,#56848,#56849,#56850,#56851,#56852,#56853,#56854,#56855,
#56856),.UNSPECIFIED.,.F.,.F.,(4,3,3,3,3,3,3,3,3,4),(7.79681765090147,7.79693246333981,
7.80264593101425,7.80335304330589,7.86482173740273,8.71154800799036,9.74463365376269,
10.2896549353898,22.5136531132542,24.4500364531805),.UNSPECIFIED.) ;
#461 = B_SPLINE_CURVE_WITH_KNOTS('',3,(#56860,#56861,#56862,#56863,#56864,
#56865,#56866,#56867,#56868,#56869,#56870,#56871,#56872,#56873,#56874,#56875,
#56876,#56877,#56878,#56879,#56880,#56881),.UNSPECIFIED.,.F.,.F.,(4,2,2,
2,2,2,2,2,2,2,4),(5.27191147799299E-6,0.0511073819017907,6.45440150746996,
7.10847604594555,7.54989318912631,7.76255058442115,7.78375285138069,7.79533495417965,
7.80147593136055,7.80371064912123,7.80389282491498),.UNSPECIFIED.) ;
#462 = B_SPLINE_CURVE_WITH_KNOTS('',3,(#56884,#56885,#56886,#56887,#56888,
#56889,#56890,#56891,#56892,#56893),.UNSPECIFIED.,.F.,.F.,(4,2,2,2,4),(7.80438554879021,
7.80496076768678,7.83948451539625,8.84807105865867,29.8486833513606),
 .UNSPECIFIED.) ;
#463 = B_SPLINE_CURVE_WITH_KNOTS('',3,(#56897,#56898,#56899,#56900,#56901,
#56902,#56903,#56904,#56905,#56906,#56907,#56908,#56909,#56910,#56911,#56912,
#56913,#56914,#56915,#56916,#56917,#56918),.UNSPECIFIED.,.F.,.F.,(4,2,2,
2,2,2,2,2,2,2,4),(5.27191166391327E-6,0.0525380308481434,6.45668644422429,
7.11071566703238,7.55213750314294,7.76474488984048,7.78594601623854,7.79752901314693,
7.80366549802474,7.8058915856127,7.80609162294199),.UNSPECIFIED.) ;
#464 = B_SPLINE_CURVE_WITH_KNOTS('',3,(#56921,#56922,#56923,#56924,#56925,
#56926,#56927,#56928,#56929,#56930,#56931,#56932),.UNSPECIFIED.,.F.,.F.,
(4,2,2,2,2,4),(7.80644056341581,7.80682262141797,7.85814957526539,8.49497231289726,
25.6284091705695,104.059811221683),.UNSPECIFIED.) ;
#465 = B_SPLINE_CURVE_WITH_KNOTS('',3,(#56938,#56939,#56940,#56941,#56942,
#56943,#56944,#56945,#56946,#56947,#56948,#56949,#56950,#56951,#56952,#56953,
#56954,#56955,#56956,#56957,#56958,#56959),.UNSPECIFIED.,.F.,.F.,(4,2,2,
2,2,2,2,2,2,2,4),(5.27191148216978E-6,0.0414743981847573,6.44013831362117,
7.09463297986845,7.53609600585336,7.74912764611573,7.77034174576342,7.78191720208803,
7.78809369888862,7.78969224195007,7.78972443835406),.UNSPECIFIED.) ;
#466 = B_SPLINE_CURVE_WITH_KNOTS('',3,(#56962,#56963,#56964,#56965,#56966,
#56967,#56968,#56969,#56970,#56971),.UNSPECIFIED.,.F.,.F.,(4,2,2,2,4),(7.78977667487699,
7.78981377673323,7.79239024212666,7.85784828520671,8.78134693044458),
 .UNSPECIFIED.) ;
#467 = B_SPLINE_CURVE_WITH_KNOTS('',3,(#56975,#56976,#56977,#56978,#56979,
#56980,#56981,#56982,#56983,#56984,#56985,#56986,#56987,#56988,#56989,#56990,
#56991,#56992,#56993,#56994,#56995,#56996),.UNSPECIFIED.,.F.,.F.,(4,2,2,
2,2,2,2,2,2,2,4),(5.27191166871522E-6,0.0356514515568032,6.43942015127324,
7.0949804845643,7.53701786178047,7.75054081785537,7.77178857574933,7.78337224535537,
7.78957964075273,7.79120607196549,7.79123706466225),.UNSPECIFIED.) ;
#468 = B_SPLINE_CURVE_WITH_KNOTS('',3,(#56999,#57000,#57001,#57002,#57003,
#57004,#57005,#57006,#57007,#57008,#57009,#57010,#57011,#57012,#57013,#57014),
 .UNSPECIFIED.,.F.,.F.,(4,2,2,2,2,2,2,4),(7.79128432176965,7.79131403753904,
7.79508710279556,7.83622558772195,8.30441129116172,8.8671118434176,9.28957449106967,
15.1690241021115),.UNSPECIFIED.) ;
#469 = B_SPLINE_CURVE_WITH_KNOTS('',3,(#57018,#57019,#57020,#57021,#57022,
#57023,#57024,#57025,#57026,#57027,#57028,#57029,#57030,#57031,#57032,#57033,
#57034,#57035,#57036,#57037,#57038,#57039),.UNSPECIFIED.,.F.,.F.,(4,2,2,
2,2,2,2,2,2,2,4),(5.27191151498337E-6,0.0359657639257141,6.43915849273793,
7.09463043773541,7.53661602976181,7.7501023827329,7.77134728693642,7.78293006298598,
7.78913549825155,7.79076040490507,7.79078675221503),.UNSPECIFIED.) ;
#470 = B_SPLINE_CURVE_WITH_KNOTS('',3,(#57042,#57043,#57044,#57045,#57046,
#57047,#57048,#57049,#57050,#57051,#57052,#57053),.UNSPECIFIED.,.F.,.F.,
(4,2,2,2,2,4),(7.79083814663995,7.79089463150174,7.79821119965064,7.89001115859904,
10.2475238105046,21.2881958971545),.UNSPECIFIED.) ;
#471 = B_SPLINE_CURVE_WITH_KNOTS('',3,(#57057,#57058,#57059,#57060,#57061,
#57062,#57063,#57064,#57065,#57066,#57067,#57068,#57069,#57070,#57071,#57072,
#57073,#57074,#57075,#57076,#57077,#57078),.UNSPECIFIED.,.F.,.F.,(4,2,2,
2,2,2,2,2,2,2,4),(5.2719118637948E-6,0.0432725905166975,6.44833055008626,
7.10331460056981,7.54515147355067,7.75829865105336,7.77952893588274,7.79111596175757,
7.79729100354606,7.79959341946853,7.79979287868427),.UNSPECIFIED.) ;
#472 = B_SPLINE_CURVE_WITH_KNOTS('',3,(#57081,#57082,#57083,#57084,#57085,
#57086,#57087,#57088,#57089,#57090),.UNSPECIFIED.,.F.,.F.,(4,2,2,2,4),(7.80028431507407,
7.80069015909249,7.83056852627773,8.69977922056581,21.3113858823424),
 .UNSPECIFIED.) ;
#473 = B_SPLINE_CURVE_WITH_KNOTS('',3,(#57096,#57097,#57098,#57099,#57100,
#57101,#57102,#57103,#57104,#57105,#57106,#57107,#57108,#57109,#57110,#57111,
#57112,#57113,#57114,#57115,#57116,#57117),.UNSPECIFIED.,.F.,.F.,(4,2,2,
2,2,2,2,2,2,2,4),(5.27191168534313E-6,0.0523927874971037,6.45501410063101,
7.10890009251696,7.55022187180551,7.7627860844029,7.78398255234983,7.79556279674482,
7.80169848168718,7.80392514223319,7.8041092694236),.UNSPECIFIED.) ;
#474 = B_SPLINE_CURVE_WITH_KNOTS('',3,(#57120,#57121,#57122,#57123,#57124,
#57125,#57126,#57127,#57128,#57129,#57130,#57131),.UNSPECIFIED.,.F.,.F.,
(4,2,2,2,2,4),(7.80477126540197,7.80558521468643,7.91497253507506,9.27554144510681,
45.7162452587849,212.471335771752),.UNSPECIFIED.) ;
#475 = B_SPLINE_CURVE_WITH_KNOTS('',3,(#57135,#57136,#57137,#57138,#57139,
#57140,#57141,#57142,#57143,#57144,#57145,#57146,#57147,#57148,#57149,#57150,
#57151,#57152,#57153,#57154,#57155,#57156,#57157,#57158,#57159,#57160),
 .UNSPECIFIED.,.F.,.F.,(4,2,2,2,2,2,2,2,2,2,2,2,4),(5.27191148861508E-6,
1.47097891395074,5.75978232176541,6.40361086116478,6.48988083888239,7.03787277637638,
7.49650945099211,7.54247660519179,7.67353711320395,7.75556392091874,7.78274835154569,
7.79406144395684,7.80522308440679),.UNSPECIFIED.) ;
#476 = B_SPLINE_CURVE_WITH_KNOTS('',3,(#57163,#57164,#57165,#57166,#57167,
#57168,#57169,#57170,#57171,#57172,#57173,#57174,#57175,#57176,#57177,#57178,
#57179,#57180,#57181,#57182),.UNSPECIFIED.,.F.,.F.,(4,2,2,2,2,2,2,2,2,4),
(7.80522308440679,7.80979087307447,8.2018949531721,9.24780316434757,9.79842768307673,
10.2918952776785,43.49970799473,58.02812605844,60.3284654325973,275.954206920472),
 .UNSPECIFIED.) ;
#477 = B_SPLINE_CURVE_WITH_KNOTS('',3,(#57186,#57187,#57188,#57189,#57190,
#57191,#57192,#57193,#57194,#57195,#57196,#57197,#57198,#57199,#57200,#57201,
#57202,#57203,#57204,#57205,#57206,#57207),.UNSPECIFIED.,.F.,.F.,(4,2,2,
2,2,2,2,2,2,2,4),(5.27191187477842E-6,0.0432725252097352,6.44831604470414,
7.1032986187713,7.54513449628265,7.75828119283847,7.77951138720516,7.79109852155536,
7.79727326708117,7.79957524268641,7.79974556459194),.UNSPECIFIED.) ;
#478 = B_SPLINE_CURVE_WITH_KNOTS('',3,(#57210,#57211,#57212,#57213,#57214,
#57215,#57216,#57217,#57218,#57219),.UNSPECIFIED.,.F.,.F.,(4,2,2,2,4),(7.79995524677398,
7.80010024939709,7.81075911559854,8.12013970698806,12.6093269820519),
 .UNSPECIFIED.) ;
#479 = B_SPLINE_CURVE_WITH_KNOTS('',3,(#57223,#57224,#57225,#57226,#57227,
#57228,#57229,#57230,#57231,#57232,#57233,#57234,#57235,#57236,#57237,#57238,
#57239,#57240,#57241,#57242,#57243,#57244),.UNSPECIFIED.,.F.,.F.,(4,2,2,
2,2,2,2,2,2,2,4),(5.271912279136E-6,0.0359879560292855,6.44510187443905,
7.10117994822179,7.54357425347277,7.75725802200454,7.77852259826938,7.79011608262715,
7.7963274350803,7.79795412309629,7.79798119670788),.UNSPECIFIED.) ;
#480 = B_SPLINE_CURVE_WITH_KNOTS('',3,(#57247,#57248,#57249,#57250,#57251,
#57252,#57253,#57254,#57255,#57256,#57257,#57258),.UNSPECIFIED.,.F.,.F.,
(4,2,2,2,2,4),(7.79803620397162,7.79809114082297,7.80515926793939,7.89384206027351,
10.1712995690942,20.8370576609684),.UNSPECIFIED.) ;
#481 = B_SPLINE_CURVE_WITH_KNOTS('',3,(#57262,#57263,#57264,#57265,#57266,
#57267,#57268,#57269,#57270,#57271,#57272,#57273,#57274,#57275,#57276,#57277,
#57278,#57279,#57280,#57281,#57282,#57283),.UNSPECIFIED.,.F.,.F.,(4,2,2,
2,2,2,2,2,2,2,4),(5.27191168080902E-6,0.0356505571059927,6.43917854529716,
7.0947142369843,7.5367349984191,7.75024992867144,7.77149687789579,7.78308023607464,
7.78928745150985,7.79091398242415,7.79094393251091),.UNSPECIFIED.) ;
#482 = B_SPLINE_CURVE_WITH_KNOTS('',3,(#57286,#57287,#57288,#57289,#57290,
#57291,#57292,#57293,#57294,#57295,#57296,#57297),.UNSPECIFIED.,.F.,.F.,
(4,2,2,2,2,4),(7.79100926174046,7.79108071178542,7.80013022621495,7.91427990087799,
10.8320810124655,24.4930959714559),.UNSPECIFIED.) ;
#483 = B_SPLINE_CURVE_WITH_KNOTS('',3,(#57301,#57302,#57303,#57304,#57305,
#57306,#57307,#57308,#57309,#57310,#57311,#57312,#57313,#57314,#57315,#57316,
#57317,#57318,#57319,#57320,#57321,#57322),.UNSPECIFIED.,.F.,.F.,(4,2,2,
2,2,2,2,2,2,2,4),(5.27191187344555E-6,0.0415033517824493,6.44685814573985,
7.10203719509694,7.54395170849138,7.75721624445404,7.77845257041729,7.79004012437634,
7.79622326565104,7.79782372936473,7.79785623932904),.UNSPECIFIED.) ;
#484 = B_SPLINE_CURVE_WITH_KNOTS('',3,(#57325,#57326,#57327,#57328,#57329,
#57330,#57331,#57332,#57333,#57334,#57335,#57336,#57337,#57338,#57339,#57340,
#57341,#57342),.UNSPECIFIED.,.F.,.F.,(4,2,2,2,2,2,2,2,4),(7.79793150207117,
7.79814723346125,7.79870043059623,7.80649383530305,7.89256327609095,7.99478803002891,
8.06034762858735,9.28573631573981,9.36839839072109),.UNSPECIFIED.) ;
#485 = B_SPLINE_CURVE_WITH_KNOTS('',3,(#57346,#57347,#57348,#57349,#57350,
#57351,#57352,#57353,#57354,#57355,#57356,#57357,#57358,#57359,#57360,#57361,
#57362,#57363,#57364,#57365,#57366,#57367,#57368,#57369,#57370,#57371,#57372,
#57373),.UNSPECIFIED.,.F.,.F.,(4,2,2,2,1,2,2,2,2,2,2,2,2,1,4),(5.27191159103619E-6,
1.04820808125431,4.7657172239378,5.66605146943146,6.11270166153183,6.41832688046243,
6.4954431947857,7.09297306404379,7.38226395613211,7.6384860640954,7.75703692454204,
7.78060543766242,7.79405002558409,7.79920996916132,7.80436991273856),
 .UNSPECIFIED.) ;
#486 = B_SPLINE_CURVE_WITH_KNOTS('',3,(#57376,#57377,#57378,#57379,#57380,
#57381,#57382,#57383,#57384,#57385,#57386,#57387,#57388,#57389,#57390,#57391,
#57392,#57393),.UNSPECIFIED.,.F.,.F.,(4,2,2,2,2,2,2,2,4),(7.80436991273856,
7.80474232030115,7.88242710709233,8.75841205662384,8.96393995438549,22.8445100409781,
28.9172594538623,29.9482351239262,120.00842073875),.UNSPECIFIED.) ;
#487 = B_SPLINE_CURVE_WITH_KNOTS('',3,(#57397,#57398,#57399,#57400,#57401,
#57402,#57403,#57404,#57405,#57406,#57407,#57408,#57409,#57410,#57411,#57412,
#57413,#57414,#57415,#57416,#57417,#57418),.UNSPECIFIED.,.F.,.F.,(4,2,2,
2,2,2,2,2,2,2,4),(5.2719118122293E-6,0.0525432957185552,6.45765275965806,
7.11178013090022,7.55326821002014,7.76590750214238,7.78711180679313,7.79869646853999,
7.80483393332087,7.80706039962179,7.80724567724711),.UNSPECIFIED.) ;
#488 = B_SPLINE_CURVE_WITH_KNOTS('',3,(#57421,#57422,#57423,#57424,#57425,
#57426,#57427,#57428,#57429,#57430,#57431,#57432),.UNSPECIFIED.,.F.,.F.,
(4,2,2,2,2,4),(7.80754124133301,7.80785818194975,7.8504276541488,8.37868320530173,
22.5834113324897,87.6053326518759),.UNSPECIFIED.) ;
#489 = B_SPLINE_CURVE_WITH_KNOTS('',3,(#57436,#57437,#57438,#57439,#57440,
#57441,#57442,#57443,#57444,#57445,#57446,#57447,#57448,#57449,#57450,#57451,
#57452,#57453,#57454,#57455,#57456,#57457),.UNSPECIFIED.,.F.,.F.,(4,2,2,
2,2,2,2,2,2,2,4),(5.27191176710306E-6,0.0511111946987736,6.45512057751185,
7.10926817712045,7.55073462661806,7.76341577672905,7.78462040594282,7.79620374455683,
7.80234564099213,7.80458100357878,7.80476406937864),.UNSPECIFIED.) ;
#490 = B_SPLINE_CURVE_WITH_KNOTS('',3,(#57460,#57461,#57462,#57463,#57464,
#57465,#57466,#57467,#57468,#57469),.UNSPECIFIED.,.F.,.F.,(4,2,2,2,4),(7.80523453137563,
7.80581761661808,7.84080868875818,8.86305145409338,30.1478164970341),
 .UNSPECIFIED.) ;
#491 = B_SPLINE_CURVE_WITH_KNOTS('',3,(#57473,#57474,#57475,#57476,#57477,
#57478,#57479,#57480,#57481,#57482,#57483,#57484,#57485,#57486,#57487,#57488,
#57489,#57490,#57491,#57492,#57493,#57494),.UNSPECIFIED.,.F.,.F.,(4,2,2,
2,2,2,2,2,2,2,4),(5.27191169017701E-6,0.0449566642310049,6.44858512306242,
7.10326581171296,7.54493982518336,7.7579465003635,7.77916725766819,7.7907515857637,
7.79691817502006,7.79920352721897,7.7993673461476),.UNSPECIFIED.) ;
#492 = B_SPLINE_CURVE_WITH_KNOTS('',3,(#57497,#57498,#57499,#57500,#57501,
#57502,#57503,#57504,#57505,#57506,#57507,#57508),.UNSPECIFIED.,.F.,.F.,
(4,2,2,2,2,4),(7.79964068154672,7.79984266942381,7.81523993495469,8.180553028938,
16.1414183538315,51.9114717465994),.UNSPECIFIED.) ;
#493 = B_SPLINE_CURVE_WITH_KNOTS('',3,(#57512,#57513,#57514,#57515,#57516,
#57517,#57518,#57519,#57520,#57521,#57522,#57523,#57524,#57525,#57526,#57527,
#57528,#57529,#57530,#57531,#57532,#57533),.UNSPECIFIED.,.F.,.F.,(4,2,2,
2,2,2,2,2,2,2,4),(5.27191157823416E-6,0.0377812881750992,6.43866511053677,
7.09373109278456,7.53548798669349,7.74879707503235,7.77002911215379,7.78160814123601,
7.78780327656431,7.78941938430865,7.78944792551213),.UNSPECIFIED.) ;
#494 = B_SPLINE_CURVE_WITH_KNOTS('',3,(#57536,#57537,#57538,#57539,#57540,
#57541,#57542,#57543,#57544,#57545),.UNSPECIFIED.,.F.,.F.,(4,2,2,2,4),(7.78950417221257,
7.78954999296874,7.79247137180975,7.86278869254345,8.75285890777793),
 .UNSPECIFIED.) ;
#495 = B_SPLINE_CURVE_WITH_KNOTS('',3,(#57549,#57550,#57551,#57552,#57553,
#57554,#57555,#57556,#57557,#57558,#57559,#57560,#57561,#57562,#57563,#57564,
#57565,#57566,#57567,#57568,#57569,#57570),.UNSPECIFIED.,.F.,.F.,(4,2,2,
2,2,2,2,2,2,2,4),(5.27191169046416E-6,0.0354948744565003,6.43922713707928,
7.09479828954679,7.53683909853423,7.7503694420143,7.77161751967803,7.78320124737355,
7.78940924098477,7.79103637023299,7.7910624807489),.UNSPECIFIED.) ;
#496 = B_SPLINE_CURVE_WITH_KNOTS('',3,(#57573,#57574,#57575,#57576,#57577,
#57578,#57579,#57580,#57581,#57582,#57583,#57584),.UNSPECIFIED.,.F.,.F.,
(4,2,2,2,2,4),(7.79111289413845,7.79116616933223,7.79788554663789,7.88286765791431,
10.0499826184928,20.1949747619141),.UNSPECIFIED.) ;
#497 = B_SPLINE_CURVE_WITH_KNOTS('',3,(#57588,#57589,#57590,#57591,#57592,
#57593,#57594,#57595,#57596,#57597,#57598,#57599,#57600,#57601,#57602,#57603,
#57604,#57605,#57606,#57607,#57608,#57609),.UNSPECIFIED.,.F.,.F.,(4,2,2,
2,2,2,2,2,2,2,4),(5.27191168177523E-6,0.0396625350310654,6.443183559499,
7.09834546596198,7.54021325882577,7.75350737242496,7.77474277060722,7.78632676826843,
7.79251614782254,7.7941243263727,7.79415422696317),.UNSPECIFIED.) ;
#498 = B_SPLINE_CURVE_WITH_KNOTS('',3,(#57612,#57613,#57614,#57615,#57616,
#57617,#57618,#57619,#57620,#57621),.UNSPECIFIED.,.F.,.F.,(4,2,2,2,4),(7.794199587327,
7.7942340932038,7.79653236739817,7.85378276088928,8.62896774962984),
 .UNSPECIFIED.) ;
#499 = B_SPLINE_CURVE_WITH_KNOTS('',3,(#57625,#57626,#57627,#57628,#57629,
#57630,#57631,#57632,#57633,#57634,#57635,#57636,#57637,#57638,#57639,#57640,
#57641,#57642,#57643,#57644,#57645,#57646),.UNSPECIFIED.,.F.,.F.,(4,2,2,
2,2,2,2,2,2,2,4),(5.2719115819804E-6,0.0465604352314907,6.44967554861822,
7.10415442622451,7.54573199163219,7.75863330383081,7.7798478022043,7.79143103500224,
7.79759014313736,7.79986010495208,7.80003908106863),.UNSPECIFIED.) ;
#500 = B_SPLINE_CURVE_WITH_KNOTS('',3,(#57649,#57650,#57651,#57652,#57653,
#57654,#57655,#57656,#57657,#57658,#57659,#57660),.UNSPECIFIED.,.F.,.F.,
(4,2,2,2,2,4),(7.80029559813691,7.80047746006334,7.81505666974208,8.27340780924998,
18.5539386231002,64.8773239617285),.UNSPECIFIED.) ;
#501 = B_SPLINE_CURVE_WITH_KNOTS('',3,(#57664,#57665,#57666,#57667,#57668,
#57669,#57670,#57671,#57672,#57673,#57674,#57675,#57676,#57677,#57678,#57679,
#57680,#57681,#57682,#57683,#57684,#57685),.UNSPECIFIED.,.F.,.F.,(4,2,2,
2,2,2,2,2,2,2,4),(5.27191148200324E-6,0.0527129873805481,6.45434578160439,
7.10810055256914,7.54934182256476,7.76185532353388,7.78304756105929,7.79462588360834,
7.8007593731596,7.8029837332684,7.80317840349864),.UNSPECIFIED.) ;
#502 = B_SPLINE_CURVE_WITH_KNOTS('',3,(#57688,#57689,#57690,#57691,#57692,
#57693,#57694,#57695,#57696,#57697,#57698,#57699),.UNSPECIFIED.,.F.,.F.,
(4,2,2,2,2,4),(7.80373274627093,7.80444564896149,7.9001288190428,9.08312630466139,
41.1183452310278,187.839302386062),.UNSPECIFIED.) ;
#503 = B_SPLINE_CURVE_WITH_KNOTS('',3,(#57702,#57703,#57704,#57705,#57706,
#57707,#57708,#57709,#57710,#57711,#57712,#57713,#57714,#57715,#57716,#57717,
#57718,#57719,#57720,#57721,#57722,#57723,#57724,#57725,#57726,#57727),
 .UNSPECIFIED.,.F.,.F.,(4,2,2,2,2,2,2,2,2,2,2,2,4),(5.27191147116053E-6,
1.14584468705305,5.27595614080581,6.27621750851155,6.42842423170021,6.49296697752034,
7.05675108509317,7.48372044806425,7.72947375032807,7.77323441341815,7.79046163520876,
7.79956239767949,7.80160940374884),.UNSPECIFIED.) ;
#504 = B_SPLINE_CURVE_WITH_KNOTS('',3,(#57730,#57731,#57732,#57733,#57734,
#57735,#57736,#57737,#57738,#57739,#57740,#57741,#57742,#57743,#57744,#57745,
#57746,#57747,#57748,#57749),.UNSPECIFIED.,.F.,.F.,(4,2,2,2,2,2,2,2,2,4),
(7.80160940758295,7.8089379799619,7.99849136645798,8.48798714708565,8.85467142169077,
9.05313731358241,24.5851715502772,31.3804365288312,32.5696272011659,133.309321825113),
 .UNSPECIFIED.) ;
#505 = B_SPLINE_CURVE_WITH_KNOTS('',3,(#57751,#57752,#57753,#57754,#57755,
#57756,#57757,#57758,#57759,#57760,#57761,#57762,#57763,#57764,#57765,#57766,
#57767,#57768,#57769,#57770,#57771,#57772,#57773,#57774,#57775,#57776,#57777,
#57778),.UNSPECIFIED.,.F.,.F.,(4,2,2,2,2,2,2,2,2,2,2,2,2,4),(5.27191147341303E-6,
1.28771119835054,3.98796378162772,5.31699434995946,5.97631810846778,6.42862113427837,
6.4934258850079,7.14815420783244,7.47423960298919,7.64928235471921,7.73777852432768,
7.78772679076623,7.79646451937251,7.80216111214384),.UNSPECIFIED.) ;
#506 = B_SPLINE_CURVE_WITH_KNOTS('',3,(#57781,#57782,#57783,#57784,#57785,
#57786,#57787,#57788,#57789,#57790,#57791,#57792,#57793,#57794,#57795,#57796,
#57797,#57798,#57799,#57800),.UNSPECIFIED.,.F.,.F.,(4,2,2,2,2,2,2,2,2,4),
(7.80216111214384,7.81235512109906,8.05788043165933,8.70649760391101,9.05150172288028,
9.31799764820168,29.9162325081877,38.9279602594316,40.3746267938085,174.103758636969),
 .UNSPECIFIED.) ;
#507 = B_SPLINE_CURVE_WITH_KNOTS('',3,(#57987,#57988,#57989,#57990,#57991,
#57992,#57993,#57994,#57995,#57996,#57997,#57998,#57999,#58000,#58001,#58002,
#58003,#58004,#58005,#58006,#58007,#58008,#58009,#58010,#58011,#58012,#58013,
#58014,#58015,#58016,#58017,#58018,#58019,#58020,#58021,#58022,#58023,#58024,
#58025,#58026,#58027,#58028,#58029,#58030,#58031,#58032,#58033,#58034,#58035,
#58036,#58037,#58038,#58039,#58040,#58041,#58042,#58043,#58044,#58045,#58046,
#58047,#58048,#58049,#58050,#58051,#58052,#58053,#58054,#58055,#58056,#58057,
#58058,#58059,#58060,#58061,#58062,#58063,#58064,#58065,#58066,#58067,#58068,
#58069,#58070,#58071,#58072,#58073,#58074,#58075,#58076),.UNSPECIFIED.,
 .F.,.F.,(4,2,2,2,2,2,2,2,2,2,2,2,2,2,2,2,2,2,2,2,2,2,2,2,2,2,2,2,2,2,2,
2,2,2,2,2,2,2,2,2,2,2,2,2,4),(1.42697216485095,1.642313125249,3.28462625049799,
4.92693937574699,6.56925250099599,7.39040906362048,8.21156562624498,9.03272218886948,
9.85387875149398,10.2644570328062,10.6750353141185,11.0856135954307,11.496191876743,
11.9067701580552,12.3173484393675,12.5226375800236,12.7279267206797,12.9332158613358,
13.138505001992,13.3261120329266,13.4199155483939,13.5137190638612,13.6075225793285,
13.6544243370621,13.7013260947958,13.7482278525294,13.7951296102631,13.8185804891299,
13.8420313679967,13.8654822468635,13.877207686297,13.8889331257304,13.9006742956463,
13.9124154655623,13.9182860505203,13.9241566354783,13.9270919279573,13.9300272204363,
13.9329625129153,13.9344301591548,13.9358978053943,13.9366528001863,13.9374077949783,
13.9381627897703,13.9385402871663),.UNSPECIFIED.) ;
#508 = B_SPLINE_CURVE_WITH_KNOTS('',3,(#58079,#58080,#58081,#58082,#58083,
#58084,#58085,#58086,#58087,#58088,#58089,#58090,#58091,#58092,#58093,#58094,
#58095,#58096,#58097,#58098,#58099,#58100,#58101,#58102,#58103,#58104,#58105,
#58106,#58107,#58108,#58109,#58110,#58111,#58112,#58113,#58114,#58115,#58116,
#58117,#58118,#58119,#58120,#58121,#58122,#58123,#58124,#58125,#58126,#58127,
#58128,#58129,#58130,#58131,#58132,#58133,#58134,#58135,#58136,#58137,#58138,
#58139,#58140,#58141,#58142,#58143,#58144,#58145,#58146,#58147,#58148,#58149,
#58150,#58151,#58152,#58153,#58154,#58155,#58156,#58157,#58158,#58159,#58160,
#58161,#58162,#58163,#58164,#58165,#58166,#58167,#58168),.UNSPECIFIED.,
 .F.,.F.,(4,2,2,2,2,2,2,2,2,2,2,2,2,2,2,2,2,2,2,2,2,2,2,2,2,2,2,2,2,2,2,
2,2,2,2,2,2,2,2,2,2,2,2,2,4),(13.9397809911914,13.9401584882633,13.9409134824073,
13.9416684765512,13.9424234706951,13.9438911167666,13.9453587628381,13.9482940549812,
13.9512293471242,13.9541646392672,13.9600352235533,13.9659058078393,13.9776469764114,
13.9893881449835,14.0011135844584,14.0128390239333,14.0362899028832,14.059740781833,
14.0831916607828,14.1300934186824,14.176995176582,14.2238969344817,14.2707986923813,
14.3646022081806,14.4584057239798,14.5522092397791,14.7398162713776,14.9451054120337,
15.1503945526898,15.355683693346,15.5609728340021,15.9715511153143,16.3821293966266,
16.7927076779388,17.2032859592511,17.6138642405633,18.0244425218756,18.8455990845001,
19.6667556471246,20.4879122097491,21.3090687723736,22.9513818976226,24.5936950228716,
26.2360081481206,26.4513491085187),.UNSPECIFIED.) ;
#509 = B_SPLINE_CURVE_WITH_KNOTS('',3,(#58173,#58174,#58175,#58176,#58177,
#58178,#58179,#58180,#58181,#58182,#58183,#58184,#58185,#58186,#58187,#58188,
#58189,#58190,#58191,#58192,#58193,#58194,#58195,#58196,#58197,#58198,#58199,
#58200,#58201,#58202,#58203,#58204,#58205,#58206,#58207,#58208,#58209,#58210,
#58211,#58212,#58213,#58214,#58215,#58216,#58217,#58218,#58219,#58220,#58221,
#58222,#58223,#58224,#58225,#58226,#58227,#58228,#58229,#58230,#58231,#58232,
#58233,#58234,#58235,#58236,#58237,#58238,#58239,#58240,#58241,#58242,#58243,
#58244,#58245,#58246,#58247,#58248,#58249,#58250,#58251,#58252,#58253,#58254,
#58255,#58256,#58257,#58258,#58259,#58260),.UNSPECIFIED.,.F.,.F.,(4,2,2,
2,2,2,2,2,2,2,2,2,2,2,2,2,2,2,2,2,2,2,2,2,2,2,2,2,2,2,2,2,2,2,2,2,2,2,2,
2,2,2,2,4),(14.1204637881216,14.1208456566844,14.1216093938099,14.1223731309355,
14.123136868061,14.1246217770385,14.1261066860159,14.1290765039707,14.1320463219256,
14.1350161398804,14.1409557757901,14.1468954116998,14.1587746835192,14.1706539553386,
14.182518573564,14.1943831917895,14.2181124282403,14.2418416646912,14.2655709011421,
14.3130293740439,14.3604878469457,14.4079463198475,14.4554047927492,14.5503217385528,
14.6452386843564,14.7401556301599,14.929989521767,15.1379533273813,15.3459171329956,
15.5538809386098,15.7618447442241,16.1777723554526,16.5936999666812,17.0096275779097,
17.4255551891382,17.8414828003668,18.2574104115953,19.0892656340524,19.9211208565095,
20.7529760789665,21.5848313014236,23.2485417463377,24.9122521912519,26.627144761),
 .UNSPECIFIED.) ;
#510 = B_SPLINE_CURVE_WITH_KNOTS('',3,(#58261,#58262,#58263,#58264,#58265,
#58266,#58267,#58268,#58269,#58270,#58271,#58272,#58273,#58274,#58275,#58276,
#58277,#58278,#58279,#58280,#58281,#58282,#58283,#58284,#58285,#58286,#58287,
#58288,#58289,#58290,#58291,#58292,#58293,#58294,#58295,#58296,#58297,#58298,
#58299,#58300,#58301,#58302,#58303,#58304,#58305,#58306,#58307,#58308,#58309,
#58310,#58311,#58312,#58313,#58314,#58315,#58316,#58317,#58318,#58319,#58320,
#58321,#58322,#58323,#58324,#58325,#58326,#58327,#58328,#58329,#58330,#58331,
#58332,#58333,#58334,#58335,#58336,#58337,#58338,#58339,#58340,#58341,#58342,
#58343,#58344,#58345,#58346,#58347,#58348,#58349,#58350),.UNSPECIFIED.,
 .F.,.F.,(4,2,2,2,2,2,2,2,2,2,2,2,2,2,2,2,2,2,2,2,2,2,2,2,2,2,2,2,2,2,2,
2,2,2,2,2,2,2,2,2,2,2,2,2,4),(1.61252832007444,1.66371044461233,3.32742088922465,
4.99113133383698,6.6548417784493,7.48669700075546,8.31855222306163,9.15040744536779,
9.98226266767395,10.398190278827,10.8141178899801,11.2300455011332,11.6459731122863,
12.0619007234394,12.4778283345924,12.685792140169,12.8937559457455,13.1017197513221,
13.3096835568986,13.4995174488634,13.5944343948458,13.6893513408282,13.7842682868105,
13.8317267598017,13.8791852327929,13.9266437057841,13.9741021787753,13.9978314152709,
14.0215606517665,14.0452898882621,14.0571545065099,14.0690191247577,14.0808983967437,
14.0927776687297,14.0987173047227,14.1046569407157,14.1076267587122,14.1105965767087,
14.1135663947052,14.1150513037034,14.1165362127017,14.1172999492339,14.1180636857662,
14.1188274222985,14.1192092905646),.UNSPECIFIED.) ;
#511 = B_SPLINE_CURVE_WITH_KNOTS('',3,(#58355,#58356,#58357,#58358,#58359,
#58360,#58361,#58362,#58363,#58364,#58365,#58366,#58367,#58368,#58369,#58370,
#58371,#58372,#58373,#58374,#58375,#58376,#58377,#58378,#58379,#58380,#58381,
#58382,#58383,#58384,#58385,#58386,#58387,#58388,#58389,#58390,#58391,#58392,
#58393,#58394,#58395,#58396,#58397,#58398,#58399,#58400,#58401,#58402,#58403,
#58404,#58405,#58406,#58407,#58408,#58409,#58410,#58411,#58412,#58413,#58414,
#58415,#58416,#58417,#58418,#58419,#58420,#58421,#58422,#58423,#58424,#58425,
#58426,#58427,#58428,#58429,#58430,#58431,#58432,#58433,#58434,#58435,#58436,
#58437,#58438,#58439,#58440,#58441,#58442),.UNSPECIFIED.,.F.,.F.,(4,2,2,
2,2,2,2,2,2,2,2,2,2,2,2,2,2,2,2,2,2,2,2,2,2,2,2,2,2,2,2,2,2,2,2,2,2,2,2,
2,2,2,2,4),(14.1663480266505,14.1667310032561,14.1674969564673,14.1682629096785,
14.1690288628896,14.1705181494738,14.1720074360579,14.1749860092261,14.1779645823943,
14.1809431555625,14.1869003018989,14.1928574482354,14.2047717409082,14.2166860335811,
14.2285859486937,14.2404858638063,14.2642856940314,14.2880855242566,14.3118853544817,
14.359485014932,14.4070846753823,14.4546843358327,14.502283996283,14.5974833171836,
14.6926826380842,14.7878819589848,14.9782806007861,15.1869236860124,15.3955667712387,
15.604209856465,15.8128529416912,16.2301391121438,16.6474252825964,17.064711453049,
17.4819976235016,17.8992837939541,18.3165699644067,19.1511423053119,19.985714646217,
20.8202869871222,21.6548593280273,23.3240040098377,24.993148691648,26.671883998059),
 .UNSPECIFIED.) ;
#512 = B_SPLINE_CURVE_WITH_KNOTS('',3,(#58443,#58444,#58445,#58446,#58447,
#58448,#58449,#58450,#58451,#58452,#58453,#58454,#58455,#58456,#58457,#58458,
#58459,#58460,#58461,#58462,#58463,#58464,#58465,#58466,#58467,#58468,#58469,
#58470,#58471,#58472,#58473,#58474,#58475,#58476,#58477,#58478,#58479,#58480,
#58481,#58482,#58483,#58484,#58485,#58486,#58487,#58488,#58489,#58490,#58491,
#58492,#58493,#58494,#58495,#58496,#58497,#58498,#58499,#58500,#58501,#58502,
#58503,#58504,#58505,#58506,#58507,#58508,#58509,#58510,#58511,#58512,#58513,
#58514,#58515,#58516,#58517,#58518,#58519,#58520,#58521,#58522,#58523,#58524,
#58525,#58526,#58527,#58528,#58529,#58530,#58531,#58532),.UNSPECIFIED.,
 .F.,.F.,(4,2,2,2,2,2,2,2,2,2,2,2,2,2,2,2,2,2,2,2,2,2,2,2,2,2,2,2,2,2,2,
2,2,2,2,2,2,2,2,2,2,2,2,2,4),(1.65955405720668,1.66914468166147,3.33828936332295,
5.00743404498442,6.6765787266459,7.51115106747663,8.34572340830737,9.18029574913811,
10.0148680899688,10.4321542603842,10.8494404307996,11.266726601215,11.6840127716303,
12.1012989420457,12.5185851124611,12.7272281976687,12.9358712828764,13.1445143680841,
13.3531574532918,13.5435560957881,13.6387554170363,13.7339547382844,13.8291540595326,
13.8767537201567,13.9243533807807,13.9719530414048,14.0195527020289,14.0433525323409,
14.067152362653,14.090952192965,14.102852108121,14.1147520232771,14.1266663151852,
14.1385806070933,14.1445377530473,14.1504948990014,14.1534734719784,14.1564520449554,
14.1594306179325,14.160919904421,14.1624091909095,14.1631751442385,14.1639410975676,
14.1647070508966,14.1650900275612),.UNSPECIFIED.) ;
#513 = B_SPLINE_CURVE_WITH_KNOTS('',3,(#58537,#58538,#58539,#58540,#58541,
#58542,#58543,#58544,#58545,#58546,#58547,#58548,#58549,#58550,#58551,#58552,
#58553,#58554,#58555,#58556,#58557,#58558,#58559,#58560,#58561,#58562,#58563,
#58564,#58565,#58566,#58567,#58568,#58569,#58570,#58571,#58572,#58573,#58574,
#58575,#58576,#58577,#58578,#58579,#58580,#58581,#58582,#58583,#58584,#58585,
#58586,#58587,#58588,#58589,#58590,#58591,#58592,#58593,#58594,#58595,#58596,
#58597,#58598,#58599,#58600,#58601,#58602,#58603,#58604,#58605,#58606,#58607,
#58608,#58609,#58610,#58611,#58612,#58613,#58614,#58615,#58616,#58617,#58618,
#58619,#58620,#58621,#58622,#58623,#58624,#58625),.UNSPECIFIED.,.F.,.F.,
(4,2,2,2,2,2,2,2,2,2,2,2,2,2,2,2,2,2,2,2,2,2,2,2,2,2,2,2,2,2,2,2,2,2,2,
2,2,2,2,2,2,2,2,1,4),(14.0669078671381,14.0672884413977,14.0680495899169,
14.0688107384361,14.0695718869553,14.0710516830252,14.0725314790952,14.075491071235,
14.0784506633748,14.0814102555147,14.0873294397944,14.093248624074,14.1050869926334,
14.1169253611927,14.1287487567706,14.1405721523484,14.164218943504,14.1878657346596,
14.2115125258153,14.2588061081265,14.3060996904378,14.3533932727491,14.4006868550603,
14.4952740196829,14.5898611843054,14.684448348928,14.873622678173,15.0807936569189,
15.2879646356648,15.4951356144107,15.7023065931566,16.1166485506484,16.5309905081402,
16.945332465632,17.3596744231238,17.7740163806156,18.1883583381074,19.0170422530911,
19.8457261680747,20.6744100830583,21.5030939980419,23.1604618280091,24.8178296579763,
26.4751974879435,26.5749735502974),.UNSPECIFIED.) ;
#514 = B_SPLINE_CURVE_WITH_KNOTS('',3,(#58626,#58627,#58628,#58629,#58630,
#58631,#58632,#58633,#58634,#58635,#58636,#58637,#58638,#58639,#58640,#58641,
#58642,#58643,#58644,#58645,#58646,#58647,#58648,#58649,#58650,#58651,#58652,
#58653,#58654,#58655,#58656,#58657,#58658,#58659,#58660,#58661,#58662,#58663,
#58664,#58665,#58666,#58667,#58668,#58669,#58670,#58671,#58672,#58673,#58674,
#58675,#58676,#58677,#58678,#58679,#58680,#58681,#58682,#58683,#58684,#58685,
#58686,#58687,#58688,#58689,#58690,#58691,#58692,#58693,#58694,#58695,#58696,
#58697,#58698,#58699,#58700,#58701,#58702,#58703,#58704,#58705,#58706,#58707,
#58708,#58709,#58710,#58711,#58712,#58713,#58714,#58715),.UNSPECIFIED.,
 .F.,.F.,(4,2,2,2,2,2,2,2,2,2,2,2,2,2,2,2,2,2,2,2,2,2,2,2,2,2,2,2,2,2,2,
2,2,2,2,2,2,2,2,2,2,2,2,2,4),(1.55759176761474,1.65736783004784,3.31473566009569,
4.97210349014353,6.62947132019138,7.4581552352153,8.28683915023922,9.11552306526314,
9.94420698028706,10.358548937799,10.772890895311,11.1872328528229,11.6015748103349,
12.0159167678469,12.4302587253588,12.6374297041148,12.8446006828708,13.0517716616268,
13.2589426403828,13.4481169692896,13.542704133743,13.6372912981964,13.7318784626498,
13.7791720448765,13.8264656271032,13.8737592093299,13.9210527915566,13.94469958267,
13.9683463737833,13.9919931648967,14.0038165604533,14.01563995601,14.0274783250456,
14.0393166940813,14.0452358785991,14.0511550631169,14.0541146553758,14.0570742476347,
14.0600338398936,14.0615136360231,14.0629934321526,14.0637545805585,14.0645157289644,
14.0652768773704,14.0656574515733),.UNSPECIFIED.) ;
#515 = B_SPLINE_CURVE_WITH_KNOTS('',3,(#58720,#58721,#58722,#58723,#58724,
#58725,#58726,#58727,#58728,#58729,#58730,#58731,#58732,#58733,#58734,#58735,
#58736,#58737,#58738,#58739,#58740,#58741,#58742,#58743,#58744,#58745,#58746,
#58747,#58748,#58749,#58750,#58751,#58752,#58753,#58754,#58755,#58756,#58757,
#58758,#58759,#58760,#58761,#58762,#58763,#58764,#58765,#58766,#58767,#58768,
#58769,#58770,#58771,#58772,#58773,#58774,#58775,#58776,#58777,#58778,#58779,
#58780,#58781,#58782,#58783,#58784,#58785,#58786,#58787,#58788,#58789,#58790,
#58791,#58792,#58793,#58794,#58795,#58796,#58797,#58798,#58799,#58800,#58801,
#58802,#58803,#58804,#58805,#58806,#58807,#58808,#58809),.UNSPECIFIED.,
 .F.,.F.,(4,2,2,2,2,2,2,2,2,2,2,2,2,2,2,2,2,2,2,2,2,2,2,2,2,2,2,2,2,2,2,
2,2,2,2,2,2,2,2,2,2,2,2,2,4),(14.021342562188,14.021722034217,14.022480978275,
14.023239922333,14.023998866391,14.0254743099342,14.0269497534774,14.0299006405638,
14.0328515276501,14.0358024147365,14.0417041889092,14.0476059630819,14.0594095114273,
14.0712130597728,14.0830013624884,14.0947896652041,14.1183662706354,14.1419428760667,
14.165519481498,14.2126726923606,14.2598259032232,14.3069791140858,14.3541323249484,
14.4484387466737,14.5427451683989,14.6370515901241,14.8256644335745,15.032160898502,
15.2386573634295,15.445153828357,15.6516502932844,16.0646432231394,16.4776361529944,
16.8906290828493,17.3036220127043,17.7166149425593,18.1296078724142,18.9555937321241,
19.7815795918341,20.607565451544,21.4335513112539,23.0855230306737,24.7374947500936,
26.3894664695134,26.5306282055506),.UNSPECIFIED.) ;
#516 = B_SPLINE_CURVE_WITH_KNOTS('',3,(#58810,#58811,#58812,#58813,#58814,
#58815,#58816,#58817,#58818,#58819,#58820,#58821,#58822,#58823,#58824,#58825,
#58826,#58827,#58828,#58829,#58830,#58831,#58832,#58833,#58834,#58835,#58836,
#58837,#58838,#58839,#58840,#58841,#58842,#58843,#58844,#58845,#58846,#58847,
#58848,#58849,#58850,#58851,#58852,#58853,#58854,#58855,#58856,#58857,#58858,
#58859,#58860,#58861,#58862,#58863,#58864,#58865,#58866,#58867,#58868,#58869,
#58870,#58871,#58872,#58873,#58874,#58875,#58876,#58877,#58878,#58879,#58880,
#58881,#58882,#58883,#58884,#58885,#58886,#58887,#58888,#58889,#58890,#58891,
#58892,#58893,#58894,#58895,#58896,#58897,#58898,#58899),.UNSPECIFIED.,
 .F.,.F.,(4,2,2,2,2,2,2,2,2,2,2,2,2,2,2,2,2,2,2,2,2,2,2,2,2,2,2,2,2,2,2,
2,2,2,2,2,2,2,2,2,2,2,2,2,4),(1.51080998338119,1.65197171933602,3.30394343867204,
4.95591515800806,6.60788687734408,7.43387273701209,8.2598585966801,9.08584445634811,
9.91183031601612,10.3248232458501,10.7378161756841,11.1508091055181,11.5638020353521,
11.9767949651861,12.3897878950202,12.5962843599372,12.8027808248542,13.0092772897712,
13.2157737546882,13.4043865989579,13.4986930210928,13.5929994432276,13.6873058653625,
13.7344590764299,13.7816122874974,13.8287654985648,13.8759187096322,13.8994953151659,
13.9230719206997,13.9466485262334,13.9584368290002,13.9702251317671,13.9820286804365,
13.9938322291059,13.9997340034405,14.0056357777752,14.0085866649426,14.0115375521099,
14.0144884392773,14.0159638828609,14.0174393264446,14.0181982693009,14.0189572121572,
14.0197161550135,14.0200956264417),.UNSPECIFIED.) ;
#517 = B_SPLINE_CURVE_WITH_KNOTS('',3,(#58904,#58905,#58906,#58907,#58908,
#58909,#58910,#58911,#58912,#58913,#58914,#58915,#58916,#58917,#58918,#58919,
#58920,#58921,#58922,#58923,#58924,#58925,#58926,#58927,#58928,#58929,#58930,
#58931,#58932,#58933,#58934,#58935,#58936,#58937,#58938,#58939,#58940,#58941,
#58942,#58943,#58944,#58945,#58946,#58947,#58948,#58949,#58950,#58951,#58952,
#58953,#58954,#58955,#58956,#58957,#58958,#58959,#58960,#58961,#58962,#58963,
#58964,#58965,#58966,#58967,#58968,#58969,#58970,#58971,#58972,#58973,#58974,
#58975,#58976,#58977,#58978,#58979,#58980,#58981,#58982,#58983,#58984,#58985,
#58986,#58987,#58988,#58989,#58990,#58991),.UNSPECIFIED.,.F.,.F.,(4,2,2,
2,2,2,2,2,2,2,2,2,2,2,2,2,2,2,2,2,2,2,2,2,2,2,2,2,2,2,2,2,2,2,2,2,2,2,2,
2,2,2,2,4),(14.1547675259996,14.1551502230512,14.1559156171545,14.1566810112577,
14.1574464053609,14.1589345873031,14.1604227692453,14.1633991331296,14.1663754970139,
14.1693518608982,14.1753045886669,14.1812573164355,14.1931627719728,14.2050682275101,
14.2169592360564,14.2288502446028,14.2526322616954,14.2764142787881,14.3001962958808,
14.3477603300661,14.3953243642515,14.4428883984368,14.4904524326222,14.5855805009929,
14.6807085693636,14.7758366377343,14.9660927744757,15.1745644176806,15.3830360608854,
15.5915077040903,15.7999793472952,16.216922633705,16.6338659201147,17.0508092065245,
17.4677524929342,17.884695779344,18.3016390657537,19.1355256385732,19.9694122113928,
20.8032987842123,21.6371853570318,23.3049585026708,24.9727316483098,26.6605889239056),
 .UNSPECIFIED.) ;
#518 = B_SPLINE_CURVE_WITH_KNOTS('',3,(#58992,#58993,#58994,#58995,#58996,
#58997,#58998,#58999,#59000,#59001,#59002,#59003,#59004,#59005,#59006,#59007,
#59008,#59009,#59010,#59011,#59012,#59013,#59014,#59015,#59016,#59017,#59018,
#59019,#59020,#59021,#59022,#59023,#59024,#59025,#59026,#59027,#59028,#59029,
#59030,#59031,#59032,#59033,#59034,#59035,#59036,#59037,#59038,#59039,#59040,
#59041,#59042,#59043,#59044,#59045,#59046,#59047,#59048,#59049,#59050,#59051,
#59052,#59053,#59054,#59055,#59056,#59057,#59058,#59059,#59060,#59061,#59062,
#59063,#59064,#59065,#59066,#59067,#59068,#59069,#59070,#59071,#59072,#59073,
#59074,#59075,#59076,#59077,#59078,#59079,#59080,#59081),.UNSPECIFIED.,
 .F.,.F.,(4,2,2,2,2,2,2,2,2,2,2,2,2,2,2,2,2,2,2,2,2,2,2,2,2,2,2,2,2,2,2,
2,2,2,2,2,2,2,2,2,2,2,2,2,4),(1.647689015682,1.66777314561885,3.33554629123771,
5.00331943685656,6.67109258247542,7.50497915528485,8.33886572809427,9.1727523009037,
10.0066388737131,10.4235821601178,10.8405254465226,11.2574687329273,11.674412019332,
12.0913553057367,12.5082985921414,12.7167702353438,12.9252418785461,13.1337135217485,
13.3421851649508,13.5324413017259,13.6275693701134,13.7226974385009,13.8178255068884,
13.8653895410822,13.912953575276,13.9605176094697,14.0080816436635,14.0318636607604,
14.0556456778572,14.0794276949541,14.0913187035026,14.103209712051,14.1151151676442,
14.1270206232375,14.1329733510341,14.1389260788307,14.141902442729,14.1448788066273,
14.1478551705256,14.1493433524748,14.1508315344239,14.151596927938,14.1523623214521,
14.1531277149662,14.1535104117233),.UNSPECIFIED.) ;
#519 = B_SPLINE_CURVE_WITH_KNOTS('',3,(#59086,#59087,#59088,#59089,#59090,
#59091,#59092,#59093,#59094,#59095,#59096,#59097,#59098,#59099,#59100,#59101,
#59102,#59103,#59104,#59105,#59106,#59107,#59108,#59109,#59110,#59111,#59112,
#59113,#59114,#59115,#59116,#59117,#59118,#59119,#59120,#59121,#59122,#59123,
#59124,#59125,#59126,#59127,#59128,#59129,#59130,#59131,#59132,#59133,#59134,
#59135,#59136,#59137,#59138,#59139,#59140,#59141,#59142,#59143,#59144,#59145,
#59146,#59147,#59148,#59149,#59150,#59151,#59152,#59153,#59154,#59155,#59156,
#59157,#59158,#59159,#59160,#59161,#59162,#59163,#59164,#59165,#59166,#59167,
#59168,#59169,#59170,#59171,#59172,#59173),.UNSPECIFIED.,.F.,.F.,(4,2,2,
2,2,2,2,2,2,2,2,2,2,2,2,2,2,2,2,2,2,2,2,2,2,2,2,2,2,2,2,2,2,2,2,2,2,2,2,
2,2,2,2,4),(14.1455560200775,14.1459384944968,14.1467034433353,14.1474683921739,
14.1482333410125,14.149720644208,14.1512079474035,14.1541825537946,14.1571571601856,
14.1601317665767,14.1660809793588,14.1720301921409,14.1839286177052,14.1958270432694,
14.2077109663326,14.2195948893957,14.2433627355219,14.2671305816482,14.2908984277745,
14.338434120027,14.3859698122795,14.433505504532,14.4810411967845,14.5761125812896,
14.6711839657946,14.7662553502996,14.9563981193097,15.1647333928276,15.3730686663455,
15.5814039398634,15.7897392133813,16.206409760417,16.6230803074528,17.0397508544886,
17.4564214015244,17.8730919485602,18.2897624955959,19.1231035896675,19.9564446837391,
20.7897857778106,21.6231268718822,23.2898090600253,24.9564912481684,26.6516061658473),
 .UNSPECIFIED.) ;
#520 = B_SPLINE_CURVE_WITH_KNOTS('',3,(#59174,#59175,#59176,#59177,#59178,
#59179,#59180,#59181,#59182,#59183,#59184,#59185,#59186,#59187,#59188,#59189,
#59190,#59191,#59192,#59193,#59194,#59195,#59196,#59197,#59198,#59199,#59200,
#59201,#59202,#59203,#59204,#59205,#59206,#59207,#59208,#59209,#59210,#59211,
#59212,#59213,#59214,#59215,#59216,#59217,#59218,#59219,#59220,#59221,#59222,
#59223,#59224,#59225,#59226,#59227,#59228,#59229,#59230,#59231,#59232,#59233,
#59234,#59235,#59236,#59237,#59238,#59239,#59240,#59241,#59242,#59243,#59244,
#59245,#59246,#59247,#59248,#59249,#59250,#59251,#59252,#59253,#59254,#59255,
#59256,#59257,#59258,#59259,#59260,#59261,#59262,#59263),.UNSPECIFIED.,
 .F.,.F.,(4,2,2,2,2,2,2,2,2,2,2,2,2,2,2,2,2,2,2,2,2,2,2,2,2,2,2,2,2,2,2,
2,2,2,2,2,2,2,2,2,2,2,2,2,4),(1.63824945860653,1.66668218810681,3.33336437621363,
5.00004656432044,6.66672875242725,7.50006984648066,8.33341094053407,9.16675203458747,
10.0000931286409,10.4167636756676,10.8334342226943,11.250104769721,11.6667753167477,
12.0834458637744,12.5001164108011,12.7084516843145,12.9167869578278,13.1251222313412,
13.3334575048545,13.5236002737055,13.618671658131,13.7137430425566,13.8088144269821,
13.8563501191948,13.9038858114076,13.9514215036203,13.9989571958331,14.0227250419395,
14.0464928880459,14.0702607341522,14.0821446572054,14.0940285802586,14.105927006162,
14.1178254320655,14.1237746450172,14.1297238579689,14.1326984644448,14.1356730709206,
14.1386476773965,14.1401349806344,14.1416222838723,14.1423872326495,14.1431521814267,
14.1439171302038,14.1442996045924),.UNSPECIFIED.) ;
#521 = B_SPLINE_CURVE_WITH_KNOTS('',3,(#59268,#59269,#59270,#59271,#59272,
#59273,#59274,#59275,#59276,#59277,#59278,#59279,#59280,#59281,#59282,#59283,
#59284,#59285,#59286,#59287,#59288,#59289,#59290,#59291,#59292,#59293,#59294,
#59295,#59296,#59297,#59298,#59299,#59300,#59301,#59302,#59303,#59304,#59305,
#59306,#59307,#59308,#59309,#59310,#59311,#59312,#59313,#59314,#59315,#59316,
#59317,#59318,#59319,#59320,#59321,#59322,#59323,#59324,#59325,#59326,#59327,
#59328,#59329,#59330,#59331,#59332,#59333,#59334,#59335,#59336,#59337,#59338,
#59339,#59340,#59341,#59342,#59343,#59344,#59345,#59346,#59347,#59348,#59349,
#59350,#59351,#59352,#59353,#59354,#59355,#59356,#59357),.UNSPECIFIED.,
 .F.,.F.,(4,2,2,2,2,2,2,2,2,2,2,2,2,2,2,2,2,2,2,2,2,2,2,2,2,2,2,2,2,2,2,
2,2,2,2,2,2,2,2,2,2,2,2,2,4),(13.9958308278144,13.9962096816943,13.9969673894541,
13.997725097214,13.9984828049738,13.9999558104743,14.0014288159747,14.0043748269757,
14.0073208379766,14.0102668489776,14.0161588709794,14.0220508929813,14.0338349369851,
14.0456189809888,14.0573876272289,14.069156273469,14.0926935659491,14.1162308584293,
14.1397681509095,14.1868427358698,14.2339173208301,14.2809919057904,14.3280664907508,
14.4222156606714,14.5163648305921,14.6105140005127,14.798812340354,15.00493115794,
15.2110499755261,15.4171687931121,15.6232876106981,16.0355252458701,16.4477628810421,
16.8600005162142,17.2722381513862,17.6844757865582,18.0967134217303,18.9211886920743,
19.7456639624184,20.5701392327624,21.3946145031065,23.0435650437946,24.6925155844827,
26.3414661251708,26.5058166413175),.UNSPECIFIED.) ;
#522 = B_SPLINE_CURVE_WITH_KNOTS('',3,(#59358,#59359,#59360,#59361,#59362,
#59363,#59364,#59365,#59366,#59367,#59368,#59369,#59370,#59371,#59372,#59373,
#59374,#59375,#59376,#59377,#59378,#59379,#59380,#59381,#59382,#59383,#59384,
#59385,#59386,#59387,#59388,#59389,#59390,#59391,#59392,#59393,#59394,#59395,
#59396,#59397,#59398,#59399,#59400,#59401,#59402,#59403,#59404,#59405,#59406,
#59407,#59408,#59409,#59410,#59411,#59412,#59413,#59414,#59415,#59416,#59417,
#59418,#59419,#59420,#59421,#59422,#59423,#59424,#59425,#59426,#59427,#59428,
#59429,#59430,#59431,#59432,#59433,#59434,#59435,#59436,#59437,#59438,#59439,
#59440,#59441,#59442,#59443,#59444,#59445,#59446,#59447),.UNSPECIFIED.,
 .F.,.F.,(4,2,2,2,2,2,2,2,2,2,2,2,2,2,2,2,2,2,2,2,2,2,2,2,2,2,2,2,2,2,2,
2,2,2,2,2,2,2,2,2,2,2,2,2,4),(1.48460002454081,1.64895054064786,3.29790108129571,
4.94685162194357,6.59580216259142,7.42027743291535,8.24475270323928,9.06922797356321,
9.89370324388713,10.3059408790491,10.7181785142111,11.130416149373,11.542653784535,
11.954891419697,12.3671290548589,12.5732478724399,12.7793666900209,12.9854855076019,
13.1916043251828,13.3799026649428,13.4740518348228,13.5682010047028,13.6623501745829,
13.7094247595229,13.7564993444629,13.8035739294029,13.8506485143429,13.8741858068129,
13.8977230992829,13.9212603917529,13.9330290379879,13.9447976842229,13.9565817286828,
13.9683657731427,13.9742577953726,13.9801498176026,13.9830958287176,13.9860418398326,
13.9889878509475,13.990460856505,13.9919338620625,13.9926915691657,13.9934492762689,
13.9942069833721,13.9945858369238),.UNSPECIFIED.) ;
#523 = B_SPLINE_CURVE_WITH_KNOTS('',3,(#59452,#59453,#59454,#59455,#59456,
#59457,#59458,#59459,#59460,#59461,#59462,#59463,#59464,#59465,#59466,#59467,
#59468,#59469,#59470,#59471,#59472,#59473,#59474,#59475,#59476,#59477,#59478,
#59479,#59480,#59481,#59482,#59483,#59484,#59485,#59486,#59487,#59488,#59489,
#59490,#59491,#59492,#59493,#59494,#59495,#59496,#59497,#59498,#59499,#59500,
#59501,#59502,#59503,#59504,#59505,#59506,#59507,#59508,#59509,#59510,#59511,
#59512,#59513,#59514,#59515,#59516,#59517,#59518,#59519,#59520,#59521,#59522,
#59523,#59524,#59525,#59526,#59527,#59528,#59529,#59530,#59531,#59532,#59533,
#59534,#59535,#59536,#59537,#59538,#59539,#59540),.UNSPECIFIED.,.F.,.F.,
(4,2,2,2,2,2,2,2,2,2,2,2,2,2,2,2,2,2,2,2,2,2,2,2,2,2,2,2,2,2,2,2,2,2,2,
2,2,2,2,2,2,2,2,1,4),(14.0868029194625,14.0871839745037,14.087946084586,
14.0887081946684,14.0894703047507,14.0909520006773,14.0924336966038,14.095397088457,
14.0983604803101,14.1013238721633,14.1072506558696,14.1131774395758,14.1250310069884,
14.136884574401,14.148723286499,14.160561998597,14.184239422793,14.207916846989,
14.231594271185,14.2789491195771,14.3263039679691,14.3736588163611,14.4210136647531,
14.5157233615372,14.6104330583212,14.7051427551052,14.8945621486733,15.1020276449097,
15.3094931411461,15.5169586373825,15.7244241336189,16.1393551260918,16.5542861185646,
16.9692171110374,17.3841481035102,17.799079095983,18.2140100884559,19.0438720734015,
19.8737340583471,20.7035960432928,21.5334580282384,23.1931819981297,24.852905968021,
26.5126299379123,26.5943480659534),.UNSPECIFIED.) ;
#524 = B_SPLINE_CURVE_WITH_KNOTS('',3,(#59541,#59542,#59543,#59544,#59545,
#59546,#59547,#59548,#59549,#59550,#59551,#59552,#59553,#59554,#59555,#59556,
#59557,#59558,#59559,#59560,#59561,#59562,#59563,#59564,#59565,#59566,#59567,
#59568,#59569,#59570,#59571,#59572,#59573,#59574,#59575,#59576,#59577,#59578,
#59579,#59580,#59581,#59582,#59583,#59584,#59585,#59586,#59587,#59588,#59589,
#59590,#59591,#59592,#59593,#59594,#59595,#59596,#59597,#59598,#59599,#59600,
#59601,#59602,#59603,#59604,#59605,#59606,#59607,#59608,#59609,#59610,#59611,
#59612,#59613,#59614,#59615,#59616,#59617,#59618,#59619,#59620,#59621,#59622,
#59623,#59624,#59625,#59626,#59627,#59628,#59629,#59630),.UNSPECIFIED.,
 .F.,.F.,(4,2,2,2,2,2,2,2,2,2,2,2,2,2,2,2,2,2,2,2,2,2,2,2,2,2,2,2,2,2,2,
2,2,2,2,2,2,2,2,2,2,2,2,2,4),(1.57800584185108,1.65972396994431,3.31944793988862,
4.97917190983293,6.63889587977724,7.4687578647494,8.29861984972155,9.12848183469371,
9.95834381966586,10.3732748121519,10.788205804638,11.2031367971241,11.6180677896102,
12.0329987820963,12.4479297745823,12.6553952708254,12.8628607670684,13.0703262633114,
13.2777917595545,13.4672111529754,13.5619208496858,13.6566305463962,13.7513402431067,
13.7986950914619,13.8460499398171,13.8934047881723,13.9407596365275,13.9644370607051,
13.9881144848827,14.0117919090603,14.0236306211492,14.035469333238,14.0473229006196,
14.0591764680012,14.065103251692,14.0710300353828,14.0739934272282,14.0769568190737,
14.0799202109191,14.0814019068418,14.0828836027645,14.0836457122491,14.0844078217337,
14.0851699312182,14.0855509859605),.UNSPECIFIED.) ;
#525 = B_SPLINE_CURVE_WITH_KNOTS('',3,(#59635,#59636,#59637,#59638,#59639,
#59640,#59641,#59642,#59643,#59644,#59645,#59646,#59647,#59648,#59649,#59650,
#59651,#59652,#59653,#59654,#59655,#59656,#59657,#59658,#59659,#59660,#59661,
#59662,#59663,#59664,#59665,#59666,#59667,#59668,#59669,#59670,#59671,#59672,
#59673,#59674,#59675,#59676,#59677,#59678,#59679,#59680,#59681,#59682,#59683,
#59684,#59685,#59686,#59687,#59688,#59689,#59690,#59691,#59692,#59693,#59694,
#59695,#59696,#59697,#59698,#59699,#59700,#59701,#59702,#59703,#59704,#59705,
#59706,#59707,#59708,#59709,#59710,#59711,#59712,#59713,#59714,#59715,#59716,
#59717,#59718,#59719,#59720,#59721,#59722),.UNSPECIFIED.,.F.,.F.,(4,2,2,
2,2,2,2,2,2,2,2,2,2,2,2,2,2,2,2,2,2,2,2,2,2,2,2,2,2,2,2,2,2,2,2,2,2,2,2,
2,2,2,2,4),(14.1686729967438,14.1690560293449,14.1698220945472,14.1705881597495,
14.1713542249518,14.1728437331919,14.1743332414321,14.1773122579123,14.1802912743926,
14.1832702908729,14.1892283238334,14.1951863567939,14.207102422715,14.219018488636,
14.2309201917689,14.2428218949018,14.2666253011676,14.2904287074334,14.3142321136991,
14.3618389262307,14.4094457387622,14.4570525512938,14.5046593638254,14.5998729888885,
14.6950866139516,14.7903002390147,14.980727489141,15.1894049942478,15.3980824993547,
15.6067600044615,15.8154375095683,16.232792519782,16.6501475299957,17.0675025402094,
17.4848575504231,17.9022125606368,18.3195675708505,19.1542775912779,19.9889876117052,
20.8236976321326,21.65840765256,23.3278276934148,24.9972477342695,26.6741519513281),
 .UNSPECIFIED.) ;
#526 = B_SPLINE_CURVE_WITH_KNOTS('',3,(#59723,#59724,#59725,#59726,#59727,
#59728,#59729,#59730,#59731,#59732,#59733,#59734,#59735,#59736,#59737,#59738,
#59739,#59740,#59741,#59742,#59743,#59744,#59745,#59746,#59747,#59748,#59749,
#59750,#59751,#59752,#59753,#59754,#59755,#59756,#59757,#59758,#59759,#59760,
#59761,#59762,#59763,#59764,#59765,#59766,#59767,#59768,#59769,#59770,#59771,
#59772,#59773,#59774,#59775,#59776,#59777,#59778,#59779,#59780,#59781,#59782,
#59783,#59784,#59785,#59786,#59787,#59788,#59789,#59790,#59791,#59792,#59793,
#59794,#59795,#59796,#59797,#59798,#59799,#59800,#59801,#59802,#59803,#59804,
#59805,#59806,#59807,#59808,#59809,#59810,#59811,#59812),.UNSPECIFIED.,
 .F.,.F.,(4,2,2,2,2,2,2,2,2,2,2,2,2,2,2,2,2,2,2,2,2,2,2,2,2,2,2,2,2,2,2,
2,2,2,2,2,2,2,2,2,2,2,2,2,4),(1.66193586464827,1.66942004071743,3.33884008143485,
5.00826012215228,6.6776801628697,7.51239018322842,8.34710020358713,9.18181022394584,
10.0165202443046,10.4338752544839,10.8512302646633,11.2685852748426,11.685940285022,
12.1032952952013,12.5206503053807,12.7293278104704,12.93800531556,13.1466828206497,
13.3553603257394,13.5457875760677,13.6410012012319,13.736214826396,13.8314284515602,
13.8790352641423,13.9266420767244,13.9742488893064,14.0218557018885,14.0456591081796,
14.0694625144706,14.0932659207616,14.1051676239072,14.1170693270527,14.1289853931201,
14.1409014591876,14.1468594922213,14.152817525255,14.1557965417719,14.1587755582887,
14.1617545748056,14.163244083064,14.1647335913224,14.1654996565209,14.1662657217195,
14.167031786918,14.1674148195172),.UNSPECIFIED.) ;
#527 = B_SPLINE_CURVE_WITH_KNOTS('',3,(#59817,#59818,#59819,#59820,#59821,
#59822,#59823,#59824,#59825,#59826,#59827,#59828,#59829,#59830,#59831,#59832,
#59833,#59834,#59835,#59836,#59837,#59838,#59839,#59840,#59841,#59842,#59843,
#59844,#59845,#59846,#59847,#59848,#59849,#59850,#59851,#59852,#59853,#59854,
#59855,#59856,#59857,#59858,#59859,#59860,#59861,#59862,#59863,#59864,#59865,
#59866,#59867,#59868,#59869,#59870,#59871,#59872,#59873,#59874,#59875,#59876,
#59877,#59878,#59879,#59880,#59881,#59882,#59883,#59884,#59885,#59886,#59887,
#59888,#59889,#59890,#59891,#59892,#59893,#59894,#59895,#59896,#59897,#59898,
#59899,#59900,#59901,#59902,#59903,#59904,#59905),.UNSPECIFIED.,.F.,.F.,
(4,2,2,2,2,2,2,2,2,2,2,2,2,2,2,2,2,2,2,2,2,2,2,2,2,2,2,2,2,2,2,2,2,2,2,
2,2,2,2,2,2,2,2,1,4),(14.1046764419688,14.1050579284097,14.1058209012915,
14.1065838741732,14.107346847055,14.1088302492569,14.1103136514588,14.1132804558627,
14.1162472602665,14.1192140646704,14.1251476734781,14.1310812822858,14.1429484999011,
14.1548157175165,14.1666681867437,14.1785206559708,14.2022255944251,14.2259305328793,
14.2496354713336,14.2970453482421,14.3444552251506,14.3918651020592,14.4392749789677,
14.5340947327848,14.6289144866018,14.7237342404189,14.913373748053,15.1211038392599,
15.3288339304668,15.5365640216737,15.7442941128806,16.1597542952945,16.5752144777083,
16.9906746601222,17.406134842536,17.8215950249498,18.2370552073637,19.0679755721913,
19.898895937019,20.7298163018467,21.5607366666744,23.2225773963297,24.884418125985,
26.5462588556404,26.6117601500675),.UNSPECIFIED.) ;
#528 = B_SPLINE_CURVE_WITH_KNOTS('',3,(#59906,#59907,#59908,#59909,#59910,
#59911,#59912,#59913,#59914,#59915,#59916,#59917,#59918,#59919,#59920,#59921,
#59922,#59923,#59924,#59925,#59926,#59927,#59928,#59929,#59930,#59931,#59932,
#59933,#59934,#59935,#59936,#59937,#59938,#59939,#59940,#59941,#59942,#59943,
#59944,#59945,#59946,#59947,#59948,#59949,#59950,#59951,#59952,#59953,#59954,
#59955,#59956,#59957,#59958,#59959,#59960,#59961,#59962,#59963,#59964,#59965,
#59966,#59967,#59968,#59969,#59970,#59971,#59972,#59973,#59974,#59975,#59976,
#59977,#59978,#59979,#59980,#59981,#59982,#59983,#59984,#59985,#59986,#59987,
#59988,#59989,#59990,#59991,#59992,#59993,#59994,#59995),.UNSPECIFIED.,
 .F.,.F.,(4,2,2,2,2,2,2,2,2,2,2,2,2,2,2,2,2,2,2,2,2,2,2,2,2,2,2,2,2,2,2,
2,2,2,2,2,2,2,2,2,2,2,2,2,4),(1.59633943522071,1.66184072925037,3.32368145850075,
4.98552218775112,6.6473629170015,7.47828328162668,8.30920364625187,9.14012401087706,
9.97104437550225,10.3865045578148,10.8019647401274,11.21742492244,11.6328851047526,
12.0483452870652,12.4638054693778,12.6715355605341,12.8792656516904,13.0869957428467,
13.294725834003,13.4843653426121,13.5791850969167,13.6740048512212,13.7688246055258,
13.8162344826781,13.8636443598303,13.9110542369826,13.9584641141349,13.982169052711,
14.0058739912872,14.0295789298633,14.0414313991514,14.0532838684395,14.0651510853518,
14.0770183022642,14.0829519107204,14.0888855191766,14.0918523234047,14.0948191276328,
14.0977859318609,14.0992693339749,14.100752736089,14.1015157095784,14.1022786830678,
14.1030416565573,14.103423143302),.UNSPECIFIED.) ;
#529 = B_SPLINE_CURVE_WITH_KNOTS('',3,(#60000,#60001,#60002,#60003,#60004,
#60005,#60006,#60007,#60008,#60009,#60010,#60011,#60012,#60013,#60014,#60015,
#60016,#60017,#60018,#60019,#60020,#60021,#60022,#60023,#60024,#60025,#60026,
#60027,#60028,#60029,#60030,#60031,#60032,#60033,#60034,#60035,#60036,#60037,
#60038,#60039,#60040,#60041,#60042,#60043,#60044,#60045,#60046,#60047,#60048,
#60049,#60050,#60051,#60052,#60053,#60054,#60055,#60056,#60057,#60058,#60059,
#60060,#60061,#60062,#60063,#60064,#60065,#60066,#60067,#60068,#60069,#60070,
#60071,#60072,#60073,#60074,#60075,#60076,#60077,#60078,#60079,#60080,#60081,
#60082,#60083,#60084,#60085,#60086,#60087,#60088,#60089),.UNSPECIFIED.,
 .F.,.F.,(4,2,2,2,2,2,2,2,2,2,2,2,2,2,2,2,2,2,2,2,2,2,2,2,2,2,2,2,2,2,2,
2,2,2,2,2,2,2,2,2,2,2,2,2,4),(13.9686134554172,13.9689916509333,13.9697480419656,
13.9705044329979,13.9712608240301,13.9727312275229,13.9742016310156,13.9771424380011,
13.9800832449866,13.9830240519721,13.9889056659431,13.994787279914,14.006550507856,
14.0183137357979,14.0300614047906,14.0418090737832,14.0653044117685,14.0887997497538,
14.1122950877391,14.1592857637096,14.2062764396802,14.2532671156508,14.3002577916213,
14.3942391435625,14.4882204955036,14.5822018474448,14.770164551327,14.9758804803237,
15.1815964093203,15.3873123383169,15.5930282673136,16.0044601253068,16.4158919833001,
16.8273238412934,17.2387556992867,17.65018755728,18.0616194152732,18.8844831312598,
19.7073468472463,20.5302105632329,21.3530742792195,22.9988017111926,24.6445291431657,
26.2902565751388,26.4793600117376),.UNSPECIFIED.) ;
#530 = B_SPLINE_CURVE_WITH_KNOTS('',3,(#60090,#60091,#60092,#60093,#60094,
#60095,#60096,#60097,#60098,#60099,#60100,#60101,#60102,#60103,#60104,#60105,
#60106,#60107,#60108,#60109,#60110,#60111,#60112,#60113,#60114,#60115,#60116,
#60117,#60118,#60119,#60120,#60121,#60122,#60123,#60124,#60125,#60126,#60127,
#60128,#60129,#60130,#60131,#60132,#60133,#60134,#60135,#60136,#60137,#60138,
#60139,#60140,#60141,#60142,#60143,#60144,#60145,#60146,#60147,#60148,#60149,
#60150,#60151,#60152,#60153,#60154,#60155,#60156,#60157,#60158,#60159,#60160,
#60161,#60162,#60163,#60164,#60165,#60166,#60167,#60168,#60169,#60170,#60171,
#60172,#60173,#60174,#60175,#60176,#60177,#60178,#60179),.UNSPECIFIED.,
 .F.,.F.,(4,2,2,2,2,2,2,2,2,2,2,2,2,2,2,2,2,2,2,2,2,2,2,2,2,2,2,2,2,2,2,
2,2,2,2,2,2,2,2,2,2,2,2,2,4),(1.45662399537573,1.64572743206755,3.29145486413511,
4.93718229620266,6.58290972827021,7.40577344430399,8.22863716033777,9.05150087637154,
9.87436459240532,10.2857964504222,10.6972283084391,11.108660166456,11.5200920244729,
11.9315238824898,12.3429557405066,12.5486716695151,12.7543875985235,12.960103527532,
13.1658194565404,13.3537821600959,13.4477635118736,13.5417448636514,13.6357262154291,
13.682716891318,13.7297075672069,13.7766982430957,13.8236889189846,13.847184256929,
13.8706795948735,13.8941749328179,13.9059226017901,13.9176702707623,13.9294334980288,
13.9411967252953,13.9470783389286,13.9529599525619,13.9559007593785,13.9588415661951,
13.9617823730117,13.9632527764201,13.9647231798284,13.9654795709265,13.9662359620246,
13.9669923531227,13.9673705486717),.UNSPECIFIED.) ;
#531 = B_SPLINE_CURVE_WITH_KNOTS('',3,(#60184,#60185,#60186,#60187,#60188,
#60189,#60190,#60191,#60192,#60193,#60194,#60195,#60196,#60197,#60198,#60199,
#60200,#60201,#60202,#60203,#60204,#60205,#60206,#60207,#60208,#60209,#60210,
#60211,#60212,#60213,#60214,#60215,#60216,#60217,#60218,#60219,#60220,#60221,
#60222,#60223,#60224,#60225,#60226,#60227,#60228,#60229,#60230,#60231,#60232,
#60233,#60234,#60235,#60236,#60237,#60238,#60239,#60240,#60241,#60242,#60243,
#60244,#60245,#60246,#60247,#60248,#60249,#60250,#60251,#60252,#60253,#60254,
#60255,#60256,#60257,#60258,#60259,#60260,#60261,#60262,#60263,#60264,#60265,
#60266,#60267,#60268,#60269,#60270,#60271),.UNSPECIFIED.,.F.,.F.,(4,2,2,
2,2,2,2,2,2,2,2,2,2,2,2,2,2,2,2,2,2,2,2,2,2,2,2,2,2,2,2,2,2,2,2,2,2,2,2,
2,2,2,2,4),(14.1341071652671,14.1344893630051,14.1352537584812,14.1360181539573,
14.1367825494334,14.1382687602835,14.1397549711335,14.1427273928336,14.1456998145336,
14.1486722362337,14.1546170796338,14.160561923034,14.1724516098342,14.1843412966345,
14.1962164121656,14.2080915276967,14.2318417587589,14.2555919898211,14.2793422208833,
14.3268426830077,14.3743431451322,14.4218436072566,14.469344069381,14.5643449936298,
14.6593459178787,14.7543468421275,14.9443486906252,15.1525144733886,15.3606802561521,
15.5688460389155,15.777011821679,16.1933433872059,16.6096749527328,17.0260065182597,
17.4423380837866,17.8586696493135,18.2750012148404,19.1076643458942,19.940327476948,
20.7729906080018,21.6056537390555,23.2709800011631,24.9363062632707,26.6404437310253),
 .UNSPECIFIED.) ;
#532 = B_SPLINE_CURVE_WITH_KNOTS('',3,(#60272,#60273,#60274,#60275,#60276,
#60277,#60278,#60279,#60280,#60281,#60282,#60283,#60284,#60285,#60286,#60287,
#60288,#60289,#60290,#60291,#60292,#60293,#60294,#60295,#60296,#60297,#60298,
#60299,#60300,#60301,#60302,#60303,#60304,#60305,#60306,#60307,#60308,#60309,
#60310,#60311,#60312,#60313,#60314,#60315,#60316,#60317,#60318,#60319,#60320,
#60321,#60322,#60323,#60324,#60325,#60326,#60327,#60328,#60329,#60330,#60331,
#60332,#60333,#60334,#60335,#60336,#60337,#60338,#60339,#60340,#60341,#60342,
#60343,#60344,#60345,#60346,#60347,#60348,#60349,#60350,#60351,#60352,#60353,
#60354,#60355,#60356,#60357,#60358,#60359,#60360,#60361),.UNSPECIFIED.,
 .F.,.F.,(4,2,2,2,2,2,2,2,2,2,2,2,2,2,2,2,2,2,2,2,2,2,2,2,2,2,2,2,2,2,2,
2,2,2,2,2,2,2,2,2,2,2,2,2,4),(1.62651505645876,1.66532626201344,3.33065252402689,
4.99597878604033,6.66130504805378,7.4939681790605,8.32663131006722,9.15929444107394,
9.99195757208066,10.408289137584,10.8246207030874,11.2409522685907,11.6572838340941,
12.0736153995975,12.4899469651008,12.6981127478525,12.9062785306042,13.1144443133559,
13.3226100961076,13.512611944883,13.6076128692707,13.7026137936585,13.7976147180462,
13.84511518024,13.8926156424339,13.9401161046278,13.9876165668216,14.0113667979186,
14.0351170290155,14.0588672601124,14.0707423756609,14.0826174912093,14.0945071774897,
14.10639686377,14.1123417069102,14.1182865500503,14.1212589716204,14.1242313931905,
14.1272038147606,14.1286900255456,14.1301762363306,14.1309406319289,14.1317050275272,
14.1324694231255,14.1328516209246),.UNSPECIFIED.) ;
#533 = B_SPLINE_CURVE_WITH_KNOTS('',3,(#60366,#60367,#60368,#60369,#60370,
#60371,#60372,#60373,#60374,#60375,#60376,#60377,#60378,#60379,#60380,#60381,
#60382,#60383,#60384,#60385,#60386,#60387,#60388,#60389,#60390,#60391,#60392,
#60393,#60394,#60395,#60396,#60397,#60398,#60399,#60400,#60401,#60402,#60403,
#60404,#60405,#60406,#60407,#60408,#60409,#60410,#60411,#60412,#60413,#60414,
#60415,#60416,#60417,#60418,#60419,#60420,#60421,#60422,#60423,#60424,#60425,
#60426,#60427,#60428,#60429,#60430,#60431,#60432,#60433,#60434,#60435,#60436,
#60437,#60438,#60439,#60440,#60441,#60442,#60443,#60444,#60445,#60446,#60447,
#60448,#60449,#60450,#60451,#60452,#60453),.UNSPECIFIED.,.F.,.F.,(4,2,2,
2,2,2,2,2,2,2,2,2,2,2,2,2,2,2,2,2,2,2,2,2,2,2,2,2,2,2,2,2,2,2,2,2,2,2,2,
2,2,2,2,4),(14.16170696931,14.1620898339262,14.1628555631585,14.1636212923909,
14.1643870216232,14.1658758654799,14.1673647093366,14.17034239705,14.1733200847634,
14.1762977724768,14.1822531479036,14.1882085233304,14.200119274184,14.2120300250377,
14.2239263708663,14.2358227166949,14.2596154083521,14.2834081000093,14.3072007916665,
14.354786174981,14.4023715582954,14.4499569416099,14.4975423249243,14.5927130915532,
14.6878838581821,14.7830546248109,14.9733961580687,15.1819705352013,15.390544912334,
15.5991192894666,15.8076936665992,16.2248424208645,16.6419911751297,17.059139929395,
17.4762886836602,17.8934374379255,18.3105861921908,19.1448837007213,19.9791812092518,
20.8134787177823,21.6477762263128,23.3163712433738,24.9849662604349,26.6673570370797),
 .UNSPECIFIED.) ;
#534 = B_SPLINE_CURVE_WITH_KNOTS('',3,(#60454,#60455,#60456,#60457,#60458,
#60459,#60460,#60461,#60462,#60463,#60464,#60465,#60466,#60467,#60468,#60469,
#60470,#60471,#60472,#60473,#60474,#60475,#60476,#60477,#60478,#60479,#60480,
#60481,#60482,#60483,#60484,#60485,#60486,#60487,#60488,#60489,#60490,#60491,
#60492,#60493,#60494,#60495,#60496,#60497,#60498,#60499,#60500,#60501,#60502,
#60503,#60504,#60505,#60506,#60507,#60508,#60509,#60510,#60511,#60512,#60513,
#60514,#60515,#60516,#60517,#60518,#60519,#60520,#60521,#60522,#60523,#60524,
#60525,#60526,#60527,#60528,#60529,#60530,#60531,#60532,#60533,#60534,#60535,
#60536,#60537,#60538,#60539,#60540,#60541,#60542,#60543),.UNSPECIFIED.,
 .F.,.F.,(4,2,2,2,2,2,2,2,2,2,2,2,2,2,2,2,2,2,2,2,2,2,2,2,2,2,2,2,2,2,2,
2,2,2,2,2,2,2,2,2,2,2,2,2,4),(1.65479925748035,1.6685950172178,3.3371900344356,
5.00578505165339,6.67438006887119,7.50867757748009,8.34297508608899,9.17727259469789,
10.0115701033068,10.4287188576112,10.8458676119157,11.2630163662201,11.6801651205246,
12.097313874829,12.5144626291335,12.7230370062857,12.9316113834379,13.1401857605902,
13.3487601377424,13.5391016710958,13.6342724377725,13.7294432044492,13.8246139711259,
13.8721993544642,13.9197847378026,13.9673701211409,14.0149555044792,14.0387481961484,
14.0625408878176,14.0863335794868,14.0982299253214,14.1101262711559,14.1220370214148,
14.1339477716737,14.1399031468032,14.1458585219326,14.1488362094973,14.1518138970621,
14.1547915846268,14.1562804284091,14.1577692721915,14.1585350011919,14.1593007301924,
14.1600664591929,14.1604493236931),.UNSPECIFIED.) ;
#535 = B_SPLINE_CURVE_WITH_KNOTS('',3,(#60548,#60549,#60550,#60551,#60552,
#60553,#60554,#60555,#60556,#60557,#60558,#60559,#60560,#60561,#60562,#60563,
#60564,#60565,#60566,#60567,#60568,#60569,#60570,#60571,#60572,#60573,#60574,
#60575,#60576,#60577,#60578,#60579,#60580,#60581,#60582,#60583,#60584,#60585,
#60586,#60587,#60588,#60589,#60590,#60591,#60592,#60593,#60594,#60595,#60596,
#60597,#60598,#60599,#60600,#60601,#60602,#60603,#60604,#60605,#60606,#60607,
#60608,#60609,#60610,#60611,#60612,#60613,#60614,#60615,#60616,#60617,#60618,
#60619,#60620,#60621,#60622,#60623,#60624,#60625,#60626,#60627,#60628,#60629,
#60630,#60631,#60632,#60633,#60634,#60635,#60636,#60637),.UNSPECIFIED.,
 .F.,.F.,(4,2,2,2,2,2,2,2,2,2,2,2,2,2,2,2,2,2,2,2,2,2,2,2,2,2,2,2,2,2,2,
2,2,2,2,2,2,2,2,2,2,2,2,2,4),(14.0450621945841,14.0454422402384,14.0462023315469,
14.0469624228554,14.0477225141639,14.0492002238686,14.0506779335734,14.0536333529828,
14.0565887723922,14.0595441918017,14.0654550306206,14.0713658694395,14.0831875470772,
14.095009224715,14.1068157979037,14.1186223710924,14.1422355174697,14.1658486638471,
14.1894618102245,14.2366881029792,14.2839143957339,14.3311406884886,14.3783669812434,
14.4728195667528,14.5672721522623,14.6617247377717,14.8506299087907,15.0574774983924,
15.2643250879942,15.4711726775959,15.6780202671977,16.0917154464012,16.5054106256047,
16.9191058048082,17.3328009840117,17.7464961632152,18.1601913424187,18.9875817008258,
19.8149720592328,20.6423624176398,21.4697527760468,23.1245334928609,24.7793142096749,
26.434094926489,26.553707918216),.UNSPECIFIED.) ;
#536 = B_SPLINE_CURVE_WITH_KNOTS('',3,(#60638,#60639,#60640,#60641,#60642,
#60643,#60644,#60645,#60646,#60647,#60648,#60649,#60650,#60651,#60652,#60653,
#60654,#60655,#60656,#60657,#60658,#60659,#60660,#60661,#60662,#60663,#60664,
#60665,#60666,#60667,#60668,#60669,#60670,#60671,#60672,#60673,#60674,#60675,
#60676,#60677,#60678,#60679,#60680,#60681,#60682,#60683,#60684,#60685,#60686,
#60687,#60688,#60689,#60690,#60691,#60692,#60693,#60694,#60695,#60696,#60697,
#60698,#60699,#60700,#60701,#60702,#60703,#60704,#60705,#60706,#60707,#60708,
#60709,#60710,#60711,#60712,#60713,#60714,#60715,#60716,#60717,#60718,#60719,
#60720,#60721,#60722,#60723,#60724,#60725,#60726,#60727),.UNSPECIFIED.,
 .F.,.F.,(4,2,2,2,2,2,2,2,2,2,2,2,2,2,2,2,2,2,2,2,2,2,2,2,2,2,2,2,2,2,2,
2,2,2,2,2,2,2,2,2,2,2,2,2,4),(1.53516772508572,1.65478071673876,3.30956143347751,
4.96434215021627,6.61912286695503,7.44651322532441,8.27390358369379,9.10129394206317,
9.92868430043254,10.3423794796172,10.7560746588019,11.1697698379866,11.5834650171713,
11.997160196356,12.4108553755407,12.617702965133,12.8245505547254,13.0313981443177,
13.2382457339101,13.4271509046269,13.5216034899854,13.6160560753438,13.7105086607022,
13.7577349533814,13.8049612460606,13.8521875387399,13.8994138314191,13.9230269777587,
13.9466401240983,13.9702532704379,13.9820598436077,13.9938664167775,14.0056880947879,
14.0175097727983,14.0234206118035,14.0293314508087,14.0322868703113,14.0352422898138,
14.0381977093164,14.0396754190677,14.041153128819,14.0419132202693,14.0426733117196,
14.04343340317,14.0438134488951),.UNSPECIFIED.) ;
#537 = B_SPLINE_CURVE_WITH_KNOTS('',3,(#60732,#60733,#60734,#60735,#60736,
#60737,#60738,#60739,#60740,#60741,#60742,#60743,#60744,#60745,#60746,#60747,
#60748,#60749,#60750,#60751,#60752,#60753,#60754,#60755,#60756,#60757,#60758,
#60759,#60760,#60761,#60762,#60763,#60764,#60765,#60766,#60767,#60768,#60769,
#60770,#60771,#60772,#60773,#60774,#60775,#60776,#60777,#60778,#60779,#60780,
#60781,#60782,#60783,#60784,#60785,#60786,#60787,#60788,#60789,#60790,#60791,
#60792,#60793,#60794,#60795,#60796,#60797,#60798,#60799,#60800,#60801,#60802,
#60803,#60804,#60805,#60806,#60807,#60808,#60809,#60810,#60811,#60812,#60813,
#60814,#60815,#60816,#60817,#60818,#60819),.UNSPECIFIED.,.F.,.F.,(4,2,2,
2,2,2,2,2,2,2,2,2,2,2,2,2,2,2,2,2,2,2,2,2,2,2,2,2,2,2,2,2,2,2,2,2,2,2,2,
2,2,2,2,4),(14.1204637958664,14.1208456641181,14.1216094006214,14.1223731371248,
14.1231368736281,14.1246217824304,14.1261066912327,14.1290765088373,14.1320463264419,
14.1350161440465,14.1409557792558,14.146895414465,14.1587746848834,14.1706539553018,
14.1825185736228,14.1943831919437,14.2181124285857,14.2418416652276,14.2655709018695,
14.3130293751534,14.3604878484372,14.4079463217211,14.4554047950049,14.5503217415727,
14.6452386881404,14.7401556347081,14.9299895278435,15.1379533334243,15.345917139005,
15.5538809445858,15.7618447501665,16.1777723613281,16.5936999724896,17.0096275836511,
17.4255551948126,17.8414828059741,18.2574104171357,19.0892656394587,19.9211208617817,
20.7529760841048,21.5848313064278,23.2485417510739,24.91225219572,26.6271447649371),
 .UNSPECIFIED.) ;
#538 = B_SPLINE_CURVE_WITH_KNOTS('',3,(#60820,#60821,#60822,#60823,#60824,
#60825,#60826,#60827,#60828,#60829,#60830,#60831,#60832,#60833,#60834,#60835,
#60836,#60837,#60838,#60839,#60840,#60841,#60842,#60843,#60844,#60845,#60846,
#60847,#60848,#60849,#60850,#60851,#60852,#60853,#60854,#60855,#60856,#60857,
#60858,#60859,#60860,#60861,#60862,#60863,#60864,#60865,#60866,#60867,#60868,
#60869,#60870,#60871,#60872,#60873,#60874,#60875,#60876,#60877,#60878,#60879,
#60880,#60881,#60882,#60883,#60884,#60885,#60886,#60887,#60888,#60889,#60890,
#60891,#60892,#60893,#60894,#60895,#60896,#60897,#60898,#60899,#60900,#60901,
#60902,#60903,#60904,#60905,#60906,#60907,#60908,#60909),.UNSPECIFIED.,
 .F.,.F.,(4,2,2,2,2,2,2,2,2,2,2,2,2,2,2,2,2,2,2,2,2,2,2,2,2,2,2,2,2,2,2,
2,2,2,2,2,2,2,2,2,2,2,2,2,4),(1.61252832008002,1.66371044490681,3.32742088981362,
4.99113133472043,6.65484177962724,7.48669700208064,8.31855222453405,9.15040744698745,
9.98226266944086,10.3981902806676,10.8141178918943,11.230045503121,11.6459731143477,
12.0619007255744,12.4778283368011,12.6857921424144,12.8937559480278,13.1017197536411,
13.3096835592545,13.4995174511513,13.5944343970998,13.6893513430482,13.7842682889966,
13.8317267619709,13.8791852349451,13.9266437079193,13.9741021808935,13.9978314173806,
14.0215606538677,14.0452898903548,14.0571545085984,14.0690191268419,14.0808983984921,
14.0927776701422,14.0987173059673,14.1046569417923,14.1076267597049,14.1105965776174,
14.1135663955299,14.1150513044862,14.1165362134425,14.1172999498782,14.1180636863139,
14.1188274227496,14.1192092909675),.UNSPECIFIED.) ;
#539 = B_SPLINE_CURVE_WITH_KNOTS('',3,(#60914,#60915,#60916,#60917,#60918,
#60919,#60920,#60921,#60922,#60923,#60924,#60925,#60926,#60927,#60928,#60929,
#60930,#60931,#60932,#60933,#60934,#60935,#60936,#60937,#60938,#60939,#60940,
#60941,#60942,#60943,#60944,#60945,#60946,#60947,#60948,#60949,#60950,#60951,
#60952,#60953,#60954,#60955,#60956,#60957,#60958,#60959,#60960,#60961,#60962,
#60963,#60964,#60965,#60966,#60967,#60968,#60969,#60970,#60971,#60972,#60973,
#60974,#60975,#60976,#60977,#60978,#60979,#60980,#60981,#60982,#60983,#60984,
#60985,#60986,#60987,#60988,#60989,#60990,#60991,#60992,#60993,#60994,#60995,
#60996,#60997,#60998,#60999,#61000,#61001),.UNSPECIFIED.,.F.,.F.,(4,2,2,
2,2,2,2,2,2,2,2,2,2,2,2,2,2,2,2,2,2,2,2,2,2,2,2,2,2,2,2,2,2,2,2,2,2,2,2,
2,2,2,2,4),(14.1663480270654,14.1667310037945,14.1674969572525,14.1682629107106,
14.1690288641686,14.1705181505994,14.1720074370301,14.1749860098916,14.1779645827531,
14.1809431556146,14.1869003013375,14.1928574470605,14.2047717385064,14.2166860299524,
14.2285859450541,14.2404858601559,14.2642856903595,14.2880855205631,14.3118853507666,
14.3594850111738,14.4070846715809,14.4546843319881,14.5022839923952,14.5974833132095,
14.6926826340238,14.787881954838,14.9782805964666,15.1869236817316,15.3955667669967,
15.6042098522617,15.8128529375267,16.2301391080568,16.6474252785868,17.0647114491168,
17.4819976196469,17.8992837901769,18.316569960707,19.1511423017671,19.9857146428272,
20.8202869838873,21.6548593249474,23.3240040070676,24.9931486891877,26.6718839962123),
 .UNSPECIFIED.) ;
#540 = B_SPLINE_CURVE_WITH_KNOTS('',3,(#61002,#61003,#61004,#61005,#61006,
#61007,#61008,#61009,#61010,#61011,#61012,#61013,#61014,#61015,#61016,#61017,
#61018,#61019,#61020,#61021,#61022,#61023,#61024,#61025,#61026,#61027,#61028,
#61029,#61030,#61031,#61032,#61033,#61034,#61035,#61036,#61037,#61038,#61039,
#61040,#61041,#61042,#61043,#61044,#61045,#61046,#61047,#61048,#61049,#61050,
#61051,#61052,#61053,#61054,#61055,#61056,#61057,#61058,#61059,#61060,#61061,
#61062,#61063,#61064,#61065,#61066,#61067,#61068,#61069,#61070,#61071,#61072,
#61073,#61074,#61075,#61076,#61077,#61078,#61079,#61080,#61081,#61082,#61083,
#61084,#61085,#61086,#61087,#61088,#61089,#61090,#61091),.UNSPECIFIED.,
 .F.,.F.,(4,2,2,2,2,2,2,2,2,2,2,2,2,2,2,2,2,2,2,2,2,2,2,2,2,2,2,2,2,2,2,
2,2,2,2,2,2,2,2,2,2,2,2,2,4),(1.65955405721383,1.66914468202407,3.33828936404814,
5.0074340460722,6.67657872809627,7.5111510691083,8.34572341012034,9.18029575113237,
10.0148680921444,10.4321542626504,10.8494404331564,11.2667266036625,11.6840127741685,
12.1012989446745,12.5185851151805,12.7272282004335,12.9358712856865,13.1445143709395,
13.3531574561925,13.5435560981363,13.6387554191082,13.7339547400801,13.829154061052,
13.8767537215379,13.9243533820239,13.9719530425098,14.0195527029958,14.0433525332387,
14.0671523634817,14.0909521937247,14.1028521088462,14.1147520239677,14.1266663162782,
14.1385806085888,14.1445377547441,14.1504949008994,14.1534734739771,14.1564520470547,
14.1594306201324,14.1609199066712,14.16240919321,14.1631751463293,14.1639410994486,
14.1647070525679,14.1650900291276),.UNSPECIFIED.) ;
#541 = B_SPLINE_CURVE_WITH_KNOTS('',3,(#61096,#61097,#61098,#61099,#61100,
#61101,#61102,#61103,#61104,#61105,#61106,#61107,#61108,#61109,#61110,#61111,
#61112,#61113,#61114,#61115,#61116,#61117,#61118,#61119,#61120,#61121,#61122,
#61123,#61124,#61125,#61126,#61127,#61128,#61129,#61130,#61131,#61132,#61133,
#61134,#61135,#61136,#61137,#61138,#61139,#61140,#61141,#61142,#61143,#61144,
#61145,#61146,#61147,#61148,#61149,#61150,#61151,#61152,#61153,#61154,#61155,
#61156,#61157,#61158,#61159,#61160,#61161,#61162,#61163,#61164,#61165,#61166,
#61167,#61168,#61169,#61170,#61171,#61172,#61173,#61174,#61175,#61176,#61177,
#61178,#61179,#61180,#61181,#61182,#61183,#61184),.UNSPECIFIED.,.F.,.F.,
(4,2,2,2,2,2,2,2,2,2,2,2,2,2,2,2,2,2,2,2,2,2,2,2,2,2,2,2,2,2,2,2,2,2,2,
2,2,2,2,2,2,2,2,1,4),(14.0669078689612,14.0672884427976,14.0680495904704,
14.0688107381431,14.0695718858159,14.0710516820229,14.0725314782298,14.0754910706438,
14.0784506630577,14.0814102554717,14.0873294402996,14.0932486251275,14.1050869947833,
14.1169253644391,14.1287487599683,14.1405721554975,14.164218946556,14.1878657376145,
14.2115125286729,14.2588061107899,14.3060996929068,14.3533932750237,14.4006868571406,
14.4952740213745,14.5898611856084,14.6844483498422,14.8736226783099,15.0807936570773,
15.2879646358446,15.4951356146119,15.7023065933792,16.1166485509138,16.5309905084485,
16.9453324659831,17.3596744235177,17.7740163810524,18.188358338587,19.0170422536563,
19.8457261687255,20.6744100837948,21.5030939988641,23.1604618290026,24.8178296591411,
26.4751974892797,26.5749735518018),.UNSPECIFIED.) ;
#542 = B_SPLINE_CURVE_WITH_KNOTS('',3,(#61185,#61186,#61187,#61188,#61189,
#61190,#61191,#61192,#61193,#61194,#61195,#61196,#61197,#61198,#61199,#61200,
#61201,#61202,#61203,#61204,#61205,#61206,#61207,#61208,#61209,#61210,#61211,
#61212,#61213,#61214,#61215,#61216,#61217,#61218,#61219,#61220,#61221,#61222,
#61223,#61224,#61225,#61226,#61227,#61228,#61229,#61230,#61231,#61232,#61233,
#61234,#61235,#61236,#61237,#61238,#61239,#61240,#61241,#61242,#61243,#61244,
#61245,#61246,#61247,#61248,#61249,#61250,#61251,#61252,#61253,#61254,#61255,
#61256,#61257,#61258,#61259,#61260,#61261,#61262,#61263,#61264,#61265,#61266,
#61267,#61268,#61269,#61270,#61271,#61272,#61273,#61274),.UNSPECIFIED.,
 .F.,.F.,(4,2,2,2,2,2,2,2,2,2,2,2,2,2,2,2,2,2,2,2,2,2,2,2,2,2,2,2,2,2,2,
2,2,2,2,2,2,2,2,2,2,2,2,2,4),(1.5575917676117,1.65736782987813,3.31473565975626,
4.97210348963439,6.62947131951252,7.45815523445158,8.28683914939064,9.11552306432971,
9.94420697926877,10.3585489367383,10.7728908942078,11.1872328516774,11.6015748091469,
12.0159167666164,12.430258724086,12.6374297028207,12.8446006815555,13.0517716602903,
13.258942639025,13.4481169687325,13.5427041335862,13.63729129844,13.7318784632937,
13.7791720457206,13.8264656281474,13.8737592105743,13.9210527930012,13.9446995842146,
13.9683463754281,13.9919931666415,14.0038165622482,14.0156399578549,14.0274783271072,
14.0393166963594,14.0452358809855,14.0511550656117,14.0541146579247,14.0570742502378,
14.0600338425508,14.0615136387074,14.0629934348639,14.0637545820743,14.0645157292847,
14.0652768764951,14.0656574501003),.UNSPECIFIED.) ;
#543 = B_SPLINE_CURVE_WITH_KNOTS('',3,(#61279,#61280,#61281,#61282,#61283,
#61284,#61285,#61286,#61287,#61288,#61289,#61290,#61291,#61292,#61293,#61294,
#61295,#61296,#61297,#61298,#61299,#61300,#61301,#61302,#61303,#61304,#61305,
#61306,#61307,#61308,#61309,#61310,#61311,#61312,#61313,#61314,#61315,#61316,
#61317,#61318,#61319,#61320,#61321,#61322,#61323,#61324,#61325,#61326,#61327,
#61328,#61329,#61330,#61331,#61332,#61333,#61334,#61335,#61336,#61337,#61338,
#61339,#61340,#61341,#61342,#61343,#61344,#61345,#61346,#61347,#61348,#61349,
#61350,#61351,#61352,#61353,#61354,#61355,#61356,#61357,#61358,#61359,#61360,
#61361,#61362,#61363,#61364,#61365,#61366,#61367,#61368),.UNSPECIFIED.,
 .F.,.F.,(4,2,2,2,2,2,2,2,2,2,2,2,2,2,2,2,2,2,2,2,2,2,2,2,2,2,2,2,2,2,2,
2,2,2,2,2,2,2,2,2,2,2,2,2,4),(14.0213425633806,14.0217220346764,14.0224809772678,
14.0232399198593,14.0239988624507,14.0254743060156,14.0269497495804,14.0299006367101,
14.0328515238398,14.0358024109695,14.041704185229,14.0476059594884,14.0594095080072,
14.0712130565261,14.0830013593196,14.0947896621131,14.1183662677001,14.1419428732872,
14.1655194788742,14.2126726900482,14.2598259012223,14.3069791123964,14.3541323235704,
14.4484387459185,14.5427451682666,14.6370515906147,14.8256644353109,15.0321609002033,
15.2386573650956,15.4451538299879,15.6516502948803,16.0646432246649,16.4776361544496,
16.8906290842342,17.3036220140189,17.7166149438035,18.1296078735882,18.9555937331575,
19.7815795927268,20.6075654522961,21.4335513118655,23.0855230310041,24.7374947501427,
26.3894664692814,26.5306282050422),.UNSPECIFIED.) ;
#544 = B_SPLINE_CURVE_WITH_KNOTS('',3,(#61369,#61370,#61371,#61372,#61373,
#61374,#61375,#61376,#61377,#61378,#61379,#61380,#61381,#61382,#61383,#61384,
#61385,#61386,#61387,#61388,#61389,#61390,#61391,#61392,#61393,#61394,#61395,
#61396,#61397,#61398,#61399,#61400,#61401,#61402,#61403,#61404,#61405,#61406,
#61407,#61408,#61409,#61410,#61411,#61412,#61413,#61414,#61415,#61416,#61417,
#61418,#61419,#61420,#61421,#61422,#61423,#61424,#61425,#61426,#61427,#61428,
#61429,#61430,#61431,#61432,#61433,#61434,#61435,#61436,#61437,#61438,#61439,
#61440,#61441,#61442,#61443,#61444,#61445,#61446,#61447,#61448,#61449,#61450,
#61451,#61452,#61453,#61454,#61455,#61456,#61457,#61458),.UNSPECIFIED.,
 .F.,.F.,(4,2,2,2,2,2,2,2,2,2,2,2,2,2,2,2,2,2,2,2,2,2,2,2,2,2,2,2,2,2,2,
2,2,2,2,2,2,2,2,2,2,2,2,2,4),(1.51080998338537,1.65197171958198,3.30394343916396,
4.95591515874594,6.60788687832792,7.4338727381189,8.25985859790989,9.08584445770088,
9.91183031749187,10.3248232473874,10.7378161772829,11.1508091071784,11.5638020370739,
11.9767949669693,12.3897878968648,12.5962843618126,12.8027808267603,13.0092772917081,
13.2157737566558,13.4043865999103,13.4986930215375,13.5929994431648,13.687305864792,
13.7344590756056,13.7816122864192,13.8287654972328,13.8759187080464,13.8994953134532,
13.9230719188601,13.9466485242669,13.9584368269703,13.9702251296737,13.9820286784839,
13.9938322272942,13.9997340016993,14.0056357761044,14.008586663307,14.0115375505096,
14.0144884377121,14.0159638813134,14.0174393249147,14.0181982678899,14.0189572108651,
14.0197161538403,14.020095625328),.UNSPECIFIED.) ;
#545 = B_SPLINE_CURVE_WITH_KNOTS('',3,(#61463,#61464,#61465,#61466,#61467,
#61468,#61469,#61470,#61471,#61472,#61473,#61474,#61475,#61476,#61477,#61478,
#61479,#61480,#61481,#61482,#61483,#61484,#61485,#61486,#61487,#61488,#61489,
#61490,#61491,#61492,#61493,#61494,#61495,#61496,#61497,#61498,#61499,#61500,
#61501,#61502,#61503,#61504,#61505,#61506,#61507,#61508,#61509,#61510,#61511,
#61512,#61513,#61514,#61515,#61516,#61517,#61518,#61519,#61520,#61521,#61522,
#61523,#61524,#61525,#61526,#61527,#61528,#61529,#61530,#61531,#61532,#61533,
#61534,#61535,#61536,#61537,#61538,#61539,#61540,#61541,#61542,#61543,#61544,
#61545,#61546,#61547,#61548,#61549,#61550),.UNSPECIFIED.,.F.,.F.,(4,2,2,
2,2,2,2,2,2,2,2,2,2,2,2,2,2,2,2,2,2,2,2,2,2,2,2,2,2,2,2,2,2,2,2,2,2,2,2,
2,2,2,2,4),(14.1547675290755,14.1551502263592,14.1559156209268,14.1566810154943,
14.1574464100618,14.158934591997,14.1604227739322,14.1633991378025,14.1663755016729,
14.1693518655432,14.1753045932839,14.1812573210246,14.193162776506,14.2050682319874,
14.2169592405274,14.2288502490674,14.2526322661473,14.2764142832273,14.3001963003072,
14.3477603344671,14.395324368627,14.4428884027869,14.4904524369468,14.5855805052665,
14.6807085735863,14.7758366419061,14.9660927785457,15.174564421742,15.3830360649383,
15.5915077081346,15.7999793513309,16.2169226377236,16.6338659241162,17.0508092105088,
17.4677524969015,17.8846957832941,18.3016390696867,19.135525642472,19.9694122152573,
20.8032987880425,21.6371853608278,23.3049585063983,24.9727316519689,26.6605889274289),
 .UNSPECIFIED.) ;
#546 = B_SPLINE_CURVE_WITH_KNOTS('',3,(#61551,#61552,#61553,#61554,#61555,
#61556,#61557,#61558,#61559,#61560,#61561,#61562,#61563,#61564,#61565,#61566,
#61567,#61568,#61569,#61570,#61571,#61572,#61573,#61574,#61575,#61576,#61577,
#61578,#61579,#61580,#61581,#61582,#61583,#61584,#61585,#61586,#61587,#61588,
#61589,#61590,#61591,#61592,#61593,#61594,#61595,#61596,#61597,#61598,#61599,
#61600,#61601,#61602,#61603,#61604,#61605,#61606,#61607,#61608,#61609,#61610,
#61611,#61612,#61613,#61614,#61615,#61616,#61617,#61618,#61619,#61620,#61621,
#61622,#61623,#61624,#61625,#61626,#61627,#61628,#61629,#61630,#61631,#61632,
#61633,#61634,#61635,#61636,#61637,#61638,#61639,#61640),.UNSPECIFIED.,
 .F.,.F.,(4,2,2,2,2,2,2,2,2,2,2,2,2,2,2,2,2,2,2,2,2,2,2,2,2,2,2,2,2,2,2,
2,2,2,2,2,2,2,2,2,2,2,2,2,4),(1.64768901568821,1.66777314593728,3.33554629187456,
5.00331943781184,6.67109258374912,7.50497915671776,8.3388657296864,9.17275230265505,
10.0066388756237,10.423582162108,10.8405254485923,11.2574687350766,11.674412021561,
12.0913553080453,12.5082985945296,12.7167702377718,12.9252418810139,13.1337135242561,
13.3421851674982,13.5324413032841,13.627569371177,13.72269743907,13.8178255069629,
13.8653895409093,13.9129535748558,13.9605176088023,14.0080816427487,14.031863659722,
14.0556456766952,14.0794276936684,14.091318702155,14.1032097106417,14.1151151666865,
14.1270206227314,14.1329733507539,14.1389260787763,14.1419024427876,14.1448788067988,
14.14785517081,14.1493433528156,14.1508315348212,14.1515969290159,14.1523623232106,
14.1531277174053,14.1535104145027),.UNSPECIFIED.) ;
#547 = B_SPLINE_CURVE_WITH_KNOTS('',3,(#61645,#61646,#61647,#61648,#61649,
#61650,#61651,#61652,#61653,#61654,#61655,#61656,#61657,#61658,#61659,#61660,
#61661,#61662,#61663,#61664,#61665,#61666,#61667,#61668,#61669,#61670,#61671,
#61672,#61673,#61674,#61675,#61676,#61677,#61678,#61679,#61680,#61681,#61682,
#61683,#61684,#61685,#61686,#61687,#61688,#61689,#61690,#61691,#61692,#61693,
#61694,#61695,#61696,#61697,#61698,#61699,#61700,#61701,#61702,#61703,#61704,
#61705,#61706,#61707,#61708,#61709,#61710,#61711,#61712,#61713,#61714,#61715,
#61716,#61717,#61718,#61719,#61720,#61721,#61722,#61723,#61724,#61725,#61726,
#61727,#61728,#61729,#61730,#61731,#61732),.UNSPECIFIED.,.F.,.F.,(4,2,2,
2,2,2,2,2,2,2,2,2,2,2,2,2,2,2,2,2,2,2,2,2,2,2,2,2,2,2,2,2,2,2,2,2,2,2,2,
2,2,2,2,4),(14.1455560202463,14.1459384946887,14.1467034435733,14.147468392458,
14.1482333413426,14.1497206445499,14.1512079477573,14.154182554172,14.1571571605867,
14.1601317670014,14.1660809798308,14.1720301926602,14.183928618319,14.1958270439778,
14.2077109670005,14.2195948900231,14.2433627360685,14.2671305821138,14.2908984281591,
14.3384341202498,14.3859698123404,14.4335055044311,14.4810411965218,14.5761125807031,
14.6711839648844,14.7662553490657,14.9563981174284,15.1647333909699,15.3730686645115,
15.581403938053,15.7897392115945,16.2064097586776,16.6230803057607,17.0397508528437,
17.4564213999268,17.8730919470099,18.2897624940929,19.1231035882591,19.9564446824252,
20.7897857765913,21.6231268707575,23.2898090590897,24.956491247422,26.6516061654756),
 .UNSPECIFIED.) ;
#548 = B_SPLINE_CURVE_WITH_KNOTS('',3,(#61733,#61734,#61735,#61736,#61737,
#61738,#61739,#61740,#61741,#61742,#61743,#61744,#61745,#61746,#61747,#61748,
#61749,#61750,#61751,#61752,#61753,#61754,#61755,#61756,#61757,#61758,#61759,
#61760,#61761,#61762,#61763,#61764,#61765,#61766,#61767,#61768,#61769,#61770,
#61771,#61772,#61773,#61774,#61775,#61776,#61777,#61778,#61779,#61780,#61781,
#61782,#61783,#61784,#61785,#61786,#61787,#61788,#61789,#61790,#61791,#61792,
#61793,#61794,#61795,#61796,#61797,#61798,#61799,#61800,#61801,#61802,#61803,
#61804,#61805,#61806,#61807,#61808,#61809,#61810,#61811,#61812,#61813,#61814,
#61815,#61816,#61817,#61818,#61819,#61820,#61821,#61822),.UNSPECIFIED.,
 .F.,.F.,(4,2,2,2,2,2,2,2,2,2,2,2,2,2,2,2,2,2,2,2,2,2,2,2,2,2,2,2,2,2,2,
2,2,2,2,2,2,2,2,2,2,2,2,2,4),(1.63824945861164,1.66668218836848,3.33336437673695,
5.00004656510543,6.6667287534739,7.50006984765814,8.33341094184238,9.16675203602662,
10.0000931302109,10.416763677303,10.8334342243951,11.2501047714872,11.6667753185793,
12.0834458656714,12.5001164127636,12.7084516863096,12.9167869598557,13.1251222334017,
13.3334575069478,13.523600275367,13.6186716595767,13.7137430437863,13.8088144279959,
13.8563501201007,13.9038858122055,13.9514215043103,13.9989571964151,14.0227250424676,
14.04649288852,14.0702607345724,14.0821446575986,14.0940285806248,14.1059270062631,
14.1178254319013,14.1237746447205,14.1297238575396,14.1326984639492,14.1356730703588,
14.1386476767684,14.1401349799731,14.1416222831779,14.1423872317731,14.1431521803684,
14.1439171289636,14.1442996032612),.UNSPECIFIED.) ;
#549 = B_SPLINE_CURVE_WITH_KNOTS('',3,(#61827,#61828,#61829,#61830,#61831,
#61832,#61833,#61834,#61835,#61836,#61837,#61838,#61839,#61840,#61841,#61842,
#61843,#61844,#61845,#61846,#61847,#61848,#61849,#61850,#61851,#61852,#61853,
#61854,#61855,#61856,#61857,#61858,#61859,#61860,#61861,#61862,#61863,#61864,
#61865,#61866,#61867,#61868,#61869,#61870,#61871,#61872,#61873,#61874,#61875,
#61876,#61877,#61878,#61879,#61880,#61881,#61882,#61883,#61884,#61885,#61886,
#61887,#61888,#61889,#61890,#61891,#61892,#61893,#61894,#61895,#61896,#61897,
#61898,#61899,#61900,#61901,#61902,#61903,#61904,#61905,#61906,#61907,#61908,
#61909,#61910,#61911,#61912,#61913,#61914,#61915,#61916),.UNSPECIFIED.,
 .F.,.F.,(4,2,2,2,2,2,2,2,2,2,2,2,2,2,2,2,2,2,2,2,2,2,2,2,2,2,2,2,2,2,2,
2,2,2,2,2,2,2,2,2,2,2,2,2,4),(13.9958308278975,13.9962096819733,13.9969673901248,
13.9977250982764,13.9984828064279,13.9999558119132,14.0014288173985,14.0043748283691,
14.0073208393397,14.0102668503103,14.0161588722515,14.0220508941927,14.0338349380751,
14.0456189819575,14.0573876282138,14.0691562744701,14.0926935669827,14.1162308594952,
14.1397681520078,14.1868427370329,14.233917322058,14.2809919070831,14.3280664921082,
14.4222156621585,14.5163648322087,14.6105140022589,14.7988123423594,15.0049311599118,
15.2110499774642,15.4171687950166,15.6232876125691,16.0355252476739,16.4477628827787,
16.8600005178836,17.2722381529884,17.6844757880933,18.0967134231981,18.9211886934078,
19.7456639636175,20.5701392338272,21.3946145040369,23.0435650444562,24.6925155848756,
26.341466125295,26.5058166411774),.UNSPECIFIED.) ;
#550 = B_SPLINE_CURVE_WITH_KNOTS('',3,(#61917,#61918,#61919,#61920,#61921,
#61922,#61923,#61924,#61925,#61926,#61927,#61928,#61929,#61930,#61931,#61932,
#61933,#61934,#61935,#61936,#61937,#61938,#61939,#61940,#61941,#61942,#61943,
#61944,#61945,#61946,#61947,#61948,#61949,#61950,#61951,#61952,#61953,#61954,
#61955,#61956,#61957,#61958,#61959,#61960,#61961,#61962,#61963,#61964,#61965,
#61966,#61967,#61968,#61969,#61970,#61971,#61972,#61973,#61974,#61975,#61976,
#61977,#61978,#61979,#61980,#61981,#61982,#61983,#61984,#61985,#61986,#61987,
#61988,#61989,#61990,#61991,#61992,#61993,#61994,#61995,#61996,#61997,#61998,
#61999,#62000,#62001,#62002,#62003,#62004,#62005,#62006),.UNSPECIFIED.,
 .F.,.F.,(4,2,2,2,2,2,2,2,2,2,2,2,2,2,2,2,2,2,2,2,2,2,2,2,2,2,2,2,2,2,2,
2,2,2,2,2,2,2,2,2,2,2,2,2,4),(1.48460002454131,1.64895054067987,3.29790108135973,
4.9468516220396,6.59580216271946,7.42027743305939,8.24475270339932,9.06922797373926,
9.89370324407919,10.3059408792492,10.7181785144191,11.1304161495891,11.5426537847591,
11.954891419929,12.367129055099,12.573247872684,12.779366690269,12.9854855078539,
13.1916043254389,13.3799026654271,13.4740518354212,13.5682010054153,13.6623501754094,
13.7094247604064,13.7564993454035,13.8035739304005,13.8506485153976,13.8741858078961,
13.8977231003946,13.9212603928931,13.9330290391424,13.9447976853916,13.9565817297195,
13.9683657740474,13.9742577962114,13.9801498183753,13.9830958294573,13.9860418405393,
13.9889878516212,13.9904608571622,13.9919338627032,13.9926915708602,13.9934492790172,
13.9942069871742,13.9945858412527),.UNSPECIFIED.) ;
#551 = B_SPLINE_CURVE_WITH_KNOTS('',3,(#62011,#62012,#62013,#62014,#62015,
#62016,#62017,#62018,#62019,#62020,#62021,#62022,#62023,#62024,#62025,#62026,
#62027,#62028,#62029,#62030,#62031,#62032,#62033,#62034,#62035,#62036,#62037,
#62038,#62039,#62040,#62041,#62042,#62043,#62044,#62045,#62046,#62047,#62048,
#62049,#62050,#62051,#62052,#62053,#62054,#62055,#62056,#62057,#62058,#62059,
#62060,#62061,#62062,#62063,#62064,#62065,#62066,#62067,#62068,#62069,#62070,
#62071,#62072,#62073,#62074,#62075,#62076,#62077,#62078,#62079,#62080,#62081,
#62082,#62083,#62084,#62085,#62086,#62087,#62088,#62089,#62090,#62091,#62092,
#62093,#62094,#62095,#62096,#62097,#62098,#62099),.UNSPECIFIED.,.F.,.F.,
(4,2,2,2,2,2,2,2,2,2,2,2,2,2,2,2,2,2,2,2,2,2,2,2,2,2,2,2,2,2,2,2,2,2,2,
2,2,2,2,2,2,2,2,1,4),(14.0868029211861,14.0871839758337,14.0879460851289,
14.0887081944242,14.0894703037194,14.0909519997192,14.092433695719,14.0953970877186,
14.0983604797182,14.1013238717178,14.107250655717,14.1131774397162,14.1250310077145,
14.1368845757129,14.1487232877793,14.1605619998456,14.1842394239783,14.2079168481109,
14.2315942722436,14.2789491205089,14.3263039687743,14.3736588170396,14.421013665305,
14.5157233618356,14.6104330583663,14.705142754897,14.8945621479584,15.1020276442232,
15.309493140488,15.5169586367529,15.7244241330177,16.1393551255474,16.5542861180771,
16.9692171106068,17.3841481031365,17.7990790956662,18.2140100881959,19.0438720732552,
19.8737340583146,20.703596043374,21.5334580284334,23.1931819985521,24.8529059686708,
26.5126299387896,26.594348067054),.UNSPECIFIED.) ;
#552 = B_SPLINE_CURVE_WITH_KNOTS('',3,(#62100,#62101,#62102,#62103,#62104,
#62105,#62106,#62107,#62108,#62109,#62110,#62111,#62112,#62113,#62114,#62115,
#62116,#62117,#62118,#62119,#62120,#62121,#62122,#62123,#62124,#62125,#62126,
#62127,#62128,#62129,#62130,#62131,#62132,#62133,#62134,#62135,#62136,#62137,
#62138,#62139,#62140,#62141,#62142,#62143,#62144,#62145,#62146,#62147,#62148,
#62149,#62150,#62151,#62152,#62153,#62154,#62155,#62156,#62157,#62158,#62159,
#62160,#62161,#62162,#62163,#62164,#62165,#62166,#62167,#62168,#62169,#62170,
#62171,#62172,#62173,#62174,#62175,#62176,#62177,#62178,#62179,#62180,#62181,
#62182,#62183,#62184,#62185,#62186,#62187,#62188,#62189),.UNSPECIFIED.,
 .F.,.F.,(4,2,2,2,2,2,2,2,2,2,2,2,2,2,2,2,2,2,2,2,2,2,2,2,2,2,2,2,2,2,2,
2,2,2,2,2,2,2,2,2,2,2,2,2,4),(1.57800584185246,1.65972397001552,3.31944794003104,
4.97917191004656,6.63889588006208,7.46875786506984,8.2986198500776,9.12848183508536,
9.95834382009312,10.373274812597,10.7882058051009,11.2031367976048,11.6180677901086,
12.0329987826125,12.4479297751164,12.6553952713683,12.8628607676203,13.0703262638722,
13.2777917601242,13.4672111537424,13.5619208505516,13.6566305473607,13.7513402441698,
13.7986950925744,13.846049940979,13.8934047893835,13.9407596377881,13.9644370619904,
13.9881144861927,14.0117919103949,14.0236306224961,14.0354693345972,14.0473229019233,
14.0591764692495,14.0651032529125,14.0710300365756,14.0739934284071,14.0769568202386,
14.0799202120702,14.0814019079859,14.0828836039017,14.0836457139642,14.0844078240268,
14.0851699340893,14.0855509891206),.UNSPECIFIED.) ;
#553 = B_SPLINE_CURVE_WITH_KNOTS('',3,(#62194,#62195,#62196,#62197,#62198,
#62199,#62200,#62201,#62202,#62203,#62204,#62205,#62206,#62207,#62208,#62209,
#62210,#62211,#62212,#62213,#62214,#62215,#62216,#62217,#62218,#62219,#62220,
#62221,#62222,#62223,#62224,#62225,#62226,#62227,#62228,#62229,#62230,#62231,
#62232,#62233,#62234,#62235,#62236,#62237,#62238,#62239,#62240,#62241,#62242,
#62243,#62244,#62245,#62246,#62247,#62248,#62249,#62250,#62251,#62252,#62253,
#62254,#62255,#62256,#62257,#62258,#62259,#62260,#62261,#62262,#62263,#62264,
#62265,#62266,#62267,#62268,#62269,#62270,#62271,#62272,#62273,#62274,#62275,
#62276,#62277,#62278,#62279,#62280,#62281),.UNSPECIFIED.,.F.,.F.,(4,2,2,
2,2,2,2,2,2,2,2,2,2,2,2,2,2,2,2,2,2,2,2,2,2,2,2,2,2,2,2,2,2,2,2,2,2,2,2,
2,2,2,2,4),(14.1686729957178,14.1690560284224,14.1698220938314,14.1705881592404,
14.1713542246494,14.1728437329402,14.1743332412309,14.1773122578124,14.1802912743938,
14.1832702909753,14.1892283241382,14.1951863573012,14.2071024236271,14.2190184899529,
14.2309201930728,14.2428218961926,14.2666253024322,14.2904287086718,14.3142321149114,
14.3618389273906,14.4094457398698,14.457052552349,14.5046593648282,14.5998729897866,
14.695086614745,14.7903002397034,14.9807274896203,15.1894049946999,15.3980824997795,
15.6067600048591,15.8154375099388,16.232792520098,16.6501475302573,17.0675025404165,
17.4848575505757,17.902212560735,18.3195675708942,19.1542775912127,19.9889876115312,
20.8236976318497,21.6584076521682,23.3278276928052,24.9972477334421,26.6741519500694),
 .UNSPECIFIED.) ;
#554 = B_SPLINE_CURVE_WITH_KNOTS('',3,(#62282,#62283,#62284,#62285,#62286,
#62287,#62288,#62289,#62290,#62291,#62292,#62293,#62294,#62295,#62296,#62297,
#62298,#62299,#62300,#62301,#62302,#62303,#62304,#62305,#62306,#62307,#62308,
#62309,#62310,#62311,#62312,#62313,#62314,#62315,#62316,#62317,#62318,#62319,
#62320,#62321,#62322,#62323,#62324,#62325,#62326,#62327,#62328,#62329,#62330,
#62331,#62332,#62333,#62334,#62335,#62336,#62337,#62338,#62339,#62340,#62341,
#62342,#62343,#62344,#62345,#62346,#62347,#62348,#62349,#62350,#62351,#62352,
#62353,#62354,#62355,#62356,#62357,#62358,#62359,#62360,#62361,#62362,#62363,
#62364,#62365,#62366,#62367,#62368,#62369,#62370,#62371),.UNSPECIFIED.,
 .F.,.F.,(4,2,2,2,2,2,2,2,2,2,2,2,2,2,2,2,2,2,2,2,2,2,2,2,2,2,2,2,2,2,2,
2,2,2,2,2,2,2,2,2,2,2,2,2,4),(1.66193586464491,1.66942004054979,3.33884008109958,
5.00826012164937,6.67768016219916,7.51239018247405,8.34710020274895,9.18181022302385,
10.0165202432987,10.4338752534362,10.8512302635736,11.2685852737111,11.6859402838485,
12.103295293986,12.5206503041234,12.7293278091921,12.9380053142609,13.1466828193296,
13.3553603243983,13.545787573842,13.6410011985639,13.7362148232857,13.8314284480076,
13.8790352603685,13.9266420727294,13.9742488850903,14.0218556974513,14.0456591036317,
14.0694625098122,14.0932659159926,14.1051676190829,14.1170693221731,14.1289853886477,
14.1409014551223,14.1468594883595,14.1528175215968,14.1557965382155,14.1587755548341,
14.1617545714527,14.1632440797621,14.1647335880714,14.1654996538429,14.1662657196144,
14.1670317853859,14.1674148182716),.UNSPECIFIED.) ;
#555 = B_SPLINE_CURVE_WITH_KNOTS('',3,(#62376,#62377,#62378,#62379,#62380,
#62381,#62382,#62383,#62384,#62385,#62386,#62387,#62388,#62389,#62390,#62391,
#62392,#62393,#62394,#62395,#62396,#62397,#62398,#62399,#62400,#62401,#62402,
#62403,#62404,#62405,#62406,#62407,#62408,#62409,#62410,#62411,#62412,#62413,
#62414,#62415,#62416,#62417,#62418,#62419,#62420,#62421,#62422,#62423,#62424,
#62425,#62426,#62427,#62428,#62429,#62430,#62431,#62432,#62433,#62434,#62435,
#62436,#62437,#62438,#62439,#62440,#62441,#62442,#62443,#62444,#62445,#62446,
#62447,#62448,#62449,#62450,#62451,#62452,#62453,#62454,#62455,#62456,#62457,
#62458,#62459,#62460,#62461,#62462,#62463,#62464),.UNSPECIFIED.,.F.,.F.,
(4,2,2,2,2,2,2,2,2,2,2,2,2,2,2,2,2,2,2,2,2,2,2,2,2,2,2,2,2,2,2,2,2,2,2,
2,2,2,2,2,2,2,2,1,4),(14.1046764400768,14.1050579266305,14.1058208997379,
14.1065838728453,14.1073468459527,14.1088302481455,14.1103136503384,14.113280454724,
14.1162472591097,14.1192140634954,14.1251476722667,14.1310812810381,14.1429484985808,
14.1548157161235,14.1666681853681,14.1785206546127,14.202225593102,14.2259305315912,
14.2496354700804,14.2970453470589,14.3444552240374,14.3918651010159,14.4392749779944,
14.5340947319514,14.6289144859084,14.7237342398654,14.9133737477793,15.1211038389457,
15.3288339301121,15.5365640212784,15.7442941124448,16.1597542947775,16.5752144771102,
16.990674659443,17.4061348417757,17.8215950241084,18.2370552064411,19.0679755711066,
19.8988959357721,20.7298163004375,21.560736665103,23.2225773944339,24.8844181237648,
26.5462588530957,26.6117601472044),.UNSPECIFIED.) ;
#556 = B_SPLINE_CURVE_WITH_KNOTS('',3,(#62465,#62466,#62467,#62468,#62469,
#62470,#62471,#62472,#62473,#62474,#62475,#62476,#62477,#62478,#62479,#62480,
#62481,#62482,#62483,#62484,#62485,#62486,#62487,#62488,#62489,#62490,#62491,
#62492,#62493,#62494,#62495,#62496,#62497,#62498,#62499,#62500,#62501,#62502,
#62503,#62504,#62505,#62506,#62507,#62508,#62509,#62510,#62511,#62512,#62513,
#62514,#62515,#62516,#62517,#62518,#62519,#62520,#62521,#62522,#62523,#62524,
#62525,#62526,#62527,#62528,#62529,#62530,#62531,#62532,#62533,#62534,#62535,
#62536,#62537,#62538,#62539,#62540,#62541,#62542,#62543,#62544,#62545,#62546,
#62547,#62548,#62549,#62550,#62551,#62552,#62553,#62554),.UNSPECIFIED.,
 .F.,.F.,(4,2,2,2,2,2,2,2,2,2,2,2,2,2,2,2,2,2,2,2,2,2,2,2,2,2,2,2,2,2,2,
2,2,2,2,2,2,2,2,2,2,2,2,2,4),(1.59633943522304,1.66184072937422,3.32368145874844,
4.98552218812266,6.64736291749688,7.47828328218399,8.3092036468711,9.14012401155821,
9.97104437624532,10.3865045585889,10.8019647409324,11.217424923276,11.6328851056195,
12.0483452879631,12.4638054703066,12.6715355614784,12.8792656526502,13.086995743822,
13.2947258349938,13.4843653425812,13.5791850963749,13.6740048501686,13.7688246039623,
13.8162344808592,13.8636443577561,13.9110542346529,13.9584641115498,13.9821690499982,
14.0058739884466,14.0295789268951,14.0414313961193,14.0532838653435,14.0651510830035,
14.0770183006634,14.0829519094934,14.0888855183234,14.0918523227384,14.0948191271534,
14.0977859315684,14.0992693337759,14.1007527359834,14.1015157096051,14.1022786832268,
14.1030416568486,14.1034231436594),.UNSPECIFIED.) ;
#557 = B_SPLINE_CURVE_WITH_KNOTS('',3,(#62559,#62560,#62561,#62562,#62563,
#62564,#62565,#62566,#62567,#62568,#62569,#62570,#62571,#62572,#62573,#62574,
#62575,#62576,#62577,#62578,#62579,#62580,#62581,#62582,#62583,#62584,#62585,
#62586,#62587,#62588,#62589,#62590,#62591,#62592,#62593,#62594,#62595,#62596,
#62597,#62598,#62599,#62600,#62601,#62602,#62603,#62604,#62605,#62606,#62607,
#62608,#62609,#62610,#62611,#62612,#62613,#62614,#62615,#62616,#62617,#62618,
#62619,#62620,#62621,#62622,#62623,#62624,#62625,#62626,#62627,#62628,#62629,
#62630,#62631,#62632,#62633,#62634,#62635,#62636,#62637,#62638,#62639,#62640,
#62641,#62642,#62643,#62644,#62645,#62646,#62647,#62648),.UNSPECIFIED.,
 .F.,.F.,(4,2,2,2,2,2,2,2,2,2,2,2,2,2,2,2,2,2,2,2,2,2,2,2,2,2,2,2,2,2,2,
2,2,2,2,2,2,2,2,2,2,2,2,2,4),(13.9686134586717,13.9689916543654,13.9697480457528,
13.9705044371402,13.9712608285275,13.9727312318299,13.9742016351324,13.9771424417372,
13.980083248342,13.9830240549468,13.9889056681565,13.9947872813661,14.0065505077854,
14.0183137342047,14.0300614031915,14.0418090721782,14.0653044101518,14.0887997481254,
14.112295086099,14.1592857620462,14.2062764379934,14.2532671139406,14.3002577898878,
14.3942391417821,14.4882204936765,14.5822018455709,14.7701645493596,14.9758804783754,
15.1815964073912,15.3873123364069,15.5930282654227,16.0044601234543,16.4158919814858,
16.8273238395174,17.2387556975489,17.6501875555805,18.061619413612,18.8844831296751,
19.7073468457382,20.5302105618013,21.3530742778644,22.9988017099906,24.6445291421168,
26.290256574243,26.4793600109925),.UNSPECIFIED.) ;
#558 = B_SPLINE_CURVE_WITH_KNOTS('',3,(#62649,#62650,#62651,#62652,#62653,
#62654,#62655,#62656,#62657,#62658,#62659,#62660,#62661,#62662,#62663,#62664,
#62665,#62666,#62667,#62668,#62669,#62670,#62671,#62672,#62673,#62674,#62675,
#62676,#62677,#62678,#62679,#62680,#62681,#62682,#62683,#62684,#62685,#62686,
#62687,#62688,#62689,#62690,#62691,#62692,#62693,#62694,#62695,#62696,#62697,
#62698,#62699,#62700,#62701,#62702,#62703,#62704,#62705,#62706,#62707,#62708,
#62709,#62710,#62711,#62712,#62713,#62714,#62715,#62716,#62717,#62718,#62719,
#62720,#62721,#62722,#62723,#62724,#62725,#62726,#62727,#62728,#62729,#62730,
#62731,#62732,#62733,#62734,#62735,#62736,#62737,#62738),.UNSPECIFIED.,
 .F.,.F.,(4,2,2,2,2,2,2,2,2,2,2,2,2,2,2,2,2,2,2,2,2,2,2,2,2,2,2,2,2,2,2,
2,2,2,2,2,2,2,2,2,2,2,2,2,4),(1.45662399537187,1.64572743182393,3.29145486364787,
4.9371822954718,6.58290972729574,7.4057734432077,8.22863715911967,9.05150087503164,
9.8743645909436,10.2857964488996,10.6972283068556,11.1086601648116,11.5200920227675,
11.9315238807235,12.3429557386795,12.5486716676575,12.7543875966355,12.9601035256135,
13.1658194545915,13.3537821585869,13.4477635105846,13.5417448625823,13.6357262145801,
13.6827168905789,13.7297075665778,13.7766982425766,13.8236889185755,13.8471842565749,
13.8706795945744,13.8941749325738,13.9059226015735,13.9176702705732,13.9294334979076,
13.941196725242,13.9470783389092,13.9529599525763,13.9559007594099,13.9588415662435,
13.9617823730771,13.9632527764939,13.9647231799107,13.9654795712734,13.9662359626361,
13.9669923539988,13.9673705496801),.UNSPECIFIED.) ;
#559 = B_SPLINE_CURVE_WITH_KNOTS('',3,(#62743,#62744,#62745,#62746,#62747,
#62748,#62749,#62750,#62751,#62752,#62753,#62754,#62755,#62756,#62757,#62758,
#62759,#62760,#62761,#62762,#62763,#62764,#62765,#62766,#62767,#62768,#62769,
#62770,#62771,#62772,#62773,#62774,#62775,#62776,#62777,#62778,#62779,#62780,
#62781,#62782,#62783,#62784,#62785,#62786,#62787,#62788,#62789,#62790,#62791,
#62792,#62793,#62794,#62795,#62796,#62797,#62798,#62799,#62800,#62801,#62802,
#62803,#62804,#62805,#62806,#62807,#62808,#62809,#62810,#62811,#62812,#62813,
#62814,#62815,#62816,#62817,#62818,#62819,#62820,#62821,#62822,#62823,#62824,
#62825,#62826,#62827,#62828,#62829,#62830),.UNSPECIFIED.,.F.,.F.,(4,2,2,
2,2,2,2,2,2,2,2,2,2,2,2,2,2,2,2,2,2,2,2,2,2,2,2,2,2,2,2,2,2,2,2,2,2,2,2,
2,2,2,2,4),(14.1341071619772,14.1344893601054,14.1352537563619,14.1360181526184,
14.1367825488748,14.1382687596458,14.1397549704169,14.1427273919589,14.1456998135009,
14.148672235043,14.1546170781271,14.1605619212112,14.1724516073793,14.1843412935475,
14.1962164091354,14.2080915247234,14.2318417558993,14.2555919870753,14.2793422182512,
14.326842680603,14.3743431429549,14.4218436053067,14.4693440676586,14.5643449923623,
14.659345917066,14.7543468417697,14.944348691177,15.1525144738915,15.3606802566059,
15.5688460393203,15.7770118220347,16.1933433874636,16.6096749528924,17.0260065183213,
17.4423380837501,17.858669649179,18.2750012146078,19.1076643454655,19.9403274763232,
20.7729906071809,21.6056537380386,23.2709799997539,24.9363062614693,26.640443728447),
 .UNSPECIFIED.) ;
#560 = B_SPLINE_CURVE_WITH_KNOTS('',3,(#62831,#62832,#62833,#62834,#62835,
#62836,#62837,#62838,#62839,#62840,#62841,#62842,#62843,#62844,#62845,#62846,
#62847,#62848,#62849,#62850,#62851,#62852,#62853,#62854,#62855,#62856,#62857,
#62858,#62859,#62860,#62861,#62862,#62863,#62864,#62865,#62866,#62867,#62868,
#62869,#62870,#62871,#62872,#62873,#62874,#62875,#62876,#62877,#62878,#62879,
#62880,#62881,#62882,#62883,#62884,#62885,#62886,#62887,#62888,#62889,#62890,
#62891,#62892,#62893,#62894,#62895,#62896,#62897,#62898,#62899,#62900,#62901,
#62902,#62903,#62904,#62905,#62906,#62907,#62908,#62909,#62910,#62911,#62912,
#62913,#62914,#62915,#62916,#62917,#62918,#62919,#62920),.UNSPECIFIED.,
 .F.,.F.,(4,2,2,2,2,2,2,2,2,2,2,2,2,2,2,2,2,2,2,2,2,2,2,2,2,2,2,2,2,2,2,
2,2,2,2,2,2,2,2,2,2,2,2,2,4),(1.62651505645996,1.66532626207607,3.33065252415214,
4.9959787862282,6.66130504830427,7.4939681793423,8.32663131038034,9.15929444141837,
9.99195757245641,10.4082891379754,10.8246207034944,11.2409522690135,11.6572838345325,
12.0736154000515,12.4899469655705,12.69811274833,12.9062785310895,13.114444313849,
13.3226100966085,13.5126119449433,13.6076128691107,13.702613793278,13.7976147174454,
13.8451151795291,13.8926156416128,13.9401161036965,13.9876165657801,14.011366796822,
14.0351170278638,14.0588672589057,14.0707423744266,14.0826174899475,14.0945071767465,
14.1063968635454,14.1123417069449,14.1182865503443,14.1212589720441,14.1242313937438,
14.1272038154435,14.1286900262934,14.1301762371433,14.1309406333205,14.1317050294977,
14.1324694256748,14.1328516237634),.UNSPECIFIED.) ;
#561 = B_SPLINE_CURVE_WITH_KNOTS('',3,(#62925,#62926,#62927,#62928,#62929,
#62930,#62931,#62932,#62933,#62934,#62935,#62936,#62937,#62938,#62939,#62940,
#62941,#62942,#62943,#62944,#62945,#62946,#62947,#62948,#62949,#62950,#62951,
#62952,#62953,#62954,#62955,#62956,#62957,#62958,#62959,#62960,#62961,#62962,
#62963,#62964,#62965,#62966,#62967,#62968,#62969,#62970,#62971,#62972,#62973,
#62974,#62975,#62976,#62977,#62978,#62979,#62980,#62981,#62982,#62983,#62984,
#62985,#62986,#62987,#62988,#62989,#62990,#62991,#62992,#62993,#62994,#62995,
#62996,#62997,#62998,#62999,#63000,#63001,#63002,#63003,#63004,#63005,#63006,
#63007,#63008,#63009,#63010,#63011,#63012),.UNSPECIFIED.,.F.,.F.,(4,2,2,
2,2,2,2,2,2,2,2,2,2,2,2,2,2,2,2,2,2,2,2,2,2,2,2,2,2,2,2,2,2,2,2,2,2,2,2,
2,2,2,2,4),(14.1617069747248,14.1620898390495,14.1628555676989,14.1636212963483,
14.1643870249977,14.165875868894,14.1673647127904,14.1703424005831,14.1733200883758,
14.1762977761685,14.1822531517539,14.1882085273393,14.2001192785101,14.2120300296809,
14.2239263755092,14.2358227213376,14.2596154129943,14.2834081046509,14.3072007963076,
14.354786179621,14.4023715629344,14.4499569462477,14.4975423295611,14.5927130961878,
14.6878838628146,14.7830546294413,14.9733961626948,15.1819705398313,15.3905449169678,
15.5991192941043,15.8076936712408,16.2248424255138,16.6419911797868,17.0591399340598,
17.4762886883328,17.8934374426059,18.3105861968789,19.1448837054249,19.9791812139709,
20.813478722517,21.647776231063,23.3163712481551,24.9849662652471,26.6673570419534),
 .UNSPECIFIED.) ;
#562 = B_SPLINE_CURVE_WITH_KNOTS('',3,(#63013,#63014,#63015,#63016,#63017,
#63018,#63019,#63020,#63021,#63022,#63023,#63024,#63025,#63026,#63027,#63028,
#63029,#63030,#63031,#63032,#63033,#63034,#63035,#63036,#63037,#63038,#63039,
#63040,#63041,#63042,#63043,#63044,#63045,#63046,#63047,#63048,#63049,#63050,
#63051,#63052,#63053,#63054,#63055,#63056,#63057,#63058,#63059,#63060,#63061,
#63062,#63063,#63064,#63065,#63066,#63067,#63068,#63069,#63070,#63071,#63072,
#63073,#63074,#63075,#63076,#63077,#63078,#63079,#63080,#63081,#63082,#63083,
#63084,#63085,#63086,#63087,#63088,#63089,#63090,#63091,#63092,#63093,#63094,
#63095,#63096,#63097,#63098,#63099,#63100,#63101,#63102),.UNSPECIFIED.,
 .F.,.F.,(4,2,2,2,2,2,2,2,2,2,2,2,2,2,2,2,2,2,2,2,2,2,2,2,2,2,2,2,2,2,2,
2,2,2,2,2,2,2,2,2,2,2,2,2,4),(1.65479925748125,1.66859501726426,3.33719003452851,
5.00578505179277,6.67438006905703,7.50867757768916,8.34297508632129,9.17727259495341,
10.0115701035855,10.4287188579016,10.8458676122177,11.2630163665337,11.6801651208498,
12.0973138751659,12.5144626294819,12.72303700664,12.931611383798,13.140185760956,
13.3487601381141,13.5391016709644,13.6342724373896,13.7294432038147,13.8246139702399,
13.8721993534525,13.9197847366651,13.9673701198777,14.0149555030903,14.0387481946965,
14.0625408863028,14.0863335779091,14.0982299237123,14.1101262695154,14.1220370206378,
14.1339477717601,14.1399031473213,14.1458585228825,14.1488362106631,14.1518138984437,
14.1547915862243,14.1562804301146,14.1577692740048,14.158535003378,14.1593007327512,
14.1600664621244,14.160449326811),.UNSPECIFIED.) ;
#563 = B_SPLINE_CURVE_WITH_KNOTS('',3,(#63107,#63108,#63109,#63110,#63111,
#63112,#63113,#63114,#63115,#63116,#63117,#63118,#63119,#63120,#63121,#63122,
#63123,#63124,#63125,#63126,#63127,#63128,#63129,#63130,#63131,#63132,#63133,
#63134,#63135,#63136,#63137,#63138,#63139,#63140,#63141,#63142,#63143,#63144,
#63145,#63146,#63147,#63148,#63149,#63150,#63151,#63152,#63153,#63154,#63155,
#63156,#63157,#63158,#63159,#63160,#63161,#63162,#63163,#63164,#63165,#63166,
#63167,#63168,#63169,#63170,#63171,#63172,#63173,#63174,#63175,#63176,#63177,
#63178,#63179,#63180,#63181,#63182,#63183,#63184,#63185,#63186,#63187,#63188,
#63189,#63190,#63191,#63192,#63193,#63194,#63195,#63196),.UNSPECIFIED.,
 .F.,.F.,(4,2,2,2,2,2,2,2,2,2,2,2,2,2,2,2,2,2,2,2,2,2,2,2,2,2,2,2,2,2,2,
2,2,2,2,2,2,2,2,2,2,2,2,2,4),(14.0450621959468,14.0454422411604,14.0462023315876,
14.0469624220149,14.0477225124421,14.049200222119,14.0506779317958,14.0536333511496,
14.0565887705033,14.0595441898571,14.0654550285646,14.071365867272,14.083187544687,
14.095009222102,14.1068157952781,14.1186223684541,14.1422355148063,14.1658486611584,
14.1894618075106,14.2366881002148,14.2839143929191,14.3311406856234,14.3783669783277,
14.4728195637362,14.5672721491448,14.6617247345534,14.8506299053705,15.0574774949646,
15.2643250845586,15.4711726741527,15.6780202637467,16.0917154429348,16.5054106221229,
16.919105801311,17.3328009804992,17.7464961596873,18.1601913388754,18.9875816972516,
19.8149720556278,20.642362414004,21.4697527723802,23.1245334891327,24.7793142058851,
26.4340949226375,26.553707914304),.UNSPECIFIED.) ;
#564 = B_SPLINE_CURVE_WITH_KNOTS('',3,(#63197,#63198,#63199,#63200,#63201,
#63202,#63203,#63204,#63205,#63206,#63207,#63208,#63209,#63210,#63211,#63212,
#63213,#63214,#63215,#63216,#63217,#63218,#63219,#63220,#63221,#63222,#63223,
#63224,#63225,#63226,#63227,#63228,#63229,#63230,#63231,#63232,#63233,#63234,
#63235,#63236,#63237,#63238,#63239,#63240,#63241,#63242,#63243,#63244,#63245,
#63246,#63247,#63248,#63249,#63250,#63251,#63252,#63253,#63254,#63255,#63256,
#63257,#63258,#63259,#63260,#63261,#63262,#63263,#63264,#63265,#63266,#63267,
#63268,#63269,#63270,#63271,#63272,#63273,#63274,#63275,#63276,#63277,#63278,
#63279,#63280,#63281,#63282,#63283,#63284,#63285,#63286),.UNSPECIFIED.,
 .F.,.F.,(4,2,2,2,2,2,2,2,2,2,2,2,2,2,2,2,2,2,2,2,2,2,2,2,2,2,2,2,2,2,2,
2,2,2,2,2,2,2,2,2,2,2,2,2,4),(1.5351677250863,1.654780716772,3.30956143354401,
4.96434215031601,6.61912286708802,7.44651322547402,8.27390358386002,9.10129394224603,
9.92868430063203,10.342379479825,10.756074659018,11.169769838211,11.583465017404,
11.997160196597,12.41085537579,12.6177029653865,12.824550554983,13.0313981445795,
13.238245734176,13.4271509053336,13.5216034909124,13.6160560764912,13.71050866207,
13.7577349548593,13.8049612476487,13.8521875404381,13.8994138332275,13.9230269796222,
13.9466401260169,13.9702532724116,13.982059845609,13.9938664188063,14.0056880957911,
14.0175097727758,14.0234206112682,14.0293314497606,14.0322868690068,14.035242288253,
14.0381977074992,14.0396754171223,14.0411531267454,14.0419132173428,14.0426733079402,
14.0434333985377,14.0438134438364),.UNSPECIFIED.) ;
#565 = SHAPE_REPRESENTATION_RELATIONSHIP('SRR','None',#63879,#580) ;
#566 = SHAPE_REPRESENTATION_RELATIONSHIP('SRR','None',#63880,#581) ;
#567 = SHAPE_REPRESENTATION_RELATIONSHIP('SRR','None',#63881,#582) ;
#568 = SHAPE_REPRESENTATION_RELATIONSHIP('SRR','None',#63882,#583) ;
#569 = SHAPE_REPRESENTATION_RELATIONSHIP('SRR','None',#63883,#584) ;
#570 = SHAPE_REPRESENTATION_RELATIONSHIP('SRR','None',#63884,#585) ;
#571 = SHAPE_REPRESENTATION_RELATIONSHIP('SRR','None',#63885,#586) ;
#572 = SHAPE_REPRESENTATION_RELATIONSHIP('SRR','None',#63886,#587) ;
#573 = SHAPE_REPRESENTATION_RELATIONSHIP('SRR','None',#63887,#588) ;
#574 = SHAPE_REPRESENTATION_RELATIONSHIP('SRR','None',#63888,#589) ;
#575 = SHAPE_REPRESENTATION_RELATIONSHIP('SRR','None',#63889,#590) ;
#576 = SHAPE_REPRESENTATION_RELATIONSHIP('SRR','None',#63890,#591) ;
#577 = SHAPE_REPRESENTATION_RELATIONSHIP('SRR','None',#63891,#592) ;
#578 = SHAPE_REPRESENTATION_RELATIONSHIP('SRR','None',#63892,#593) ;
#579 = SHAPE_REPRESENTATION_RELATIONSHIP('SRR','None',#63893,#594) ;
#580 = ADVANCED_BREP_SHAPE_REPRESENTATION('',(#610),#63809) ;
#581 = ADVANCED_BREP_SHAPE_REPRESENTATION('',(#611),#63810) ;
#582 = ADVANCED_BREP_SHAPE_REPRESENTATION('',(#612),#63811) ;
#583 = ADVANCED_BREP_SHAPE_REPRESENTATION('',(#613),#63812) ;
#584 = ADVANCED_BREP_SHAPE_REPRESENTATION('',(#614),#63813) ;
#585 = ADVANCED_BREP_SHAPE_REPRESENTATION('',(#615),#63814) ;
#586 = ADVANCED_BREP_SHAPE_REPRESENTATION('',(#616),#63815) ;
#587 = ADVANCED_BREP_SHAPE_REPRESENTATION('',(#617),#63816) ;
#588 = ADVANCED_BREP_SHAPE_REPRESENTATION('',(#618),#63817) ;
#589 = ADVANCED_BREP_SHAPE_REPRESENTATION('',(#619),#63818) ;
#590 = ADVANCED_BREP_SHAPE_REPRESENTATION('',(#620),#63819) ;
#591 = ADVANCED_BREP_SHAPE_REPRESENTATION('',(#621),#63820) ;
#592 = ADVANCED_BREP_SHAPE_REPRESENTATION('',(#622),#63821) ;
#593 = ADVANCED_BREP_SHAPE_REPRESENTATION('',(#623),#63822) ;
#594 = ADVANCED_BREP_SHAPE_REPRESENTATION('',(#624),#63823) ;
#595 = STYLED_ITEM('',(#63963),#610) ;
#596 = STYLED_ITEM('',(#63963),#611) ;
#597 = STYLED_ITEM('',(#63963),#612) ;
#598 = STYLED_ITEM('',(#63963),#613) ;
#599 = STYLED_ITEM('',(#63963),#614) ;
#600 = STYLED_ITEM('',(#63964),#615) ;
#601 = STYLED_ITEM('',(#63963),#616) ;
#602 = STYLED_ITEM('',(#63963),#617) ;
#603 = STYLED_ITEM('',(#63965),#618) ;
#604 = STYLED_ITEM('',(#63963),#619) ;
#605 = STYLED_ITEM('',(#63966),#620) ;
#606 = STYLED_ITEM('',(#63963),#621) ;
#607 = STYLED_ITEM('',(#63963),#622) ;
#608 = STYLED_ITEM('',(#63963),#623) ;
#609 = STYLED_ITEM('',(#63963),#624) ;
#610 = MANIFOLD_SOLID_BREP('Body1',#15494) ;
#611 = MANIFOLD_SOLID_BREP('Body1',#15495) ;
#612 = MANIFOLD_SOLID_BREP('Body1',#15496) ;
#613 = MANIFOLD_SOLID_BREP('Body1',#15497) ;
#614 = MANIFOLD_SOLID_BREP('Body1',#15498) ;
#615 = MANIFOLD_SOLID_BREP('Body1',#15499) ;
#616 = MANIFOLD_SOLID_BREP('Body1',#15500) ;
#617 = MANIFOLD_SOLID_BREP('Body1',#15501) ;
#618 = MANIFOLD_SOLID_BREP('Body1',#15502) ;
#619 = MANIFOLD_SOLID_BREP('Body1',#15503) ;
#620 = MANIFOLD_SOLID_BREP('Body1',#15504) ;
#621 = MANIFOLD_SOLID_BREP('Body1',#15505) ;
#622 = MANIFOLD_SOLID_BREP('Body1',#15506) ;
#623 = MANIFOLD_SOLID_BREP('Body1',#15507) ;
#624 = MANIFOLD_SOLID_BREP('Body1',#15508) ;
#625 = FACE_BOUND('',#2415,.T.) ;
#626 = FACE_BOUND('',#2419,.T.) ;
#627 = FACE_BOUND('',#2423,.T.) ;
#628 = FACE_BOUND('',#2427,.T.) ;
#629 = FACE_BOUND('',#2448,.T.) ;
#630 = FACE_BOUND('',#2449,.T.) ;
#631 = FACE_BOUND('',#2452,.T.) ;
#632 = FACE_BOUND('',#2453,.T.) ;
#633 = FACE_BOUND('',#2456,.T.) ;
#634 = FACE_BOUND('',#2457,.T.) ;
#635 = FACE_BOUND('',#2458,.T.) ;
#636 = FACE_BOUND('',#2459,.T.) ;
#637 = FACE_BOUND('',#2460,.T.) ;
#638 = FACE_BOUND('',#2462,.T.) ;
#639 = FACE_BOUND('',#2463,.T.) ;
#640 = FACE_BOUND('',#2464,.T.) ;
#641 = FACE_BOUND('',#2465,.T.) ;
#642 = FACE_BOUND('',#2466,.T.) ;
#643 = FACE_BOUND('',#2467,.T.) ;
#644 = FACE_BOUND('',#2468,.T.) ;
#645 = FACE_BOUND('',#2469,.T.) ;
#646 = FACE_BOUND('',#2470,.T.) ;
#647 = FACE_BOUND('',#2471,.T.) ;
#648 = FACE_BOUND('',#2472,.T.) ;
#649 = FACE_BOUND('',#2473,.T.) ;
#650 = FACE_BOUND('',#2474,.T.) ;
#651 = FACE_BOUND('',#2476,.T.) ;
#652 = FACE_BOUND('',#2480,.T.) ;
#653 = FACE_BOUND('',#2484,.T.) ;
#654 = FACE_BOUND('',#2488,.T.) ;
#655 = FACE_BOUND('',#2492,.T.) ;
#656 = FACE_BOUND('',#2496,.T.) ;
#657 = FACE_BOUND('',#2500,.T.) ;
#658 = FACE_BOUND('',#2504,.T.) ;
#659 = FACE_BOUND('',#2508,.T.) ;
#660 = FACE_BOUND('',#2512,.T.) ;
#661 = FACE_BOUND('',#2516,.T.) ;
#662 = FACE_BOUND('',#2520,.T.) ;
#663 = FACE_BOUND('',#2524,.T.) ;
#664 = FACE_BOUND('',#2525,.T.) ;
#665 = FACE_BOUND('',#2526,.T.) ;
#666 = FACE_BOUND('',#2527,.T.) ;
#667 = FACE_BOUND('',#2528,.T.) ;
#668 = FACE_BOUND('',#2529,.T.) ;
#669 = FACE_BOUND('',#2530,.T.) ;
#670 = FACE_BOUND('',#2531,.T.) ;
#671 = FACE_BOUND('',#2532,.T.) ;
#672 = FACE_BOUND('',#2533,.T.) ;
#673 = FACE_BOUND('',#2534,.T.) ;
#674 = FACE_BOUND('',#2535,.T.) ;
#675 = FACE_BOUND('',#2538,.T.) ;
#676 = FACE_BOUND('',#2539,.T.) ;
#677 = FACE_BOUND('',#2540,.T.) ;
#678 = FACE_BOUND('',#2541,.T.) ;
#679 = FACE_BOUND('',#2542,.T.) ;
#680 = FACE_BOUND('',#2543,.T.) ;
#681 = FACE_BOUND('',#2544,.T.) ;
#682 = FACE_BOUND('',#2545,.T.) ;
#683 = FACE_BOUND('',#2546,.T.) ;
#684 = FACE_BOUND('',#2547,.T.) ;
#685 = FACE_BOUND('',#2548,.T.) ;
#686 = FACE_BOUND('',#2549,.T.) ;
#687 = FACE_BOUND('',#2566,.T.) ;
#688 = FACE_BOUND('',#2567,.T.) ;
#689 = FACE_BOUND('',#2574,.T.) ;
#690 = FACE_BOUND('',#2575,.T.) ;
#691 = FACE_BOUND('',#2578,.T.) ;
#692 = FACE_BOUND('',#2579,.T.) ;
#693 = FACE_BOUND('',#2581,.T.) ;
#694 = FACE_BOUND('',#2582,.T.) ;
#695 = FACE_BOUND('',#2596,.T.) ;
#696 = FACE_BOUND('',#2600,.T.) ;
#697 = FACE_BOUND('',#2604,.T.) ;
#698 = FACE_BOUND('',#2608,.T.) ;
#699 = FACE_BOUND('',#2629,.T.) ;
#700 = FACE_BOUND('',#2630,.T.) ;
#701 = FACE_BOUND('',#2633,.T.) ;
#702 = FACE_BOUND('',#2634,.T.) ;
#703 = FACE_BOUND('',#2637,.T.) ;
#704 = FACE_BOUND('',#2638,.T.) ;
#705 = FACE_BOUND('',#2639,.T.) ;
#706 = FACE_BOUND('',#2640,.T.) ;
#707 = FACE_BOUND('',#2641,.T.) ;
#708 = FACE_BOUND('',#2642,.T.) ;
#709 = FACE_BOUND('',#2643,.T.) ;
#710 = FACE_BOUND('',#2645,.T.) ;
#711 = FACE_BOUND('',#2646,.T.) ;
#712 = FACE_BOUND('',#2647,.T.) ;
#713 = FACE_BOUND('',#2648,.T.) ;
#714 = FACE_BOUND('',#2649,.T.) ;
#715 = FACE_BOUND('',#2650,.T.) ;
#716 = FACE_BOUND('',#2651,.T.) ;
#717 = FACE_BOUND('',#2652,.T.) ;
#718 = FACE_BOUND('',#2653,.T.) ;
#719 = FACE_BOUND('',#2654,.T.) ;
#720 = FACE_BOUND('',#2655,.T.) ;
#721 = FACE_BOUND('',#2656,.T.) ;
#722 = FACE_BOUND('',#2657,.T.) ;
#723 = FACE_BOUND('',#2671,.T.) ;
#724 = FACE_BOUND('',#2672,.T.) ;
#725 = FACE_BOUND('',#2679,.T.) ;
#726 = FACE_BOUND('',#2680,.T.) ;
#727 = FACE_BOUND('',#2683,.T.) ;
#728 = FACE_BOUND('',#2684,.T.) ;
#729 = FACE_BOUND('',#2686,.T.) ;
#730 = FACE_BOUND('',#2687,.T.) ;
#731 = FACE_BOUND('',#2733,.T.) ;
#732 = FACE_BOUND('',#2739,.T.) ;
#733 = FACE_BOUND('',#2741,.T.) ;
#734 = FACE_BOUND('',#2745,.T.) ;
#735 = FACE_BOUND('',#2751,.T.) ;
#736 = FACE_BOUND('',#2755,.T.) ;
#737 = FACE_BOUND('',#2758,.T.) ;
#738 = FACE_BOUND('',#2759,.T.) ;
#739 = FACE_BOUND('',#2760,.T.) ;
#740 = FACE_BOUND('',#2762,.T.) ;
#741 = FACE_BOUND('',#2765,.T.) ;
#742 = FACE_BOUND('',#2775,.T.) ;
#743 = FACE_BOUND('',#2779,.T.) ;
#744 = FACE_BOUND('',#2787,.T.) ;
#745 = FACE_BOUND('',#2792,.T.) ;
#746 = FACE_BOUND('',#2795,.T.) ;
#747 = FACE_BOUND('',#2798,.T.) ;
#748 = FACE_BOUND('',#2811,.T.) ;
#749 = FACE_BOUND('',#2817,.T.) ;
#750 = FACE_BOUND('',#2823,.T.) ;
#751 = FACE_BOUND('',#2886,.T.) ;
#752 = FACE_BOUND('',#2894,.T.) ;
#753 = FACE_BOUND('',#2897,.T.) ;
#754 = FACE_BOUND('',#2900,.T.) ;
#755 = FACE_BOUND('',#3205,.T.) ;
#756 = FACE_BOUND('',#3210,.T.) ;
#757 = FACE_BOUND('',#3216,.T.) ;
#758 = FACE_BOUND('',#3235,.T.) ;
#759 = FACE_BOUND('',#3239,.T.) ;
#760 = FACE_BOUND('',#3240,.T.) ;
#761 = FACE_BOUND('',#3243,.T.) ;
#762 = FACE_BOUND('',#3244,.T.) ;
#763 = FACE_BOUND('',#3245,.T.) ;
#764 = FACE_BOUND('',#3246,.T.) ;
#765 = FACE_BOUND('',#3247,.T.) ;
#766 = FACE_BOUND('',#3248,.T.) ;
#767 = FACE_BOUND('',#3249,.T.) ;
#768 = FACE_BOUND('',#3250,.T.) ;
#769 = FACE_BOUND('',#3251,.T.) ;
#770 = FACE_BOUND('',#3252,.T.) ;
#771 = FACE_BOUND('',#3253,.T.) ;
#772 = FACE_BOUND('',#3254,.T.) ;
#773 = FACE_BOUND('',#3255,.T.) ;
#774 = FACE_BOUND('',#3256,.T.) ;
#775 = FACE_BOUND('',#3257,.T.) ;
#776 = FACE_BOUND('',#3258,.T.) ;
#777 = FACE_BOUND('',#3259,.T.) ;
#778 = FACE_BOUND('',#3260,.T.) ;
#779 = FACE_BOUND('',#3261,.T.) ;
#780 = FACE_BOUND('',#3262,.T.) ;
#781 = FACE_BOUND('',#3263,.T.) ;
#782 = FACE_BOUND('',#3264,.T.) ;
#783 = FACE_BOUND('',#3265,.T.) ;
#784 = FACE_BOUND('',#3266,.T.) ;
#785 = FACE_BOUND('',#3267,.T.) ;
#786 = FACE_BOUND('',#3268,.T.) ;
#787 = FACE_BOUND('',#3269,.T.) ;
#788 = FACE_BOUND('',#3270,.T.) ;
#789 = FACE_BOUND('',#3271,.T.) ;
#790 = FACE_BOUND('',#3280,.T.) ;
#791 = FACE_BOUND('',#3282,.T.) ;
#792 = FACE_BOUND('',#3284,.T.) ;
#793 = FACE_BOUND('',#3314,.T.) ;
#794 = FACE_BOUND('',#3406,.T.) ;
#795 = FACE_BOUND('',#3412,.T.) ;
#796 = FACE_BOUND('',#3425,.T.) ;
#797 = FACE_BOUND('',#3426,.T.) ;
#798 = FACE_BOUND('',#3427,.T.) ;
#799 = FACE_BOUND('',#3428,.T.) ;
#800 = FACE_BOUND('',#3429,.T.) ;
#801 = FACE_BOUND('',#3430,.T.) ;
#802 = FACE_BOUND('',#3431,.T.) ;
#803 = FACE_BOUND('',#3432,.T.) ;
#804 = FACE_BOUND('',#3433,.T.) ;
#805 = FACE_BOUND('',#3435,.T.) ;
#806 = FACE_BOUND('',#3436,.T.) ;
#807 = FACE_BOUND('',#3437,.T.) ;
#808 = FACE_BOUND('',#3438,.T.) ;
#809 = FACE_BOUND('',#3439,.T.) ;
#810 = FACE_BOUND('',#3440,.T.) ;
#811 = FACE_BOUND('',#3441,.T.) ;
#812 = FACE_BOUND('',#3442,.T.) ;
#813 = FACE_BOUND('',#3443,.T.) ;
#814 = FACE_BOUND('',#3455,.T.) ;
#815 = FACE_BOUND('',#3456,.T.) ;
#816 = FACE_BOUND('',#3457,.T.) ;
#817 = FACE_BOUND('',#3458,.T.) ;
#818 = FACE_BOUND('',#3459,.T.) ;
#819 = FACE_BOUND('',#3460,.T.) ;
#820 = FACE_BOUND('',#3461,.T.) ;
#821 = FACE_BOUND('',#3462,.T.) ;
#822 = FACE_BOUND('',#3463,.T.) ;
#823 = FACE_BOUND('',#3465,.T.) ;
#824 = FACE_BOUND('',#3466,.T.) ;
#825 = FACE_BOUND('',#3467,.T.) ;
#826 = FACE_BOUND('',#3468,.T.) ;
#827 = FACE_BOUND('',#3469,.T.) ;
#828 = FACE_BOUND('',#3470,.T.) ;
#829 = FACE_BOUND('',#3471,.T.) ;
#830 = FACE_BOUND('',#3472,.T.) ;
#831 = FACE_BOUND('',#3473,.T.) ;
#832 = PLANE('',#15693) ;
#833 = PLANE('',#15700) ;
#834 = PLANE('',#15707) ;
#835 = PLANE('',#15714) ;
#836 = PLANE('',#15756) ;
#837 = PLANE('',#15757) ;
#838 = PLANE('',#15758) ;
#839 = PLANE('',#15759) ;
#840 = PLANE('',#15760) ;
#841 = PLANE('',#15761) ;
#842 = PLANE('',#15763) ;
#843 = PLANE('',#15770) ;
#844 = PLANE('',#15777) ;
#845 = PLANE('',#15784) ;
#846 = PLANE('',#15791) ;
#847 = PLANE('',#15798) ;
#848 = PLANE('',#15805) ;
#849 = PLANE('',#15812) ;
#850 = PLANE('',#15819) ;
#851 = PLANE('',#15826) ;
#852 = PLANE('',#15833) ;
#853 = PLANE('',#15840) ;
#854 = PLANE('',#15847) ;
#855 = PLANE('',#15848) ;
#856 = PLANE('',#15849) ;
#857 = PLANE('',#15850) ;
#858 = PLANE('',#15851) ;
#859 = PLANE('',#15852) ;
#860 = PLANE('',#15878) ;
#861 = PLANE('',#15887) ;
#862 = PLANE('',#15888) ;
#863 = PLANE('',#15889) ;
#864 = PLANE('',#15890) ;
#865 = PLANE('',#15891) ;
#866 = PLANE('',#15917) ;
#867 = PLANE('',#15924) ;
#868 = PLANE('',#15931) ;
#869 = PLANE('',#15938) ;
#870 = PLANE('',#15980) ;
#871 = PLANE('',#15981) ;
#872 = PLANE('',#15982) ;
#873 = PLANE('',#15983) ;
#874 = PLANE('',#15984) ;
#875 = PLANE('',#15985) ;
#876 = PLANE('',#16011) ;
#877 = PLANE('',#16020) ;
#878 = PLANE('',#16021) ;
#879 = PLANE('',#16022) ;
#880 = PLANE('',#16023) ;
#881 = PLANE('',#16024) ;
#882 = PLANE('',#16082) ;
#883 = PLANE('',#16097) ;
#884 = PLANE('',#16105) ;
#885 = PLANE('',#16118) ;
#886 = PLANE('',#16125) ;
#887 = PLANE('',#16133) ;
#888 = PLANE('',#16137) ;
#889 = PLANE('',#16142) ;
#890 = PLANE('',#16143) ;
#891 = PLANE('',#16145) ;
#892 = PLANE('',#16148) ;
#893 = PLANE('',#16151) ;
#894 = PLANE('',#16154) ;
#895 = PLANE('',#16160) ;
#896 = PLANE('',#16164) ;
#897 = PLANE('',#16167) ;
#898 = PLANE('',#16176) ;
#899 = PLANE('',#16184) ;
#900 = PLANE('',#16185) ;
#901 = PLANE('',#16186) ;
#902 = PLANE('',#16187) ;
#903 = PLANE('',#16188) ;
#904 = PLANE('',#16189) ;
#905 = PLANE('',#16190) ;
#906 = PLANE('',#16195) ;
#907 = PLANE('',#16205) ;
#908 = PLANE('',#16209) ;
#909 = PLANE('',#16210) ;
#910 = PLANE('',#16211) ;
#911 = PLANE('',#16212) ;
#912 = PLANE('',#16397) ;
#913 = PLANE('',#16536) ;
#914 = PLANE('',#16540) ;
#915 = PLANE('',#16544) ;
#916 = PLANE('',#16546) ;
#917 = PLANE('',#16550) ;
#918 = PLANE('',#16557) ;
#919 = PLANE('',#16561) ;
#920 = PLANE('',#16568) ;
#921 = PLANE('',#16572) ;
#922 = PLANE('',#16579) ;
#923 = PLANE('',#16583) ;
#924 = PLANE('',#16590) ;
#925 = PLANE('',#16594) ;
#926 = PLANE('',#16601) ;
#927 = PLANE('',#16605) ;
#928 = PLANE('',#16612) ;
#929 = PLANE('',#16616) ;
#930 = PLANE('',#16623) ;
#931 = PLANE('',#16627) ;
#932 = PLANE('',#16634) ;
#933 = PLANE('',#16638) ;
#934 = PLANE('',#16645) ;
#935 = PLANE('',#16649) ;
#936 = PLANE('',#16656) ;
#937 = PLANE('',#16660) ;
#938 = PLANE('',#16667) ;
#939 = PLANE('',#16671) ;
#940 = PLANE('',#16678) ;
#941 = PLANE('',#16682) ;
#942 = PLANE('',#16689) ;
#943 = PLANE('',#16693) ;
#944 = PLANE('',#16700) ;
#945 = PLANE('',#16704) ;
#946 = PLANE('',#16711) ;
#947 = PLANE('',#16715) ;
#948 = PLANE('',#16722) ;
#949 = PLANE('',#16726) ;
#950 = PLANE('',#16733) ;
#951 = PLANE('',#16737) ;
#952 = PLANE('',#16744) ;
#953 = PLANE('',#16748) ;
#954 = PLANE('',#16755) ;
#955 = PLANE('',#16759) ;
#956 = PLANE('',#16766) ;
#957 = PLANE('',#16770) ;
#958 = PLANE('',#16777) ;
#959 = PLANE('',#16781) ;
#960 = PLANE('',#16788) ;
#961 = PLANE('',#16792) ;
#962 = PLANE('',#16799) ;
#963 = PLANE('',#16803) ;
#964 = PLANE('',#16810) ;
#965 = PLANE('',#16814) ;
#966 = PLANE('',#16821) ;
#967 = PLANE('',#16825) ;
#968 = PLANE('',#16832) ;
#969 = PLANE('',#16836) ;
#970 = PLANE('',#16843) ;
#971 = PLANE('',#16847) ;
#972 = PLANE('',#16854) ;
#973 = PLANE('',#16858) ;
#974 = PLANE('',#16865) ;
#975 = PLANE('',#16869) ;
#976 = PLANE('',#16876) ;
#977 = PLANE('',#16880) ;
#978 = PLANE('',#16887) ;
#979 = PLANE('',#16891) ;
#980 = PLANE('',#16898) ;
#981 = PLANE('',#16902) ;
#982 = PLANE('',#16909) ;
#983 = PLANE('',#16913) ;
#984 = PLANE('',#16920) ;
#985 = PLANE('',#16924) ;
#986 = PLANE('',#16931) ;
#987 = PLANE('',#16935) ;
#988 = PLANE('',#16942) ;
#989 = PLANE('',#16946) ;
#990 = PLANE('',#16953) ;
#991 = PLANE('',#16957) ;
#992 = PLANE('',#16964) ;
#993 = PLANE('',#16968) ;
#994 = PLANE('',#16975) ;
#995 = PLANE('',#16979) ;
#996 = PLANE('',#16986) ;
#997 = PLANE('',#16990) ;
#998 = PLANE('',#16997) ;
#999 = PLANE('',#17001) ;
#1000 = PLANE('',#17008) ;
#1001 = PLANE('',#17012) ;
#1002 = PLANE('',#17019) ;
#1003 = PLANE('',#17023) ;
#1004 = PLANE('',#17030) ;
#1005 = PLANE('',#17034) ;
#1006 = PLANE('',#17041) ;
#1007 = PLANE('',#17045) ;
#1008 = PLANE('',#17052) ;
#1009 = PLANE('',#17056) ;
#1010 = PLANE('',#17063) ;
#1011 = PLANE('',#17067) ;
#1012 = PLANE('',#17074) ;
#1013 = PLANE('',#17078) ;
#1014 = PLANE('',#17085) ;
#1015 = PLANE('',#17089) ;
#1016 = PLANE('',#17096) ;
#1017 = PLANE('',#17100) ;
#1018 = PLANE('',#17107) ;
#1019 = PLANE('',#17111) ;
#1020 = PLANE('',#17118) ;
#1021 = PLANE('',#17122) ;
#1022 = PLANE('',#17129) ;
#1023 = PLANE('',#17133) ;
#1024 = PLANE('',#17140) ;
#1025 = PLANE('',#17144) ;
#1026 = PLANE('',#17151) ;
#1027 = PLANE('',#17155) ;
#1028 = PLANE('',#17162) ;
#1029 = PLANE('',#17166) ;
#1030 = PLANE('',#17173) ;
#1031 = PLANE('',#17177) ;
#1032 = PLANE('',#17184) ;
#1033 = PLANE('',#17188) ;
#1034 = PLANE('',#17195) ;
#1035 = PLANE('',#17199) ;
#1036 = PLANE('',#17214) ;
#1037 = PLANE('',#17223) ;
#1038 = PLANE('',#17227) ;
#1039 = PLANE('',#17228) ;
#1040 = PLANE('',#17232) ;
#1041 = PLANE('',#17245) ;
#1042 = PLANE('',#17246) ;
#1043 = PLANE('',#17253) ;
#1044 = PLANE('',#17254) ;
#1045 = PLANE('',#17261) ;
#1046 = PLANE('',#17262) ;
#1047 = PLANE('',#17269) ;
#1048 = PLANE('',#17507) ;
#1049 = PLANE('',#17508) ;
#1050 = PLANE('',#17509) ;
#1051 = PLANE('',#17510) ;
#1052 = PLANE('',#17513) ;
#1053 = PLANE('',#17516) ;
#1054 = PLANE('',#17519) ;
#1055 = PLANE('',#17522) ;
#1056 = PLANE('',#17525) ;
#1057 = PLANE('',#17528) ;
#1058 = PLANE('',#17531) ;
#1059 = PLANE('',#17534) ;
#1060 = PLANE('',#17537) ;
#1061 = PLANE('',#17540) ;
#1062 = PLANE('',#17543) ;
#1063 = PLANE('',#17546) ;
#1064 = PLANE('',#17549) ;
#1065 = PLANE('',#17552) ;
#1066 = PLANE('',#17555) ;
#1067 = PLANE('',#17558) ;
#1068 = PLANE('',#17561) ;
#1069 = PLANE('',#17564) ;
#1070 = PLANE('',#17567) ;
#1071 = PLANE('',#17570) ;
#1072 = PLANE('',#17573) ;
#1073 = PLANE('',#17576) ;
#1074 = PLANE('',#17579) ;
#1075 = PLANE('',#17582) ;
#1076 = PLANE('',#17585) ;
#1077 = PLANE('',#17588) ;
#1078 = PLANE('',#17591) ;
#1079 = PLANE('',#17594) ;
#1080 = PLANE('',#17595) ;
#1081 = PLANE('',#17602) ;
#1082 = PLANE('',#17609) ;
#1083 = PLANE('',#17616) ;
#1084 = PLANE('',#17623) ;
#1085 = PLANE('',#17630) ;
#1086 = PLANE('',#17637) ;
#1087 = PLANE('',#17644) ;
#1088 = PLANE('',#17651) ;
#1089 = PLANE('',#17658) ;
#1090 = PLANE('',#17665) ;
#1091 = PLANE('',#17672) ;
#1092 = PLANE('',#17679) ;
#1093 = PLANE('',#17686) ;
#1094 = PLANE('',#17693) ;
#1095 = PLANE('',#17700) ;
#1096 = PLANE('',#17707) ;
#1097 = PLANE('',#17714) ;
#1098 = PLANE('',#17721) ;
#1099 = PLANE('',#17728) ;
#1100 = PLANE('',#17735) ;
#1101 = PLANE('',#17742) ;
#1102 = PLANE('',#17749) ;
#1103 = PLANE('',#17756) ;
#1104 = PLANE('',#17763) ;
#1105 = PLANE('',#17770) ;
#1106 = PLANE('',#17777) ;
#1107 = PLANE('',#17784) ;
#1108 = PLANE('',#17791) ;
#1109 = PLANE('',#17798) ;
#1110 = PLANE('',#17806) ;
#1111 = PLANE('',#17816) ;
#1112 = PLANE('',#17850) ;
#1113 = PLANE('',#17851) ;
#1114 = PLANE('',#17883) ;
#1115 = PLANE('',#17884) ;
#1116 = CYLINDRICAL_SURFACE('',#15679,4.263) ;
#1117 = CYLINDRICAL_SURFACE('',#15683,4.263) ;
#1118 = CYLINDRICAL_SURFACE('',#15687,4.263) ;
#1119 = CYLINDRICAL_SURFACE('',#15691,4.263) ;
#1120 = CYLINDRICAL_SURFACE('',#15696,9.) ;
#1121 = CYLINDRICAL_SURFACE('',#15698,5.5) ;
#1122 = CYLINDRICAL_SURFACE('',#15703,9.) ;
#1123 = CYLINDRICAL_SURFACE('',#15705,5.5) ;
#1124 = CYLINDRICAL_SURFACE('',#15710,9.) ;
#1125 = CYLINDRICAL_SURFACE('',#15712,5.5) ;
#1126 = CYLINDRICAL_SURFACE('',#15717,9.) ;
#1127 = CYLINDRICAL_SURFACE('',#15719,5.5) ;
#1128 = CYLINDRICAL_SURFACE('',#15723,3.3) ;
#1129 = CYLINDRICAL_SURFACE('',#15727,2.5175) ;
#1130 = CYLINDRICAL_SURFACE('',#15731,2.5175) ;
#1131 = CYLINDRICAL_SURFACE('',#15735,2.5175) ;
#1132 = CYLINDRICAL_SURFACE('',#15739,2.5175) ;
#1133 = CYLINDRICAL_SURFACE('',#15743,2.5175) ;
#1134 = CYLINDRICAL_SURFACE('',#15747,2.5175) ;
#1135 = CYLINDRICAL_SURFACE('',#15751,3.3) ;
#1136 = CYLINDRICAL_SURFACE('',#15753,37.5) ;
#1137 = CYLINDRICAL_SURFACE('',#15766,9.) ;
#1138 = CYLINDRICAL_SURFACE('',#15768,5.5) ;
#1139 = CYLINDRICAL_SURFACE('',#15773,9.) ;
#1140 = CYLINDRICAL_SURFACE('',#15775,5.5) ;
#1141 = CYLINDRICAL_SURFACE('',#15780,9.) ;
#1142 = CYLINDRICAL_SURFACE('',#15782,5.5) ;
#1143 = CYLINDRICAL_SURFACE('',#15787,9.) ;
#1144 = CYLINDRICAL_SURFACE('',#15789,5.5) ;
#1145 = CYLINDRICAL_SURFACE('',#15794,9.) ;
#1146 = CYLINDRICAL_SURFACE('',#15796,5.5) ;
#1147 = CYLINDRICAL_SURFACE('',#15801,9.) ;
#1148 = CYLINDRICAL_SURFACE('',#15803,5.5) ;
#1149 = CYLINDRICAL_SURFACE('',#15808,9.) ;
#1150 = CYLINDRICAL_SURFACE('',#15810,5.5) ;
#1151 = CYLINDRICAL_SURFACE('',#15815,9.) ;
#1152 = CYLINDRICAL_SURFACE('',#15817,5.5) ;
#1153 = CYLINDRICAL_SURFACE('',#15822,9.) ;
#1154 = CYLINDRICAL_SURFACE('',#15824,5.5) ;
#1155 = CYLINDRICAL_SURFACE('',#15829,9.) ;
#1156 = CYLINDRICAL_SURFACE('',#15831,5.5) ;
#1157 = CYLINDRICAL_SURFACE('',#15836,9.) ;
#1158 = CYLINDRICAL_SURFACE('',#15838,5.5) ;
#1159 = CYLINDRICAL_SURFACE('',#15843,9.) ;
#1160 = CYLINDRICAL_SURFACE('',#15845,5.5) ;
#1161 = CYLINDRICAL_SURFACE('',#15856,4.263) ;
#1162 = CYLINDRICAL_SURFACE('',#15860,4.263) ;
#1163 = CYLINDRICAL_SURFACE('',#15864,4.263) ;
#1164 = CYLINDRICAL_SURFACE('',#15868,4.263) ;
#1165 = CYLINDRICAL_SURFACE('',#15872,4.263) ;
#1166 = CYLINDRICAL_SURFACE('',#15876,4.263) ;
#1167 = CYLINDRICAL_SURFACE('',#15881,4.263) ;
#1168 = CYLINDRICAL_SURFACE('',#15885,4.263) ;
#1169 = CYLINDRICAL_SURFACE('',#15895,2.117) ;
#1170 = CYLINDRICAL_SURFACE('',#15899,2.117) ;
#1171 = CYLINDRICAL_SURFACE('',#15903,4.263) ;
#1172 = CYLINDRICAL_SURFACE('',#15907,4.263) ;
#1173 = CYLINDRICAL_SURFACE('',#15911,4.263) ;
#1174 = CYLINDRICAL_SURFACE('',#15915,4.263) ;
#1175 = CYLINDRICAL_SURFACE('',#15920,9.) ;
#1176 = CYLINDRICAL_SURFACE('',#15922,5.5) ;
#1177 = CYLINDRICAL_SURFACE('',#15927,9.) ;
#1178 = CYLINDRICAL_SURFACE('',#15929,5.5) ;
#1179 = CYLINDRICAL_SURFACE('',#15934,9.) ;
#1180 = CYLINDRICAL_SURFACE('',#15936,5.5) ;
#1181 = CYLINDRICAL_SURFACE('',#15941,9.) ;
#1182 = CYLINDRICAL_SURFACE('',#15943,5.5) ;
#1183 = CYLINDRICAL_SURFACE('',#15947,3.3) ;
#1184 = CYLINDRICAL_SURFACE('',#15951,2.5175) ;
#1185 = CYLINDRICAL_SURFACE('',#15955,2.5175) ;
#1186 = CYLINDRICAL_SURFACE('',#15959,2.5175) ;
#1187 = CYLINDRICAL_SURFACE('',#15963,2.5175) ;
#1188 = CYLINDRICAL_SURFACE('',#15967,2.5175) ;
#1189 = CYLINDRICAL_SURFACE('',#15971,2.5175) ;
#1190 = CYLINDRICAL_SURFACE('',#15975,3.3) ;
#1191 = CYLINDRICAL_SURFACE('',#15977,37.5) ;
#1192 = CYLINDRICAL_SURFACE('',#15989,4.263) ;
#1193 = CYLINDRICAL_SURFACE('',#15993,4.263) ;
#1194 = CYLINDRICAL_SURFACE('',#15997,4.263) ;
#1195 = CYLINDRICAL_SURFACE('',#16001,4.263) ;
#1196 = CYLINDRICAL_SURFACE('',#16005,4.263) ;
#1197 = CYLINDRICAL_SURFACE('',#16009,4.263) ;
#1198 = CYLINDRICAL_SURFACE('',#16014,4.263) ;
#1199 = CYLINDRICAL_SURFACE('',#16018,4.263) ;
#1200 = CYLINDRICAL_SURFACE('',#16026,19.425) ;
#1201 = CYLINDRICAL_SURFACE('',#16028,19.425) ;
#1202 = CYLINDRICAL_SURFACE('',#16029,19.425) ;
#1203 = CYLINDRICAL_SURFACE('',#16030,19.425) ;
#1204 = CYLINDRICAL_SURFACE('',#16031,19.425) ;
#1205 = CYLINDRICAL_SURFACE('',#16032,19.425) ;
#1206 = CYLINDRICAL_SURFACE('',#16033,19.425) ;
#1207 = CYLINDRICAL_SURFACE('',#16034,19.425) ;
#1208 = CYLINDRICAL_SURFACE('',#16035,19.425) ;
#1209 = CYLINDRICAL_SURFACE('',#16036,19.425) ;
#1210 = CYLINDRICAL_SURFACE('',#16037,19.425) ;
#1211 = CYLINDRICAL_SURFACE('',#16038,19.425) ;
#1212 = CYLINDRICAL_SURFACE('',#16039,19.425) ;
#1213 = CYLINDRICAL_SURFACE('',#16040,22.12975) ;
#1214 = CYLINDRICAL_SURFACE('',#16042,22.12975) ;
#1215 = CYLINDRICAL_SURFACE('',#16043,22.12975) ;
#1216 = CYLINDRICAL_SURFACE('',#16044,22.12975) ;
#1217 = CYLINDRICAL_SURFACE('',#16045,22.12975) ;
#1218 = CYLINDRICAL_SURFACE('',#16046,22.12975) ;
#1219 = CYLINDRICAL_SURFACE('',#16047,22.12975) ;
#1220 = CYLINDRICAL_SURFACE('',#16049,20.33524) ;
#1221 = CYLINDRICAL_SURFACE('',#16051,20.33524) ;
#1222 = CYLINDRICAL_SURFACE('',#16052,20.33524) ;
#1223 = CYLINDRICAL_SURFACE('',#16053,20.33524) ;
#1224 = CYLINDRICAL_SURFACE('',#16054,20.33524) ;
#1225 = CYLINDRICAL_SURFACE('',#16055,20.33524) ;
#1226 = CYLINDRICAL_SURFACE('',#16056,18.56595) ;
#1227 = CYLINDRICAL_SURFACE('',#16058,18.56595) ;
#1228 = CYLINDRICAL_SURFACE('',#16059,18.56595) ;
#1229 = CYLINDRICAL_SURFACE('',#16060,18.56595) ;
#1230 = CYLINDRICAL_SURFACE('',#16061,18.56595) ;
#1231 = CYLINDRICAL_SURFACE('',#16062,18.56595) ;
#1232 = CYLINDRICAL_SURFACE('',#16063,18.56595) ;
#1233 = CYLINDRICAL_SURFACE('',#16064,18.56595) ;
#1234 = CYLINDRICAL_SURFACE('',#16065,18.56595) ;
#1235 = CYLINDRICAL_SURFACE('',#16066,18.56595) ;
#1236 = CYLINDRICAL_SURFACE('',#16067,18.56595) ;
#1237 = CYLINDRICAL_SURFACE('',#16068,18.56595) ;
#1238 = CYLINDRICAL_SURFACE('',#16069,18.56595) ;
#1239 = CYLINDRICAL_SURFACE('',#16070,18.56595) ;
#1240 = CYLINDRICAL_SURFACE('',#16072,20.33524) ;
#1241 = CYLINDRICAL_SURFACE('',#16074,22.12975) ;
#1242 = CYLINDRICAL_SURFACE('',#16076,19.425) ;
#1243 = CYLINDRICAL_SURFACE('',#16084,13.2000000000001) ;
#1244 = CYLINDRICAL_SURFACE('',#16089,17.5) ;
#1245 = CYLINDRICAL_SURFACE('',#16095,19.9999999999999) ;
#1246 = CYLINDRICAL_SURFACE('',#16103,22.5) ;
#1247 = CYLINDRICAL_SURFACE('',#16111,33.5) ;
#1248 = CYLINDRICAL_SURFACE('',#16130,33.5) ;
#1249 = CYLINDRICAL_SURFACE('',#16139,33.5) ;
#1250 = CYLINDRICAL_SURFACE('',#16140,33.5) ;
#1251 = CYLINDRICAL_SURFACE('',#16141,33.5) ;
#1252 = CYLINDRICAL_SURFACE('',#16146,5.00000000000251) ;
#1253 = CYLINDRICAL_SURFACE('',#16149,5.00000000000251) ;
#1254 = CYLINDRICAL_SURFACE('',#16152,20.065) ;
#1255 = CYLINDRICAL_SURFACE('',#16156,23.) ;
#1256 = CYLINDRICAL_SURFACE('',#16157,20.065) ;
#1257 = CYLINDRICAL_SURFACE('',#16158,22.5) ;
#1258 = CYLINDRICAL_SURFACE('',#16162,22.25) ;
#1259 = CYLINDRICAL_SURFACE('',#16165,18.) ;
#1260 = CYLINDRICAL_SURFACE('',#16169,5.) ;
#1261 = CYLINDRICAL_SURFACE('',#16177,4.99999999999999) ;
#1262 = CYLINDRICAL_SURFACE('',#16197,27.) ;
#1263 = CYLINDRICAL_SURFACE('',#16201,22.5) ;
#1264 = CYLINDRICAL_SURFACE('',#16215,47.175) ;
#1265 = CYLINDRICAL_SURFACE('',#16218,47.175) ;
#1266 = CYLINDRICAL_SURFACE('',#16221,47.175) ;
#1267 = CYLINDRICAL_SURFACE('',#16224,47.175) ;
#1268 = CYLINDRICAL_SURFACE('',#16227,47.175) ;
#1269 = CYLINDRICAL_SURFACE('',#16230,47.175) ;
#1270 = CYLINDRICAL_SURFACE('',#16233,47.175) ;
#1271 = CYLINDRICAL_SURFACE('',#16236,47.175) ;
#1272 = CYLINDRICAL_SURFACE('',#16239,47.175) ;
#1273 = CYLINDRICAL_SURFACE('',#16242,47.175) ;
#1274 = CYLINDRICAL_SURFACE('',#16245,47.175) ;
#1275 = CYLINDRICAL_SURFACE('',#16248,47.175) ;
#1276 = CYLINDRICAL_SURFACE('',#16251,47.175) ;
#1277 = CYLINDRICAL_SURFACE('',#16254,47.175) ;
#1278 = CYLINDRICAL_SURFACE('',#16257,47.175) ;
#1279 = CYLINDRICAL_SURFACE('',#16260,47.175) ;
#1280 = CYLINDRICAL_SURFACE('',#16263,47.175) ;
#1281 = CYLINDRICAL_SURFACE('',#16266,47.175) ;
#1282 = CYLINDRICAL_SURFACE('',#16269,47.175) ;
#1283 = CYLINDRICAL_SURFACE('',#16272,47.175) ;
#1284 = CYLINDRICAL_SURFACE('',#16275,47.175) ;
#1285 = CYLINDRICAL_SURFACE('',#16278,47.175) ;
#1286 = CYLINDRICAL_SURFACE('',#16281,47.175) ;
#1287 = CYLINDRICAL_SURFACE('',#16284,47.175) ;
#1288 = CYLINDRICAL_SURFACE('',#16287,47.175) ;
#1289 = CYLINDRICAL_SURFACE('',#16290,47.175) ;
#1290 = CYLINDRICAL_SURFACE('',#16293,47.175) ;
#1291 = CYLINDRICAL_SURFACE('',#16296,47.175) ;
#1292 = CYLINDRICAL_SURFACE('',#16299,47.175) ;
#1293 = CYLINDRICAL_SURFACE('',#16302,47.175) ;
#1294 = CYLINDRICAL_SURFACE('',#16305,47.175) ;
#1295 = CYLINDRICAL_SURFACE('',#16308,47.175) ;
#1296 = CYLINDRICAL_SURFACE('',#16311,47.175) ;
#1297 = CYLINDRICAL_SURFACE('',#16314,47.175) ;
#1298 = CYLINDRICAL_SURFACE('',#16317,47.175) ;
#1299 = CYLINDRICAL_SURFACE('',#16320,47.175) ;
#1300 = CYLINDRICAL_SURFACE('',#16323,47.175) ;
#1301 = CYLINDRICAL_SURFACE('',#16326,47.175) ;
#1302 = CYLINDRICAL_SURFACE('',#16329,47.175) ;
#1303 = CYLINDRICAL_SURFACE('',#16332,47.175) ;
#1304 = CYLINDRICAL_SURFACE('',#16335,47.175) ;
#1305 = CYLINDRICAL_SURFACE('',#16338,47.175) ;
#1306 = CYLINDRICAL_SURFACE('',#16341,47.175) ;
#1307 = CYLINDRICAL_SURFACE('',#16344,47.175) ;
#1308 = CYLINDRICAL_SURFACE('',#16347,47.175) ;
#1309 = CYLINDRICAL_SURFACE('',#16350,47.175) ;
#1310 = CYLINDRICAL_SURFACE('',#16353,47.175) ;
#1311 = CYLINDRICAL_SURFACE('',#16356,47.175) ;
#1312 = CYLINDRICAL_SURFACE('',#16359,47.175) ;
#1313 = CYLINDRICAL_SURFACE('',#16362,47.175) ;
#1314 = CYLINDRICAL_SURFACE('',#16365,47.175) ;
#1315 = CYLINDRICAL_SURFACE('',#16368,47.175) ;
#1316 = CYLINDRICAL_SURFACE('',#16371,47.175) ;
#1317 = CYLINDRICAL_SURFACE('',#16374,47.175) ;
#1318 = CYLINDRICAL_SURFACE('',#16377,47.175) ;
#1319 = CYLINDRICAL_SURFACE('',#16380,47.175) ;
#1320 = CYLINDRICAL_SURFACE('',#16383,47.175) ;
#1321 = CYLINDRICAL_SURFACE('',#16386,47.175) ;
#1322 = CYLINDRICAL_SURFACE('',#16389,47.175) ;
#1323 = CYLINDRICAL_SURFACE('',#16392,47.175) ;
#1324 = CYLINDRICAL_SURFACE('',#16395,40.) ;
#1325 = CYLINDRICAL_SURFACE('',#16538,40.) ;
#1326 = CYLINDRICAL_SURFACE('',#16542,37.5) ;
#1327 = CYLINDRICAL_SURFACE('',#16554,0.539999999999996) ;
#1328 = CYLINDRICAL_SURFACE('',#16555,1.4) ;
#1329 = CYLINDRICAL_SURFACE('',#16556,0.539999999999986) ;
#1330 = CYLINDRICAL_SURFACE('',#16565,0.539999999999996) ;
#1331 = CYLINDRICAL_SURFACE('',#16566,1.4) ;
#1332 = CYLINDRICAL_SURFACE('',#16567,0.539999999999986) ;
#1333 = CYLINDRICAL_SURFACE('',#16576,0.539999999999996) ;
#1334 = CYLINDRICAL_SURFACE('',#16577,1.4) ;
#1335 = CYLINDRICAL_SURFACE('',#16578,0.539999999999986) ;
#1336 = CYLINDRICAL_SURFACE('',#16587,0.539999999999996) ;
#1337 = CYLINDRICAL_SURFACE('',#16588,1.4) ;
#1338 = CYLINDRICAL_SURFACE('',#16589,0.539999999999986) ;
#1339 = CYLINDRICAL_SURFACE('',#16598,0.539999999999996) ;
#1340 = CYLINDRICAL_SURFACE('',#16599,1.4) ;
#1341 = CYLINDRICAL_SURFACE('',#16600,0.539999999999986) ;
#1342 = CYLINDRICAL_SURFACE('',#16609,0.539999999999996) ;
#1343 = CYLINDRICAL_SURFACE('',#16610,1.4) ;
#1344 = CYLINDRICAL_SURFACE('',#16611,0.539999999999986) ;
#1345 = CYLINDRICAL_SURFACE('',#16620,0.539999999999996) ;
#1346 = CYLINDRICAL_SURFACE('',#16621,1.4) ;
#1347 = CYLINDRICAL_SURFACE('',#16622,0.539999999999986) ;
#1348 = CYLINDRICAL_SURFACE('',#16631,0.539999999999996) ;
#1349 = CYLINDRICAL_SURFACE('',#16632,1.4) ;
#1350 = CYLINDRICAL_SURFACE('',#16633,0.539999999999986) ;
#1351 = CYLINDRICAL_SURFACE('',#16642,0.539999999999996) ;
#1352 = CYLINDRICAL_SURFACE('',#16643,1.4) ;
#1353 = CYLINDRICAL_SURFACE('',#16644,0.539999999999986) ;
#1354 = CYLINDRICAL_SURFACE('',#16653,0.539999999999996) ;
#1355 = CYLINDRICAL_SURFACE('',#16654,1.4) ;
#1356 = CYLINDRICAL_SURFACE('',#16655,0.539999999999986) ;
#1357 = CYLINDRICAL_SURFACE('',#16664,0.539999999999996) ;
#1358 = CYLINDRICAL_SURFACE('',#16665,1.4) ;
#1359 = CYLINDRICAL_SURFACE('',#16666,0.539999999999986) ;
#1360 = CYLINDRICAL_SURFACE('',#16675,0.539999999999996) ;
#1361 = CYLINDRICAL_SURFACE('',#16676,1.4) ;
#1362 = CYLINDRICAL_SURFACE('',#16677,0.539999999999986) ;
#1363 = CYLINDRICAL_SURFACE('',#16686,0.539999999999996) ;
#1364 = CYLINDRICAL_SURFACE('',#16687,1.4) ;
#1365 = CYLINDRICAL_SURFACE('',#16688,0.539999999999986) ;
#1366 = CYLINDRICAL_SURFACE('',#16697,0.539999999999996) ;
#1367 = CYLINDRICAL_SURFACE('',#16698,1.4) ;
#1368 = CYLINDRICAL_SURFACE('',#16699,0.539999999999986) ;
#1369 = CYLINDRICAL_SURFACE('',#16708,0.539999999999996) ;
#1370 = CYLINDRICAL_SURFACE('',#16709,1.4) ;
#1371 = CYLINDRICAL_SURFACE('',#16710,0.539999999999986) ;
#1372 = CYLINDRICAL_SURFACE('',#16719,0.539999999999996) ;
#1373 = CYLINDRICAL_SURFACE('',#16720,1.4) ;
#1374 = CYLINDRICAL_SURFACE('',#16721,0.539999999999986) ;
#1375 = CYLINDRICAL_SURFACE('',#16730,0.539999999999996) ;
#1376 = CYLINDRICAL_SURFACE('',#16731,1.4) ;
#1377 = CYLINDRICAL_SURFACE('',#16732,0.539999999999986) ;
#1378 = CYLINDRICAL_SURFACE('',#16741,0.539999999999996) ;
#1379 = CYLINDRICAL_SURFACE('',#16742,1.4) ;
#1380 = CYLINDRICAL_SURFACE('',#16743,0.539999999999986) ;
#1381 = CYLINDRICAL_SURFACE('',#16752,0.539999999999996) ;
#1382 = CYLINDRICAL_SURFACE('',#16753,1.4) ;
#1383 = CYLINDRICAL_SURFACE('',#16754,0.539999999999986) ;
#1384 = CYLINDRICAL_SURFACE('',#16763,0.539999999999996) ;
#1385 = CYLINDRICAL_SURFACE('',#16764,1.4) ;
#1386 = CYLINDRICAL_SURFACE('',#16765,0.539999999999986) ;
#1387 = CYLINDRICAL_SURFACE('',#16774,0.539999999999996) ;
#1388 = CYLINDRICAL_SURFACE('',#16775,1.4) ;
#1389 = CYLINDRICAL_SURFACE('',#16776,0.539999999999986) ;
#1390 = CYLINDRICAL_SURFACE('',#16785,0.539999999999996) ;
#1391 = CYLINDRICAL_SURFACE('',#16786,1.4) ;
#1392 = CYLINDRICAL_SURFACE('',#16787,0.539999999999986) ;
#1393 = CYLINDRICAL_SURFACE('',#16796,0.539999999999996) ;
#1394 = CYLINDRICAL_SURFACE('',#16797,1.4) ;
#1395 = CYLINDRICAL_SURFACE('',#16798,0.539999999999986) ;
#1396 = CYLINDRICAL_SURFACE('',#16807,0.539999999999996) ;
#1397 = CYLINDRICAL_SURFACE('',#16808,1.4) ;
#1398 = CYLINDRICAL_SURFACE('',#16809,0.539999999999986) ;
#1399 = CYLINDRICAL_SURFACE('',#16818,0.539999999999996) ;
#1400 = CYLINDRICAL_SURFACE('',#16819,1.4) ;
#1401 = CYLINDRICAL_SURFACE('',#16820,0.539999999999986) ;
#1402 = CYLINDRICAL_SURFACE('',#16829,0.539999999999996) ;
#1403 = CYLINDRICAL_SURFACE('',#16830,1.4) ;
#1404 = CYLINDRICAL_SURFACE('',#16831,0.539999999999986) ;
#1405 = CYLINDRICAL_SURFACE('',#16840,0.539999999999996) ;
#1406 = CYLINDRICAL_SURFACE('',#16841,1.4) ;
#1407 = CYLINDRICAL_SURFACE('',#16842,0.539999999999986) ;
#1408 = CYLINDRICAL_SURFACE('',#16851,0.539999999999996) ;
#1409 = CYLINDRICAL_SURFACE('',#16852,1.4) ;
#1410 = CYLINDRICAL_SURFACE('',#16853,0.539999999999986) ;
#1411 = CYLINDRICAL_SURFACE('',#16862,0.539999999999996) ;
#1412 = CYLINDRICAL_SURFACE('',#16863,1.4) ;
#1413 = CYLINDRICAL_SURFACE('',#16864,0.539999999999986) ;
#1414 = CYLINDRICAL_SURFACE('',#16873,0.539999999999996) ;
#1415 = CYLINDRICAL_SURFACE('',#16874,1.4) ;
#1416 = CYLINDRICAL_SURFACE('',#16875,0.539999999999986) ;
#1417 = CYLINDRICAL_SURFACE('',#16884,0.539999999999996) ;
#1418 = CYLINDRICAL_SURFACE('',#16885,1.4) ;
#1419 = CYLINDRICAL_SURFACE('',#16886,0.539999999999986) ;
#1420 = CYLINDRICAL_SURFACE('',#16895,0.539999999999996) ;
#1421 = CYLINDRICAL_SURFACE('',#16896,1.4) ;
#1422 = CYLINDRICAL_SURFACE('',#16897,0.539999999999986) ;
#1423 = CYLINDRICAL_SURFACE('',#16906,0.539999999999996) ;
#1424 = CYLINDRICAL_SURFACE('',#16907,1.4) ;
#1425 = CYLINDRICAL_SURFACE('',#16908,0.539999999999986) ;
#1426 = CYLINDRICAL_SURFACE('',#16917,0.539999999999996) ;
#1427 = CYLINDRICAL_SURFACE('',#16918,1.4) ;
#1428 = CYLINDRICAL_SURFACE('',#16919,0.539999999999986) ;
#1429 = CYLINDRICAL_SURFACE('',#16928,0.539999999999996) ;
#1430 = CYLINDRICAL_SURFACE('',#16929,1.4) ;
#1431 = CYLINDRICAL_SURFACE('',#16930,0.539999999999986) ;
#1432 = CYLINDRICAL_SURFACE('',#16939,0.539999999999996) ;
#1433 = CYLINDRICAL_SURFACE('',#16940,1.4) ;
#1434 = CYLINDRICAL_SURFACE('',#16941,0.539999999999986) ;
#1435 = CYLINDRICAL_SURFACE('',#16950,0.539999999999996) ;
#1436 = CYLINDRICAL_SURFACE('',#16951,1.4) ;
#1437 = CYLINDRICAL_SURFACE('',#16952,0.539999999999986) ;
#1438 = CYLINDRICAL_SURFACE('',#16961,0.539999999999996) ;
#1439 = CYLINDRICAL_SURFACE('',#16962,1.4) ;
#1440 = CYLINDRICAL_SURFACE('',#16963,0.539999999999986) ;
#1441 = CYLINDRICAL_SURFACE('',#16972,0.539999999999996) ;
#1442 = CYLINDRICAL_SURFACE('',#16973,1.4) ;
#1443 = CYLINDRICAL_SURFACE('',#16974,0.539999999999986) ;
#1444 = CYLINDRICAL_SURFACE('',#16983,0.539999999999996) ;
#1445 = CYLINDRICAL_SURFACE('',#16984,1.4) ;
#1446 = CYLINDRICAL_SURFACE('',#16985,0.539999999999986) ;
#1447 = CYLINDRICAL_SURFACE('',#16994,0.539999999999996) ;
#1448 = CYLINDRICAL_SURFACE('',#16995,1.4) ;
#1449 = CYLINDRICAL_SURFACE('',#16996,0.539999999999986) ;
#1450 = CYLINDRICAL_SURFACE('',#17005,0.539999999999996) ;
#1451 = CYLINDRICAL_SURFACE('',#17006,1.4) ;
#1452 = CYLINDRICAL_SURFACE('',#17007,0.539999999999986) ;
#1453 = CYLINDRICAL_SURFACE('',#17016,0.539999999999996) ;
#1454 = CYLINDRICAL_SURFACE('',#17017,1.4) ;
#1455 = CYLINDRICAL_SURFACE('',#17018,0.539999999999986) ;
#1456 = CYLINDRICAL_SURFACE('',#17027,0.539999999999996) ;
#1457 = CYLINDRICAL_SURFACE('',#17028,1.4) ;
#1458 = CYLINDRICAL_SURFACE('',#17029,0.539999999999986) ;
#1459 = CYLINDRICAL_SURFACE('',#17038,0.539999999999996) ;
#1460 = CYLINDRICAL_SURFACE('',#17039,1.4) ;
#1461 = CYLINDRICAL_SURFACE('',#17040,0.539999999999986) ;
#1462 = CYLINDRICAL_SURFACE('',#17049,0.539999999999996) ;
#1463 = CYLINDRICAL_SURFACE('',#17050,1.4) ;
#1464 = CYLINDRICAL_SURFACE('',#17051,0.539999999999986) ;
#1465 = CYLINDRICAL_SURFACE('',#17060,0.539999999999996) ;
#1466 = CYLINDRICAL_SURFACE('',#17061,1.4) ;
#1467 = CYLINDRICAL_SURFACE('',#17062,0.539999999999986) ;
#1468 = CYLINDRICAL_SURFACE('',#17071,0.539999999999996) ;
#1469 = CYLINDRICAL_SURFACE('',#17072,1.4) ;
#1470 = CYLINDRICAL_SURFACE('',#17073,0.539999999999986) ;
#1471 = CYLINDRICAL_SURFACE('',#17082,0.539999999999996) ;
#1472 = CYLINDRICAL_SURFACE('',#17083,1.4) ;
#1473 = CYLINDRICAL_SURFACE('',#17084,0.539999999999986) ;
#1474 = CYLINDRICAL_SURFACE('',#17093,0.539999999999996) ;
#1475 = CYLINDRICAL_SURFACE('',#17094,1.4) ;
#1476 = CYLINDRICAL_SURFACE('',#17095,0.539999999999986) ;
#1477 = CYLINDRICAL_SURFACE('',#17104,0.539999999999996) ;
#1478 = CYLINDRICAL_SURFACE('',#17105,1.4) ;
#1479 = CYLINDRICAL_SURFACE('',#17106,0.539999999999986) ;
#1480 = CYLINDRICAL_SURFACE('',#17115,0.539999999999996) ;
#1481 = CYLINDRICAL_SURFACE('',#17116,1.4) ;
#1482 = CYLINDRICAL_SURFACE('',#17117,0.539999999999986) ;
#1483 = CYLINDRICAL_SURFACE('',#17126,0.539999999999996) ;
#1484 = CYLINDRICAL_SURFACE('',#17127,1.4) ;
#1485 = CYLINDRICAL_SURFACE('',#17128,0.539999999999986) ;
#1486 = CYLINDRICAL_SURFACE('',#17137,0.539999999999996) ;
#1487 = CYLINDRICAL_SURFACE('',#17138,1.4) ;
#1488 = CYLINDRICAL_SURFACE('',#17139,0.539999999999986) ;
#1489 = CYLINDRICAL_SURFACE('',#17148,0.539999999999996) ;
#1490 = CYLINDRICAL_SURFACE('',#17149,1.4) ;
#1491 = CYLINDRICAL_SURFACE('',#17150,0.539999999999986) ;
#1492 = CYLINDRICAL_SURFACE('',#17159,0.539999999999996) ;
#1493 = CYLINDRICAL_SURFACE('',#17160,1.4) ;
#1494 = CYLINDRICAL_SURFACE('',#17161,0.539999999999986) ;
#1495 = CYLINDRICAL_SURFACE('',#17170,0.539999999999996) ;
#1496 = CYLINDRICAL_SURFACE('',#17171,1.4) ;
#1497 = CYLINDRICAL_SURFACE('',#17172,0.539999999999986) ;
#1498 = CYLINDRICAL_SURFACE('',#17181,0.539999999999996) ;
#1499 = CYLINDRICAL_SURFACE('',#17182,1.4) ;
#1500 = CYLINDRICAL_SURFACE('',#17183,0.539999999999986) ;
#1501 = CYLINDRICAL_SURFACE('',#17192,0.539999999999996) ;
#1502 = CYLINDRICAL_SURFACE('',#17193,1.4) ;
#1503 = CYLINDRICAL_SURFACE('',#17194,0.539999999999986) ;
#1504 = CYLINDRICAL_SURFACE('',#17203,0.539999999999996) ;
#1505 = CYLINDRICAL_SURFACE('',#17204,1.4) ;
#1506 = CYLINDRICAL_SURFACE('',#17205,0.539999999999986) ;
#1507 = CYLINDRICAL_SURFACE('',#17206,20.) ;
#1508 = CYLINDRICAL_SURFACE('',#17208,20.) ;
#1509 = CYLINDRICAL_SURFACE('',#17219,25.) ;
#1510 = CYLINDRICAL_SURFACE('',#17229,25.) ;
#1511 = CYLINDRICAL_SURFACE('',#17241,29.) ;
#1512 = CYLINDRICAL_SURFACE('',#17247,25.) ;
#1513 = CYLINDRICAL_SURFACE('',#17249,29.) ;
#1514 = CYLINDRICAL_SURFACE('',#17255,25.) ;
#1515 = CYLINDRICAL_SURFACE('',#17257,29.) ;
#1516 = CYLINDRICAL_SURFACE('',#17263,25.) ;
#1517 = CYLINDRICAL_SURFACE('',#17268,29.) ;
#1518 = CYLINDRICAL_SURFACE('',#17271,18.7631) ;
#1519 = CYLINDRICAL_SURFACE('',#17394,29.3077933083081) ;
#1520 = CYLINDRICAL_SURFACE('',#17486,27.082990178354) ;
#1521 = CYLINDRICAL_SURFACE('',#17501,22.5) ;
#1522 = CYLINDRICAL_SURFACE('',#17506,37.5) ;
#1523 = CYLINDRICAL_SURFACE('',#17808,36.5) ;
#1524 = CYLINDRICAL_SURFACE('',#17812,22.5) ;
#1525 = CYLINDRICAL_SURFACE('',#17820,3.3) ;
#1526 = CYLINDRICAL_SURFACE('',#17823,3.3) ;
#1527 = CYLINDRICAL_SURFACE('',#17826,3.3) ;
#1528 = CYLINDRICAL_SURFACE('',#17829,3.3) ;
#1529 = CYLINDRICAL_SURFACE('',#17832,3.3) ;
#1530 = CYLINDRICAL_SURFACE('',#17835,3.3) ;
#1531 = CYLINDRICAL_SURFACE('',#17838,3.3) ;
#1532 = CYLINDRICAL_SURFACE('',#17841,3.3) ;
#1533 = CYLINDRICAL_SURFACE('',#17844,33.5) ;
#1534 = CYLINDRICAL_SURFACE('',#17847,50.) ;
#1535 = CYLINDRICAL_SURFACE('',#17853,3.3) ;
#1536 = CYLINDRICAL_SURFACE('',#17856,3.3) ;
#1537 = CYLINDRICAL_SURFACE('',#17859,3.3) ;
#1538 = CYLINDRICAL_SURFACE('',#17862,3.3) ;
#1539 = CYLINDRICAL_SURFACE('',#17865,3.3) ;
#1540 = CYLINDRICAL_SURFACE('',#17868,3.3) ;
#1541 = CYLINDRICAL_SURFACE('',#17871,3.3) ;
#1542 = CYLINDRICAL_SURFACE('',#17874,3.3) ;
#1543 = CYLINDRICAL_SURFACE('',#17877,33.5) ;
#1544 = CYLINDRICAL_SURFACE('',#17880,50.) ;
#1545 = FACE_OUTER_BOUND('',#2406,.T.) ;
#1546 = FACE_OUTER_BOUND('',#2407,.T.) ;
#1547 = FACE_OUTER_BOUND('',#2408,.T.) ;
#1548 = FACE_OUTER_BOUND('',#2409,.T.) ;
#1549 = FACE_OUTER_BOUND('',#2410,.T.) ;
#1550 = FACE_OUTER_BOUND('',#2411,.T.) ;
#1551 = FACE_OUTER_BOUND('',#2412,.T.) ;
#1552 = FACE_OUTER_BOUND('',#2413,.T.) ;
#1553 = FACE_OUTER_BOUND('',#2414,.T.) ;
#1554 = FACE_OUTER_BOUND('',#2416,.T.) ;
#1555 = FACE_OUTER_BOUND('',#2417,.T.) ;
#1556 = FACE_OUTER_BOUND('',#2418,.T.) ;
#1557 = FACE_OUTER_BOUND('',#2420,.T.) ;
#1558 = FACE_OUTER_BOUND('',#2421,.T.) ;
#1559 = FACE_OUTER_BOUND('',#2422,.T.) ;
#1560 = FACE_OUTER_BOUND('',#2424,.T.) ;
#1561 = FACE_OUTER_BOUND('',#2425,.T.) ;
#1562 = FACE_OUTER_BOUND('',#2426,.T.) ;
#1563 = FACE_OUTER_BOUND('',#2428,.T.) ;
#1564 = FACE_OUTER_BOUND('',#2429,.T.) ;
#1565 = FACE_OUTER_BOUND('',#2430,.T.) ;
#1566 = FACE_OUTER_BOUND('',#2431,.T.) ;
#1567 = FACE_OUTER_BOUND('',#2432,.T.) ;
#1568 = FACE_OUTER_BOUND('',#2433,.T.) ;
#1569 = FACE_OUTER_BOUND('',#2434,.T.) ;
#1570 = FACE_OUTER_BOUND('',#2435,.T.) ;
#1571 = FACE_OUTER_BOUND('',#2436,.T.) ;
#1572 = FACE_OUTER_BOUND('',#2437,.T.) ;
#1573 = FACE_OUTER_BOUND('',#2438,.T.) ;
#1574 = FACE_OUTER_BOUND('',#2439,.T.) ;
#1575 = FACE_OUTER_BOUND('',#2440,.T.) ;
#1576 = FACE_OUTER_BOUND('',#2441,.T.) ;
#1577 = FACE_OUTER_BOUND('',#2442,.T.) ;
#1578 = FACE_OUTER_BOUND('',#2443,.T.) ;
#1579 = FACE_OUTER_BOUND('',#2444,.T.) ;
#1580 = FACE_OUTER_BOUND('',#2445,.T.) ;
#1581 = FACE_OUTER_BOUND('',#2446,.T.) ;
#1582 = FACE_OUTER_BOUND('',#2447,.T.) ;
#1583 = FACE_OUTER_BOUND('',#2450,.T.) ;
#1584 = FACE_OUTER_BOUND('',#2451,.T.) ;
#1585 = FACE_OUTER_BOUND('',#2454,.T.) ;
#1586 = FACE_OUTER_BOUND('',#2455,.T.) ;
#1587 = FACE_OUTER_BOUND('',#2461,.T.) ;
#1588 = FACE_OUTER_BOUND('',#2475,.T.) ;
#1589 = FACE_OUTER_BOUND('',#2477,.T.) ;
#1590 = FACE_OUTER_BOUND('',#2478,.T.) ;
#1591 = FACE_OUTER_BOUND('',#2479,.T.) ;
#1592 = FACE_OUTER_BOUND('',#2481,.T.) ;
#1593 = FACE_OUTER_BOUND('',#2482,.T.) ;
#1594 = FACE_OUTER_BOUND('',#2483,.T.) ;
#1595 = FACE_OUTER_BOUND('',#2485,.T.) ;
#1596 = FACE_OUTER_BOUND('',#2486,.T.) ;
#1597 = FACE_OUTER_BOUND('',#2487,.T.) ;
#1598 = FACE_OUTER_BOUND('',#2489,.T.) ;
#1599 = FACE_OUTER_BOUND('',#2490,.T.) ;
#1600 = FACE_OUTER_BOUND('',#2491,.T.) ;
#1601 = FACE_OUTER_BOUND('',#2493,.T.) ;
#1602 = FACE_OUTER_BOUND('',#2494,.T.) ;
#1603 = FACE_OUTER_BOUND('',#2495,.T.) ;
#1604 = FACE_OUTER_BOUND('',#2497,.T.) ;
#1605 = FACE_OUTER_BOUND('',#2498,.T.) ;
#1606 = FACE_OUTER_BOUND('',#2499,.T.) ;
#1607 = FACE_OUTER_BOUND('',#2501,.T.) ;
#1608 = FACE_OUTER_BOUND('',#2502,.T.) ;
#1609 = FACE_OUTER_BOUND('',#2503,.T.) ;
#1610 = FACE_OUTER_BOUND('',#2505,.T.) ;
#1611 = FACE_OUTER_BOUND('',#2506,.T.) ;
#1612 = FACE_OUTER_BOUND('',#2507,.T.) ;
#1613 = FACE_OUTER_BOUND('',#2509,.T.) ;
#1614 = FACE_OUTER_BOUND('',#2510,.T.) ;
#1615 = FACE_OUTER_BOUND('',#2511,.T.) ;
#1616 = FACE_OUTER_BOUND('',#2513,.T.) ;
#1617 = FACE_OUTER_BOUND('',#2514,.T.) ;
#1618 = FACE_OUTER_BOUND('',#2515,.T.) ;
#1619 = FACE_OUTER_BOUND('',#2517,.T.) ;
#1620 = FACE_OUTER_BOUND('',#2518,.T.) ;
#1621 = FACE_OUTER_BOUND('',#2519,.T.) ;
#1622 = FACE_OUTER_BOUND('',#2521,.T.) ;
#1623 = FACE_OUTER_BOUND('',#2522,.T.) ;
#1624 = FACE_OUTER_BOUND('',#2523,.T.) ;
#1625 = FACE_OUTER_BOUND('',#2536,.T.) ;
#1626 = FACE_OUTER_BOUND('',#2537,.T.) ;
#1627 = FACE_OUTER_BOUND('',#2550,.T.) ;
#1628 = FACE_OUTER_BOUND('',#2551,.T.) ;
#1629 = FACE_OUTER_BOUND('',#2552,.T.) ;
#1630 = FACE_OUTER_BOUND('',#2553,.T.) ;
#1631 = FACE_OUTER_BOUND('',#2554,.T.) ;
#1632 = FACE_OUTER_BOUND('',#2555,.T.) ;
#1633 = FACE_OUTER_BOUND('',#2556,.T.) ;
#1634 = FACE_OUTER_BOUND('',#2557,.T.) ;
#1635 = FACE_OUTER_BOUND('',#2558,.T.) ;
#1636 = FACE_OUTER_BOUND('',#2559,.T.) ;
#1637 = FACE_OUTER_BOUND('',#2560,.T.) ;
#1638 = FACE_OUTER_BOUND('',#2561,.T.) ;
#1639 = FACE_OUTER_BOUND('',#2562,.T.) ;
#1640 = FACE_OUTER_BOUND('',#2563,.T.) ;
#1641 = FACE_OUTER_BOUND('',#2564,.T.) ;
#1642 = FACE_OUTER_BOUND('',#2565,.T.) ;
#1643 = FACE_OUTER_BOUND('',#2568,.T.) ;
#1644 = FACE_OUTER_BOUND('',#2569,.T.) ;
#1645 = FACE_OUTER_BOUND('',#2570,.T.) ;
#1646 = FACE_OUTER_BOUND('',#2571,.T.) ;
#1647 = FACE_OUTER_BOUND('',#2572,.T.) ;
#1648 = FACE_OUTER_BOUND('',#2573,.T.) ;
#1649 = FACE_OUTER_BOUND('',#2576,.T.) ;
#1650 = FACE_OUTER_BOUND('',#2577,.T.) ;
#1651 = FACE_OUTER_BOUND('',#2580,.T.) ;
#1652 = FACE_OUTER_BOUND('',#2583,.T.) ;
#1653 = FACE_OUTER_BOUND('',#2584,.T.) ;
#1654 = FACE_OUTER_BOUND('',#2585,.T.) ;
#1655 = FACE_OUTER_BOUND('',#2586,.T.) ;
#1656 = FACE_OUTER_BOUND('',#2587,.T.) ;
#1657 = FACE_OUTER_BOUND('',#2588,.T.) ;
#1658 = FACE_OUTER_BOUND('',#2589,.T.) ;
#1659 = FACE_OUTER_BOUND('',#2590,.T.) ;
#1660 = FACE_OUTER_BOUND('',#2591,.T.) ;
#1661 = FACE_OUTER_BOUND('',#2592,.T.) ;
#1662 = FACE_OUTER_BOUND('',#2593,.T.) ;
#1663 = FACE_OUTER_BOUND('',#2594,.T.) ;
#1664 = FACE_OUTER_BOUND('',#2595,.T.) ;
#1665 = FACE_OUTER_BOUND('',#2597,.T.) ;
#1666 = FACE_OUTER_BOUND('',#2598,.T.) ;
#1667 = FACE_OUTER_BOUND('',#2599,.T.) ;
#1668 = FACE_OUTER_BOUND('',#2601,.T.) ;
#1669 = FACE_OUTER_BOUND('',#2602,.T.) ;
#1670 = FACE_OUTER_BOUND('',#2603,.T.) ;
#1671 = FACE_OUTER_BOUND('',#2605,.T.) ;
#1672 = FACE_OUTER_BOUND('',#2606,.T.) ;
#1673 = FACE_OUTER_BOUND('',#2607,.T.) ;
#1674 = FACE_OUTER_BOUND('',#2609,.T.) ;
#1675 = FACE_OUTER_BOUND('',#2610,.T.) ;
#1676 = FACE_OUTER_BOUND('',#2611,.T.) ;
#1677 = FACE_OUTER_BOUND('',#2612,.T.) ;
#1678 = FACE_OUTER_BOUND('',#2613,.T.) ;
#1679 = FACE_OUTER_BOUND('',#2614,.T.) ;
#1680 = FACE_OUTER_BOUND('',#2615,.T.) ;
#1681 = FACE_OUTER_BOUND('',#2616,.T.) ;
#1682 = FACE_OUTER_BOUND('',#2617,.T.) ;
#1683 = FACE_OUTER_BOUND('',#2618,.T.) ;
#1684 = FACE_OUTER_BOUND('',#2619,.T.) ;
#1685 = FACE_OUTER_BOUND('',#2620,.T.) ;
#1686 = FACE_OUTER_BOUND('',#2621,.T.) ;
#1687 = FACE_OUTER_BOUND('',#2622,.T.) ;
#1688 = FACE_OUTER_BOUND('',#2623,.T.) ;
#1689 = FACE_OUTER_BOUND('',#2624,.T.) ;
#1690 = FACE_OUTER_BOUND('',#2625,.T.) ;
#1691 = FACE_OUTER_BOUND('',#2626,.T.) ;
#1692 = FACE_OUTER_BOUND('',#2627,.T.) ;
#1693 = FACE_OUTER_BOUND('',#2628,.T.) ;
#1694 = FACE_OUTER_BOUND('',#2631,.T.) ;
#1695 = FACE_OUTER_BOUND('',#2632,.T.) ;
#1696 = FACE_OUTER_BOUND('',#2635,.T.) ;
#1697 = FACE_OUTER_BOUND('',#2636,.T.) ;
#1698 = FACE_OUTER_BOUND('',#2644,.T.) ;
#1699 = FACE_OUTER_BOUND('',#2658,.T.) ;
#1700 = FACE_OUTER_BOUND('',#2659,.T.) ;
#1701 = FACE_OUTER_BOUND('',#2660,.T.) ;
#1702 = FACE_OUTER_BOUND('',#2661,.T.) ;
#1703 = FACE_OUTER_BOUND('',#2662,.T.) ;
#1704 = FACE_OUTER_BOUND('',#2663,.T.) ;
#1705 = FACE_OUTER_BOUND('',#2664,.T.) ;
#1706 = FACE_OUTER_BOUND('',#2665,.T.) ;
#1707 = FACE_OUTER_BOUND('',#2666,.T.) ;
#1708 = FACE_OUTER_BOUND('',#2667,.T.) ;
#1709 = FACE_OUTER_BOUND('',#2668,.T.) ;
#1710 = FACE_OUTER_BOUND('',#2669,.T.) ;
#1711 = FACE_OUTER_BOUND('',#2670,.T.) ;
#1712 = FACE_OUTER_BOUND('',#2673,.T.) ;
#1713 = FACE_OUTER_BOUND('',#2674,.T.) ;
#1714 = FACE_OUTER_BOUND('',#2675,.T.) ;
#1715 = FACE_OUTER_BOUND('',#2676,.T.) ;
#1716 = FACE_OUTER_BOUND('',#2677,.T.) ;
#1717 = FACE_OUTER_BOUND('',#2678,.T.) ;
#1718 = FACE_OUTER_BOUND('',#2681,.T.) ;
#1719 = FACE_OUTER_BOUND('',#2682,.T.) ;
#1720 = FACE_OUTER_BOUND('',#2685,.T.) ;
#1721 = FACE_OUTER_BOUND('',#2688,.T.) ;
#1722 = FACE_OUTER_BOUND('',#2689,.T.) ;
#1723 = FACE_OUTER_BOUND('',#2690,.T.) ;
#1724 = FACE_OUTER_BOUND('',#2691,.T.) ;
#1725 = FACE_OUTER_BOUND('',#2692,.T.) ;
#1726 = FACE_OUTER_BOUND('',#2693,.T.) ;
#1727 = FACE_OUTER_BOUND('',#2694,.T.) ;
#1728 = FACE_OUTER_BOUND('',#2695,.T.) ;
#1729 = FACE_OUTER_BOUND('',#2696,.T.) ;
#1730 = FACE_OUTER_BOUND('',#2697,.T.) ;
#1731 = FACE_OUTER_BOUND('',#2698,.T.) ;
#1732 = FACE_OUTER_BOUND('',#2699,.T.) ;
#1733 = FACE_OUTER_BOUND('',#2700,.T.) ;
#1734 = FACE_OUTER_BOUND('',#2701,.T.) ;
#1735 = FACE_OUTER_BOUND('',#2702,.T.) ;
#1736 = FACE_OUTER_BOUND('',#2703,.T.) ;
#1737 = FACE_OUTER_BOUND('',#2704,.T.) ;
#1738 = FACE_OUTER_BOUND('',#2705,.T.) ;
#1739 = FACE_OUTER_BOUND('',#2706,.T.) ;
#1740 = FACE_OUTER_BOUND('',#2707,.T.) ;
#1741 = FACE_OUTER_BOUND('',#2708,.T.) ;
#1742 = FACE_OUTER_BOUND('',#2709,.T.) ;
#1743 = FACE_OUTER_BOUND('',#2710,.T.) ;
#1744 = FACE_OUTER_BOUND('',#2711,.T.) ;
#1745 = FACE_OUTER_BOUND('',#2712,.T.) ;
#1746 = FACE_OUTER_BOUND('',#2713,.T.) ;
#1747 = FACE_OUTER_BOUND('',#2714,.T.) ;
#1748 = FACE_OUTER_BOUND('',#2715,.T.) ;
#1749 = FACE_OUTER_BOUND('',#2716,.T.) ;
#1750 = FACE_OUTER_BOUND('',#2717,.T.) ;
#1751 = FACE_OUTER_BOUND('',#2718,.T.) ;
#1752 = FACE_OUTER_BOUND('',#2719,.T.) ;
#1753 = FACE_OUTER_BOUND('',#2720,.T.) ;
#1754 = FACE_OUTER_BOUND('',#2721,.T.) ;
#1755 = FACE_OUTER_BOUND('',#2722,.T.) ;
#1756 = FACE_OUTER_BOUND('',#2723,.T.) ;
#1757 = FACE_OUTER_BOUND('',#2724,.T.) ;
#1758 = FACE_OUTER_BOUND('',#2725,.T.) ;
#1759 = FACE_OUTER_BOUND('',#2726,.T.) ;
#1760 = FACE_OUTER_BOUND('',#2727,.T.) ;
#1761 = FACE_OUTER_BOUND('',#2728,.T.) ;
#1762 = FACE_OUTER_BOUND('',#2729,.T.) ;
#1763 = FACE_OUTER_BOUND('',#2730,.T.) ;
#1764 = FACE_OUTER_BOUND('',#2731,.T.) ;
#1765 = FACE_OUTER_BOUND('',#2732,.T.) ;
#1766 = FACE_OUTER_BOUND('',#2734,.T.) ;
#1767 = FACE_OUTER_BOUND('',#2735,.T.) ;
#1768 = FACE_OUTER_BOUND('',#2736,.T.) ;
#1769 = FACE_OUTER_BOUND('',#2737,.T.) ;
#1770 = FACE_OUTER_BOUND('',#2738,.T.) ;
#1771 = FACE_OUTER_BOUND('',#2740,.T.) ;
#1772 = FACE_OUTER_BOUND('',#2742,.T.) ;
#1773 = FACE_OUTER_BOUND('',#2743,.T.) ;
#1774 = FACE_OUTER_BOUND('',#2744,.T.) ;
#1775 = FACE_OUTER_BOUND('',#2746,.T.) ;
#1776 = FACE_OUTER_BOUND('',#2747,.T.) ;
#1777 = FACE_OUTER_BOUND('',#2748,.T.) ;
#1778 = FACE_OUTER_BOUND('',#2749,.T.) ;
#1779 = FACE_OUTER_BOUND('',#2750,.T.) ;
#1780 = FACE_OUTER_BOUND('',#2752,.T.) ;
#1781 = FACE_OUTER_BOUND('',#2753,.T.) ;
#1782 = FACE_OUTER_BOUND('',#2754,.T.) ;
#1783 = FACE_OUTER_BOUND('',#2756,.T.) ;
#1784 = FACE_OUTER_BOUND('',#2757,.T.) ;
#1785 = FACE_OUTER_BOUND('',#2761,.T.) ;
#1786 = FACE_OUTER_BOUND('',#2763,.T.) ;
#1787 = FACE_OUTER_BOUND('',#2764,.T.) ;
#1788 = FACE_OUTER_BOUND('',#2766,.T.) ;
#1789 = FACE_OUTER_BOUND('',#2767,.T.) ;
#1790 = FACE_OUTER_BOUND('',#2768,.T.) ;
#1791 = FACE_OUTER_BOUND('',#2769,.T.) ;
#1792 = FACE_OUTER_BOUND('',#2770,.T.) ;
#1793 = FACE_OUTER_BOUND('',#2771,.T.) ;
#1794 = FACE_OUTER_BOUND('',#2772,.T.) ;
#1795 = FACE_OUTER_BOUND('',#2773,.T.) ;
#1796 = FACE_OUTER_BOUND('',#2774,.T.) ;
#1797 = FACE_OUTER_BOUND('',#2776,.T.) ;
#1798 = FACE_OUTER_BOUND('',#2777,.T.) ;
#1799 = FACE_OUTER_BOUND('',#2778,.T.) ;
#1800 = FACE_OUTER_BOUND('',#2780,.T.) ;
#1801 = FACE_OUTER_BOUND('',#2781,.T.) ;
#1802 = FACE_OUTER_BOUND('',#2782,.T.) ;
#1803 = FACE_OUTER_BOUND('',#2783,.T.) ;
#1804 = FACE_OUTER_BOUND('',#2784,.T.) ;
#1805 = FACE_OUTER_BOUND('',#2785,.T.) ;
#1806 = FACE_OUTER_BOUND('',#2786,.T.) ;
#1807 = FACE_OUTER_BOUND('',#2788,.T.) ;
#1808 = FACE_OUTER_BOUND('',#2789,.T.) ;
#1809 = FACE_OUTER_BOUND('',#2790,.T.) ;
#1810 = FACE_OUTER_BOUND('',#2791,.T.) ;
#1811 = FACE_OUTER_BOUND('',#2793,.T.) ;
#1812 = FACE_OUTER_BOUND('',#2794,.T.) ;
#1813 = FACE_OUTER_BOUND('',#2796,.T.) ;
#1814 = FACE_OUTER_BOUND('',#2797,.T.) ;
#1815 = FACE_OUTER_BOUND('',#2799,.T.) ;
#1816 = FACE_OUTER_BOUND('',#2800,.T.) ;
#1817 = FACE_OUTER_BOUND('',#2801,.T.) ;
#1818 = FACE_OUTER_BOUND('',#2802,.T.) ;
#1819 = FACE_OUTER_BOUND('',#2803,.T.) ;
#1820 = FACE_OUTER_BOUND('',#2804,.T.) ;
#1821 = FACE_OUTER_BOUND('',#2805,.T.) ;
#1822 = FACE_OUTER_BOUND('',#2806,.T.) ;
#1823 = FACE_OUTER_BOUND('',#2807,.T.) ;
#1824 = FACE_OUTER_BOUND('',#2808,.T.) ;
#1825 = FACE_OUTER_BOUND('',#2809,.T.) ;
#1826 = FACE_OUTER_BOUND('',#2810,.T.) ;
#1827 = FACE_OUTER_BOUND('',#2812,.T.) ;
#1828 = FACE_OUTER_BOUND('',#2813,.T.) ;
#1829 = FACE_OUTER_BOUND('',#2814,.T.) ;
#1830 = FACE_OUTER_BOUND('',#2815,.T.) ;
#1831 = FACE_OUTER_BOUND('',#2816,.T.) ;
#1832 = FACE_OUTER_BOUND('',#2818,.T.) ;
#1833 = FACE_OUTER_BOUND('',#2819,.T.) ;
#1834 = FACE_OUTER_BOUND('',#2820,.T.) ;
#1835 = FACE_OUTER_BOUND('',#2821,.T.) ;
#1836 = FACE_OUTER_BOUND('',#2822,.T.) ;
#1837 = FACE_OUTER_BOUND('',#2824,.T.) ;
#1838 = FACE_OUTER_BOUND('',#2825,.T.) ;
#1839 = FACE_OUTER_BOUND('',#2826,.T.) ;
#1840 = FACE_OUTER_BOUND('',#2827,.T.) ;
#1841 = FACE_OUTER_BOUND('',#2828,.T.) ;
#1842 = FACE_OUTER_BOUND('',#2829,.T.) ;
#1843 = FACE_OUTER_BOUND('',#2830,.T.) ;
#1844 = FACE_OUTER_BOUND('',#2831,.T.) ;
#1845 = FACE_OUTER_BOUND('',#2832,.T.) ;
#1846 = FACE_OUTER_BOUND('',#2833,.T.) ;
#1847 = FACE_OUTER_BOUND('',#2834,.T.) ;
#1848 = FACE_OUTER_BOUND('',#2835,.T.) ;
#1849 = FACE_OUTER_BOUND('',#2836,.T.) ;
#1850 = FACE_OUTER_BOUND('',#2837,.T.) ;
#1851 = FACE_OUTER_BOUND('',#2838,.T.) ;
#1852 = FACE_OUTER_BOUND('',#2839,.T.) ;
#1853 = FACE_OUTER_BOUND('',#2840,.T.) ;
#1854 = FACE_OUTER_BOUND('',#2841,.T.) ;
#1855 = FACE_OUTER_BOUND('',#2842,.T.) ;
#1856 = FACE_OUTER_BOUND('',#2843,.T.) ;
#1857 = FACE_OUTER_BOUND('',#2844,.T.) ;
#1858 = FACE_OUTER_BOUND('',#2845,.T.) ;
#1859 = FACE_OUTER_BOUND('',#2846,.T.) ;
#1860 = FACE_OUTER_BOUND('',#2847,.T.) ;
#1861 = FACE_OUTER_BOUND('',#2848,.T.) ;
#1862 = FACE_OUTER_BOUND('',#2849,.T.) ;
#1863 = FACE_OUTER_BOUND('',#2850,.T.) ;
#1864 = FACE_OUTER_BOUND('',#2851,.T.) ;
#1865 = FACE_OUTER_BOUND('',#2852,.T.) ;
#1866 = FACE_OUTER_BOUND('',#2853,.T.) ;
#1867 = FACE_OUTER_BOUND('',#2854,.T.) ;
#1868 = FACE_OUTER_BOUND('',#2855,.T.) ;
#1869 = FACE_OUTER_BOUND('',#2856,.T.) ;
#1870 = FACE_OUTER_BOUND('',#2857,.T.) ;
#1871 = FACE_OUTER_BOUND('',#2858,.T.) ;
#1872 = FACE_OUTER_BOUND('',#2859,.T.) ;
#1873 = FACE_OUTER_BOUND('',#2860,.T.) ;
#1874 = FACE_OUTER_BOUND('',#2861,.T.) ;
#1875 = FACE_OUTER_BOUND('',#2862,.T.) ;
#1876 = FACE_OUTER_BOUND('',#2863,.T.) ;
#1877 = FACE_OUTER_BOUND('',#2864,.T.) ;
#1878 = FACE_OUTER_BOUND('',#2865,.T.) ;
#1879 = FACE_OUTER_BOUND('',#2866,.T.) ;
#1880 = FACE_OUTER_BOUND('',#2867,.T.) ;
#1881 = FACE_OUTER_BOUND('',#2868,.T.) ;
#1882 = FACE_OUTER_BOUND('',#2869,.T.) ;
#1883 = FACE_OUTER_BOUND('',#2870,.T.) ;
#1884 = FACE_OUTER_BOUND('',#2871,.T.) ;
#1885 = FACE_OUTER_BOUND('',#2872,.T.) ;
#1886 = FACE_OUTER_BOUND('',#2873,.T.) ;
#1887 = FACE_OUTER_BOUND('',#2874,.T.) ;
#1888 = FACE_OUTER_BOUND('',#2875,.T.) ;
#1889 = FACE_OUTER_BOUND('',#2876,.T.) ;
#1890 = FACE_OUTER_BOUND('',#2877,.T.) ;
#1891 = FACE_OUTER_BOUND('',#2878,.T.) ;
#1892 = FACE_OUTER_BOUND('',#2879,.T.) ;
#1893 = FACE_OUTER_BOUND('',#2880,.T.) ;
#1894 = FACE_OUTER_BOUND('',#2881,.T.) ;
#1895 = FACE_OUTER_BOUND('',#2882,.T.) ;
#1896 = FACE_OUTER_BOUND('',#2883,.T.) ;
#1897 = FACE_OUTER_BOUND('',#2884,.T.) ;
#1898 = FACE_OUTER_BOUND('',#2885,.T.) ;
#1899 = FACE_OUTER_BOUND('',#2887,.T.) ;
#1900 = FACE_OUTER_BOUND('',#2888,.T.) ;
#1901 = FACE_OUTER_BOUND('',#2889,.T.) ;
#1902 = FACE_OUTER_BOUND('',#2890,.T.) ;
#1903 = FACE_OUTER_BOUND('',#2891,.T.) ;
#1904 = FACE_OUTER_BOUND('',#2892,.T.) ;
#1905 = FACE_OUTER_BOUND('',#2893,.T.) ;
#1906 = FACE_OUTER_BOUND('',#2895,.T.) ;
#1907 = FACE_OUTER_BOUND('',#2896,.T.) ;
#1908 = FACE_OUTER_BOUND('',#2898,.T.) ;
#1909 = FACE_OUTER_BOUND('',#2899,.T.) ;
#1910 = FACE_OUTER_BOUND('',#2901,.T.) ;
#1911 = FACE_OUTER_BOUND('',#2902,.T.) ;
#1912 = FACE_OUTER_BOUND('',#2903,.T.) ;
#1913 = FACE_OUTER_BOUND('',#2904,.T.) ;
#1914 = FACE_OUTER_BOUND('',#2905,.T.) ;
#1915 = FACE_OUTER_BOUND('',#2906,.T.) ;
#1916 = FACE_OUTER_BOUND('',#2907,.T.) ;
#1917 = FACE_OUTER_BOUND('',#2908,.T.) ;
#1918 = FACE_OUTER_BOUND('',#2909,.T.) ;
#1919 = FACE_OUTER_BOUND('',#2910,.T.) ;
#1920 = FACE_OUTER_BOUND('',#2911,.T.) ;
#1921 = FACE_OUTER_BOUND('',#2912,.T.) ;
#1922 = FACE_OUTER_BOUND('',#2913,.T.) ;
#1923 = FACE_OUTER_BOUND('',#2914,.T.) ;
#1924 = FACE_OUTER_BOUND('',#2915,.T.) ;
#1925 = FACE_OUTER_BOUND('',#2916,.T.) ;
#1926 = FACE_OUTER_BOUND('',#2917,.T.) ;
#1927 = FACE_OUTER_BOUND('',#2918,.T.) ;
#1928 = FACE_OUTER_BOUND('',#2919,.T.) ;
#1929 = FACE_OUTER_BOUND('',#2920,.T.) ;
#1930 = FACE_OUTER_BOUND('',#2921,.T.) ;
#1931 = FACE_OUTER_BOUND('',#2922,.T.) ;
#1932 = FACE_OUTER_BOUND('',#2923,.T.) ;
#1933 = FACE_OUTER_BOUND('',#2924,.T.) ;
#1934 = FACE_OUTER_BOUND('',#2925,.T.) ;
#1935 = FACE_OUTER_BOUND('',#2926,.T.) ;
#1936 = FACE_OUTER_BOUND('',#2927,.T.) ;
#1937 = FACE_OUTER_BOUND('',#2928,.T.) ;
#1938 = FACE_OUTER_BOUND('',#2929,.T.) ;
#1939 = FACE_OUTER_BOUND('',#2930,.T.) ;
#1940 = FACE_OUTER_BOUND('',#2931,.T.) ;
#1941 = FACE_OUTER_BOUND('',#2932,.T.) ;
#1942 = FACE_OUTER_BOUND('',#2933,.T.) ;
#1943 = FACE_OUTER_BOUND('',#2934,.T.) ;
#1944 = FACE_OUTER_BOUND('',#2935,.T.) ;
#1945 = FACE_OUTER_BOUND('',#2936,.T.) ;
#1946 = FACE_OUTER_BOUND('',#2937,.T.) ;
#1947 = FACE_OUTER_BOUND('',#2938,.T.) ;
#1948 = FACE_OUTER_BOUND('',#2939,.T.) ;
#1949 = FACE_OUTER_BOUND('',#2940,.T.) ;
#1950 = FACE_OUTER_BOUND('',#2941,.T.) ;
#1951 = FACE_OUTER_BOUND('',#2942,.T.) ;
#1952 = FACE_OUTER_BOUND('',#2943,.T.) ;
#1953 = FACE_OUTER_BOUND('',#2944,.T.) ;
#1954 = FACE_OUTER_BOUND('',#2945,.T.) ;
#1955 = FACE_OUTER_BOUND('',#2946,.T.) ;
#1956 = FACE_OUTER_BOUND('',#2947,.T.) ;
#1957 = FACE_OUTER_BOUND('',#2948,.T.) ;
#1958 = FACE_OUTER_BOUND('',#2949,.T.) ;
#1959 = FACE_OUTER_BOUND('',#2950,.T.) ;
#1960 = FACE_OUTER_BOUND('',#2951,.T.) ;
#1961 = FACE_OUTER_BOUND('',#2952,.T.) ;
#1962 = FACE_OUTER_BOUND('',#2953,.T.) ;
#1963 = FACE_OUTER_BOUND('',#2954,.T.) ;
#1964 = FACE_OUTER_BOUND('',#2955,.T.) ;
#1965 = FACE_OUTER_BOUND('',#2956,.T.) ;
#1966 = FACE_OUTER_BOUND('',#2957,.T.) ;
#1967 = FACE_OUTER_BOUND('',#2958,.T.) ;
#1968 = FACE_OUTER_BOUND('',#2959,.T.) ;
#1969 = FACE_OUTER_BOUND('',#2960,.T.) ;
#1970 = FACE_OUTER_BOUND('',#2961,.T.) ;
#1971 = FACE_OUTER_BOUND('',#2962,.T.) ;
#1972 = FACE_OUTER_BOUND('',#2963,.T.) ;
#1973 = FACE_OUTER_BOUND('',#2964,.T.) ;
#1974 = FACE_OUTER_BOUND('',#2965,.T.) ;
#1975 = FACE_OUTER_BOUND('',#2966,.T.) ;
#1976 = FACE_OUTER_BOUND('',#2967,.T.) ;
#1977 = FACE_OUTER_BOUND('',#2968,.T.) ;
#1978 = FACE_OUTER_BOUND('',#2969,.T.) ;
#1979 = FACE_OUTER_BOUND('',#2970,.T.) ;
#1980 = FACE_OUTER_BOUND('',#2971,.T.) ;
#1981 = FACE_OUTER_BOUND('',#2972,.T.) ;
#1982 = FACE_OUTER_BOUND('',#2973,.T.) ;
#1983 = FACE_OUTER_BOUND('',#2974,.T.) ;
#1984 = FACE_OUTER_BOUND('',#2975,.T.) ;
#1985 = FACE_OUTER_BOUND('',#2976,.T.) ;
#1986 = FACE_OUTER_BOUND('',#2977,.T.) ;
#1987 = FACE_OUTER_BOUND('',#2978,.T.) ;
#1988 = FACE_OUTER_BOUND('',#2979,.T.) ;
#1989 = FACE_OUTER_BOUND('',#2980,.T.) ;
#1990 = FACE_OUTER_BOUND('',#2981,.T.) ;
#1991 = FACE_OUTER_BOUND('',#2982,.T.) ;
#1992 = FACE_OUTER_BOUND('',#2983,.T.) ;
#1993 = FACE_OUTER_BOUND('',#2984,.T.) ;
#1994 = FACE_OUTER_BOUND('',#2985,.T.) ;
#1995 = FACE_OUTER_BOUND('',#2986,.T.) ;
#1996 = FACE_OUTER_BOUND('',#2987,.T.) ;
#1997 = FACE_OUTER_BOUND('',#2988,.T.) ;
#1998 = FACE_OUTER_BOUND('',#2989,.T.) ;
#1999 = FACE_OUTER_BOUND('',#2990,.T.) ;
#2000 = FACE_OUTER_BOUND('',#2991,.T.) ;
#2001 = FACE_OUTER_BOUND('',#2992,.T.) ;
#2002 = FACE_OUTER_BOUND('',#2993,.T.) ;
#2003 = FACE_OUTER_BOUND('',#2994,.T.) ;
#2004 = FACE_OUTER_BOUND('',#2995,.T.) ;
#2005 = FACE_OUTER_BOUND('',#2996,.T.) ;
#2006 = FACE_OUTER_BOUND('',#2997,.T.) ;
#2007 = FACE_OUTER_BOUND('',#2998,.T.) ;
#2008 = FACE_OUTER_BOUND('',#2999,.T.) ;
#2009 = FACE_OUTER_BOUND('',#3000,.T.) ;
#2010 = FACE_OUTER_BOUND('',#3001,.T.) ;
#2011 = FACE_OUTER_BOUND('',#3002,.T.) ;
#2012 = FACE_OUTER_BOUND('',#3003,.T.) ;
#2013 = FACE_OUTER_BOUND('',#3004,.T.) ;
#2014 = FACE_OUTER_BOUND('',#3005,.T.) ;
#2015 = FACE_OUTER_BOUND('',#3006,.T.) ;
#2016 = FACE_OUTER_BOUND('',#3007,.T.) ;
#2017 = FACE_OUTER_BOUND('',#3008,.T.) ;
#2018 = FACE_OUTER_BOUND('',#3009,.T.) ;
#2019 = FACE_OUTER_BOUND('',#3010,.T.) ;
#2020 = FACE_OUTER_BOUND('',#3011,.T.) ;
#2021 = FACE_OUTER_BOUND('',#3012,.T.) ;
#2022 = FACE_OUTER_BOUND('',#3013,.T.) ;
#2023 = FACE_OUTER_BOUND('',#3014,.T.) ;
#2024 = FACE_OUTER_BOUND('',#3015,.T.) ;
#2025 = FACE_OUTER_BOUND('',#3016,.T.) ;
#2026 = FACE_OUTER_BOUND('',#3017,.T.) ;
#2027 = FACE_OUTER_BOUND('',#3018,.T.) ;
#2028 = FACE_OUTER_BOUND('',#3019,.T.) ;
#2029 = FACE_OUTER_BOUND('',#3020,.T.) ;
#2030 = FACE_OUTER_BOUND('',#3021,.T.) ;
#2031 = FACE_OUTER_BOUND('',#3022,.T.) ;
#2032 = FACE_OUTER_BOUND('',#3023,.T.) ;
#2033 = FACE_OUTER_BOUND('',#3024,.T.) ;
#2034 = FACE_OUTER_BOUND('',#3025,.T.) ;
#2035 = FACE_OUTER_BOUND('',#3026,.T.) ;
#2036 = FACE_OUTER_BOUND('',#3027,.T.) ;
#2037 = FACE_OUTER_BOUND('',#3028,.T.) ;
#2038 = FACE_OUTER_BOUND('',#3029,.T.) ;
#2039 = FACE_OUTER_BOUND('',#3030,.T.) ;
#2040 = FACE_OUTER_BOUND('',#3031,.T.) ;
#2041 = FACE_OUTER_BOUND('',#3032,.T.) ;
#2042 = FACE_OUTER_BOUND('',#3033,.T.) ;
#2043 = FACE_OUTER_BOUND('',#3034,.T.) ;
#2044 = FACE_OUTER_BOUND('',#3035,.T.) ;
#2045 = FACE_OUTER_BOUND('',#3036,.T.) ;
#2046 = FACE_OUTER_BOUND('',#3037,.T.) ;
#2047 = FACE_OUTER_BOUND('',#3038,.T.) ;
#2048 = FACE_OUTER_BOUND('',#3039,.T.) ;
#2049 = FACE_OUTER_BOUND('',#3040,.T.) ;
#2050 = FACE_OUTER_BOUND('',#3041,.T.) ;
#2051 = FACE_OUTER_BOUND('',#3042,.T.) ;
#2052 = FACE_OUTER_BOUND('',#3043,.T.) ;
#2053 = FACE_OUTER_BOUND('',#3044,.T.) ;
#2054 = FACE_OUTER_BOUND('',#3045,.T.) ;
#2055 = FACE_OUTER_BOUND('',#3046,.T.) ;
#2056 = FACE_OUTER_BOUND('',#3047,.T.) ;
#2057 = FACE_OUTER_BOUND('',#3048,.T.) ;
#2058 = FACE_OUTER_BOUND('',#3049,.T.) ;
#2059 = FACE_OUTER_BOUND('',#3050,.T.) ;
#2060 = FACE_OUTER_BOUND('',#3051,.T.) ;
#2061 = FACE_OUTER_BOUND('',#3052,.T.) ;
#2062 = FACE_OUTER_BOUND('',#3053,.T.) ;
#2063 = FACE_OUTER_BOUND('',#3054,.T.) ;
#2064 = FACE_OUTER_BOUND('',#3055,.T.) ;
#2065 = FACE_OUTER_BOUND('',#3056,.T.) ;
#2066 = FACE_OUTER_BOUND('',#3057,.T.) ;
#2067 = FACE_OUTER_BOUND('',#3058,.T.) ;
#2068 = FACE_OUTER_BOUND('',#3059,.T.) ;
#2069 = FACE_OUTER_BOUND('',#3060,.T.) ;
#2070 = FACE_OUTER_BOUND('',#3061,.T.) ;
#2071 = FACE_OUTER_BOUND('',#3062,.T.) ;
#2072 = FACE_OUTER_BOUND('',#3063,.T.) ;
#2073 = FACE_OUTER_BOUND('',#3064,.T.) ;
#2074 = FACE_OUTER_BOUND('',#3065,.T.) ;
#2075 = FACE_OUTER_BOUND('',#3066,.T.) ;
#2076 = FACE_OUTER_BOUND('',#3067,.T.) ;
#2077 = FACE_OUTER_BOUND('',#3068,.T.) ;
#2078 = FACE_OUTER_BOUND('',#3069,.T.) ;
#2079 = FACE_OUTER_BOUND('',#3070,.T.) ;
#2080 = FACE_OUTER_BOUND('',#3071,.T.) ;
#2081 = FACE_OUTER_BOUND('',#3072,.T.) ;
#2082 = FACE_OUTER_BOUND('',#3073,.T.) ;
#2083 = FACE_OUTER_BOUND('',#3074,.T.) ;
#2084 = FACE_OUTER_BOUND('',#3075,.T.) ;
#2085 = FACE_OUTER_BOUND('',#3076,.T.) ;
#2086 = FACE_OUTER_BOUND('',#3077,.T.) ;
#2087 = FACE_OUTER_BOUND('',#3078,.T.) ;
#2088 = FACE_OUTER_BOUND('',#3079,.T.) ;
#2089 = FACE_OUTER_BOUND('',#3080,.T.) ;
#2090 = FACE_OUTER_BOUND('',#3081,.T.) ;
#2091 = FACE_OUTER_BOUND('',#3082,.T.) ;
#2092 = FACE_OUTER_BOUND('',#3083,.T.) ;
#2093 = FACE_OUTER_BOUND('',#3084,.T.) ;
#2094 = FACE_OUTER_BOUND('',#3085,.T.) ;
#2095 = FACE_OUTER_BOUND('',#3086,.T.) ;
#2096 = FACE_OUTER_BOUND('',#3087,.T.) ;
#2097 = FACE_OUTER_BOUND('',#3088,.T.) ;
#2098 = FACE_OUTER_BOUND('',#3089,.T.) ;
#2099 = FACE_OUTER_BOUND('',#3090,.T.) ;
#2100 = FACE_OUTER_BOUND('',#3091,.T.) ;
#2101 = FACE_OUTER_BOUND('',#3092,.T.) ;
#2102 = FACE_OUTER_BOUND('',#3093,.T.) ;
#2103 = FACE_OUTER_BOUND('',#3094,.T.) ;
#2104 = FACE_OUTER_BOUND('',#3095,.T.) ;
#2105 = FACE_OUTER_BOUND('',#3096,.T.) ;
#2106 = FACE_OUTER_BOUND('',#3097,.T.) ;
#2107 = FACE_OUTER_BOUND('',#3098,.T.) ;
#2108 = FACE_OUTER_BOUND('',#3099,.T.) ;
#2109 = FACE_OUTER_BOUND('',#3100,.T.) ;
#2110 = FACE_OUTER_BOUND('',#3101,.T.) ;
#2111 = FACE_OUTER_BOUND('',#3102,.T.) ;
#2112 = FACE_OUTER_BOUND('',#3103,.T.) ;
#2113 = FACE_OUTER_BOUND('',#3104,.T.) ;
#2114 = FACE_OUTER_BOUND('',#3105,.T.) ;
#2115 = FACE_OUTER_BOUND('',#3106,.T.) ;
#2116 = FACE_OUTER_BOUND('',#3107,.T.) ;
#2117 = FACE_OUTER_BOUND('',#3108,.T.) ;
#2118 = FACE_OUTER_BOUND('',#3109,.T.) ;
#2119 = FACE_OUTER_BOUND('',#3110,.T.) ;
#2120 = FACE_OUTER_BOUND('',#3111,.T.) ;
#2121 = FACE_OUTER_BOUND('',#3112,.T.) ;
#2122 = FACE_OUTER_BOUND('',#3113,.T.) ;
#2123 = FACE_OUTER_BOUND('',#3114,.T.) ;
#2124 = FACE_OUTER_BOUND('',#3115,.T.) ;
#2125 = FACE_OUTER_BOUND('',#3116,.T.) ;
#2126 = FACE_OUTER_BOUND('',#3117,.T.) ;
#2127 = FACE_OUTER_BOUND('',#3118,.T.) ;
#2128 = FACE_OUTER_BOUND('',#3119,.T.) ;
#2129 = FACE_OUTER_BOUND('',#3120,.T.) ;
#2130 = FACE_OUTER_BOUND('',#3121,.T.) ;
#2131 = FACE_OUTER_BOUND('',#3122,.T.) ;
#2132 = FACE_OUTER_BOUND('',#3123,.T.) ;
#2133 = FACE_OUTER_BOUND('',#3124,.T.) ;
#2134 = FACE_OUTER_BOUND('',#3125,.T.) ;
#2135 = FACE_OUTER_BOUND('',#3126,.T.) ;
#2136 = FACE_OUTER_BOUND('',#3127,.T.) ;
#2137 = FACE_OUTER_BOUND('',#3128,.T.) ;
#2138 = FACE_OUTER_BOUND('',#3129,.T.) ;
#2139 = FACE_OUTER_BOUND('',#3130,.T.) ;
#2140 = FACE_OUTER_BOUND('',#3131,.T.) ;
#2141 = FACE_OUTER_BOUND('',#3132,.T.) ;
#2142 = FACE_OUTER_BOUND('',#3133,.T.) ;
#2143 = FACE_OUTER_BOUND('',#3134,.T.) ;
#2144 = FACE_OUTER_BOUND('',#3135,.T.) ;
#2145 = FACE_OUTER_BOUND('',#3136,.T.) ;
#2146 = FACE_OUTER_BOUND('',#3137,.T.) ;
#2147 = FACE_OUTER_BOUND('',#3138,.T.) ;
#2148 = FACE_OUTER_BOUND('',#3139,.T.) ;
#2149 = FACE_OUTER_BOUND('',#3140,.T.) ;
#2150 = FACE_OUTER_BOUND('',#3141,.T.) ;
#2151 = FACE_OUTER_BOUND('',#3142,.T.) ;
#2152 = FACE_OUTER_BOUND('',#3143,.T.) ;
#2153 = FACE_OUTER_BOUND('',#3144,.T.) ;
#2154 = FACE_OUTER_BOUND('',#3145,.T.) ;
#2155 = FACE_OUTER_BOUND('',#3146,.T.) ;
#2156 = FACE_OUTER_BOUND('',#3147,.T.) ;
#2157 = FACE_OUTER_BOUND('',#3148,.T.) ;
#2158 = FACE_OUTER_BOUND('',#3149,.T.) ;
#2159 = FACE_OUTER_BOUND('',#3150,.T.) ;
#2160 = FACE_OUTER_BOUND('',#3151,.T.) ;
#2161 = FACE_OUTER_BOUND('',#3152,.T.) ;
#2162 = FACE_OUTER_BOUND('',#3153,.T.) ;
#2163 = FACE_OUTER_BOUND('',#3154,.T.) ;
#2164 = FACE_OUTER_BOUND('',#3155,.T.) ;
#2165 = FACE_OUTER_BOUND('',#3156,.T.) ;
#2166 = FACE_OUTER_BOUND('',#3157,.T.) ;
#2167 = FACE_OUTER_BOUND('',#3158,.T.) ;
#2168 = FACE_OUTER_BOUND('',#3159,.T.) ;
#2169 = FACE_OUTER_BOUND('',#3160,.T.) ;
#2170 = FACE_OUTER_BOUND('',#3161,.T.) ;
#2171 = FACE_OUTER_BOUND('',#3162,.T.) ;
#2172 = FACE_OUTER_BOUND('',#3163,.T.) ;
#2173 = FACE_OUTER_BOUND('',#3164,.T.) ;
#2174 = FACE_OUTER_BOUND('',#3165,.T.) ;
#2175 = FACE_OUTER_BOUND('',#3166,.T.) ;
#2176 = FACE_OUTER_BOUND('',#3167,.T.) ;
#2177 = FACE_OUTER_BOUND('',#3168,.T.) ;
#2178 = FACE_OUTER_BOUND('',#3169,.T.) ;
#2179 = FACE_OUTER_BOUND('',#3170,.T.) ;
#2180 = FACE_OUTER_BOUND('',#3171,.T.) ;
#2181 = FACE_OUTER_BOUND('',#3172,.T.) ;
#2182 = FACE_OUTER_BOUND('',#3173,.T.) ;
#2183 = FACE_OUTER_BOUND('',#3174,.T.) ;
#2184 = FACE_OUTER_BOUND('',#3175,.T.) ;
#2185 = FACE_OUTER_BOUND('',#3176,.T.) ;
#2186 = FACE_OUTER_BOUND('',#3177,.T.) ;
#2187 = FACE_OUTER_BOUND('',#3178,.T.) ;
#2188 = FACE_OUTER_BOUND('',#3179,.T.) ;
#2189 = FACE_OUTER_BOUND('',#3180,.T.) ;
#2190 = FACE_OUTER_BOUND('',#3181,.T.) ;
#2191 = FACE_OUTER_BOUND('',#3182,.T.) ;
#2192 = FACE_OUTER_BOUND('',#3183,.T.) ;
#2193 = FACE_OUTER_BOUND('',#3184,.T.) ;
#2194 = FACE_OUTER_BOUND('',#3185,.T.) ;
#2195 = FACE_OUTER_BOUND('',#3186,.T.) ;
#2196 = FACE_OUTER_BOUND('',#3187,.T.) ;
#2197 = FACE_OUTER_BOUND('',#3188,.T.) ;
#2198 = FACE_OUTER_BOUND('',#3189,.T.) ;
#2199 = FACE_OUTER_BOUND('',#3190,.T.) ;
#2200 = FACE_OUTER_BOUND('',#3191,.T.) ;
#2201 = FACE_OUTER_BOUND('',#3192,.T.) ;
#2202 = FACE_OUTER_BOUND('',#3193,.T.) ;
#2203 = FACE_OUTER_BOUND('',#3194,.T.) ;
#2204 = FACE_OUTER_BOUND('',#3195,.T.) ;
#2205 = FACE_OUTER_BOUND('',#3196,.T.) ;
#2206 = FACE_OUTER_BOUND('',#3197,.T.) ;
#2207 = FACE_OUTER_BOUND('',#3198,.T.) ;
#2208 = FACE_OUTER_BOUND('',#3199,.T.) ;
#2209 = FACE_OUTER_BOUND('',#3200,.T.) ;
#2210 = FACE_OUTER_BOUND('',#3201,.T.) ;
#2211 = FACE_OUTER_BOUND('',#3202,.T.) ;
#2212 = FACE_OUTER_BOUND('',#3203,.T.) ;
#2213 = FACE_OUTER_BOUND('',#3204,.T.) ;
#2214 = FACE_OUTER_BOUND('',#3206,.T.) ;
#2215 = FACE_OUTER_BOUND('',#3207,.T.) ;
#2216 = FACE_OUTER_BOUND('',#3208,.T.) ;
#2217 = FACE_OUTER_BOUND('',#3209,.T.) ;
#2218 = FACE_OUTER_BOUND('',#3211,.T.) ;
#2219 = FACE_OUTER_BOUND('',#3212,.T.) ;
#2220 = FACE_OUTER_BOUND('',#3213,.T.) ;
#2221 = FACE_OUTER_BOUND('',#3214,.T.) ;
#2222 = FACE_OUTER_BOUND('',#3215,.T.) ;
#2223 = FACE_OUTER_BOUND('',#3217,.T.) ;
#2224 = FACE_OUTER_BOUND('',#3218,.T.) ;
#2225 = FACE_OUTER_BOUND('',#3219,.T.) ;
#2226 = FACE_OUTER_BOUND('',#3220,.T.) ;
#2227 = FACE_OUTER_BOUND('',#3221,.T.) ;
#2228 = FACE_OUTER_BOUND('',#3222,.T.) ;
#2229 = FACE_OUTER_BOUND('',#3223,.T.) ;
#2230 = FACE_OUTER_BOUND('',#3224,.T.) ;
#2231 = FACE_OUTER_BOUND('',#3225,.T.) ;
#2232 = FACE_OUTER_BOUND('',#3226,.T.) ;
#2233 = FACE_OUTER_BOUND('',#3227,.T.) ;
#2234 = FACE_OUTER_BOUND('',#3228,.T.) ;
#2235 = FACE_OUTER_BOUND('',#3229,.T.) ;
#2236 = FACE_OUTER_BOUND('',#3230,.T.) ;
#2237 = FACE_OUTER_BOUND('',#3231,.T.) ;
#2238 = FACE_OUTER_BOUND('',#3232,.T.) ;
#2239 = FACE_OUTER_BOUND('',#3233,.T.) ;
#2240 = FACE_OUTER_BOUND('',#3234,.T.) ;
#2241 = FACE_OUTER_BOUND('',#3236,.T.) ;
#2242 = FACE_OUTER_BOUND('',#3237,.T.) ;
#2243 = FACE_OUTER_BOUND('',#3238,.T.) ;
#2244 = FACE_OUTER_BOUND('',#3241,.T.) ;
#2245 = FACE_OUTER_BOUND('',#3242,.T.) ;
#2246 = FACE_OUTER_BOUND('',#3272,.T.) ;
#2247 = FACE_OUTER_BOUND('',#3273,.T.) ;
#2248 = FACE_OUTER_BOUND('',#3274,.T.) ;
#2249 = FACE_OUTER_BOUND('',#3275,.T.) ;
#2250 = FACE_OUTER_BOUND('',#3276,.T.) ;
#2251 = FACE_OUTER_BOUND('',#3277,.T.) ;
#2252 = FACE_OUTER_BOUND('',#3278,.T.) ;
#2253 = FACE_OUTER_BOUND('',#3279,.T.) ;
#2254 = FACE_OUTER_BOUND('',#3281,.T.) ;
#2255 = FACE_OUTER_BOUND('',#3283,.T.) ;
#2256 = FACE_OUTER_BOUND('',#3285,.T.) ;
#2257 = FACE_OUTER_BOUND('',#3286,.T.) ;
#2258 = FACE_OUTER_BOUND('',#3287,.T.) ;
#2259 = FACE_OUTER_BOUND('',#3288,.T.) ;
#2260 = FACE_OUTER_BOUND('',#3289,.T.) ;
#2261 = FACE_OUTER_BOUND('',#3290,.T.) ;
#2262 = FACE_OUTER_BOUND('',#3291,.T.) ;
#2263 = FACE_OUTER_BOUND('',#3292,.T.) ;
#2264 = FACE_OUTER_BOUND('',#3293,.T.) ;
#2265 = FACE_OUTER_BOUND('',#3294,.T.) ;
#2266 = FACE_OUTER_BOUND('',#3295,.T.) ;
#2267 = FACE_OUTER_BOUND('',#3296,.T.) ;
#2268 = FACE_OUTER_BOUND('',#3297,.T.) ;
#2269 = FACE_OUTER_BOUND('',#3298,.T.) ;
#2270 = FACE_OUTER_BOUND('',#3299,.T.) ;
#2271 = FACE_OUTER_BOUND('',#3300,.T.) ;
#2272 = FACE_OUTER_BOUND('',#3301,.T.) ;
#2273 = FACE_OUTER_BOUND('',#3302,.T.) ;
#2274 = FACE_OUTER_BOUND('',#3303,.T.) ;
#2275 = FACE_OUTER_BOUND('',#3304,.T.) ;
#2276 = FACE_OUTER_BOUND('',#3305,.T.) ;
#2277 = FACE_OUTER_BOUND('',#3306,.T.) ;
#2278 = FACE_OUTER_BOUND('',#3307,.T.) ;
#2279 = FACE_OUTER_BOUND('',#3308,.T.) ;
#2280 = FACE_OUTER_BOUND('',#3309,.T.) ;
#2281 = FACE_OUTER_BOUND('',#3310,.T.) ;
#2282 = FACE_OUTER_BOUND('',#3311,.T.) ;
#2283 = FACE_OUTER_BOUND('',#3312,.T.) ;
#2284 = FACE_OUTER_BOUND('',#3313,.T.) ;
#2285 = FACE_OUTER_BOUND('',#3315,.T.) ;
#2286 = FACE_OUTER_BOUND('',#3316,.T.) ;
#2287 = FACE_OUTER_BOUND('',#3317,.T.) ;
#2288 = FACE_OUTER_BOUND('',#3318,.T.) ;
#2289 = FACE_OUTER_BOUND('',#3319,.T.) ;
#2290 = FACE_OUTER_BOUND('',#3320,.T.) ;
#2291 = FACE_OUTER_BOUND('',#3321,.T.) ;
#2292 = FACE_OUTER_BOUND('',#3322,.T.) ;
#2293 = FACE_OUTER_BOUND('',#3323,.T.) ;
#2294 = FACE_OUTER_BOUND('',#3324,.T.) ;
#2295 = FACE_OUTER_BOUND('',#3325,.T.) ;
#2296 = FACE_OUTER_BOUND('',#3326,.T.) ;
#2297 = FACE_OUTER_BOUND('',#3327,.T.) ;
#2298 = FACE_OUTER_BOUND('',#3328,.T.) ;
#2299 = FACE_OUTER_BOUND('',#3329,.T.) ;
#2300 = FACE_OUTER_BOUND('',#3330,.T.) ;
#2301 = FACE_OUTER_BOUND('',#3331,.T.) ;
#2302 = FACE_OUTER_BOUND('',#3332,.T.) ;
#2303 = FACE_OUTER_BOUND('',#3333,.T.) ;
#2304 = FACE_OUTER_BOUND('',#3334,.T.) ;
#2305 = FACE_OUTER_BOUND('',#3335,.T.) ;
#2306 = FACE_OUTER_BOUND('',#3336,.T.) ;
#2307 = FACE_OUTER_BOUND('',#3337,.T.) ;
#2308 = FACE_OUTER_BOUND('',#3338,.T.) ;
#2309 = FACE_OUTER_BOUND('',#3339,.T.) ;
#2310 = FACE_OUTER_BOUND('',#3340,.T.) ;
#2311 = FACE_OUTER_BOUND('',#3341,.T.) ;
#2312 = FACE_OUTER_BOUND('',#3342,.T.) ;
#2313 = FACE_OUTER_BOUND('',#3343,.T.) ;
#2314 = FACE_OUTER_BOUND('',#3344,.T.) ;
#2315 = FACE_OUTER_BOUND('',#3345,.T.) ;
#2316 = FACE_OUTER_BOUND('',#3346,.T.) ;
#2317 = FACE_OUTER_BOUND('',#3347,.T.) ;
#2318 = FACE_OUTER_BOUND('',#3348,.T.) ;
#2319 = FACE_OUTER_BOUND('',#3349,.T.) ;
#2320 = FACE_OUTER_BOUND('',#3350,.T.) ;
#2321 = FACE_OUTER_BOUND('',#3351,.T.) ;
#2322 = FACE_OUTER_BOUND('',#3352,.T.) ;
#2323 = FACE_OUTER_BOUND('',#3353,.T.) ;
#2324 = FACE_OUTER_BOUND('',#3354,.T.) ;
#2325 = FACE_OUTER_BOUND('',#3355,.T.) ;
#2326 = FACE_OUTER_BOUND('',#3356,.T.) ;
#2327 = FACE_OUTER_BOUND('',#3357,.T.) ;
#2328 = FACE_OUTER_BOUND('',#3358,.T.) ;
#2329 = FACE_OUTER_BOUND('',#3359,.T.) ;
#2330 = FACE_OUTER_BOUND('',#3360,.T.) ;
#2331 = FACE_OUTER_BOUND('',#3361,.T.) ;
#2332 = FACE_OUTER_BOUND('',#3362,.T.) ;
#2333 = FACE_OUTER_BOUND('',#3363,.T.) ;
#2334 = FACE_OUTER_BOUND('',#3364,.T.) ;
#2335 = FACE_OUTER_BOUND('',#3365,.T.) ;
#2336 = FACE_OUTER_BOUND('',#3366,.T.) ;
#2337 = FACE_OUTER_BOUND('',#3367,.T.) ;
#2338 = FACE_OUTER_BOUND('',#3368,.T.) ;
#2339 = FACE_OUTER_BOUND('',#3369,.T.) ;
#2340 = FACE_OUTER_BOUND('',#3370,.T.) ;
#2341 = FACE_OUTER_BOUND('',#3371,.T.) ;
#2342 = FACE_OUTER_BOUND('',#3372,.T.) ;
#2343 = FACE_OUTER_BOUND('',#3373,.T.) ;
#2344 = FACE_OUTER_BOUND('',#3374,.T.) ;
#2345 = FACE_OUTER_BOUND('',#3375,.T.) ;
#2346 = FACE_OUTER_BOUND('',#3376,.T.) ;
#2347 = FACE_OUTER_BOUND('',#3377,.T.) ;
#2348 = FACE_OUTER_BOUND('',#3378,.T.) ;
#2349 = FACE_OUTER_BOUND('',#3379,.T.) ;
#2350 = FACE_OUTER_BOUND('',#3380,.T.) ;
#2351 = FACE_OUTER_BOUND('',#3381,.T.) ;
#2352 = FACE_OUTER_BOUND('',#3382,.T.) ;
#2353 = FACE_OUTER_BOUND('',#3383,.T.) ;
#2354 = FACE_OUTER_BOUND('',#3384,.T.) ;
#2355 = FACE_OUTER_BOUND('',#3385,.T.) ;
#2356 = FACE_OUTER_BOUND('',#3386,.T.) ;
#2357 = FACE_OUTER_BOUND('',#3387,.T.) ;
#2358 = FACE_OUTER_BOUND('',#3388,.T.) ;
#2359 = FACE_OUTER_BOUND('',#3389,.T.) ;
#2360 = FACE_OUTER_BOUND('',#3390,.T.) ;
#2361 = FACE_OUTER_BOUND('',#3391,.T.) ;
#2362 = FACE_OUTER_BOUND('',#3392,.T.) ;
#2363 = FACE_OUTER_BOUND('',#3393,.T.) ;
#2364 = FACE_OUTER_BOUND('',#3394,.T.) ;
#2365 = FACE_OUTER_BOUND('',#3395,.T.) ;
#2366 = FACE_OUTER_BOUND('',#3396,.T.) ;
#2367 = FACE_OUTER_BOUND('',#3397,.T.) ;
#2368 = FACE_OUTER_BOUND('',#3398,.T.) ;
#2369 = FACE_OUTER_BOUND('',#3399,.T.) ;
#2370 = FACE_OUTER_BOUND('',#3400,.T.) ;
#2371 = FACE_OUTER_BOUND('',#3401,.T.) ;
#2372 = FACE_OUTER_BOUND('',#3402,.T.) ;
#2373 = FACE_OUTER_BOUND('',#3403,.T.) ;
#2374 = FACE_OUTER_BOUND('',#3404,.T.) ;
#2375 = FACE_OUTER_BOUND('',#3405,.T.) ;
#2376 = FACE_OUTER_BOUND('',#3407,.T.) ;
#2377 = FACE_OUTER_BOUND('',#3408,.T.) ;
#2378 = FACE_OUTER_BOUND('',#3409,.T.) ;
#2379 = FACE_OUTER_BOUND('',#3410,.T.) ;
#2380 = FACE_OUTER_BOUND('',#3411,.T.) ;
#2381 = FACE_OUTER_BOUND('',#3413,.T.) ;
#2382 = FACE_OUTER_BOUND('',#3414,.T.) ;
#2383 = FACE_OUTER_BOUND('',#3415,.T.) ;
#2384 = FACE_OUTER_BOUND('',#3416,.T.) ;
#2385 = FACE_OUTER_BOUND('',#3417,.T.) ;
#2386 = FACE_OUTER_BOUND('',#3418,.T.) ;
#2387 = FACE_OUTER_BOUND('',#3419,.T.) ;
#2388 = FACE_OUTER_BOUND('',#3420,.T.) ;
#2389 = FACE_OUTER_BOUND('',#3421,.T.) ;
#2390 = FACE_OUTER_BOUND('',#3422,.T.) ;
#2391 = FACE_OUTER_BOUND('',#3423,.T.) ;
#2392 = FACE_OUTER_BOUND('',#3424,.T.) ;
#2393 = FACE_OUTER_BOUND('',#3434,.T.) ;
#2394 = FACE_OUTER_BOUND('',#3444,.T.) ;
#2395 = FACE_OUTER_BOUND('',#3445,.T.) ;
#2396 = FACE_OUTER_BOUND('',#3446,.T.) ;
#2397 = FACE_OUTER_BOUND('',#3447,.T.) ;
#2398 = FACE_OUTER_BOUND('',#3448,.T.) ;
#2399 = FACE_OUTER_BOUND('',#3449,.T.) ;
#2400 = FACE_OUTER_BOUND('',#3450,.T.) ;
#2401 = FACE_OUTER_BOUND('',#3451,.T.) ;
#2402 = FACE_OUTER_BOUND('',#3452,.T.) ;
#2403 = FACE_OUTER_BOUND('',#3453,.T.) ;
#2404 = FACE_OUTER_BOUND('',#3454,.T.) ;
#2405 = FACE_OUTER_BOUND('',#3464,.T.) ;
#2406 = EDGE_LOOP('',(#9802,#9803,#9804)) ;
#2407 = EDGE_LOOP('',(#9805,#9806,#9807,#9808)) ;
#2408 = EDGE_LOOP('',(#9809,#9810,#9811)) ;
#2409 = EDGE_LOOP('',(#9812,#9813,#9814,#9815)) ;
#2410 = EDGE_LOOP('',(#9816,#9817,#9818)) ;
#2411 = EDGE_LOOP('',(#9819,#9820,#9821,#9822)) ;
#2412 = EDGE_LOOP('',(#9823,#9824,#9825)) ;
#2413 = EDGE_LOOP('',(#9826,#9827,#9828,#9829)) ;
#2414 = EDGE_LOOP('',(#9830)) ;
#2415 = EDGE_LOOP('',(#9831)) ;
#2416 = EDGE_LOOP('',(#9832,#9833,#9834,#9835)) ;
#2417 = EDGE_LOOP('',(#9836,#9837,#9838,#9839)) ;
#2418 = EDGE_LOOP('',(#9840)) ;
#2419 = EDGE_LOOP('',(#9841)) ;
#2420 = EDGE_LOOP('',(#9842,#9843,#9844,#9845)) ;
#2421 = EDGE_LOOP('',(#9846,#9847,#9848,#9849)) ;
#2422 = EDGE_LOOP('',(#9850)) ;
#2423 = EDGE_LOOP('',(#9851)) ;
#2424 = EDGE_LOOP('',(#9852,#9853,#9854,#9855)) ;
#2425 = EDGE_LOOP('',(#9856,#9857,#9858,#9859)) ;
#2426 = EDGE_LOOP('',(#9860)) ;
#2427 = EDGE_LOOP('',(#9861)) ;
#2428 = EDGE_LOOP('',(#9862,#9863,#9864,#9865)) ;
#2429 = EDGE_LOOP('',(#9866,#9867,#9868,#9869)) ;
#2430 = EDGE_LOOP('',(#9870,#9871,#9872)) ;
#2431 = EDGE_LOOP('',(#9873,#9874,#9875,#9876)) ;
#2432 = EDGE_LOOP('',(#9877,#9878,#9879)) ;
#2433 = EDGE_LOOP('',(#9880,#9881,#9882,#9883)) ;
#2434 = EDGE_LOOP('',(#9884,#9885,#9886)) ;
#2435 = EDGE_LOOP('',(#9887,#9888,#9889,#9890)) ;
#2436 = EDGE_LOOP('',(#9891,#9892,#9893)) ;
#2437 = EDGE_LOOP('',(#9894,#9895,#9896,#9897)) ;
#2438 = EDGE_LOOP('',(#9898,#9899,#9900)) ;
#2439 = EDGE_LOOP('',(#9901,#9902,#9903,#9904)) ;
#2440 = EDGE_LOOP('',(#9905,#9906,#9907)) ;
#2441 = EDGE_LOOP('',(#9908,#9909,#9910,#9911)) ;
#2442 = EDGE_LOOP('',(#9912,#9913,#9914)) ;
#2443 = EDGE_LOOP('',(#9915,#9916,#9917,#9918)) ;
#2444 = EDGE_LOOP('',(#9919,#9920,#9921)) ;
#2445 = EDGE_LOOP('',(#9922,#9923,#9924,#9925)) ;
#2446 = EDGE_LOOP('',(#9926,#9927,#9928,#9929)) ;
#2447 = EDGE_LOOP('',(#9930,#9931,#9932,#9933)) ;
#2448 = EDGE_LOOP('',(#9934)) ;
#2449 = EDGE_LOOP('',(#9935)) ;
#2450 = EDGE_LOOP('',(#9936,#9937,#9938,#9939)) ;
#2451 = EDGE_LOOP('',(#9940,#9941,#9942,#9943)) ;
#2452 = EDGE_LOOP('',(#9944)) ;
#2453 = EDGE_LOOP('',(#9945)) ;
#2454 = EDGE_LOOP('',(#9946,#9947,#9948,#9949)) ;
#2455 = EDGE_LOOP('',(#9950,#9951,#9952,#9953)) ;
#2456 = EDGE_LOOP('',(#9954)) ;
#2457 = EDGE_LOOP('',(#9955)) ;
#2458 = EDGE_LOOP('',(#9956)) ;
#2459 = EDGE_LOOP('',(#9957)) ;
#2460 = EDGE_LOOP('',(#9958)) ;
#2461 = EDGE_LOOP('',(#9959,#9960,#9961,#9962)) ;
#2462 = EDGE_LOOP('',(#9963)) ;
#2463 = EDGE_LOOP('',(#9964)) ;
#2464 = EDGE_LOOP('',(#9965)) ;
#2465 = EDGE_LOOP('',(#9966)) ;
#2466 = EDGE_LOOP('',(#9967)) ;
#2467 = EDGE_LOOP('',(#9968)) ;
#2468 = EDGE_LOOP('',(#9969)) ;
#2469 = EDGE_LOOP('',(#9970)) ;
#2470 = EDGE_LOOP('',(#9971)) ;
#2471 = EDGE_LOOP('',(#9972)) ;
#2472 = EDGE_LOOP('',(#9973)) ;
#2473 = EDGE_LOOP('',(#9974)) ;
#2474 = EDGE_LOOP('',(#9975)) ;
#2475 = EDGE_LOOP('',(#9976)) ;
#2476 = EDGE_LOOP('',(#9977)) ;
#2477 = EDGE_LOOP('',(#9978,#9979,#9980,#9981)) ;
#2478 = EDGE_LOOP('',(#9982,#9983,#9984,#9985)) ;
#2479 = EDGE_LOOP('',(#9986)) ;
#2480 = EDGE_LOOP('',(#9987)) ;
#2481 = EDGE_LOOP('',(#9988,#9989,#9990,#9991)) ;
#2482 = EDGE_LOOP('',(#9992,#9993,#9994,#9995)) ;
#2483 = EDGE_LOOP('',(#9996)) ;
#2484 = EDGE_LOOP('',(#9997)) ;
#2485 = EDGE_LOOP('',(#9998,#9999,#10000,#10001)) ;
#2486 = EDGE_LOOP('',(#10002,#10003,#10004,#10005)) ;
#2487 = EDGE_LOOP('',(#10006)) ;
#2488 = EDGE_LOOP('',(#10007)) ;
#2489 = EDGE_LOOP('',(#10008,#10009,#10010,#10011)) ;
#2490 = EDGE_LOOP('',(#10012,#10013,#10014,#10015)) ;
#2491 = EDGE_LOOP('',(#10016)) ;
#2492 = EDGE_LOOP('',(#10017)) ;
#2493 = EDGE_LOOP('',(#10018,#10019,#10020,#10021)) ;
#2494 = EDGE_LOOP('',(#10022,#10023,#10024,#10025)) ;
#2495 = EDGE_LOOP('',(#10026)) ;
#2496 = EDGE_LOOP('',(#10027)) ;
#2497 = EDGE_LOOP('',(#10028,#10029,#10030,#10031)) ;
#2498 = EDGE_LOOP('',(#10032,#10033,#10034,#10035)) ;
#2499 = EDGE_LOOP('',(#10036)) ;
#2500 = EDGE_LOOP('',(#10037)) ;
#2501 = EDGE_LOOP('',(#10038,#10039,#10040,#10041)) ;
#2502 = EDGE_LOOP('',(#10042,#10043,#10044,#10045)) ;
#2503 = EDGE_LOOP('',(#10046)) ;
#2504 = EDGE_LOOP('',(#10047)) ;
#2505 = EDGE_LOOP('',(#10048,#10049,#10050,#10051)) ;
#2506 = EDGE_LOOP('',(#10052,#10053,#10054,#10055)) ;
#2507 = EDGE_LOOP('',(#10056)) ;
#2508 = EDGE_LOOP('',(#10057)) ;
#2509 = EDGE_LOOP('',(#10058,#10059,#10060,#10061)) ;
#2510 = EDGE_LOOP('',(#10062,#10063,#10064,#10065)) ;
#2511 = EDGE_LOOP('',(#10066)) ;
#2512 = EDGE_LOOP('',(#10067)) ;
#2513 = EDGE_LOOP('',(#10068,#10069,#10070,#10071)) ;
#2514 = EDGE_LOOP('',(#10072,#10073,#10074,#10075)) ;
#2515 = EDGE_LOOP('',(#10076)) ;
#2516 = EDGE_LOOP('',(#10077)) ;
#2517 = EDGE_LOOP('',(#10078,#10079,#10080,#10081)) ;
#2518 = EDGE_LOOP('',(#10082,#10083,#10084,#10085)) ;
#2519 = EDGE_LOOP('',(#10086)) ;
#2520 = EDGE_LOOP('',(#10087)) ;
#2521 = EDGE_LOOP('',(#10088,#10089,#10090,#10091)) ;
#2522 = EDGE_LOOP('',(#10092,#10093,#10094,#10095)) ;
#2523 = EDGE_LOOP('',(#10096,#10097,#10098,#10099)) ;
#2524 = EDGE_LOOP('',(#10100)) ;
#2525 = EDGE_LOOP('',(#10101)) ;
#2526 = EDGE_LOOP('',(#10102)) ;
#2527 = EDGE_LOOP('',(#10103)) ;
#2528 = EDGE_LOOP('',(#10104)) ;
#2529 = EDGE_LOOP('',(#10105)) ;
#2530 = EDGE_LOOP('',(#10106)) ;
#2531 = EDGE_LOOP('',(#10107)) ;
#2532 = EDGE_LOOP('',(#10108)) ;
#2533 = EDGE_LOOP('',(#10109)) ;
#2534 = EDGE_LOOP('',(#10110)) ;
#2535 = EDGE_LOOP('',(#10111)) ;
#2536 = EDGE_LOOP('',(#10112,#10113,#10114,#10115)) ;
#2537 = EDGE_LOOP('',(#10116,#10117,#10118,#10119)) ;
#2538 = EDGE_LOOP('',(#10120)) ;
#2539 = EDGE_LOOP('',(#10121)) ;
#2540 = EDGE_LOOP('',(#10122)) ;
#2541 = EDGE_LOOP('',(#10123)) ;
#2542 = EDGE_LOOP('',(#10124)) ;
#2543 = EDGE_LOOP('',(#10125)) ;
#2544 = EDGE_LOOP('',(#10126)) ;
#2545 = EDGE_LOOP('',(#10127)) ;
#2546 = EDGE_LOOP('',(#10128)) ;
#2547 = EDGE_LOOP('',(#10129)) ;
#2548 = EDGE_LOOP('',(#10130)) ;
#2549 = EDGE_LOOP('',(#10131)) ;
#2550 = EDGE_LOOP('',(#10132,#10133,#10134,#10135)) ;
#2551 = EDGE_LOOP('',(#10136,#10137,#10138,#10139)) ;
#2552 = EDGE_LOOP('',(#10140,#10141,#10142,#10143)) ;
#2553 = EDGE_LOOP('',(#10144,#10145,#10146)) ;
#2554 = EDGE_LOOP('',(#10147,#10148,#10149,#10150)) ;
#2555 = EDGE_LOOP('',(#10151,#10152,#10153)) ;
#2556 = EDGE_LOOP('',(#10154,#10155,#10156,#10157)) ;
#2557 = EDGE_LOOP('',(#10158,#10159,#10160)) ;
#2558 = EDGE_LOOP('',(#10161,#10162,#10163,#10164)) ;
#2559 = EDGE_LOOP('',(#10165,#10166,#10167)) ;
#2560 = EDGE_LOOP('',(#10168,#10169,#10170,#10171)) ;
#2561 = EDGE_LOOP('',(#10172,#10173,#10174)) ;
#2562 = EDGE_LOOP('',(#10175,#10176,#10177,#10178)) ;
#2563 = EDGE_LOOP('',(#10179,#10180,#10181)) ;
#2564 = EDGE_LOOP('',(#10182,#10183,#10184,#10185)) ;
#2565 = EDGE_LOOP('',(#10186,#10187,#10188,#10189)) ;
#2566 = EDGE_LOOP('',(#10190)) ;
#2567 = EDGE_LOOP('',(#10191)) ;
#2568 = EDGE_LOOP('',(#10192,#10193,#10194)) ;
#2569 = EDGE_LOOP('',(#10195,#10196,#10197,#10198)) ;
#2570 = EDGE_LOOP('',(#10199,#10200,#10201)) ;
#2571 = EDGE_LOOP('',(#10202,#10203,#10204,#10205)) ;
#2572 = EDGE_LOOP('',(#10206,#10207,#10208,#10209)) ;
#2573 = EDGE_LOOP('',(#10210,#10211,#10212,#10213)) ;
#2574 = EDGE_LOOP('',(#10214)) ;
#2575 = EDGE_LOOP('',(#10215)) ;
#2576 = EDGE_LOOP('',(#10216,#10217,#10218,#10219)) ;
#2577 = EDGE_LOOP('',(#10220,#10221,#10222,#10223)) ;
#2578 = EDGE_LOOP('',(#10224)) ;
#2579 = EDGE_LOOP('',(#10225)) ;
#2580 = EDGE_LOOP('',(#10226,#10227,#10228,#10229)) ;
#2581 = EDGE_LOOP('',(#10230)) ;
#2582 = EDGE_LOOP('',(#10231)) ;
#2583 = EDGE_LOOP('',(#10232,#10233,#10234)) ;
#2584 = EDGE_LOOP('',(#10235,#10236,#10237,#10238)) ;
#2585 = EDGE_LOOP('',(#10239,#10240,#10241)) ;
#2586 = EDGE_LOOP('',(#10242,#10243,#10244,#10245)) ;
#2587 = EDGE_LOOP('',(#10246,#10247,#10248)) ;
#2588 = EDGE_LOOP('',(#10249,#10250,#10251,#10252)) ;
#2589 = EDGE_LOOP('',(#10253,#10254,#10255)) ;
#2590 = EDGE_LOOP('',(#10256,#10257,#10258,#10259)) ;
#2591 = EDGE_LOOP('',(#10260,#10261,#10262)) ;
#2592 = EDGE_LOOP('',(#10263,#10264,#10265,#10266)) ;
#2593 = EDGE_LOOP('',(#10267,#10268,#10269)) ;
#2594 = EDGE_LOOP('',(#10270,#10271,#10272,#10273)) ;
#2595 = EDGE_LOOP('',(#10274)) ;
#2596 = EDGE_LOOP('',(#10275)) ;
#2597 = EDGE_LOOP('',(#10276,#10277,#10278,#10279)) ;
#2598 = EDGE_LOOP('',(#10280,#10281,#10282,#10283)) ;
#2599 = EDGE_LOOP('',(#10284)) ;
#2600 = EDGE_LOOP('',(#10285)) ;
#2601 = EDGE_LOOP('',(#10286,#10287,#10288,#10289)) ;
#2602 = EDGE_LOOP('',(#10290,#10291,#10292,#10293)) ;
#2603 = EDGE_LOOP('',(#10294)) ;
#2604 = EDGE_LOOP('',(#10295)) ;
#2605 = EDGE_LOOP('',(#10296,#10297,#10298,#10299)) ;
#2606 = EDGE_LOOP('',(#10300,#10301,#10302,#10303)) ;
#2607 = EDGE_LOOP('',(#10304)) ;
#2608 = EDGE_LOOP('',(#10305)) ;
#2609 = EDGE_LOOP('',(#10306,#10307,#10308,#10309)) ;
#2610 = EDGE_LOOP('',(#10310,#10311,#10312,#10313)) ;
#2611 = EDGE_LOOP('',(#10314,#10315,#10316)) ;
#2612 = EDGE_LOOP('',(#10317,#10318,#10319,#10320)) ;
#2613 = EDGE_LOOP('',(#10321,#10322,#10323)) ;
#2614 = EDGE_LOOP('',(#10324,#10325,#10326,#10327)) ;
#2615 = EDGE_LOOP('',(#10328,#10329,#10330)) ;
#2616 = EDGE_LOOP('',(#10331,#10332,#10333,#10334)) ;
#2617 = EDGE_LOOP('',(#10335,#10336,#10337)) ;
#2618 = EDGE_LOOP('',(#10338,#10339,#10340,#10341)) ;
#2619 = EDGE_LOOP('',(#10342,#10343,#10344)) ;
#2620 = EDGE_LOOP('',(#10345,#10346,#10347,#10348)) ;
#2621 = EDGE_LOOP('',(#10349,#10350,#10351)) ;
#2622 = EDGE_LOOP('',(#10352,#10353,#10354,#10355)) ;
#2623 = EDGE_LOOP('',(#10356,#10357,#10358)) ;
#2624 = EDGE_LOOP('',(#10359,#10360,#10361,#10362)) ;
#2625 = EDGE_LOOP('',(#10363,#10364,#10365)) ;
#2626 = EDGE_LOOP('',(#10366,#10367,#10368,#10369)) ;
#2627 = EDGE_LOOP('',(#10370,#10371,#10372,#10373)) ;
#2628 = EDGE_LOOP('',(#10374,#10375,#10376,#10377)) ;
#2629 = EDGE_LOOP('',(#10378)) ;
#2630 = EDGE_LOOP('',(#10379)) ;
#2631 = EDGE_LOOP('',(#10380,#10381,#10382,#10383)) ;
#2632 = EDGE_LOOP('',(#10384,#10385,#10386,#10387)) ;
#2633 = EDGE_LOOP('',(#10388)) ;
#2634 = EDGE_LOOP('',(#10389)) ;
#2635 = EDGE_LOOP('',(#10390,#10391,#10392,#10393)) ;
#2636 = EDGE_LOOP('',(#10394,#10395,#10396,#10397)) ;
#2637 = EDGE_LOOP('',(#10398)) ;
#2638 = EDGE_LOOP('',(#10399)) ;
#2639 = EDGE_LOOP('',(#10400)) ;
#2640 = EDGE_LOOP('',(#10401)) ;
#2641 = EDGE_LOOP('',(#10402)) ;
#2642 = EDGE_LOOP('',(#10403)) ;
#2643 = EDGE_LOOP('',(#10404)) ;
#2644 = EDGE_LOOP('',(#10405,#10406,#10407,#10408)) ;
#2645 = EDGE_LOOP('',(#10409)) ;
#2646 = EDGE_LOOP('',(#10410)) ;
#2647 = EDGE_LOOP('',(#10411)) ;
#2648 = EDGE_LOOP('',(#10412)) ;
#2649 = EDGE_LOOP('',(#10413)) ;
#2650 = EDGE_LOOP('',(#10414)) ;
#2651 = EDGE_LOOP('',(#10415)) ;
#2652 = EDGE_LOOP('',(#10416)) ;
#2653 = EDGE_LOOP('',(#10417)) ;
#2654 = EDGE_LOOP('',(#10418)) ;
#2655 = EDGE_LOOP('',(#10419)) ;
#2656 = EDGE_LOOP('',(#10420)) ;
#2657 = EDGE_LOOP('',(#10421)) ;
#2658 = EDGE_LOOP('',(#10422,#10423,#10424)) ;
#2659 = EDGE_LOOP('',(#10425,#10426,#10427,#10428)) ;
#2660 = EDGE_LOOP('',(#10429,#10430,#10431)) ;
#2661 = EDGE_LOOP('',(#10432,#10433,#10434,#10435)) ;
#2662 = EDGE_LOOP('',(#10436,#10437,#10438)) ;
#2663 = EDGE_LOOP('',(#10439,#10440,#10441,#10442)) ;
#2664 = EDGE_LOOP('',(#10443,#10444,#10445)) ;
#2665 = EDGE_LOOP('',(#10446,#10447,#10448,#10449)) ;
#2666 = EDGE_LOOP('',(#10450,#10451,#10452)) ;
#2667 = EDGE_LOOP('',(#10453,#10454,#10455,#10456)) ;
#2668 = EDGE_LOOP('',(#10457,#10458,#10459)) ;
#2669 = EDGE_LOOP('',(#10460,#10461,#10462,#10463)) ;
#2670 = EDGE_LOOP('',(#10464,#10465,#10466,#10467)) ;
#2671 = EDGE_LOOP('',(#10468)) ;
#2672 = EDGE_LOOP('',(#10469)) ;
#2673 = EDGE_LOOP('',(#10470,#10471,#10472)) ;
#2674 = EDGE_LOOP('',(#10473,#10474,#10475,#10476)) ;
#2675 = EDGE_LOOP('',(#10477,#10478,#10479)) ;
#2676 = EDGE_LOOP('',(#10480,#10481,#10482,#10483)) ;
#2677 = EDGE_LOOP('',(#10484,#10485,#10486,#10487)) ;
#2678 = EDGE_LOOP('',(#10488,#10489,#10490,#10491)) ;
#2679 = EDGE_LOOP('',(#10492)) ;
#2680 = EDGE_LOOP('',(#10493)) ;
#2681 = EDGE_LOOP('',(#10494,#10495,#10496,#10497)) ;
#2682 = EDGE_LOOP('',(#10498,#10499,#10500,#10501)) ;
#2683 = EDGE_LOOP('',(#10502)) ;
#2684 = EDGE_LOOP('',(#10503)) ;
#2685 = EDGE_LOOP('',(#10504,#10505,#10506,#10507)) ;
#2686 = EDGE_LOOP('',(#10508)) ;
#2687 = EDGE_LOOP('',(#10509)) ;
#2688 = EDGE_LOOP('',(#10510,#10511,#10512,#10513)) ;
#2689 = EDGE_LOOP('',(#10514,#10515,#10516,#10517)) ;
#2690 = EDGE_LOOP('',(#10518,#10519,#10520,#10521)) ;
#2691 = EDGE_LOOP('',(#10522,#10523,#10524,#10525)) ;
#2692 = EDGE_LOOP('',(#10526,#10527,#10528,#10529)) ;
#2693 = EDGE_LOOP('',(#10530,#10531,#10532,#10533)) ;
#2694 = EDGE_LOOP('',(#10534,#10535,#10536,#10537)) ;
#2695 = EDGE_LOOP('',(#10538,#10539,#10540,#10541)) ;
#2696 = EDGE_LOOP('',(#10542,#10543,#10544,#10545)) ;
#2697 = EDGE_LOOP('',(#10546,#10547,#10548,#10549)) ;
#2698 = EDGE_LOOP('',(#10550,#10551,#10552,#10553)) ;
#2699 = EDGE_LOOP('',(#10554,#10555,#10556,#10557)) ;
#2700 = EDGE_LOOP('',(#10558,#10559,#10560,#10561)) ;
#2701 = EDGE_LOOP('',(#10562,#10563,#10564,#10565)) ;
#2702 = EDGE_LOOP('',(#10566,#10567,#10568,#10569)) ;
#2703 = EDGE_LOOP('',(#10570,#10571,#10572,#10573)) ;
#2704 = EDGE_LOOP('',(#10574,#10575,#10576,#10577)) ;
#2705 = EDGE_LOOP('',(#10578,#10579,#10580,#10581)) ;
#2706 = EDGE_LOOP('',(#10582,#10583,#10584,#10585)) ;
#2707 = EDGE_LOOP('',(#10586,#10587,#10588,#10589,#10590)) ;
#2708 = EDGE_LOOP('',(#10591,#10592,#10593,#10594)) ;
#2709 = EDGE_LOOP('',(#10595,#10596,#10597,#10598)) ;
#2710 = EDGE_LOOP('',(#10599,#10600,#10601,#10602)) ;
#2711 = EDGE_LOOP('',(#10603,#10604,#10605,#10606)) ;
#2712 = EDGE_LOOP('',(#10607,#10608,#10609,#10610)) ;
#2713 = EDGE_LOOP('',(#10611,#10612,#10613,#10614)) ;
#2714 = EDGE_LOOP('',(#10615,#10616,#10617,#10618)) ;
#2715 = EDGE_LOOP('',(#10619,#10620,#10621,#10622)) ;
#2716 = EDGE_LOOP('',(#10623,#10624,#10625,#10626)) ;
#2717 = EDGE_LOOP('',(#10627,#10628,#10629,#10630,#10631)) ;
#2718 = EDGE_LOOP('',(#10632,#10633,#10634,#10635)) ;
#2719 = EDGE_LOOP('',(#10636,#10637,#10638,#10639)) ;
#2720 = EDGE_LOOP('',(#10640,#10641,#10642,#10643)) ;
#2721 = EDGE_LOOP('',(#10644,#10645,#10646,#10647)) ;
#2722 = EDGE_LOOP('',(#10648,#10649,#10650,#10651,#10652,#10653)) ;
#2723 = EDGE_LOOP('',(#10654,#10655,#10656,#10657)) ;
#2724 = EDGE_LOOP('',(#10658,#10659,#10660,#10661,#10662)) ;
#2725 = EDGE_LOOP('',(#10663,#10664,#10665,#10666)) ;
#2726 = EDGE_LOOP('',(#10667,#10668,#10669,#10670)) ;
#2727 = EDGE_LOOP('',(#10671,#10672,#10673,#10674)) ;
#2728 = EDGE_LOOP('',(#10675,#10676,#10677,#10678)) ;
#2729 = EDGE_LOOP('',(#10679,#10680,#10681)) ;
#2730 = EDGE_LOOP('',(#10682,#10683,#10684,#10685)) ;
#2731 = EDGE_LOOP('',(#10686,#10687,#10688,#10689,#10690)) ;
#2732 = EDGE_LOOP('',(#10691)) ;
#2733 = EDGE_LOOP('',(#10692)) ;
#2734 = EDGE_LOOP('',(#10693,#10694,#10695,#10696,#10697)) ;
#2735 = EDGE_LOOP('',(#10698,#10699,#10700,#10701,#10702)) ;
#2736 = EDGE_LOOP('',(#10703,#10704,#10705,#10706,#10707)) ;
#2737 = EDGE_LOOP('',(#10708,#10709,#10710,#10711,#10712)) ;
#2738 = EDGE_LOOP('',(#10713,#10714,#10715,#10716,#10717)) ;
#2739 = EDGE_LOOP('',(#10718,#10719,#10720,#10721)) ;
#2740 = EDGE_LOOP('',(#10722)) ;
#2741 = EDGE_LOOP('',(#10723)) ;
#2742 = EDGE_LOOP('',(#10724,#10725,#10726,#10727,#10728)) ;
#2743 = EDGE_LOOP('',(#10729,#10730,#10731,#10732,#10733)) ;
#2744 = EDGE_LOOP('',(#10734)) ;
#2745 = EDGE_LOOP('',(#10735)) ;
#2746 = EDGE_LOOP('',(#10736,#10737,#10738,#10739,#10740,#10741)) ;
#2747 = EDGE_LOOP('',(#10742,#10743,#10744,#10745,#10746,#10747)) ;
#2748 = EDGE_LOOP('',(#10748,#10749,#10750,#10751,#10752)) ;
#2749 = EDGE_LOOP('',(#10753,#10754,#10755,#10756,#10757)) ;
#2750 = EDGE_LOOP('',(#10758)) ;
#2751 = EDGE_LOOP('',(#10759)) ;
#2752 = EDGE_LOOP('',(#10760,#10761,#10762,#10763,#10764)) ;
#2753 = EDGE_LOOP('',(#10765,#10766,#10767,#10768,#10769)) ;
#2754 = EDGE_LOOP('',(#10770,#10771,#10772,#10773)) ;
#2755 = EDGE_LOOP('',(#10774)) ;
#2756 = EDGE_LOOP('',(#10775,#10776,#10777,#10778,#10779)) ;
#2757 = EDGE_LOOP('',(#10780,#10781,#10782,#10783,#10784,#10785)) ;
#2758 = EDGE_LOOP('',(#10786)) ;
#2759 = EDGE_LOOP('',(#10787)) ;
#2760 = EDGE_LOOP('',(#10788)) ;
#2761 = EDGE_LOOP('',(#10789)) ;
#2762 = EDGE_LOOP('',(#10790)) ;
#2763 = EDGE_LOOP('',(#10791,#10792,#10793,#10794,#10795)) ;
#2764 = EDGE_LOOP('',(#10796)) ;
#2765 = EDGE_LOOP('',(#10797)) ;
#2766 = EDGE_LOOP('',(#10798,#10799,#10800,#10801)) ;
#2767 = EDGE_LOOP('',(#10802)) ;
#2768 = EDGE_LOOP('',(#10803,#10804,#10805,#10806)) ;
#2769 = EDGE_LOOP('',(#10807)) ;
#2770 = EDGE_LOOP('',(#10808,#10809,#10810,#10811)) ;
#2771 = EDGE_LOOP('',(#10812)) ;
#2772 = EDGE_LOOP('',(#10813,#10814,#10815,#10816,#10817,#10818,#10819,#10820,
#10821,#10822,#10823,#10824,#10825,#10826,#10827,#10828,#10829,#10830,#10831,
#10832,#10833,#10834,#10835,#10836,#10837,#10838,#10839,#10840,#10841,#10842,
#10843,#10844)) ;
#2773 = EDGE_LOOP('',(#10845,#10846,#10847,#10848,#10849,#10850,#10851,#10852,
#10853,#10854,#10855,#10856,#10857,#10858,#10859,#10860,#10861,#10862,#10863,
#10864,#10865,#10866,#10867,#10868,#10869,#10870,#10871,#10872,#10873,#10874,
#10875,#10876,#10877,#10878)) ;
#2774 = EDGE_LOOP('',(#10879,#10880,#10881,#10882,#10883)) ;
#2775 = EDGE_LOOP('',(#10884)) ;
#2776 = EDGE_LOOP('',(#10885,#10886,#10887,#10888,#10889,#10890,#10891,#10892,
#10893,#10894,#10895,#10896,#10897,#10898,#10899,#10900,#10901)) ;
#2777 = EDGE_LOOP('',(#10902,#10903,#10904,#10905,#10906,#10907,#10908,#10909,
#10910,#10911,#10912,#10913,#10914,#10915,#10916,#10917,#10918)) ;
#2778 = EDGE_LOOP('',(#10919,#10920,#10921,#10922,#10923,#10924)) ;
#2779 = EDGE_LOOP('',(#10925)) ;
#2780 = EDGE_LOOP('',(#10926,#10927,#10928,#10929)) ;
#2781 = EDGE_LOOP('',(#10930,#10931,#10932,#10933)) ;
#2782 = EDGE_LOOP('',(#10934,#10935,#10936,#10937)) ;
#2783 = EDGE_LOOP('',(#10938,#10939,#10940,#10941)) ;
#2784 = EDGE_LOOP('',(#10942,#10943,#10944,#10945)) ;
#2785 = EDGE_LOOP('',(#10946,#10947,#10948,#10949)) ;
#2786 = EDGE_LOOP('',(#10950)) ;
#2787 = EDGE_LOOP('',(#10951)) ;
#2788 = EDGE_LOOP('',(#10952,#10953,#10954,#10955)) ;
#2789 = EDGE_LOOP('',(#10956,#10957,#10958,#10959)) ;
#2790 = EDGE_LOOP('',(#10960,#10961,#10962,#10963)) ;
#2791 = EDGE_LOOP('',(#10964)) ;
#2792 = EDGE_LOOP('',(#10965)) ;
#2793 = EDGE_LOOP('',(#10966,#10967,#10968,#10969)) ;
#2794 = EDGE_LOOP('',(#10970)) ;
#2795 = EDGE_LOOP('',(#10971)) ;
#2796 = EDGE_LOOP('',(#10972,#10973,#10974,#10975)) ;
#2797 = EDGE_LOOP('',(#10976,#10977,#10978,#10979,#10980)) ;
#2798 = EDGE_LOOP('',(#10981)) ;
#2799 = EDGE_LOOP('',(#10982,#10983,#10984,#10985,#10986,#10987,#10988,#10989)) ;
#2800 = EDGE_LOOP('',(#10990,#10991,#10992,#10993)) ;
#2801 = EDGE_LOOP('',(#10994,#10995,#10996,#10997,#10998,#10999,#11000,#11001)) ;
#2802 = EDGE_LOOP('',(#11002,#11003,#11004,#11005)) ;
#2803 = EDGE_LOOP('',(#11006,#11007,#11008,#11009)) ;
#2804 = EDGE_LOOP('',(#11010,#11011,#11012,#11013)) ;
#2805 = EDGE_LOOP('',(#11014,#11015,#11016,#11017)) ;
#2806 = EDGE_LOOP('',(#11018,#11019,#11020,#11021)) ;
#2807 = EDGE_LOOP('',(#11022,#11023,#11024,#11025)) ;
#2808 = EDGE_LOOP('',(#11026,#11027,#11028,#11029)) ;
#2809 = EDGE_LOOP('',(#11030,#11031,#11032,#11033)) ;
#2810 = EDGE_LOOP('',(#11034)) ;
#2811 = EDGE_LOOP('',(#11035)) ;
#2812 = EDGE_LOOP('',(#11036,#11037,#11038,#11039)) ;
#2813 = EDGE_LOOP('',(#11040,#11041,#11042,#11043)) ;
#2814 = EDGE_LOOP('',(#11044,#11045,#11046,#11047)) ;
#2815 = EDGE_LOOP('',(#11048,#11049,#11050,#11051)) ;
#2816 = EDGE_LOOP('',(#11052)) ;
#2817 = EDGE_LOOP('',(#11053)) ;
#2818 = EDGE_LOOP('',(#11054,#11055,#11056,#11057)) ;
#2819 = EDGE_LOOP('',(#11058,#11059,#11060,#11061)) ;
#2820 = EDGE_LOOP('',(#11062,#11063,#11064,#11065)) ;
#2821 = EDGE_LOOP('',(#11066,#11067,#11068,#11069)) ;
#2822 = EDGE_LOOP('',(#11070)) ;
#2823 = EDGE_LOOP('',(#11071,#11072,#11073,#11074)) ;
#2824 = EDGE_LOOP('',(#11075,#11076,#11077,#11078)) ;
#2825 = EDGE_LOOP('',(#11079,#11080,#11081,#11082)) ;
#2826 = EDGE_LOOP('',(#11083,#11084,#11085,#11086)) ;
#2827 = EDGE_LOOP('',(#11087,#11088,#11089,#11090)) ;
#2828 = EDGE_LOOP('',(#11091,#11092,#11093,#11094)) ;
#2829 = EDGE_LOOP('',(#11095,#11096,#11097,#11098)) ;
#2830 = EDGE_LOOP('',(#11099,#11100,#11101,#11102)) ;
#2831 = EDGE_LOOP('',(#11103,#11104,#11105,#11106)) ;
#2832 = EDGE_LOOP('',(#11107,#11108,#11109,#11110)) ;
#2833 = EDGE_LOOP('',(#11111,#11112,#11113,#11114)) ;
#2834 = EDGE_LOOP('',(#11115,#11116,#11117,#11118)) ;
#2835 = EDGE_LOOP('',(#11119,#11120,#11121,#11122)) ;
#2836 = EDGE_LOOP('',(#11123,#11124,#11125,#11126)) ;
#2837 = EDGE_LOOP('',(#11127,#11128,#11129,#11130)) ;
#2838 = EDGE_LOOP('',(#11131,#11132,#11133,#11134)) ;
#2839 = EDGE_LOOP('',(#11135,#11136,#11137,#11138)) ;
#2840 = EDGE_LOOP('',(#11139,#11140,#11141,#11142)) ;
#2841 = EDGE_LOOP('',(#11143,#11144,#11145,#11146)) ;
#2842 = EDGE_LOOP('',(#11147,#11148,#11149,#11150)) ;
#2843 = EDGE_LOOP('',(#11151,#11152,#11153,#11154)) ;
#2844 = EDGE_LOOP('',(#11155,#11156,#11157,#11158)) ;
#2845 = EDGE_LOOP('',(#11159,#11160,#11161,#11162)) ;
#2846 = EDGE_LOOP('',(#11163,#11164,#11165,#11166)) ;
#2847 = EDGE_LOOP('',(#11167,#11168,#11169,#11170)) ;
#2848 = EDGE_LOOP('',(#11171,#11172,#11173,#11174)) ;
#2849 = EDGE_LOOP('',(#11175,#11176,#11177,#11178)) ;
#2850 = EDGE_LOOP('',(#11179,#11180,#11181,#11182)) ;
#2851 = EDGE_LOOP('',(#11183,#11184,#11185,#11186)) ;
#2852 = EDGE_LOOP('',(#11187,#11188,#11189,#11190)) ;
#2853 = EDGE_LOOP('',(#11191,#11192,#11193,#11194)) ;
#2854 = EDGE_LOOP('',(#11195,#11196,#11197,#11198)) ;
#2855 = EDGE_LOOP('',(#11199,#11200,#11201,#11202)) ;
#2856 = EDGE_LOOP('',(#11203,#11204,#11205,#11206)) ;
#2857 = EDGE_LOOP('',(#11207,#11208,#11209,#11210)) ;
#2858 = EDGE_LOOP('',(#11211,#11212,#11213,#11214)) ;
#2859 = EDGE_LOOP('',(#11215,#11216,#11217,#11218)) ;
#2860 = EDGE_LOOP('',(#11219,#11220,#11221,#11222)) ;
#2861 = EDGE_LOOP('',(#11223,#11224,#11225,#11226)) ;
#2862 = EDGE_LOOP('',(#11227,#11228,#11229,#11230)) ;
#2863 = EDGE_LOOP('',(#11231,#11232,#11233,#11234)) ;
#2864 = EDGE_LOOP('',(#11235,#11236,#11237,#11238)) ;
#2865 = EDGE_LOOP('',(#11239,#11240,#11241,#11242)) ;
#2866 = EDGE_LOOP('',(#11243,#11244,#11245,#11246)) ;
#2867 = EDGE_LOOP('',(#11247,#11248,#11249,#11250)) ;
#2868 = EDGE_LOOP('',(#11251,#11252,#11253,#11254)) ;
#2869 = EDGE_LOOP('',(#11255,#11256,#11257,#11258)) ;
#2870 = EDGE_LOOP('',(#11259,#11260,#11261,#11262)) ;
#2871 = EDGE_LOOP('',(#11263,#11264,#11265,#11266)) ;
#2872 = EDGE_LOOP('',(#11267,#11268,#11269,#11270)) ;
#2873 = EDGE_LOOP('',(#11271,#11272,#11273,#11274)) ;
#2874 = EDGE_LOOP('',(#11275,#11276,#11277,#11278)) ;
#2875 = EDGE_LOOP('',(#11279,#11280,#11281,#11282)) ;
#2876 = EDGE_LOOP('',(#11283,#11284,#11285,#11286)) ;
#2877 = EDGE_LOOP('',(#11287,#11288,#11289,#11290)) ;
#2878 = EDGE_LOOP('',(#11291,#11292,#11293,#11294)) ;
#2879 = EDGE_LOOP('',(#11295,#11296,#11297,#11298)) ;
#2880 = EDGE_LOOP('',(#11299,#11300,#11301,#11302)) ;
#2881 = EDGE_LOOP('',(#11303,#11304,#11305,#11306)) ;
#2882 = EDGE_LOOP('',(#11307,#11308,#11309,#11310)) ;
#2883 = EDGE_LOOP('',(#11311,#11312,#11313,#11314)) ;
#2884 = EDGE_LOOP('',(#11315,#11316,#11317,#11318)) ;
#2885 = EDGE_LOOP('',(#11319)) ;
#2886 = EDGE_LOOP('',(#11320)) ;
#2887 = EDGE_LOOP('',(#11321,#11322,#11323,#11324,#11325)) ;
#2888 = EDGE_LOOP('',(#11326,#11327,#11328,#11329,#11330,#11331)) ;
#2889 = EDGE_LOOP('',(#11332,#11333,#11334,#11335,#11336,#11337,#11338,#11339,
#11340,#11341,#11342,#11343,#11344,#11345,#11346,#11347,#11348,#11349,#11350,
#11351,#11352,#11353,#11354,#11355,#11356,#11357,#11358,#11359,#11360,#11361,
#11362,#11363,#11364,#11365,#11366,#11367,#11368,#11369,#11370,#11371,#11372,
#11373,#11374,#11375,#11376,#11377,#11378,#11379,#11380,#11381,#11382,#11383,
#11384,#11385,#11386,#11387,#11388,#11389,#11390,#11391,#11392,#11393,#11394,
#11395,#11396,#11397,#11398,#11399,#11400,#11401,#11402,#11403,#11404,#11405,
#11406,#11407,#11408,#11409,#11410,#11411,#11412,#11413,#11414,#11415,#11416,
#11417,#11418,#11419,#11420,#11421,#11422,#11423,#11424,#11425,#11426,#11427,
#11428,#11429,#11430,#11431,#11432,#11433,#11434,#11435,#11436,#11437,#11438,
#11439,#11440,#11441,#11442,#11443,#11444,#11445,#11446,#11447,#11448,#11449,
#11450,#11451,#11452,#11453,#11454,#11455,#11456)) ;
#2890 = EDGE_LOOP('',(#11457,#11458,#11459,#11460,#11461,#11462,#11463,#11464,
#11465,#11466,#11467,#11468,#11469,#11470,#11471,#11472,#11473,#11474,#11475,
#11476,#11477,#11478,#11479,#11480,#11481,#11482,#11483,#11484,#11485,#11486,
#11487,#11488,#11489,#11490,#11491,#11492,#11493,#11494,#11495,#11496,#11497,
#11498,#11499,#11500,#11501,#11502,#11503,#11504,#11505,#11506,#11507,#11508,
#11509,#11510,#11511,#11512,#11513,#11514,#11515,#11516,#11517,#11518,#11519,
#11520,#11521,#11522,#11523,#11524,#11525,#11526,#11527,#11528,#11529,#11530,
#11531,#11532,#11533,#11534,#11535,#11536,#11537,#11538,#11539,#11540,#11541,
#11542,#11543,#11544,#11545,#11546,#11547,#11548,#11549,#11550,#11551,#11552,
#11553,#11554,#11555,#11556,#11557,#11558,#11559,#11560,#11561,#11562,#11563,
#11564,#11565,#11566,#11567,#11568,#11569,#11570,#11571,#11572,#11573,#11574,
#11575,#11576,#11577,#11578,#11579,#11580,#11581)) ;
#2891 = EDGE_LOOP('',(#11582,#11583,#11584,#11585,#11586,#11587)) ;
#2892 = EDGE_LOOP('',(#11588,#11589,#11590,#11591,#11592)) ;
#2893 = EDGE_LOOP('',(#11593)) ;
#2894 = EDGE_LOOP('',(#11594)) ;
#2895 = EDGE_LOOP('',(#11595,#11596,#11597,#11598)) ;
#2896 = EDGE_LOOP('',(#11599)) ;
#2897 = EDGE_LOOP('',(#11600)) ;
#2898 = EDGE_LOOP('',(#11601,#11602,#11603,#11604)) ;
#2899 = EDGE_LOOP('',(#11605)) ;
#2900 = EDGE_LOOP('',(#11606,#11607,#11608,#11609)) ;
#2901 = EDGE_LOOP('',(#11610,#11611,#11612,#11613)) ;
#2902 = EDGE_LOOP('',(#11614,#11615,#11616,#11617)) ;
#2903 = EDGE_LOOP('',(#11618,#11619,#11620,#11621)) ;
#2904 = EDGE_LOOP('',(#11622,#11623,#11624,#11625)) ;
#2905 = EDGE_LOOP('',(#11626,#11627,#11628,#11629)) ;
#2906 = EDGE_LOOP('',(#11630,#11631,#11632,#11633)) ;
#2907 = EDGE_LOOP('',(#11634,#11635,#11636,#11637)) ;
#2908 = EDGE_LOOP('',(#11638,#11639,#11640,#11641)) ;
#2909 = EDGE_LOOP('',(#11642,#11643,#11644,#11645)) ;
#2910 = EDGE_LOOP('',(#11646,#11647,#11648,#11649)) ;
#2911 = EDGE_LOOP('',(#11650,#11651,#11652,#11653)) ;
#2912 = EDGE_LOOP('',(#11654,#11655,#11656,#11657)) ;
#2913 = EDGE_LOOP('',(#11658,#11659,#11660,#11661)) ;
#2914 = EDGE_LOOP('',(#11662,#11663,#11664,#11665)) ;
#2915 = EDGE_LOOP('',(#11666,#11667,#11668,#11669)) ;
#2916 = EDGE_LOOP('',(#11670,#11671,#11672,#11673)) ;
#2917 = EDGE_LOOP('',(#11674,#11675,#11676,#11677)) ;
#2918 = EDGE_LOOP('',(#11678,#11679,#11680,#11681)) ;
#2919 = EDGE_LOOP('',(#11682,#11683,#11684,#11685)) ;
#2920 = EDGE_LOOP('',(#11686,#11687,#11688,#11689)) ;
#2921 = EDGE_LOOP('',(#11690,#11691,#11692,#11693)) ;
#2922 = EDGE_LOOP('',(#11694,#11695,#11696,#11697)) ;
#2923 = EDGE_LOOP('',(#11698,#11699,#11700,#11701)) ;
#2924 = EDGE_LOOP('',(#11702,#11703,#11704,#11705)) ;
#2925 = EDGE_LOOP('',(#11706,#11707,#11708,#11709)) ;
#2926 = EDGE_LOOP('',(#11710,#11711,#11712,#11713)) ;
#2927 = EDGE_LOOP('',(#11714,#11715,#11716,#11717)) ;
#2928 = EDGE_LOOP('',(#11718,#11719,#11720,#11721)) ;
#2929 = EDGE_LOOP('',(#11722,#11723,#11724,#11725)) ;
#2930 = EDGE_LOOP('',(#11726,#11727,#11728,#11729)) ;
#2931 = EDGE_LOOP('',(#11730,#11731,#11732,#11733)) ;
#2932 = EDGE_LOOP('',(#11734,#11735,#11736,#11737)) ;
#2933 = EDGE_LOOP('',(#11738,#11739,#11740,#11741)) ;
#2934 = EDGE_LOOP('',(#11742,#11743,#11744,#11745)) ;
#2935 = EDGE_LOOP('',(#11746,#11747,#11748,#11749)) ;
#2936 = EDGE_LOOP('',(#11750,#11751,#11752,#11753)) ;
#2937 = EDGE_LOOP('',(#11754,#11755,#11756,#11757)) ;
#2938 = EDGE_LOOP('',(#11758,#11759,#11760,#11761)) ;
#2939 = EDGE_LOOP('',(#11762,#11763,#11764,#11765)) ;
#2940 = EDGE_LOOP('',(#11766,#11767,#11768,#11769)) ;
#2941 = EDGE_LOOP('',(#11770,#11771,#11772,#11773)) ;
#2942 = EDGE_LOOP('',(#11774,#11775,#11776,#11777)) ;
#2943 = EDGE_LOOP('',(#11778,#11779,#11780,#11781)) ;
#2944 = EDGE_LOOP('',(#11782,#11783,#11784,#11785)) ;
#2945 = EDGE_LOOP('',(#11786,#11787,#11788,#11789)) ;
#2946 = EDGE_LOOP('',(#11790,#11791,#11792,#11793)) ;
#2947 = EDGE_LOOP('',(#11794,#11795,#11796,#11797)) ;
#2948 = EDGE_LOOP('',(#11798,#11799,#11800,#11801)) ;
#2949 = EDGE_LOOP('',(#11802,#11803,#11804,#11805)) ;
#2950 = EDGE_LOOP('',(#11806,#11807,#11808,#11809)) ;
#2951 = EDGE_LOOP('',(#11810,#11811,#11812,#11813)) ;
#2952 = EDGE_LOOP('',(#11814,#11815,#11816,#11817)) ;
#2953 = EDGE_LOOP('',(#11818,#11819,#11820,#11821)) ;
#2954 = EDGE_LOOP('',(#11822,#11823,#11824,#11825)) ;
#2955 = EDGE_LOOP('',(#11826,#11827,#11828,#11829)) ;
#2956 = EDGE_LOOP('',(#11830,#11831,#11832,#11833)) ;
#2957 = EDGE_LOOP('',(#11834,#11835,#11836,#11837)) ;
#2958 = EDGE_LOOP('',(#11838,#11839,#11840,#11841)) ;
#2959 = EDGE_LOOP('',(#11842,#11843,#11844,#11845)) ;
#2960 = EDGE_LOOP('',(#11846,#11847,#11848,#11849)) ;
#2961 = EDGE_LOOP('',(#11850,#11851,#11852,#11853)) ;
#2962 = EDGE_LOOP('',(#11854,#11855,#11856,#11857)) ;
#2963 = EDGE_LOOP('',(#11858,#11859,#11860,#11861)) ;
#2964 = EDGE_LOOP('',(#11862,#11863,#11864,#11865)) ;
#2965 = EDGE_LOOP('',(#11866,#11867,#11868,#11869)) ;
#2966 = EDGE_LOOP('',(#11870,#11871,#11872,#11873)) ;
#2967 = EDGE_LOOP('',(#11874,#11875,#11876,#11877)) ;
#2968 = EDGE_LOOP('',(#11878,#11879,#11880,#11881)) ;
#2969 = EDGE_LOOP('',(#11882,#11883,#11884,#11885)) ;
#2970 = EDGE_LOOP('',(#11886,#11887,#11888,#11889)) ;
#2971 = EDGE_LOOP('',(#11890,#11891,#11892,#11893)) ;
#2972 = EDGE_LOOP('',(#11894,#11895,#11896,#11897)) ;
#2973 = EDGE_LOOP('',(#11898,#11899,#11900,#11901)) ;
#2974 = EDGE_LOOP('',(#11902,#11903,#11904,#11905)) ;
#2975 = EDGE_LOOP('',(#11906,#11907,#11908,#11909)) ;
#2976 = EDGE_LOOP('',(#11910,#11911,#11912,#11913)) ;
#2977 = EDGE_LOOP('',(#11914,#11915,#11916,#11917)) ;
#2978 = EDGE_LOOP('',(#11918,#11919,#11920,#11921)) ;
#2979 = EDGE_LOOP('',(#11922,#11923,#11924,#11925)) ;
#2980 = EDGE_LOOP('',(#11926,#11927,#11928,#11929)) ;
#2981 = EDGE_LOOP('',(#11930,#11931,#11932,#11933,#11934)) ;
#2982 = EDGE_LOOP('',(#11935,#11936,#11937,#11938)) ;
#2983 = EDGE_LOOP('',(#11939,#11940,#11941,#11942)) ;
#2984 = EDGE_LOOP('',(#11943,#11944,#11945,#11946)) ;
#2985 = EDGE_LOOP('',(#11947,#11948,#11949,#11950)) ;
#2986 = EDGE_LOOP('',(#11951,#11952,#11953,#11954)) ;
#2987 = EDGE_LOOP('',(#11955,#11956,#11957,#11958)) ;
#2988 = EDGE_LOOP('',(#11959,#11960,#11961,#11962)) ;
#2989 = EDGE_LOOP('',(#11963,#11964,#11965,#11966)) ;
#2990 = EDGE_LOOP('',(#11967,#11968,#11969,#11970)) ;
#2991 = EDGE_LOOP('',(#11971,#11972,#11973,#11974)) ;
#2992 = EDGE_LOOP('',(#11975,#11976,#11977,#11978)) ;
#2993 = EDGE_LOOP('',(#11979,#11980,#11981,#11982)) ;
#2994 = EDGE_LOOP('',(#11983,#11984,#11985,#11986)) ;
#2995 = EDGE_LOOP('',(#11987,#11988,#11989,#11990)) ;
#2996 = EDGE_LOOP('',(#11991,#11992,#11993,#11994)) ;
#2997 = EDGE_LOOP('',(#11995,#11996,#11997,#11998)) ;
#2998 = EDGE_LOOP('',(#11999,#12000,#12001,#12002)) ;
#2999 = EDGE_LOOP('',(#12003,#12004,#12005,#12006)) ;
#3000 = EDGE_LOOP('',(#12007,#12008,#12009,#12010)) ;
#3001 = EDGE_LOOP('',(#12011,#12012,#12013,#12014)) ;
#3002 = EDGE_LOOP('',(#12015,#12016,#12017,#12018)) ;
#3003 = EDGE_LOOP('',(#12019,#12020,#12021,#12022)) ;
#3004 = EDGE_LOOP('',(#12023,#12024,#12025,#12026)) ;
#3005 = EDGE_LOOP('',(#12027,#12028,#12029,#12030)) ;
#3006 = EDGE_LOOP('',(#12031,#12032,#12033,#12034)) ;
#3007 = EDGE_LOOP('',(#12035,#12036,#12037,#12038)) ;
#3008 = EDGE_LOOP('',(#12039,#12040,#12041,#12042)) ;
#3009 = EDGE_LOOP('',(#12043,#12044,#12045,#12046)) ;
#3010 = EDGE_LOOP('',(#12047,#12048,#12049,#12050)) ;
#3011 = EDGE_LOOP('',(#12051,#12052,#12053,#12054)) ;
#3012 = EDGE_LOOP('',(#12055,#12056,#12057,#12058)) ;
#3013 = EDGE_LOOP('',(#12059,#12060,#12061,#12062)) ;
#3014 = EDGE_LOOP('',(#12063,#12064,#12065,#12066)) ;
#3015 = EDGE_LOOP('',(#12067,#12068,#12069,#12070)) ;
#3016 = EDGE_LOOP('',(#12071,#12072,#12073,#12074)) ;
#3017 = EDGE_LOOP('',(#12075,#12076,#12077,#12078)) ;
#3018 = EDGE_LOOP('',(#12079,#12080,#12081,#12082)) ;
#3019 = EDGE_LOOP('',(#12083,#12084,#12085,#12086)) ;
#3020 = EDGE_LOOP('',(#12087,#12088,#12089,#12090)) ;
#3021 = EDGE_LOOP('',(#12091,#12092,#12093,#12094)) ;
#3022 = EDGE_LOOP('',(#12095,#12096,#12097,#12098)) ;
#3023 = EDGE_LOOP('',(#12099,#12100,#12101,#12102)) ;
#3024 = EDGE_LOOP('',(#12103,#12104,#12105,#12106)) ;
#3025 = EDGE_LOOP('',(#12107,#12108,#12109,#12110)) ;
#3026 = EDGE_LOOP('',(#12111,#12112,#12113,#12114)) ;
#3027 = EDGE_LOOP('',(#12115,#12116,#12117,#12118)) ;
#3028 = EDGE_LOOP('',(#12119,#12120,#12121,#12122)) ;
#3029 = EDGE_LOOP('',(#12123,#12124,#12125,#12126)) ;
#3030 = EDGE_LOOP('',(#12127,#12128,#12129,#12130)) ;
#3031 = EDGE_LOOP('',(#12131,#12132,#12133,#12134)) ;
#3032 = EDGE_LOOP('',(#12135,#12136,#12137,#12138)) ;
#3033 = EDGE_LOOP('',(#12139,#12140,#12141,#12142)) ;
#3034 = EDGE_LOOP('',(#12143,#12144,#12145,#12146)) ;
#3035 = EDGE_LOOP('',(#12147,#12148,#12149,#12150)) ;
#3036 = EDGE_LOOP('',(#12151,#12152,#12153,#12154)) ;
#3037 = EDGE_LOOP('',(#12155,#12156,#12157,#12158)) ;
#3038 = EDGE_LOOP('',(#12159,#12160,#12161,#12162)) ;
#3039 = EDGE_LOOP('',(#12163,#12164,#12165,#12166)) ;
#3040 = EDGE_LOOP('',(#12167,#12168,#12169,#12170)) ;
#3041 = EDGE_LOOP('',(#12171,#12172,#12173,#12174)) ;
#3042 = EDGE_LOOP('',(#12175,#12176,#12177,#12178)) ;
#3043 = EDGE_LOOP('',(#12179,#12180,#12181,#12182)) ;
#3044 = EDGE_LOOP('',(#12183,#12184,#12185,#12186)) ;
#3045 = EDGE_LOOP('',(#12187,#12188,#12189,#12190)) ;
#3046 = EDGE_LOOP('',(#12191,#12192,#12193,#12194)) ;
#3047 = EDGE_LOOP('',(#12195,#12196,#12197,#12198)) ;
#3048 = EDGE_LOOP('',(#12199,#12200,#12201,#12202)) ;
#3049 = EDGE_LOOP('',(#12203,#12204,#12205,#12206)) ;
#3050 = EDGE_LOOP('',(#12207,#12208,#12209,#12210)) ;
#3051 = EDGE_LOOP('',(#12211,#12212,#12213,#12214)) ;
#3052 = EDGE_LOOP('',(#12215,#12216,#12217,#12218)) ;
#3053 = EDGE_LOOP('',(#12219,#12220,#12221,#12222)) ;
#3054 = EDGE_LOOP('',(#12223,#12224,#12225,#12226)) ;
#3055 = EDGE_LOOP('',(#12227,#12228,#12229,#12230)) ;
#3056 = EDGE_LOOP('',(#12231,#12232,#12233,#12234)) ;
#3057 = EDGE_LOOP('',(#12235,#12236,#12237,#12238)) ;
#3058 = EDGE_LOOP('',(#12239,#12240,#12241,#12242)) ;
#3059 = EDGE_LOOP('',(#12243,#12244,#12245,#12246)) ;
#3060 = EDGE_LOOP('',(#12247,#12248,#12249,#12250)) ;
#3061 = EDGE_LOOP('',(#12251,#12252,#12253,#12254)) ;
#3062 = EDGE_LOOP('',(#12255,#12256,#12257,#12258)) ;
#3063 = EDGE_LOOP('',(#12259,#12260,#12261,#12262)) ;
#3064 = EDGE_LOOP('',(#12263,#12264,#12265,#12266)) ;
#3065 = EDGE_LOOP('',(#12267,#12268,#12269,#12270)) ;
#3066 = EDGE_LOOP('',(#12271,#12272,#12273,#12274)) ;
#3067 = EDGE_LOOP('',(#12275,#12276,#12277,#12278)) ;
#3068 = EDGE_LOOP('',(#12279,#12280,#12281,#12282)) ;
#3069 = EDGE_LOOP('',(#12283,#12284,#12285,#12286)) ;
#3070 = EDGE_LOOP('',(#12287,#12288,#12289,#12290)) ;
#3071 = EDGE_LOOP('',(#12291,#12292,#12293,#12294)) ;
#3072 = EDGE_LOOP('',(#12295,#12296,#12297,#12298)) ;
#3073 = EDGE_LOOP('',(#12299,#12300,#12301,#12302)) ;
#3074 = EDGE_LOOP('',(#12303,#12304,#12305,#12306)) ;
#3075 = EDGE_LOOP('',(#12307,#12308,#12309,#12310)) ;
#3076 = EDGE_LOOP('',(#12311,#12312,#12313,#12314)) ;
#3077 = EDGE_LOOP('',(#12315,#12316,#12317,#12318)) ;
#3078 = EDGE_LOOP('',(#12319,#12320,#12321,#12322)) ;
#3079 = EDGE_LOOP('',(#12323,#12324,#12325,#12326)) ;
#3080 = EDGE_LOOP('',(#12327,#12328,#12329,#12330)) ;
#3081 = EDGE_LOOP('',(#12331,#12332,#12333,#12334)) ;
#3082 = EDGE_LOOP('',(#12335,#12336,#12337,#12338)) ;
#3083 = EDGE_LOOP('',(#12339,#12340,#12341,#12342)) ;
#3084 = EDGE_LOOP('',(#12343,#12344,#12345,#12346)) ;
#3085 = EDGE_LOOP('',(#12347,#12348,#12349,#12350)) ;
#3086 = EDGE_LOOP('',(#12351,#12352,#12353,#12354)) ;
#3087 = EDGE_LOOP('',(#12355,#12356,#12357,#12358)) ;
#3088 = EDGE_LOOP('',(#12359,#12360,#12361,#12362)) ;
#3089 = EDGE_LOOP('',(#12363,#12364,#12365,#12366)) ;
#3090 = EDGE_LOOP('',(#12367,#12368,#12369,#12370)) ;
#3091 = EDGE_LOOP('',(#12371,#12372,#12373,#12374)) ;
#3092 = EDGE_LOOP('',(#12375,#12376,#12377,#12378)) ;
#3093 = EDGE_LOOP('',(#12379,#12380,#12381,#12382)) ;
#3094 = EDGE_LOOP('',(#12383,#12384,#12385,#12386)) ;
#3095 = EDGE_LOOP('',(#12387,#12388,#12389,#12390)) ;
#3096 = EDGE_LOOP('',(#12391,#12392,#12393,#12394)) ;
#3097 = EDGE_LOOP('',(#12395,#12396,#12397,#12398)) ;
#3098 = EDGE_LOOP('',(#12399,#12400,#12401,#12402)) ;
#3099 = EDGE_LOOP('',(#12403,#12404,#12405,#12406)) ;
#3100 = EDGE_LOOP('',(#12407,#12408,#12409,#12410)) ;
#3101 = EDGE_LOOP('',(#12411,#12412,#12413,#12414)) ;
#3102 = EDGE_LOOP('',(#12415,#12416,#12417,#12418)) ;
#3103 = EDGE_LOOP('',(#12419,#12420,#12421,#12422)) ;
#3104 = EDGE_LOOP('',(#12423,#12424,#12425,#12426)) ;
#3105 = EDGE_LOOP('',(#12427,#12428,#12429,#12430)) ;
#3106 = EDGE_LOOP('',(#12431,#12432,#12433,#12434)) ;
#3107 = EDGE_LOOP('',(#12435,#12436,#12437,#12438)) ;
#3108 = EDGE_LOOP('',(#12439,#12440,#12441,#12442)) ;
#3109 = EDGE_LOOP('',(#12443,#12444,#12445,#12446)) ;
#3110 = EDGE_LOOP('',(#12447,#12448,#12449,#12450)) ;
#3111 = EDGE_LOOP('',(#12451,#12452,#12453,#12454)) ;
#3112 = EDGE_LOOP('',(#12455,#12456,#12457,#12458)) ;
#3113 = EDGE_LOOP('',(#12459,#12460,#12461,#12462)) ;
#3114 = EDGE_LOOP('',(#12463,#12464,#12465,#12466)) ;
#3115 = EDGE_LOOP('',(#12467,#12468,#12469,#12470)) ;
#3116 = EDGE_LOOP('',(#12471,#12472,#12473,#12474)) ;
#3117 = EDGE_LOOP('',(#12475,#12476,#12477,#12478)) ;
#3118 = EDGE_LOOP('',(#12479,#12480,#12481,#12482)) ;
#3119 = EDGE_LOOP('',(#12483,#12484,#12485,#12486)) ;
#3120 = EDGE_LOOP('',(#12487,#12488,#12489,#12490)) ;
#3121 = EDGE_LOOP('',(#12491,#12492,#12493,#12494)) ;
#3122 = EDGE_LOOP('',(#12495,#12496,#12497,#12498)) ;
#3123 = EDGE_LOOP('',(#12499,#12500,#12501,#12502)) ;
#3124 = EDGE_LOOP('',(#12503,#12504,#12505,#12506)) ;
#3125 = EDGE_LOOP('',(#12507,#12508,#12509,#12510)) ;
#3126 = EDGE_LOOP('',(#12511,#12512,#12513,#12514)) ;
#3127 = EDGE_LOOP('',(#12515,#12516,#12517,#12518)) ;
#3128 = EDGE_LOOP('',(#12519,#12520,#12521,#12522)) ;
#3129 = EDGE_LOOP('',(#12523,#12524,#12525,#12526)) ;
#3130 = EDGE_LOOP('',(#12527,#12528,#12529,#12530)) ;
#3131 = EDGE_LOOP('',(#12531,#12532,#12533,#12534)) ;
#3132 = EDGE_LOOP('',(#12535,#12536,#12537,#12538,#12539)) ;
#3133 = EDGE_LOOP('',(#12540,#12541,#12542,#12543)) ;
#3134 = EDGE_LOOP('',(#12544,#12545,#12546,#12547)) ;
#3135 = EDGE_LOOP('',(#12548,#12549,#12550,#12551)) ;
#3136 = EDGE_LOOP('',(#12552,#12553,#12554,#12555)) ;
#3137 = EDGE_LOOP('',(#12556,#12557,#12558,#12559)) ;
#3138 = EDGE_LOOP('',(#12560,#12561,#12562,#12563)) ;
#3139 = EDGE_LOOP('',(#12564,#12565,#12566,#12567)) ;
#3140 = EDGE_LOOP('',(#12568,#12569,#12570,#12571)) ;
#3141 = EDGE_LOOP('',(#12572,#12573,#12574,#12575)) ;
#3142 = EDGE_LOOP('',(#12576,#12577,#12578,#12579)) ;
#3143 = EDGE_LOOP('',(#12580,#12581,#12582,#12583)) ;
#3144 = EDGE_LOOP('',(#12584,#12585,#12586,#12587)) ;
#3145 = EDGE_LOOP('',(#12588,#12589,#12590,#12591)) ;
#3146 = EDGE_LOOP('',(#12592,#12593,#12594,#12595)) ;
#3147 = EDGE_LOOP('',(#12596,#12597,#12598,#12599)) ;
#3148 = EDGE_LOOP('',(#12600,#12601,#12602,#12603)) ;
#3149 = EDGE_LOOP('',(#12604,#12605,#12606,#12607)) ;
#3150 = EDGE_LOOP('',(#12608,#12609,#12610,#12611)) ;
#3151 = EDGE_LOOP('',(#12612,#12613,#12614,#12615)) ;
#3152 = EDGE_LOOP('',(#12616,#12617,#12618,#12619)) ;
#3153 = EDGE_LOOP('',(#12620,#12621,#12622,#12623)) ;
#3154 = EDGE_LOOP('',(#12624,#12625,#12626,#12627)) ;
#3155 = EDGE_LOOP('',(#12628,#12629,#12630,#12631)) ;
#3156 = EDGE_LOOP('',(#12632,#12633,#12634,#12635)) ;
#3157 = EDGE_LOOP('',(#12636,#12637,#12638,#12639)) ;
#3158 = EDGE_LOOP('',(#12640,#12641,#12642,#12643)) ;
#3159 = EDGE_LOOP('',(#12644,#12645,#12646,#12647)) ;
#3160 = EDGE_LOOP('',(#12648,#12649,#12650,#12651)) ;
#3161 = EDGE_LOOP('',(#12652,#12653,#12654,#12655)) ;
#3162 = EDGE_LOOP('',(#12656,#12657,#12658,#12659)) ;
#3163 = EDGE_LOOP('',(#12660,#12661,#12662,#12663)) ;
#3164 = EDGE_LOOP('',(#12664,#12665,#12666,#12667)) ;
#3165 = EDGE_LOOP('',(#12668,#12669,#12670,#12671)) ;
#3166 = EDGE_LOOP('',(#12672,#12673,#12674,#12675)) ;
#3167 = EDGE_LOOP('',(#12676,#12677,#12678,#12679)) ;
#3168 = EDGE_LOOP('',(#12680,#12681,#12682,#12683)) ;
#3169 = EDGE_LOOP('',(#12684,#12685,#12686,#12687)) ;
#3170 = EDGE_LOOP('',(#12688,#12689,#12690,#12691)) ;
#3171 = EDGE_LOOP('',(#12692,#12693,#12694,#12695)) ;
#3172 = EDGE_LOOP('',(#12696,#12697,#12698,#12699)) ;
#3173 = EDGE_LOOP('',(#12700,#12701,#12702,#12703)) ;
#3174 = EDGE_LOOP('',(#12704,#12705,#12706,#12707)) ;
#3175 = EDGE_LOOP('',(#12708,#12709,#12710,#12711)) ;
#3176 = EDGE_LOOP('',(#12712,#12713,#12714,#12715)) ;
#3177 = EDGE_LOOP('',(#12716,#12717,#12718,#12719)) ;
#3178 = EDGE_LOOP('',(#12720,#12721,#12722,#12723)) ;
#3179 = EDGE_LOOP('',(#12724,#12725,#12726,#12727)) ;
#3180 = EDGE_LOOP('',(#12728,#12729,#12730,#12731)) ;
#3181 = EDGE_LOOP('',(#12732,#12733,#12734,#12735)) ;
#3182 = EDGE_LOOP('',(#12736,#12737,#12738,#12739)) ;
#3183 = EDGE_LOOP('',(#12740,#12741,#12742,#12743)) ;
#3184 = EDGE_LOOP('',(#12744,#12745,#12746,#12747)) ;
#3185 = EDGE_LOOP('',(#12748,#12749,#12750,#12751)) ;
#3186 = EDGE_LOOP('',(#12752,#12753,#12754,#12755)) ;
#3187 = EDGE_LOOP('',(#12756,#12757,#12758,#12759)) ;
#3188 = EDGE_LOOP('',(#12760,#12761,#12762,#12763)) ;
#3189 = EDGE_LOOP('',(#12764,#12765,#12766,#12767)) ;
#3190 = EDGE_LOOP('',(#12768,#12769,#12770,#12771)) ;
#3191 = EDGE_LOOP('',(#12772,#12773,#12774,#12775)) ;
#3192 = EDGE_LOOP('',(#12776,#12777,#12778,#12779)) ;
#3193 = EDGE_LOOP('',(#12780,#12781,#12782,#12783)) ;
#3194 = EDGE_LOOP('',(#12784,#12785,#12786,#12787)) ;
#3195 = EDGE_LOOP('',(#12788,#12789,#12790,#12791)) ;
#3196 = EDGE_LOOP('',(#12792,#12793,#12794,#12795)) ;
#3197 = EDGE_LOOP('',(#12796,#12797,#12798,#12799)) ;
#3198 = EDGE_LOOP('',(#12800,#12801,#12802,#12803)) ;
#3199 = EDGE_LOOP('',(#12804,#12805,#12806,#12807)) ;
#3200 = EDGE_LOOP('',(#12808,#12809,#12810,#12811)) ;
#3201 = EDGE_LOOP('',(#12812,#12813,#12814,#12815)) ;
#3202 = EDGE_LOOP('',(#12816,#12817,#12818,#12819,#12820)) ;
#3203 = EDGE_LOOP('',(#12821,#12822,#12823,#12824)) ;
#3204 = EDGE_LOOP('',(#12825)) ;
#3205 = EDGE_LOOP('',(#12826)) ;
#3206 = EDGE_LOOP('',(#12827,#12828,#12829,#12830,#12831)) ;
#3207 = EDGE_LOOP('',(#12832,#12833,#12834,#12835,#12836)) ;
#3208 = EDGE_LOOP('',(#12837,#12838,#12839,#12840)) ;
#3209 = EDGE_LOOP('',(#12841)) ;
#3210 = EDGE_LOOP('',(#12842)) ;
#3211 = EDGE_LOOP('',(#12843,#12844,#12845,#12846,#12847)) ;
#3212 = EDGE_LOOP('',(#12848,#12849,#12850,#12851)) ;
#3213 = EDGE_LOOP('',(#12852,#12853,#12854,#12855)) ;
#3214 = EDGE_LOOP('',(#12856,#12857,#12858,#12859)) ;
#3215 = EDGE_LOOP('',(#12860,#12861,#12862,#12863,#12864,#12865,#12866,#12867,
#12868,#12869,#12870,#12871,#12872,#12873,#12874,#12875)) ;
#3216 = EDGE_LOOP('',(#12876)) ;
#3217 = EDGE_LOOP('',(#12877,#12878,#12879,#12880)) ;
#3218 = EDGE_LOOP('',(#12881,#12882,#12883,#12884)) ;
#3219 = EDGE_LOOP('',(#12885,#12886,#12887,#12888)) ;
#3220 = EDGE_LOOP('',(#12889,#12890,#12891,#12892)) ;
#3221 = EDGE_LOOP('',(#12893,#12894,#12895,#12896)) ;
#3222 = EDGE_LOOP('',(#12897,#12898,#12899,#12900)) ;
#3223 = EDGE_LOOP('',(#12901,#12902,#12903,#12904)) ;
#3224 = EDGE_LOOP('',(#12905,#12906,#12907,#12908)) ;
#3225 = EDGE_LOOP('',(#12909,#12910,#12911,#12912)) ;
#3226 = EDGE_LOOP('',(#12913,#12914,#12915,#12916)) ;
#3227 = EDGE_LOOP('',(#12917,#12918,#12919,#12920)) ;
#3228 = EDGE_LOOP('',(#12921,#12922,#12923,#12924)) ;
#3229 = EDGE_LOOP('',(#12925,#12926,#12927,#12928)) ;
#3230 = EDGE_LOOP('',(#12929,#12930,#12931,#12932)) ;
#3231 = EDGE_LOOP('',(#12933,#12934,#12935,#12936)) ;
#3232 = EDGE_LOOP('',(#12937,#12938,#12939,#12940)) ;
#3233 = EDGE_LOOP('',(#12941,#12942,#12943,#12944)) ;
#3234 = EDGE_LOOP('',(#12945,#12946,#12947,#12948,#12949,#12950,#12951,#12952)) ;
#3235 = EDGE_LOOP('',(#12953)) ;
#3236 = EDGE_LOOP('',(#12954,#12955,#12956,#12957)) ;
#3237 = EDGE_LOOP('',(#12958,#12959,#12960,#12961,#12962,#12963,#12964,#12965,
#12966,#12967,#12968,#12969,#12970,#12971,#12972,#12973,#12974,#12975,#12976,
#12977,#12978,#12979,#12980,#12981,#12982,#12983,#12984,#12985,#12986,#12987,
#12988,#12989,#12990,#12991,#12992,#12993,#12994,#12995,#12996,#12997,#12998,
#12999,#13000,#13001,#13002,#13003,#13004,#13005,#13006,#13007,#13008,#13009,
#13010,#13011,#13012,#13013,#13014,#13015,#13016,#13017,#13018,#13019,#13020,
#13021,#13022,#13023,#13024,#13025,#13026,#13027,#13028,#13029,#13030,#13031,
#13032,#13033,#13034,#13035,#13036,#13037,#13038,#13039,#13040,#13041,#13042,
#13043,#13044,#13045,#13046,#13047,#13048,#13049,#13050,#13051,#13052,#13053,
#13054,#13055,#13056,#13057,#13058,#13059,#13060,#13061,#13062,#13063,#13064,
#13065,#13066,#13067,#13068,#13069,#13070,#13071,#13072,#13073,#13074,#13075,
#13076,#13077,#13078,#13079,#13080,#13081,#13082,#13083,#13084,#13085,#13086,
#13087,#13088,#13089,#13090,#13091,#13092,#13093,#13094,#13095,#13096,#13097,
#13098,#13099,#13100,#13101,#13102,#13103,#13104,#13105,#13106,#13107,#13108,
#13109,#13110,#13111,#13112,#13113,#13114,#13115,#13116,#13117,#13118,#13119,
#13120,#13121,#13122,#13123,#13124,#13125,#13126,#13127,#13128,#13129,#13130,
#13131,#13132,#13133,#13134,#13135)) ;
#3238 = EDGE_LOOP('',(#13136,#13137,#13138,#13139,#13140,#13141,#13142,#13143,
#13144,#13145,#13146,#13147,#13148,#13149,#13150,#13151,#13152,#13153,#13154,
#13155,#13156,#13157,#13158,#13159,#13160,#13161,#13162,#13163,#13164,#13165,
#13166,#13167,#13168,#13169,#13170,#13171,#13172,#13173,#13174,#13175,#13176,
#13177,#13178,#13179,#13180,#13181,#13182,#13183,#13184,#13185,#13186,#13187,
#13188,#13189,#13190,#13191,#13192,#13193,#13194,#13195,#13196,#13197,#13198,
#13199,#13200,#13201,#13202,#13203,#13204,#13205,#13206,#13207,#13208,#13209,
#13210,#13211,#13212,#13213,#13214,#13215,#13216,#13217,#13218,#13219,#13220,
#13221,#13222,#13223,#13224,#13225,#13226,#13227,#13228,#13229,#13230,#13231,
#13232,#13233,#13234,#13235,#13236,#13237,#13238,#13239,#13240,#13241,#13242,
#13243,#13244,#13245,#13246,#13247,#13248,#13249)) ;
#3239 = EDGE_LOOP('',(#13250,#13251,#13252)) ;
#3240 = EDGE_LOOP('',(#13253,#13254,#13255)) ;
#3241 = EDGE_LOOP('',(#13256,#13257,#13258,#13259,#13260,#13261,#13262,#13263,
#13264,#13265,#13266,#13267,#13268,#13269,#13270,#13271,#13272,#13273,#13274,
#13275,#13276,#13277,#13278,#13279,#13280,#13281,#13282,#13283,#13284,#13285,
#13286,#13287,#13288,#13289,#13290,#13291,#13292,#13293,#13294,#13295,#13296,
#13297,#13298,#13299,#13300,#13301,#13302,#13303,#13304,#13305,#13306,#13307,
#13308,#13309,#13310,#13311,#13312,#13313,#13314,#13315,#13316,#13317,#13318,
#13319,#13320,#13321,#13322,#13323,#13324,#13325,#13326,#13327,#13328,#13329,
#13330,#13331,#13332,#13333,#13334,#13335,#13336,#13337,#13338,#13339,#13340,
#13341,#13342,#13343,#13344,#13345,#13346,#13347,#13348,#13349,#13350,#13351,
#13352,#13353,#13354,#13355,#13356,#13357,#13358,#13359,#13360,#13361,#13362,
#13363,#13364,#13365,#13366,#13367,#13368,#13369,#13370,#13371,#13372,#13373,
#13374,#13375,#13376,#13377,#13378,#13379,#13380,#13381,#13382,#13383,#13384,
#13385,#13386,#13387,#13388,#13389,#13390,#13391,#13392,#13393,#13394,#13395,
#13396,#13397,#13398,#13399,#13400,#13401,#13402,#13403,#13404,#13405,#13406,
#13407,#13408,#13409,#13410,#13411,#13412,#13413,#13414,#13415,#13416,#13417,
#13418,#13419,#13420,#13421,#13422,#13423,#13424,#13425,#13426,#13427,#13428,
#13429,#13430,#13431,#13432,#13433)) ;
#3242 = EDGE_LOOP('',(#13434,#13435,#13436,#13437)) ;
#3243 = EDGE_LOOP('',(#13438,#13439,#13440)) ;
#3244 = EDGE_LOOP('',(#13441,#13442,#13443)) ;
#3245 = EDGE_LOOP('',(#13444,#13445,#13446)) ;
#3246 = EDGE_LOOP('',(#13447,#13448,#13449)) ;
#3247 = EDGE_LOOP('',(#13450,#13451,#13452)) ;
#3248 = EDGE_LOOP('',(#13453,#13454,#13455)) ;
#3249 = EDGE_LOOP('',(#13456,#13457,#13458)) ;
#3250 = EDGE_LOOP('',(#13459,#13460,#13461)) ;
#3251 = EDGE_LOOP('',(#13462,#13463,#13464)) ;
#3252 = EDGE_LOOP('',(#13465,#13466,#13467)) ;
#3253 = EDGE_LOOP('',(#13468,#13469,#13470)) ;
#3254 = EDGE_LOOP('',(#13471,#13472,#13473)) ;
#3255 = EDGE_LOOP('',(#13474,#13475,#13476)) ;
#3256 = EDGE_LOOP('',(#13477,#13478,#13479)) ;
#3257 = EDGE_LOOP('',(#13480,#13481,#13482)) ;
#3258 = EDGE_LOOP('',(#13483,#13484,#13485)) ;
#3259 = EDGE_LOOP('',(#13486,#13487,#13488)) ;
#3260 = EDGE_LOOP('',(#13489,#13490,#13491)) ;
#3261 = EDGE_LOOP('',(#13492,#13493,#13494)) ;
#3262 = EDGE_LOOP('',(#13495,#13496,#13497)) ;
#3263 = EDGE_LOOP('',(#13498,#13499,#13500)) ;
#3264 = EDGE_LOOP('',(#13501,#13502,#13503)) ;
#3265 = EDGE_LOOP('',(#13504,#13505,#13506)) ;
#3266 = EDGE_LOOP('',(#13507,#13508,#13509)) ;
#3267 = EDGE_LOOP('',(#13510,#13511,#13512)) ;
#3268 = EDGE_LOOP('',(#13513,#13514,#13515)) ;
#3269 = EDGE_LOOP('',(#13516,#13517,#13518)) ;
#3270 = EDGE_LOOP('',(#13519,#13520,#13521)) ;
#3271 = EDGE_LOOP('',(#13522,#13523,#13524)) ;
#3272 = EDGE_LOOP('',(#13525,#13526,#13527,#13528)) ;
#3273 = EDGE_LOOP('',(#13529,#13530,#13531,#13532)) ;
#3274 = EDGE_LOOP('',(#13533,#13534,#13535,#13536)) ;
#3275 = EDGE_LOOP('',(#13537,#13538,#13539,#13540)) ;
#3276 = EDGE_LOOP('',(#13541,#13542,#13543,#13544)) ;
#3277 = EDGE_LOOP('',(#13545,#13546,#13547,#13548)) ;
#3278 = EDGE_LOOP('',(#13549,#13550,#13551,#13552)) ;
#3279 = EDGE_LOOP('',(#13553)) ;
#3280 = EDGE_LOOP('',(#13554)) ;
#3281 = EDGE_LOOP('',(#13555)) ;
#3282 = EDGE_LOOP('',(#13556)) ;
#3283 = EDGE_LOOP('',(#13557)) ;
#3284 = EDGE_LOOP('',(#13558)) ;
#3285 = EDGE_LOOP('',(#13559,#13560)) ;
#3286 = EDGE_LOOP('',(#13561,#13562)) ;
#3287 = EDGE_LOOP('',(#13563,#13564)) ;
#3288 = EDGE_LOOP('',(#13565,#13566)) ;
#3289 = EDGE_LOOP('',(#13567,#13568)) ;
#3290 = EDGE_LOOP('',(#13569,#13570)) ;
#3291 = EDGE_LOOP('',(#13571,#13572)) ;
#3292 = EDGE_LOOP('',(#13573,#13574)) ;
#3293 = EDGE_LOOP('',(#13575,#13576)) ;
#3294 = EDGE_LOOP('',(#13577,#13578)) ;
#3295 = EDGE_LOOP('',(#13579,#13580)) ;
#3296 = EDGE_LOOP('',(#13581,#13582)) ;
#3297 = EDGE_LOOP('',(#13583,#13584)) ;
#3298 = EDGE_LOOP('',(#13585,#13586)) ;
#3299 = EDGE_LOOP('',(#13587,#13588)) ;
#3300 = EDGE_LOOP('',(#13589,#13590)) ;
#3301 = EDGE_LOOP('',(#13591,#13592)) ;
#3302 = EDGE_LOOP('',(#13593,#13594)) ;
#3303 = EDGE_LOOP('',(#13595,#13596)) ;
#3304 = EDGE_LOOP('',(#13597,#13598)) ;
#3305 = EDGE_LOOP('',(#13599,#13600)) ;
#3306 = EDGE_LOOP('',(#13601,#13602)) ;
#3307 = EDGE_LOOP('',(#13603,#13604)) ;
#3308 = EDGE_LOOP('',(#13605,#13606)) ;
#3309 = EDGE_LOOP('',(#13607,#13608)) ;
#3310 = EDGE_LOOP('',(#13609,#13610)) ;
#3311 = EDGE_LOOP('',(#13611,#13612)) ;
#3312 = EDGE_LOOP('',(#13613,#13614)) ;
#3313 = EDGE_LOOP('',(#13615)) ;
#3314 = EDGE_LOOP('',(#13616)) ;
#3315 = EDGE_LOOP('',(#13617,#13618)) ;
#3316 = EDGE_LOOP('',(#13619,#13620,#13621,#13622,#13623,#13624,#13625,#13626,
#13627,#13628,#13629,#13630,#13631,#13632,#13633,#13634,#13635,#13636,#13637,
#13638,#13639,#13640,#13641,#13642,#13643,#13644,#13645,#13646,#13647,#13648,
#13649,#13650,#13651)) ;
#3317 = EDGE_LOOP('',(#13652,#13653,#13654,#13655,#13656,#13657,#13658)) ;
#3318 = EDGE_LOOP('',(#13659,#13660,#13661,#13662,#13663,#13664,#13665,#13666,
#13667,#13668)) ;
#3319 = EDGE_LOOP('',(#13669,#13670,#13671,#13672,#13673,#13674,#13675)) ;
#3320 = EDGE_LOOP('',(#13676,#13677,#13678,#13679,#13680,#13681,#13682)) ;
#3321 = EDGE_LOOP('',(#13683,#13684,#13685,#13686,#13687,#13688,#13689,#13690,
#13691,#13692)) ;
#3322 = EDGE_LOOP('',(#13693,#13694,#13695,#13696,#13697,#13698,#13699)) ;
#3323 = EDGE_LOOP('',(#13700,#13701,#13702,#13703,#13704,#13705,#13706)) ;
#3324 = EDGE_LOOP('',(#13707,#13708,#13709,#13710,#13711,#13712,#13713,#13714,
#13715,#13716)) ;
#3325 = EDGE_LOOP('',(#13717,#13718,#13719,#13720,#13721,#13722,#13723)) ;
#3326 = EDGE_LOOP('',(#13724,#13725,#13726,#13727,#13728,#13729,#13730)) ;
#3327 = EDGE_LOOP('',(#13731,#13732,#13733,#13734,#13735,#13736,#13737,#13738,
#13739,#13740)) ;
#3328 = EDGE_LOOP('',(#13741,#13742,#13743,#13744,#13745,#13746,#13747)) ;
#3329 = EDGE_LOOP('',(#13748,#13749,#13750,#13751,#13752,#13753,#13754)) ;
#3330 = EDGE_LOOP('',(#13755,#13756,#13757,#13758,#13759,#13760,#13761,#13762,
#13763,#13764)) ;
#3331 = EDGE_LOOP('',(#13765,#13766,#13767,#13768,#13769,#13770,#13771)) ;
#3332 = EDGE_LOOP('',(#13772,#13773,#13774,#13775,#13776,#13777,#13778)) ;
#3333 = EDGE_LOOP('',(#13779,#13780,#13781,#13782,#13783,#13784,#13785,#13786,
#13787,#13788)) ;
#3334 = EDGE_LOOP('',(#13789,#13790,#13791,#13792,#13793,#13794,#13795)) ;
#3335 = EDGE_LOOP('',(#13796,#13797,#13798,#13799,#13800,#13801,#13802)) ;
#3336 = EDGE_LOOP('',(#13803,#13804,#13805,#13806,#13807,#13808,#13809,#13810,
#13811,#13812)) ;
#3337 = EDGE_LOOP('',(#13813,#13814,#13815,#13816,#13817,#13818,#13819)) ;
#3338 = EDGE_LOOP('',(#13820,#13821,#13822,#13823,#13824,#13825,#13826)) ;
#3339 = EDGE_LOOP('',(#13827,#13828,#13829,#13830,#13831,#13832,#13833,#13834,
#13835,#13836)) ;
#3340 = EDGE_LOOP('',(#13837,#13838,#13839,#13840,#13841,#13842,#13843)) ;
#3341 = EDGE_LOOP('',(#13844,#13845,#13846,#13847,#13848,#13849,#13850)) ;
#3342 = EDGE_LOOP('',(#13851,#13852,#13853,#13854,#13855,#13856,#13857,#13858,
#13859,#13860)) ;
#3343 = EDGE_LOOP('',(#13861,#13862,#13863,#13864,#13865,#13866,#13867)) ;
#3344 = EDGE_LOOP('',(#13868,#13869,#13870,#13871,#13872,#13873,#13874)) ;
#3345 = EDGE_LOOP('',(#13875,#13876,#13877,#13878,#13879,#13880,#13881,#13882,
#13883,#13884)) ;
#3346 = EDGE_LOOP('',(#13885,#13886,#13887,#13888,#13889,#13890,#13891)) ;
#3347 = EDGE_LOOP('',(#13892,#13893,#13894,#13895,#13896,#13897,#13898)) ;
#3348 = EDGE_LOOP('',(#13899,#13900,#13901,#13902,#13903,#13904,#13905,#13906,
#13907,#13908)) ;
#3349 = EDGE_LOOP('',(#13909,#13910,#13911,#13912,#13913,#13914,#13915)) ;
#3350 = EDGE_LOOP('',(#13916,#13917,#13918,#13919,#13920,#13921,#13922)) ;
#3351 = EDGE_LOOP('',(#13923,#13924,#13925,#13926,#13927,#13928,#13929,#13930,
#13931,#13932)) ;
#3352 = EDGE_LOOP('',(#13933,#13934,#13935,#13936,#13937,#13938,#13939)) ;
#3353 = EDGE_LOOP('',(#13940,#13941,#13942,#13943,#13944,#13945,#13946)) ;
#3354 = EDGE_LOOP('',(#13947,#13948,#13949,#13950,#13951,#13952,#13953,#13954,
#13955,#13956)) ;
#3355 = EDGE_LOOP('',(#13957,#13958,#13959,#13960,#13961,#13962,#13963)) ;
#3356 = EDGE_LOOP('',(#13964,#13965,#13966,#13967,#13968,#13969,#13970)) ;
#3357 = EDGE_LOOP('',(#13971,#13972,#13973,#13974,#13975,#13976,#13977,#13978,
#13979,#13980)) ;
#3358 = EDGE_LOOP('',(#13981,#13982,#13983,#13984,#13985,#13986,#13987)) ;
#3359 = EDGE_LOOP('',(#13988,#13989,#13990,#13991,#13992,#13993,#13994)) ;
#3360 = EDGE_LOOP('',(#13995,#13996,#13997,#13998,#13999,#14000,#14001,#14002,
#14003,#14004)) ;
#3361 = EDGE_LOOP('',(#14005,#14006,#14007,#14008,#14009,#14010,#14011)) ;
#3362 = EDGE_LOOP('',(#14012,#14013,#14014,#14015,#14016,#14017,#14018)) ;
#3363 = EDGE_LOOP('',(#14019,#14020,#14021,#14022,#14023,#14024,#14025,#14026,
#14027,#14028)) ;
#3364 = EDGE_LOOP('',(#14029,#14030,#14031,#14032,#14033,#14034,#14035)) ;
#3365 = EDGE_LOOP('',(#14036,#14037,#14038,#14039,#14040,#14041,#14042)) ;
#3366 = EDGE_LOOP('',(#14043,#14044,#14045,#14046,#14047,#14048,#14049,#14050,
#14051,#14052)) ;
#3367 = EDGE_LOOP('',(#14053,#14054,#14055,#14056,#14057,#14058,#14059)) ;
#3368 = EDGE_LOOP('',(#14060,#14061,#14062,#14063,#14064,#14065,#14066)) ;
#3369 = EDGE_LOOP('',(#14067,#14068,#14069,#14070,#14071,#14072,#14073,#14074,
#14075,#14076)) ;
#3370 = EDGE_LOOP('',(#14077,#14078,#14079,#14080,#14081,#14082,#14083)) ;
#3371 = EDGE_LOOP('',(#14084,#14085,#14086,#14087,#14088,#14089,#14090)) ;
#3372 = EDGE_LOOP('',(#14091,#14092,#14093,#14094,#14095,#14096,#14097,#14098,
#14099,#14100)) ;
#3373 = EDGE_LOOP('',(#14101,#14102,#14103,#14104,#14105,#14106,#14107)) ;
#3374 = EDGE_LOOP('',(#14108,#14109,#14110,#14111,#14112,#14113,#14114)) ;
#3375 = EDGE_LOOP('',(#14115,#14116,#14117,#14118,#14119,#14120,#14121,#14122,
#14123,#14124)) ;
#3376 = EDGE_LOOP('',(#14125,#14126,#14127,#14128,#14129,#14130,#14131)) ;
#3377 = EDGE_LOOP('',(#14132,#14133,#14134,#14135,#14136,#14137,#14138)) ;
#3378 = EDGE_LOOP('',(#14139,#14140,#14141,#14142,#14143,#14144,#14145,#14146,
#14147,#14148)) ;
#3379 = EDGE_LOOP('',(#14149,#14150,#14151,#14152,#14153,#14154,#14155)) ;
#3380 = EDGE_LOOP('',(#14156,#14157,#14158,#14159,#14160,#14161,#14162)) ;
#3381 = EDGE_LOOP('',(#14163,#14164,#14165,#14166,#14167,#14168,#14169,#14170,
#14171,#14172)) ;
#3382 = EDGE_LOOP('',(#14173,#14174,#14175,#14176,#14177,#14178,#14179)) ;
#3383 = EDGE_LOOP('',(#14180,#14181,#14182,#14183,#14184,#14185,#14186)) ;
#3384 = EDGE_LOOP('',(#14187,#14188,#14189,#14190,#14191,#14192,#14193,#14194,
#14195,#14196)) ;
#3385 = EDGE_LOOP('',(#14197,#14198,#14199,#14200,#14201,#14202,#14203)) ;
#3386 = EDGE_LOOP('',(#14204,#14205,#14206,#14207,#14208,#14209,#14210)) ;
#3387 = EDGE_LOOP('',(#14211,#14212,#14213,#14214,#14215,#14216,#14217,#14218,
#14219,#14220)) ;
#3388 = EDGE_LOOP('',(#14221,#14222,#14223,#14224,#14225,#14226,#14227)) ;
#3389 = EDGE_LOOP('',(#14228,#14229,#14230,#14231,#14232,#14233,#14234)) ;
#3390 = EDGE_LOOP('',(#14235,#14236,#14237,#14238,#14239,#14240,#14241,#14242,
#14243,#14244)) ;
#3391 = EDGE_LOOP('',(#14245,#14246,#14247,#14248,#14249,#14250,#14251)) ;
#3392 = EDGE_LOOP('',(#14252,#14253,#14254,#14255,#14256,#14257,#14258)) ;
#3393 = EDGE_LOOP('',(#14259,#14260,#14261,#14262,#14263,#14264,#14265,#14266,
#14267,#14268)) ;
#3394 = EDGE_LOOP('',(#14269,#14270,#14271,#14272,#14273,#14274,#14275)) ;
#3395 = EDGE_LOOP('',(#14276,#14277,#14278,#14279,#14280,#14281,#14282)) ;
#3396 = EDGE_LOOP('',(#14283,#14284,#14285,#14286,#14287,#14288,#14289,#14290,
#14291,#14292)) ;
#3397 = EDGE_LOOP('',(#14293,#14294,#14295,#14296,#14297,#14298,#14299)) ;
#3398 = EDGE_LOOP('',(#14300,#14301,#14302,#14303,#14304,#14305,#14306)) ;
#3399 = EDGE_LOOP('',(#14307,#14308,#14309,#14310,#14311,#14312,#14313,#14314,
#14315,#14316)) ;
#3400 = EDGE_LOOP('',(#14317,#14318,#14319,#14320,#14321,#14322,#14323)) ;
#3401 = EDGE_LOOP('',(#14324,#14325,#14326,#14327,#14328,#14329,#14330)) ;
#3402 = EDGE_LOOP('',(#14331,#14332,#14333,#14334,#14335,#14336,#14337,#14338,
#14339,#14340)) ;
#3403 = EDGE_LOOP('',(#14341,#14342,#14343,#14344,#14345,#14346,#14347)) ;
#3404 = EDGE_LOOP('',(#14348,#14349,#14350,#14351)) ;
#3405 = EDGE_LOOP('',(#14352)) ;
#3406 = EDGE_LOOP('',(#14353)) ;
#3407 = EDGE_LOOP('',(#14354,#14355,#14356,#14357)) ;
#3408 = EDGE_LOOP('',(#14358,#14359,#14360,#14361)) ;
#3409 = EDGE_LOOP('',(#14362,#14363,#14364,#14365)) ;
#3410 = EDGE_LOOP('',(#14366,#14367,#14368,#14369)) ;
#3411 = EDGE_LOOP('',(#14370)) ;
#3412 = EDGE_LOOP('',(#14371)) ;
#3413 = EDGE_LOOP('',(#14372,#14373,#14374,#14375)) ;
#3414 = EDGE_LOOP('',(#14376,#14377,#14378,#14379)) ;
#3415 = EDGE_LOOP('',(#14380,#14381,#14382,#14383)) ;
#3416 = EDGE_LOOP('',(#14384,#14385,#14386,#14387)) ;
#3417 = EDGE_LOOP('',(#14388,#14389,#14390,#14391)) ;
#3418 = EDGE_LOOP('',(#14392,#14393,#14394,#14395)) ;
#3419 = EDGE_LOOP('',(#14396,#14397,#14398,#14399)) ;
#3420 = EDGE_LOOP('',(#14400,#14401,#14402,#14403)) ;
#3421 = EDGE_LOOP('',(#14404,#14405,#14406,#14407)) ;
#3422 = EDGE_LOOP('',(#14408,#14409,#14410,#14411)) ;
#3423 = EDGE_LOOP('',(#14412,#14413,#14414,#14415)) ;
#3424 = EDGE_LOOP('',(#14416)) ;
#3425 = EDGE_LOOP('',(#14417)) ;
#3426 = EDGE_LOOP('',(#14418)) ;
#3427 = EDGE_LOOP('',(#14419)) ;
#3428 = EDGE_LOOP('',(#14420)) ;
#3429 = EDGE_LOOP('',(#14421)) ;
#3430 = EDGE_LOOP('',(#14422)) ;
#3431 = EDGE_LOOP('',(#14423)) ;
#3432 = EDGE_LOOP('',(#14424)) ;
#3433 = EDGE_LOOP('',(#14425)) ;
#3434 = EDGE_LOOP('',(#14426)) ;
#3435 = EDGE_LOOP('',(#14427)) ;
#3436 = EDGE_LOOP('',(#14428)) ;
#3437 = EDGE_LOOP('',(#14429)) ;
#3438 = EDGE_LOOP('',(#14430)) ;
#3439 = EDGE_LOOP('',(#14431)) ;
#3440 = EDGE_LOOP('',(#14432)) ;
#3441 = EDGE_LOOP('',(#14433)) ;
#3442 = EDGE_LOOP('',(#14434)) ;
#3443 = EDGE_LOOP('',(#14435)) ;
#3444 = EDGE_LOOP('',(#14436,#14437,#14438,#14439)) ;
#3445 = EDGE_LOOP('',(#14440,#14441,#14442,#14443)) ;
#3446 = EDGE_LOOP('',(#14444,#14445,#14446,#14447)) ;
#3447 = EDGE_LOOP('',(#14448,#14449,#14450,#14451)) ;
#3448 = EDGE_LOOP('',(#14452,#14453,#14454,#14455)) ;
#3449 = EDGE_LOOP('',(#14456,#14457,#14458,#14459)) ;
#3450 = EDGE_LOOP('',(#14460,#14461,#14462,#14463)) ;
#3451 = EDGE_LOOP('',(#14464,#14465,#14466,#14467)) ;
#3452 = EDGE_LOOP('',(#14468,#14469,#14470,#14471)) ;
#3453 = EDGE_LOOP('',(#14472,#14473,#14474,#14475)) ;
#3454 = EDGE_LOOP('',(#14476)) ;
#3455 = EDGE_LOOP('',(#14477)) ;
#3456 = EDGE_LOOP('',(#14478)) ;
#3457 = EDGE_LOOP('',(#14479)) ;
#3458 = EDGE_LOOP('',(#14480)) ;
#3459 = EDGE_LOOP('',(#14481)) ;
#3460 = EDGE_LOOP('',(#14482)) ;
#3461 = EDGE_LOOP('',(#14483)) ;
#3462 = EDGE_LOOP('',(#14484)) ;
#3463 = EDGE_LOOP('',(#14485)) ;
#3464 = EDGE_LOOP('',(#14486)) ;
#3465 = EDGE_LOOP('',(#14487)) ;
#3466 = EDGE_LOOP('',(#14488)) ;
#3467 = EDGE_LOOP('',(#14489)) ;
#3468 = EDGE_LOOP('',(#14490)) ;
#3469 = EDGE_LOOP('',(#14491)) ;
#3470 = EDGE_LOOP('',(#14492)) ;
#3471 = EDGE_LOOP('',(#14493)) ;
#3472 = EDGE_LOOP('',(#14494)) ;
#3473 = EDGE_LOOP('',(#14495)) ;
#3474 = CIRCLE('',#15678,4.263) ;
#3475 = CIRCLE('',#15680,4.263) ;
#3476 = CIRCLE('',#15682,4.263) ;
#3477 = CIRCLE('',#15684,4.263) ;
#3478 = CIRCLE('',#15686,4.263) ;
#3479 = CIRCLE('',#15688,4.263) ;
#3480 = CIRCLE('',#15690,4.263) ;
#3481 = CIRCLE('',#15692,4.263) ;
#3482 = CIRCLE('',#15694,9.) ;
#3483 = CIRCLE('',#15695,5.5) ;
#3484 = CIRCLE('',#15697,9.) ;
#3485 = CIRCLE('',#15699,5.5) ;
#3486 = CIRCLE('',#15701,9.) ;
#3487 = CIRCLE('',#15702,5.5) ;
#3488 = CIRCLE('',#15704,9.) ;
#3489 = CIRCLE('',#15706,5.5) ;
#3490 = CIRCLE('',#15708,9.) ;
#3491 = CIRCLE('',#15709,5.5) ;
#3492 = CIRCLE('',#15711,9.) ;
#3493 = CIRCLE('',#15713,5.5) ;
#3494 = CIRCLE('',#15715,9.) ;
#3495 = CIRCLE('',#15716,5.5) ;
#3496 = CIRCLE('',#15718,9.) ;
#3497 = CIRCLE('',#15720,5.5) ;
#3498 = CIRCLE('',#15722,3.3) ;
#3499 = CIRCLE('',#15724,3.3) ;
#3500 = CIRCLE('',#15726,2.5175) ;
#3501 = CIRCLE('',#15728,2.5175) ;
#3502 = CIRCLE('',#15730,2.5175) ;
#3503 = CIRCLE('',#15732,2.5175) ;
#3504 = CIRCLE('',#15734,2.5175) ;
#3505 = CIRCLE('',#15736,2.5175) ;
#3506 = CIRCLE('',#15738,2.5175) ;
#3507 = CIRCLE('',#15740,2.5175) ;
#3508 = CIRCLE('',#15742,2.5175) ;
#3509 = CIRCLE('',#15744,2.5175) ;
#3510 = CIRCLE('',#15746,2.5175) ;
#3511 = CIRCLE('',#15748,2.5175) ;
#3512 = CIRCLE('',#15750,3.3) ;
#3513 = CIRCLE('',#15752,3.3) ;
#3514 = CIRCLE('',#15754,37.5) ;
#3515 = CIRCLE('',#15755,37.5) ;
#3516 = CIRCLE('',#15764,9.) ;
#3517 = CIRCLE('',#15765,5.5) ;
#3518 = CIRCLE('',#15767,9.) ;
#3519 = CIRCLE('',#15769,5.5) ;
#3520 = CIRCLE('',#15771,9.) ;
#3521 = CIRCLE('',#15772,5.5) ;
#3522 = CIRCLE('',#15774,9.) ;
#3523 = CIRCLE('',#15776,5.5) ;
#3524 = CIRCLE('',#15778,9.) ;
#3525 = CIRCLE('',#15779,5.5) ;
#3526 = CIRCLE('',#15781,9.) ;
#3527 = CIRCLE('',#15783,5.5) ;
#3528 = CIRCLE('',#15785,9.) ;
#3529 = CIRCLE('',#15786,5.5) ;
#3530 = CIRCLE('',#15788,9.) ;
#3531 = CIRCLE('',#15790,5.5) ;
#3532 = CIRCLE('',#15792,9.) ;
#3533 = CIRCLE('',#15793,5.5) ;
#3534 = CIRCLE('',#15795,9.) ;
#3535 = CIRCLE('',#15797,5.5) ;
#3536 = CIRCLE('',#15799,9.) ;
#3537 = CIRCLE('',#15800,5.5) ;
#3538 = CIRCLE('',#15802,9.) ;
#3539 = CIRCLE('',#15804,5.5) ;
#3540 = CIRCLE('',#15806,9.) ;
#3541 = CIRCLE('',#15807,5.5) ;
#3542 = CIRCLE('',#15809,9.) ;
#3543 = CIRCLE('',#15811,5.5) ;
#3544 = CIRCLE('',#15813,9.) ;
#3545 = CIRCLE('',#15814,5.5) ;
#3546 = CIRCLE('',#15816,9.) ;
#3547 = CIRCLE('',#15818,5.5) ;
#3548 = CIRCLE('',#15820,9.) ;
#3549 = CIRCLE('',#15821,5.5) ;
#3550 = CIRCLE('',#15823,9.) ;
#3551 = CIRCLE('',#15825,5.5) ;
#3552 = CIRCLE('',#15827,9.) ;
#3553 = CIRCLE('',#15828,5.5) ;
#3554 = CIRCLE('',#15830,9.) ;
#3555 = CIRCLE('',#15832,5.5) ;
#3556 = CIRCLE('',#15834,9.) ;
#3557 = CIRCLE('',#15835,5.5) ;
#3558 = CIRCLE('',#15837,9.) ;
#3559 = CIRCLE('',#15839,5.5) ;
#3560 = CIRCLE('',#15841,9.) ;
#3561 = CIRCLE('',#15842,5.5) ;
#3562 = CIRCLE('',#15844,9.) ;
#3563 = CIRCLE('',#15846,5.5) ;
#3564 = CIRCLE('',#15855,4.263) ;
#3565 = CIRCLE('',#15857,4.263) ;
#3566 = CIRCLE('',#15859,4.263) ;
#3567 = CIRCLE('',#15861,4.263) ;
#3568 = CIRCLE('',#15863,4.263) ;
#3569 = CIRCLE('',#15865,4.263) ;
#3570 = CIRCLE('',#15867,4.263) ;
#3571 = CIRCLE('',#15869,4.263) ;
#3572 = CIRCLE('',#15871,4.263) ;
#3573 = CIRCLE('',#15873,4.263) ;
#3574 = CIRCLE('',#15875,4.263) ;
#3575 = CIRCLE('',#15877,4.263) ;
#3576 = CIRCLE('',#15880,4.263) ;
#3577 = CIRCLE('',#15882,4.263) ;
#3578 = CIRCLE('',#15884,4.263) ;
#3579 = CIRCLE('',#15886,4.263) ;
#3580 = CIRCLE('',#15894,2.117) ;
#3581 = CIRCLE('',#15896,2.117) ;
#3582 = CIRCLE('',#15898,2.117) ;
#3583 = CIRCLE('',#15900,2.117) ;
#3584 = CIRCLE('',#15902,4.263) ;
#3585 = CIRCLE('',#15904,4.263) ;
#3586 = CIRCLE('',#15906,4.263) ;
#3587 = CIRCLE('',#15908,4.263) ;
#3588 = CIRCLE('',#15910,4.263) ;
#3589 = CIRCLE('',#15912,4.263) ;
#3590 = CIRCLE('',#15914,4.263) ;
#3591 = CIRCLE('',#15916,4.263) ;
#3592 = CIRCLE('',#15918,9.) ;
#3593 = CIRCLE('',#15919,5.5) ;
#3594 = CIRCLE('',#15921,9.) ;
#3595 = CIRCLE('',#15923,5.5) ;
#3596 = CIRCLE('',#15925,9.) ;
#3597 = CIRCLE('',#15926,5.5) ;
#3598 = CIRCLE('',#15928,9.) ;
#3599 = CIRCLE('',#15930,5.5) ;
#3600 = CIRCLE('',#15932,9.) ;
#3601 = CIRCLE('',#15933,5.5) ;
#3602 = CIRCLE('',#15935,9.) ;
#3603 = CIRCLE('',#15937,5.5) ;
#3604 = CIRCLE('',#15939,9.) ;
#3605 = CIRCLE('',#15940,5.5) ;
#3606 = CIRCLE('',#15942,9.) ;
#3607 = CIRCLE('',#15944,5.5) ;
#3608 = CIRCLE('',#15946,3.3) ;
#3609 = CIRCLE('',#15948,3.3) ;
#3610 = CIRCLE('',#15950,2.5175) ;
#3611 = CIRCLE('',#15952,2.5175) ;
#3612 = CIRCLE('',#15954,2.5175) ;
#3613 = CIRCLE('',#15956,2.5175) ;
#3614 = CIRCLE('',#15958,2.5175) ;
#3615 = CIRCLE('',#15960,2.5175) ;
#3616 = CIRCLE('',#15962,2.5175) ;
#3617 = CIRCLE('',#15964,2.5175) ;
#3618 = CIRCLE('',#15966,2.5175) ;
#3619 = CIRCLE('',#15968,2.5175) ;
#3620 = CIRCLE('',#15970,2.5175) ;
#3621 = CIRCLE('',#15972,2.5175) ;
#3622 = CIRCLE('',#15974,3.3) ;
#3623 = CIRCLE('',#15976,3.3) ;
#3624 = CIRCLE('',#15978,37.5) ;
#3625 = CIRCLE('',#15979,37.5) ;
#3626 = CIRCLE('',#15988,4.263) ;
#3627 = CIRCLE('',#15990,4.263) ;
#3628 = CIRCLE('',#15992,4.263) ;
#3629 = CIRCLE('',#15994,4.263) ;
#3630 = CIRCLE('',#15996,4.263) ;
#3631 = CIRCLE('',#15998,4.263) ;
#3632 = CIRCLE('',#16000,4.263) ;
#3633 = CIRCLE('',#16002,4.263) ;
#3634 = CIRCLE('',#16004,4.263) ;
#3635 = CIRCLE('',#16006,4.263) ;
#3636 = CIRCLE('',#16008,4.263) ;
#3637 = CIRCLE('',#16010,4.263) ;
#3638 = CIRCLE('',#16013,4.263) ;
#3639 = CIRCLE('',#16015,4.263) ;
#3640 = CIRCLE('',#16017,4.263) ;
#3641 = CIRCLE('',#16019,4.263) ;
#3642 = CIRCLE('',#16027,19.425) ;
#3643 = CIRCLE('',#16041,22.12975) ;
#3644 = CIRCLE('',#16048,22.12975) ;
#3645 = CIRCLE('',#16050,20.33524) ;
#3646 = CIRCLE('',#16057,18.56595) ;
#3647 = CIRCLE('',#16071,18.56595) ;
#3648 = CIRCLE('',#16073,20.33524) ;
#3649 = CIRCLE('',#16075,22.12975) ;
#3650 = CIRCLE('',#16077,19.425) ;
#3651 = CIRCLE('',#16079,13.2000000000001) ;
#3652 = CIRCLE('',#16080,13.4500000000001) ;
#3653 = CIRCLE('',#16081,13.2000000000001) ;
#3654 = CIRCLE('',#16083,17.25) ;
#3655 = CIRCLE('',#16085,13.2) ;
#3656 = CIRCLE('',#16087,17.5) ;
#3657 = CIRCLE('',#16088,17.5) ;
#3658 = CIRCLE('',#16090,17.5) ;
#3659 = CIRCLE('',#16092,19.9999999999999) ;
#3660 = CIRCLE('',#16093,19.7499999999997) ;
#3661 = CIRCLE('',#16094,19.9999999999999) ;
#3662 = CIRCLE('',#16096,20.) ;
#3663 = CIRCLE('',#16098,18.) ;
#3664 = CIRCLE('',#16100,22.5) ;
#3665 = CIRCLE('',#16101,22.25) ;
#3666 = CIRCLE('',#16102,22.5) ;
#3667 = CIRCLE('',#16104,22.5) ;
#3668 = CIRCLE('',#16107,33.5) ;
#3669 = CIRCLE('',#16108,33.2649649327684) ;
#3670 = CIRCLE('',#16109,33.2649649327684) ;
#3671 = CIRCLE('',#16110,33.5) ;
#3672 = CIRCLE('',#16112,33.5) ;
#3673 = CIRCLE('',#16113,33.5) ;
#3674 = CIRCLE('',#16115,20.065) ;
#3675 = CIRCLE('',#16117,33.25) ;
#3676 = CIRCLE('',#16119,23.) ;
#3677 = CIRCLE('',#16121,15.6275202784794) ;
#3678 = CIRCLE('',#16122,15.8837) ;
#3679 = CIRCLE('',#16123,15.6275202784794) ;
#3680 = CIRCLE('',#16127,33.5) ;
#3681 = CIRCLE('',#16128,33.25) ;
#3682 = CIRCLE('',#16129,33.5) ;
#3683 = CIRCLE('',#16131,33.5) ;
#3684 = CIRCLE('',#16132,33.5) ;
#3685 = CIRCLE('',#16134,22.5) ;
#3686 = CIRCLE('',#16136,33.25) ;
#3687 = CIRCLE('',#16138,20.065) ;
#3688 = CIRCLE('',#16144,20.065) ;
#3689 = CIRCLE('',#16147,5.00000000000251) ;
#3690 = CIRCLE('',#16150,5.00000000000251) ;
#3691 = CIRCLE('',#16153,20.065) ;
#3692 = CIRCLE('',#16155,23.) ;
#3693 = CIRCLE('',#16159,22.5) ;
#3694 = CIRCLE('',#16161,22.25) ;
#3695 = CIRCLE('',#16163,22.25) ;
#3696 = CIRCLE('',#16166,18.) ;
#3697 = CIRCLE('',#16170,5.) ;
#3698 = CIRCLE('',#16173,5.) ;
#3699 = CIRCLE('',#16179,4.99999999999999) ;
#3700 = CIRCLE('',#16182,4.99999999999999) ;
#3701 = CIRCLE('',#16193,27.) ;
#3702 = CIRCLE('',#16194,26.8) ;
#3703 = CIRCLE('',#16196,22.7) ;
#3704 = CIRCLE('',#16198,27.) ;
#3705 = CIRCLE('',#16200,22.5) ;
#3706 = CIRCLE('',#16202,22.5) ;
#3707 = CIRCLE('',#16204,26.8) ;
#3708 = CIRCLE('',#16206,22.7) ;
#3709 = CIRCLE('',#16213,40.) ;
#3710 = CIRCLE('',#16214,20.) ;
#3711 = CIRCLE('',#16216,47.175) ;
#3712 = CIRCLE('',#16217,47.175) ;
#3713 = CIRCLE('',#16219,47.175) ;
#3714 = CIRCLE('',#16220,47.175) ;
#3715 = CIRCLE('',#16222,47.175) ;
#3716 = CIRCLE('',#16223,47.175) ;
#3717 = CIRCLE('',#16225,47.175) ;
#3718 = CIRCLE('',#16226,47.175) ;
#3719 = CIRCLE('',#16228,47.175) ;
#3720 = CIRCLE('',#16229,47.175) ;
#3721 = CIRCLE('',#16231,47.175) ;
#3722 = CIRCLE('',#16232,47.175) ;
#3723 = CIRCLE('',#16234,47.175) ;
#3724 = CIRCLE('',#16235,47.175) ;
#3725 = CIRCLE('',#16237,47.175) ;
#3726 = CIRCLE('',#16238,47.175) ;
#3727 = CIRCLE('',#16240,47.175) ;
#3728 = CIRCLE('',#16241,47.175) ;
#3729 = CIRCLE('',#16243,47.175) ;
#3730 = CIRCLE('',#16244,47.175) ;
#3731 = CIRCLE('',#16246,47.175) ;
#3732 = CIRCLE('',#16247,47.175) ;
#3733 = CIRCLE('',#16249,47.175) ;
#3734 = CIRCLE('',#16250,47.175) ;
#3735 = CIRCLE('',#16252,47.175) ;
#3736 = CIRCLE('',#16253,47.175) ;
#3737 = CIRCLE('',#16255,47.175) ;
#3738 = CIRCLE('',#16256,47.175) ;
#3739 = CIRCLE('',#16258,47.175) ;
#3740 = CIRCLE('',#16259,47.175) ;
#3741 = CIRCLE('',#16261,47.175) ;
#3742 = CIRCLE('',#16262,47.175) ;
#3743 = CIRCLE('',#16264,47.175) ;
#3744 = CIRCLE('',#16265,47.175) ;
#3745 = CIRCLE('',#16267,47.175) ;
#3746 = CIRCLE('',#16268,47.175) ;
#3747 = CIRCLE('',#16270,47.175) ;
#3748 = CIRCLE('',#16271,47.175) ;
#3749 = CIRCLE('',#16273,47.175) ;
#3750 = CIRCLE('',#16274,47.175) ;
#3751 = CIRCLE('',#16276,47.175) ;
#3752 = CIRCLE('',#16277,47.175) ;
#3753 = CIRCLE('',#16279,47.175) ;
#3754 = CIRCLE('',#16280,47.175) ;
#3755 = CIRCLE('',#16282,47.175) ;
#3756 = CIRCLE('',#16283,47.175) ;
#3757 = CIRCLE('',#16285,47.175) ;
#3758 = CIRCLE('',#16286,47.175) ;
#3759 = CIRCLE('',#16288,47.175) ;
#3760 = CIRCLE('',#16289,47.175) ;
#3761 = CIRCLE('',#16291,47.175) ;
#3762 = CIRCLE('',#16292,47.175) ;
#3763 = CIRCLE('',#16294,47.175) ;
#3764 = CIRCLE('',#16295,47.175) ;
#3765 = CIRCLE('',#16297,47.175) ;
#3766 = CIRCLE('',#16298,47.175) ;
#3767 = CIRCLE('',#16300,47.175) ;
#3768 = CIRCLE('',#16301,47.175) ;
#3769 = CIRCLE('',#16303,47.175) ;
#3770 = CIRCLE('',#16304,47.175) ;
#3771 = CIRCLE('',#16306,47.175) ;
#3772 = CIRCLE('',#16307,47.175) ;
#3773 = CIRCLE('',#16309,47.175) ;
#3774 = CIRCLE('',#16310,47.175) ;
#3775 = CIRCLE('',#16312,47.175) ;
#3776 = CIRCLE('',#16313,47.175) ;
#3777 = CIRCLE('',#16315,47.175) ;
#3778 = CIRCLE('',#16316,47.175) ;
#3779 = CIRCLE('',#16318,47.175) ;
#3780 = CIRCLE('',#16319,47.175) ;
#3781 = CIRCLE('',#16321,47.175) ;
#3782 = CIRCLE('',#16322,47.175) ;
#3783 = CIRCLE('',#16324,47.175) ;
#3784 = CIRCLE('',#16325,47.175) ;
#3785 = CIRCLE('',#16327,47.175) ;
#3786 = CIRCLE('',#16328,47.175) ;
#3787 = CIRCLE('',#16330,47.175) ;
#3788 = CIRCLE('',#16331,47.175) ;
#3789 = CIRCLE('',#16333,47.175) ;
#3790 = CIRCLE('',#16334,47.175) ;
#3791 = CIRCLE('',#16336,47.175) ;
#3792 = CIRCLE('',#16337,47.175) ;
#3793 = CIRCLE('',#16339,47.175) ;
#3794 = CIRCLE('',#16340,47.175) ;
#3795 = CIRCLE('',#16342,47.175) ;
#3796 = CIRCLE('',#16343,47.175) ;
#3797 = CIRCLE('',#16345,47.175) ;
#3798 = CIRCLE('',#16346,47.175) ;
#3799 = CIRCLE('',#16348,47.175) ;
#3800 = CIRCLE('',#16349,47.175) ;
#3801 = CIRCLE('',#16351,47.175) ;
#3802 = CIRCLE('',#16352,47.175) ;
#3803 = CIRCLE('',#16354,47.175) ;
#3804 = CIRCLE('',#16355,47.175) ;
#3805 = CIRCLE('',#16357,47.175) ;
#3806 = CIRCLE('',#16358,47.175) ;
#3807 = CIRCLE('',#16360,47.175) ;
#3808 = CIRCLE('',#16361,47.175) ;
#3809 = CIRCLE('',#16363,47.175) ;
#3810 = CIRCLE('',#16364,47.175) ;
#3811 = CIRCLE('',#16366,47.175) ;
#3812 = CIRCLE('',#16367,47.175) ;
#3813 = CIRCLE('',#16369,47.175) ;
#3814 = CIRCLE('',#16370,47.175) ;
#3815 = CIRCLE('',#16372,47.175) ;
#3816 = CIRCLE('',#16373,47.175) ;
#3817 = CIRCLE('',#16375,47.175) ;
#3818 = CIRCLE('',#16376,47.175) ;
#3819 = CIRCLE('',#16378,47.175) ;
#3820 = CIRCLE('',#16379,47.175) ;
#3821 = CIRCLE('',#16381,47.175) ;
#3822 = CIRCLE('',#16382,47.175) ;
#3823 = CIRCLE('',#16384,47.175) ;
#3824 = CIRCLE('',#16385,47.175) ;
#3825 = CIRCLE('',#16387,47.175) ;
#3826 = CIRCLE('',#16388,47.175) ;
#3827 = CIRCLE('',#16390,47.175) ;
#3828 = CIRCLE('',#16391,47.175) ;
#3829 = CIRCLE('',#16393,47.175) ;
#3830 = CIRCLE('',#16394,47.175) ;
#3831 = CIRCLE('',#16396,40.) ;
#3832 = CIRCLE('',#16398,47.0433475024125) ;
#3833 = CIRCLE('',#16400,49.2411809548974) ;
#3834 = CIRCLE('',#16401,49.2411809548974) ;
#3835 = CIRCLE('',#16403,49.5) ;
#3836 = CIRCLE('',#16404,49.5) ;
#3837 = CIRCLE('',#16406,47.175) ;
#3838 = CIRCLE('',#16407,47.175) ;
#3839 = CIRCLE('',#16408,47.175) ;
#3840 = CIRCLE('',#16409,47.175) ;
#3841 = CIRCLE('',#16410,47.175) ;
#3842 = CIRCLE('',#16411,47.175) ;
#3843 = CIRCLE('',#16412,47.175) ;
#3844 = CIRCLE('',#16413,47.175) ;
#3845 = CIRCLE('',#16414,47.175) ;
#3846 = CIRCLE('',#16415,47.175) ;
#3847 = CIRCLE('',#16416,47.175) ;
#3848 = CIRCLE('',#16417,47.175) ;
#3849 = CIRCLE('',#16418,47.175) ;
#3850 = CIRCLE('',#16419,47.175) ;
#3851 = CIRCLE('',#16420,47.175) ;
#3852 = CIRCLE('',#16421,47.175) ;
#3853 = CIRCLE('',#16422,47.175) ;
#3854 = CIRCLE('',#16423,47.175) ;
#3855 = CIRCLE('',#16424,47.175) ;
#3856 = CIRCLE('',#16425,47.175) ;
#3857 = CIRCLE('',#16426,47.175) ;
#3858 = CIRCLE('',#16427,47.175) ;
#3859 = CIRCLE('',#16428,47.175) ;
#3860 = CIRCLE('',#16429,47.175) ;
#3861 = CIRCLE('',#16430,47.175) ;
#3862 = CIRCLE('',#16431,47.175) ;
#3863 = CIRCLE('',#16432,47.175) ;
#3864 = CIRCLE('',#16433,47.175) ;
#3865 = CIRCLE('',#16434,47.175) ;
#3866 = CIRCLE('',#16435,47.175) ;
#3867 = CIRCLE('',#16436,47.175) ;
#3868 = CIRCLE('',#16437,47.175) ;
#3869 = CIRCLE('',#16438,47.175) ;
#3870 = CIRCLE('',#16439,47.175) ;
#3871 = CIRCLE('',#16440,47.175) ;
#3872 = CIRCLE('',#16441,47.175) ;
#3873 = CIRCLE('',#16442,47.175) ;
#3874 = CIRCLE('',#16443,47.175) ;
#3875 = CIRCLE('',#16444,47.175) ;
#3876 = CIRCLE('',#16445,47.175) ;
#3877 = CIRCLE('',#16446,47.175) ;
#3878 = CIRCLE('',#16447,47.175) ;
#3879 = CIRCLE('',#16448,47.175) ;
#3880 = CIRCLE('',#16449,47.175) ;
#3881 = CIRCLE('',#16450,47.175) ;
#3882 = CIRCLE('',#16451,47.175) ;
#3883 = CIRCLE('',#16452,47.175) ;
#3884 = CIRCLE('',#16453,47.175) ;
#3885 = CIRCLE('',#16454,47.175) ;
#3886 = CIRCLE('',#16455,47.175) ;
#3887 = CIRCLE('',#16456,47.175) ;
#3888 = CIRCLE('',#16457,47.175) ;
#3889 = CIRCLE('',#16458,47.175) ;
#3890 = CIRCLE('',#16459,47.175) ;
#3891 = CIRCLE('',#16460,47.175) ;
#3892 = CIRCLE('',#16461,47.175) ;
#3893 = CIRCLE('',#16462,47.175) ;
#3894 = CIRCLE('',#16463,47.175) ;
#3895 = CIRCLE('',#16464,47.175) ;
#3896 = CIRCLE('',#16465,47.175) ;
#3897 = CIRCLE('',#16466,47.175) ;
#3898 = CIRCLE('',#16468,49.5) ;
#3899 = CIRCLE('',#16469,49.5) ;
#3900 = CIRCLE('',#16470,47.175) ;
#3901 = CIRCLE('',#16471,47.175) ;
#3902 = CIRCLE('',#16472,47.175) ;
#3903 = CIRCLE('',#16473,47.175) ;
#3904 = CIRCLE('',#16474,47.175) ;
#3905 = CIRCLE('',#16475,47.175) ;
#3906 = CIRCLE('',#16476,47.175) ;
#3907 = CIRCLE('',#16477,47.175) ;
#3908 = CIRCLE('',#16478,47.175) ;
#3909 = CIRCLE('',#16479,47.175) ;
#3910 = CIRCLE('',#16480,47.175) ;
#3911 = CIRCLE('',#16481,47.175) ;
#3912 = CIRCLE('',#16482,47.175) ;
#3913 = CIRCLE('',#16483,47.175) ;
#3914 = CIRCLE('',#16484,47.175) ;
#3915 = CIRCLE('',#16485,47.175) ;
#3916 = CIRCLE('',#16486,47.175) ;
#3917 = CIRCLE('',#16487,47.175) ;
#3918 = CIRCLE('',#16488,47.175) ;
#3919 = CIRCLE('',#16489,47.175) ;
#3920 = CIRCLE('',#16490,47.175) ;
#3921 = CIRCLE('',#16491,47.175) ;
#3922 = CIRCLE('',#16492,47.175) ;
#3923 = CIRCLE('',#16493,47.175) ;
#3924 = CIRCLE('',#16494,47.175) ;
#3925 = CIRCLE('',#16495,47.175) ;
#3926 = CIRCLE('',#16496,47.175) ;
#3927 = CIRCLE('',#16497,47.175) ;
#3928 = CIRCLE('',#16498,47.175) ;
#3929 = CIRCLE('',#16499,47.175) ;
#3930 = CIRCLE('',#16500,47.175) ;
#3931 = CIRCLE('',#16501,47.175) ;
#3932 = CIRCLE('',#16502,47.175) ;
#3933 = CIRCLE('',#16503,47.175) ;
#3934 = CIRCLE('',#16504,47.175) ;
#3935 = CIRCLE('',#16505,47.175) ;
#3936 = CIRCLE('',#16506,47.175) ;
#3937 = CIRCLE('',#16507,47.175) ;
#3938 = CIRCLE('',#16508,47.175) ;
#3939 = CIRCLE('',#16509,47.175) ;
#3940 = CIRCLE('',#16510,47.175) ;
#3941 = CIRCLE('',#16511,47.175) ;
#3942 = CIRCLE('',#16512,47.175) ;
#3943 = CIRCLE('',#16513,47.175) ;
#3944 = CIRCLE('',#16514,47.175) ;
#3945 = CIRCLE('',#16515,47.175) ;
#3946 = CIRCLE('',#16516,47.175) ;
#3947 = CIRCLE('',#16517,47.175) ;
#3948 = CIRCLE('',#16518,47.175) ;
#3949 = CIRCLE('',#16519,47.175) ;
#3950 = CIRCLE('',#16520,47.175) ;
#3951 = CIRCLE('',#16521,47.175) ;
#3952 = CIRCLE('',#16522,47.175) ;
#3953 = CIRCLE('',#16523,47.175) ;
#3954 = CIRCLE('',#16524,47.175) ;
#3955 = CIRCLE('',#16525,47.175) ;
#3956 = CIRCLE('',#16526,47.175) ;
#3957 = CIRCLE('',#16527,47.175) ;
#3958 = CIRCLE('',#16528,47.175) ;
#3959 = CIRCLE('',#16529,47.175) ;
#3960 = CIRCLE('',#16530,47.175) ;
#3961 = CIRCLE('',#16532,49.2411809548975) ;
#3962 = CIRCLE('',#16533,49.2411809548975) ;
#3963 = CIRCLE('',#16535,47.0433475024126) ;
#3964 = CIRCLE('',#16537,40.) ;
#3965 = CIRCLE('',#16539,40.) ;
#3966 = CIRCLE('',#16541,37.5) ;
#3967 = CIRCLE('',#16543,37.5) ;
#3968 = CIRCLE('',#16545,20.) ;
#3969 = CIRCLE('',#16547,0.539999999999986) ;
#3970 = CIRCLE('',#16548,0.539999999999996) ;
#3971 = CIRCLE('',#16549,1.4) ;
#3972 = CIRCLE('',#16551,0.539999999999986) ;
#3973 = CIRCLE('',#16552,1.4) ;
#3974 = CIRCLE('',#16553,0.539999999999996) ;
#3975 = CIRCLE('',#16558,0.539999999999996) ;
#3976 = CIRCLE('',#16559,1.4) ;
#3977 = CIRCLE('',#16560,0.539999999999986) ;
#3978 = CIRCLE('',#16562,0.539999999999986) ;
#3979 = CIRCLE('',#16563,1.4) ;
#3980 = CIRCLE('',#16564,0.539999999999996) ;
#3981 = CIRCLE('',#16569,0.539999999999996) ;
#3982 = CIRCLE('',#16570,1.4) ;
#3983 = CIRCLE('',#16571,0.539999999999986) ;
#3984 = CIRCLE('',#16573,0.539999999999986) ;
#3985 = CIRCLE('',#16574,1.4) ;
#3986 = CIRCLE('',#16575,0.539999999999996) ;
#3987 = CIRCLE('',#16580,0.539999999999996) ;
#3988 = CIRCLE('',#16581,1.4) ;
#3989 = CIRCLE('',#16582,0.539999999999986) ;
#3990 = CIRCLE('',#16584,0.539999999999986) ;
#3991 = CIRCLE('',#16585,1.4) ;
#3992 = CIRCLE('',#16586,0.539999999999996) ;
#3993 = CIRCLE('',#16591,0.539999999999996) ;
#3994 = CIRCLE('',#16592,1.4) ;
#3995 = CIRCLE('',#16593,0.539999999999986) ;
#3996 = CIRCLE('',#16595,0.539999999999986) ;
#3997 = CIRCLE('',#16596,1.4) ;
#3998 = CIRCLE('',#16597,0.539999999999996) ;
#3999 = CIRCLE('',#16602,0.539999999999996) ;
#4000 = CIRCLE('',#16603,1.4) ;
#4001 = CIRCLE('',#16604,0.539999999999986) ;
#4002 = CIRCLE('',#16606,0.539999999999986) ;
#4003 = CIRCLE('',#16607,1.4) ;
#4004 = CIRCLE('',#16608,0.539999999999996) ;
#4005 = CIRCLE('',#16613,0.539999999999996) ;
#4006 = CIRCLE('',#16614,1.4) ;
#4007 = CIRCLE('',#16615,0.539999999999986) ;
#4008 = CIRCLE('',#16617,0.539999999999986) ;
#4009 = CIRCLE('',#16618,1.4) ;
#4010 = CIRCLE('',#16619,0.539999999999996) ;
#4011 = CIRCLE('',#16624,0.539999999999996) ;
#4012 = CIRCLE('',#16625,1.4) ;
#4013 = CIRCLE('',#16626,0.539999999999986) ;
#4014 = CIRCLE('',#16628,0.539999999999986) ;
#4015 = CIRCLE('',#16629,1.4) ;
#4016 = CIRCLE('',#16630,0.539999999999996) ;
#4017 = CIRCLE('',#16635,0.539999999999996) ;
#4018 = CIRCLE('',#16636,1.4) ;
#4019 = CIRCLE('',#16637,0.539999999999986) ;
#4020 = CIRCLE('',#16639,0.539999999999986) ;
#4021 = CIRCLE('',#16640,1.4) ;
#4022 = CIRCLE('',#16641,0.539999999999996) ;
#4023 = CIRCLE('',#16646,0.539999999999996) ;
#4024 = CIRCLE('',#16647,1.4) ;
#4025 = CIRCLE('',#16648,0.539999999999986) ;
#4026 = CIRCLE('',#16650,0.539999999999986) ;
#4027 = CIRCLE('',#16651,1.4) ;
#4028 = CIRCLE('',#16652,0.539999999999996) ;
#4029 = CIRCLE('',#16657,0.539999999999996) ;
#4030 = CIRCLE('',#16658,1.4) ;
#4031 = CIRCLE('',#16659,0.539999999999986) ;
#4032 = CIRCLE('',#16661,0.539999999999986) ;
#4033 = CIRCLE('',#16662,1.4) ;
#4034 = CIRCLE('',#16663,0.539999999999996) ;
#4035 = CIRCLE('',#16668,0.539999999999996) ;
#4036 = CIRCLE('',#16669,1.4) ;
#4037 = CIRCLE('',#16670,0.539999999999986) ;
#4038 = CIRCLE('',#16672,0.539999999999986) ;
#4039 = CIRCLE('',#16673,1.4) ;
#4040 = CIRCLE('',#16674,0.539999999999996) ;
#4041 = CIRCLE('',#16679,0.539999999999996) ;
#4042 = CIRCLE('',#16680,1.4) ;
#4043 = CIRCLE('',#16681,0.539999999999986) ;
#4044 = CIRCLE('',#16683,0.539999999999986) ;
#4045 = CIRCLE('',#16684,1.4) ;
#4046 = CIRCLE('',#16685,0.539999999999996) ;
#4047 = CIRCLE('',#16690,0.539999999999996) ;
#4048 = CIRCLE('',#16691,1.4) ;
#4049 = CIRCLE('',#16692,0.539999999999986) ;
#4050 = CIRCLE('',#16694,0.539999999999986) ;
#4051 = CIRCLE('',#16695,1.4) ;
#4052 = CIRCLE('',#16696,0.539999999999996) ;
#4053 = CIRCLE('',#16701,0.539999999999996) ;
#4054 = CIRCLE('',#16702,1.4) ;
#4055 = CIRCLE('',#16703,0.539999999999986) ;
#4056 = CIRCLE('',#16705,0.539999999999986) ;
#4057 = CIRCLE('',#16706,1.4) ;
#4058 = CIRCLE('',#16707,0.539999999999996) ;
#4059 = CIRCLE('',#16712,0.539999999999996) ;
#4060 = CIRCLE('',#16713,1.4) ;
#4061 = CIRCLE('',#16714,0.539999999999986) ;
#4062 = CIRCLE('',#16716,0.539999999999986) ;
#4063 = CIRCLE('',#16717,1.4) ;
#4064 = CIRCLE('',#16718,0.539999999999996) ;
#4065 = CIRCLE('',#16723,0.539999999999996) ;
#4066 = CIRCLE('',#16724,1.4) ;
#4067 = CIRCLE('',#16725,0.539999999999986) ;
#4068 = CIRCLE('',#16727,0.539999999999986) ;
#4069 = CIRCLE('',#16728,1.4) ;
#4070 = CIRCLE('',#16729,0.539999999999996) ;
#4071 = CIRCLE('',#16734,0.539999999999996) ;
#4072 = CIRCLE('',#16735,1.4) ;
#4073 = CIRCLE('',#16736,0.539999999999986) ;
#4074 = CIRCLE('',#16738,0.539999999999986) ;
#4075 = CIRCLE('',#16739,1.4) ;
#4076 = CIRCLE('',#16740,0.539999999999996) ;
#4077 = CIRCLE('',#16745,0.539999999999996) ;
#4078 = CIRCLE('',#16746,1.4) ;
#4079 = CIRCLE('',#16747,0.539999999999986) ;
#4080 = CIRCLE('',#16749,0.539999999999986) ;
#4081 = CIRCLE('',#16750,1.4) ;
#4082 = CIRCLE('',#16751,0.539999999999996) ;
#4083 = CIRCLE('',#16756,0.539999999999996) ;
#4084 = CIRCLE('',#16757,1.4) ;
#4085 = CIRCLE('',#16758,0.539999999999986) ;
#4086 = CIRCLE('',#16760,0.539999999999986) ;
#4087 = CIRCLE('',#16761,1.4) ;
#4088 = CIRCLE('',#16762,0.539999999999996) ;
#4089 = CIRCLE('',#16767,0.539999999999996) ;
#4090 = CIRCLE('',#16768,1.4) ;
#4091 = CIRCLE('',#16769,0.539999999999986) ;
#4092 = CIRCLE('',#16771,0.539999999999986) ;
#4093 = CIRCLE('',#16772,1.4) ;
#4094 = CIRCLE('',#16773,0.539999999999996) ;
#4095 = CIRCLE('',#16778,0.539999999999996) ;
#4096 = CIRCLE('',#16779,1.4) ;
#4097 = CIRCLE('',#16780,0.539999999999986) ;
#4098 = CIRCLE('',#16782,0.539999999999986) ;
#4099 = CIRCLE('',#16783,1.4) ;
#4100 = CIRCLE('',#16784,0.539999999999996) ;
#4101 = CIRCLE('',#16789,0.539999999999996) ;
#4102 = CIRCLE('',#16790,1.4) ;
#4103 = CIRCLE('',#16791,0.539999999999986) ;
#4104 = CIRCLE('',#16793,0.539999999999986) ;
#4105 = CIRCLE('',#16794,1.4) ;
#4106 = CIRCLE('',#16795,0.539999999999996) ;
#4107 = CIRCLE('',#16800,0.539999999999996) ;
#4108 = CIRCLE('',#16801,1.4) ;
#4109 = CIRCLE('',#16802,0.539999999999986) ;
#4110 = CIRCLE('',#16804,0.539999999999986) ;
#4111 = CIRCLE('',#16805,1.4) ;
#4112 = CIRCLE('',#16806,0.539999999999996) ;
#4113 = CIRCLE('',#16811,0.539999999999996) ;
#4114 = CIRCLE('',#16812,1.4) ;
#4115 = CIRCLE('',#16813,0.539999999999986) ;
#4116 = CIRCLE('',#16815,0.539999999999986) ;
#4117 = CIRCLE('',#16816,1.4) ;
#4118 = CIRCLE('',#16817,0.539999999999996) ;
#4119 = CIRCLE('',#16822,0.539999999999996) ;
#4120 = CIRCLE('',#16823,1.4) ;
#4121 = CIRCLE('',#16824,0.539999999999986) ;
#4122 = CIRCLE('',#16826,0.539999999999986) ;
#4123 = CIRCLE('',#16827,1.4) ;
#4124 = CIRCLE('',#16828,0.539999999999996) ;
#4125 = CIRCLE('',#16833,0.539999999999996) ;
#4126 = CIRCLE('',#16834,1.4) ;
#4127 = CIRCLE('',#16835,0.539999999999986) ;
#4128 = CIRCLE('',#16837,0.539999999999986) ;
#4129 = CIRCLE('',#16838,1.4) ;
#4130 = CIRCLE('',#16839,0.539999999999996) ;
#4131 = CIRCLE('',#16844,0.539999999999996) ;
#4132 = CIRCLE('',#16845,1.4) ;
#4133 = CIRCLE('',#16846,0.539999999999986) ;
#4134 = CIRCLE('',#16848,0.539999999999986) ;
#4135 = CIRCLE('',#16849,1.4) ;
#4136 = CIRCLE('',#16850,0.539999999999996) ;
#4137 = CIRCLE('',#16855,0.539999999999996) ;
#4138 = CIRCLE('',#16856,1.4) ;
#4139 = CIRCLE('',#16857,0.539999999999986) ;
#4140 = CIRCLE('',#16859,0.539999999999986) ;
#4141 = CIRCLE('',#16860,1.4) ;
#4142 = CIRCLE('',#16861,0.539999999999996) ;
#4143 = CIRCLE('',#16866,0.539999999999996) ;
#4144 = CIRCLE('',#16867,1.4) ;
#4145 = CIRCLE('',#16868,0.539999999999986) ;
#4146 = CIRCLE('',#16870,0.539999999999986) ;
#4147 = CIRCLE('',#16871,1.4) ;
#4148 = CIRCLE('',#16872,0.539999999999996) ;
#4149 = CIRCLE('',#16877,0.539999999999996) ;
#4150 = CIRCLE('',#16878,1.4) ;
#4151 = CIRCLE('',#16879,0.539999999999986) ;
#4152 = CIRCLE('',#16881,0.539999999999986) ;
#4153 = CIRCLE('',#16882,1.4) ;
#4154 = CIRCLE('',#16883,0.539999999999996) ;
#4155 = CIRCLE('',#16888,0.539999999999996) ;
#4156 = CIRCLE('',#16889,1.4) ;
#4157 = CIRCLE('',#16890,0.539999999999986) ;
#4158 = CIRCLE('',#16892,0.539999999999986) ;
#4159 = CIRCLE('',#16893,1.4) ;
#4160 = CIRCLE('',#16894,0.539999999999996) ;
#4161 = CIRCLE('',#16899,0.539999999999996) ;
#4162 = CIRCLE('',#16900,1.4) ;
#4163 = CIRCLE('',#16901,0.539999999999986) ;
#4164 = CIRCLE('',#16903,0.539999999999986) ;
#4165 = CIRCLE('',#16904,1.4) ;
#4166 = CIRCLE('',#16905,0.539999999999996) ;
#4167 = CIRCLE('',#16910,0.539999999999996) ;
#4168 = CIRCLE('',#16911,1.4) ;
#4169 = CIRCLE('',#16912,0.539999999999986) ;
#4170 = CIRCLE('',#16914,0.539999999999986) ;
#4171 = CIRCLE('',#16915,1.4) ;
#4172 = CIRCLE('',#16916,0.539999999999996) ;
#4173 = CIRCLE('',#16921,0.539999999999996) ;
#4174 = CIRCLE('',#16922,1.4) ;
#4175 = CIRCLE('',#16923,0.539999999999986) ;
#4176 = CIRCLE('',#16925,0.539999999999986) ;
#4177 = CIRCLE('',#16926,1.4) ;
#4178 = CIRCLE('',#16927,0.539999999999996) ;
#4179 = CIRCLE('',#16932,0.539999999999996) ;
#4180 = CIRCLE('',#16933,1.4) ;
#4181 = CIRCLE('',#16934,0.539999999999986) ;
#4182 = CIRCLE('',#16936,0.539999999999986) ;
#4183 = CIRCLE('',#16937,1.4) ;
#4184 = CIRCLE('',#16938,0.539999999999996) ;
#4185 = CIRCLE('',#16943,0.539999999999996) ;
#4186 = CIRCLE('',#16944,1.4) ;
#4187 = CIRCLE('',#16945,0.539999999999986) ;
#4188 = CIRCLE('',#16947,0.539999999999986) ;
#4189 = CIRCLE('',#16948,1.4) ;
#4190 = CIRCLE('',#16949,0.539999999999996) ;
#4191 = CIRCLE('',#16954,0.539999999999996) ;
#4192 = CIRCLE('',#16955,1.4) ;
#4193 = CIRCLE('',#16956,0.539999999999986) ;
#4194 = CIRCLE('',#16958,0.539999999999986) ;
#4195 = CIRCLE('',#16959,1.4) ;
#4196 = CIRCLE('',#16960,0.539999999999996) ;
#4197 = CIRCLE('',#16965,0.539999999999996) ;
#4198 = CIRCLE('',#16966,1.4) ;
#4199 = CIRCLE('',#16967,0.539999999999986) ;
#4200 = CIRCLE('',#16969,0.539999999999986) ;
#4201 = CIRCLE('',#16970,1.4) ;
#4202 = CIRCLE('',#16971,0.539999999999996) ;
#4203 = CIRCLE('',#16976,0.539999999999996) ;
#4204 = CIRCLE('',#16977,1.4) ;
#4205 = CIRCLE('',#16978,0.539999999999986) ;
#4206 = CIRCLE('',#16980,0.539999999999986) ;
#4207 = CIRCLE('',#16981,1.4) ;
#4208 = CIRCLE('',#16982,0.539999999999996) ;
#4209 = CIRCLE('',#16987,0.539999999999996) ;
#4210 = CIRCLE('',#16988,1.4) ;
#4211 = CIRCLE('',#16989,0.539999999999986) ;
#4212 = CIRCLE('',#16991,0.539999999999986) ;
#4213 = CIRCLE('',#16992,1.4) ;
#4214 = CIRCLE('',#16993,0.539999999999996) ;
#4215 = CIRCLE('',#16998,0.539999999999996) ;
#4216 = CIRCLE('',#16999,1.4) ;
#4217 = CIRCLE('',#17000,0.539999999999986) ;
#4218 = CIRCLE('',#17002,0.539999999999986) ;
#4219 = CIRCLE('',#17003,1.4) ;
#4220 = CIRCLE('',#17004,0.539999999999996) ;
#4221 = CIRCLE('',#17009,0.539999999999996) ;
#4222 = CIRCLE('',#17010,1.4) ;
#4223 = CIRCLE('',#17011,0.539999999999986) ;
#4224 = CIRCLE('',#17013,0.539999999999986) ;
#4225 = CIRCLE('',#17014,1.4) ;
#4226 = CIRCLE('',#17015,0.539999999999996) ;
#4227 = CIRCLE('',#17020,0.539999999999996) ;
#4228 = CIRCLE('',#17021,1.4) ;
#4229 = CIRCLE('',#17022,0.539999999999986) ;
#4230 = CIRCLE('',#17024,0.539999999999986) ;
#4231 = CIRCLE('',#17025,1.4) ;
#4232 = CIRCLE('',#17026,0.539999999999996) ;
#4233 = CIRCLE('',#17031,0.539999999999996) ;
#4234 = CIRCLE('',#17032,1.4) ;
#4235 = CIRCLE('',#17033,0.539999999999986) ;
#4236 = CIRCLE('',#17035,0.539999999999986) ;
#4237 = CIRCLE('',#17036,1.4) ;
#4238 = CIRCLE('',#17037,0.539999999999996) ;
#4239 = CIRCLE('',#17042,0.539999999999996) ;
#4240 = CIRCLE('',#17043,1.4) ;
#4241 = CIRCLE('',#17044,0.539999999999986) ;
#4242 = CIRCLE('',#17046,0.539999999999986) ;
#4243 = CIRCLE('',#17047,1.4) ;
#4244 = CIRCLE('',#17048,0.539999999999996) ;
#4245 = CIRCLE('',#17053,0.539999999999996) ;
#4246 = CIRCLE('',#17054,1.4) ;
#4247 = CIRCLE('',#17055,0.539999999999986) ;
#4248 = CIRCLE('',#17057,0.539999999999986) ;
#4249 = CIRCLE('',#17058,1.4) ;
#4250 = CIRCLE('',#17059,0.539999999999996) ;
#4251 = CIRCLE('',#17064,0.539999999999996) ;
#4252 = CIRCLE('',#17065,1.4) ;
#4253 = CIRCLE('',#17066,0.539999999999986) ;
#4254 = CIRCLE('',#17068,0.539999999999986) ;
#4255 = CIRCLE('',#17069,1.4) ;
#4256 = CIRCLE('',#17070,0.539999999999996) ;
#4257 = CIRCLE('',#17075,0.539999999999996) ;
#4258 = CIRCLE('',#17076,1.4) ;
#4259 = CIRCLE('',#17077,0.539999999999986) ;
#4260 = CIRCLE('',#17079,0.539999999999986) ;
#4261 = CIRCLE('',#17080,1.4) ;
#4262 = CIRCLE('',#17081,0.539999999999996) ;
#4263 = CIRCLE('',#17086,0.539999999999996) ;
#4264 = CIRCLE('',#17087,1.4) ;
#4265 = CIRCLE('',#17088,0.539999999999986) ;
#4266 = CIRCLE('',#17090,0.539999999999986) ;
#4267 = CIRCLE('',#17091,1.4) ;
#4268 = CIRCLE('',#17092,0.539999999999996) ;
#4269 = CIRCLE('',#17097,0.539999999999996) ;
#4270 = CIRCLE('',#17098,1.4) ;
#4271 = CIRCLE('',#17099,0.539999999999986) ;
#4272 = CIRCLE('',#17101,0.539999999999986) ;
#4273 = CIRCLE('',#17102,1.4) ;
#4274 = CIRCLE('',#17103,0.539999999999996) ;
#4275 = CIRCLE('',#17108,0.539999999999996) ;
#4276 = CIRCLE('',#17109,1.4) ;
#4277 = CIRCLE('',#17110,0.539999999999986) ;
#4278 = CIRCLE('',#17112,0.539999999999986) ;
#4279 = CIRCLE('',#17113,1.4) ;
#4280 = CIRCLE('',#17114,0.539999999999996) ;
#4281 = CIRCLE('',#17119,0.539999999999996) ;
#4282 = CIRCLE('',#17120,1.4) ;
#4283 = CIRCLE('',#17121,0.539999999999986) ;
#4284 = CIRCLE('',#17123,0.539999999999986) ;
#4285 = CIRCLE('',#17124,1.4) ;
#4286 = CIRCLE('',#17125,0.539999999999996) ;
#4287 = CIRCLE('',#17130,0.539999999999996) ;
#4288 = CIRCLE('',#17131,1.4) ;
#4289 = CIRCLE('',#17132,0.539999999999986) ;
#4290 = CIRCLE('',#17134,0.539999999999986) ;
#4291 = CIRCLE('',#17135,1.4) ;
#4292 = CIRCLE('',#17136,0.539999999999996) ;
#4293 = CIRCLE('',#17141,0.539999999999996) ;
#4294 = CIRCLE('',#17142,1.4) ;
#4295 = CIRCLE('',#17143,0.539999999999986) ;
#4296 = CIRCLE('',#17145,0.539999999999986) ;
#4297 = CIRCLE('',#17146,1.4) ;
#4298 = CIRCLE('',#17147,0.539999999999996) ;
#4299 = CIRCLE('',#17152,0.539999999999996) ;
#4300 = CIRCLE('',#17153,1.4) ;
#4301 = CIRCLE('',#17154,0.539999999999986) ;
#4302 = CIRCLE('',#17156,0.539999999999986) ;
#4303 = CIRCLE('',#17157,1.4) ;
#4304 = CIRCLE('',#17158,0.539999999999996) ;
#4305 = CIRCLE('',#17163,0.539999999999996) ;
#4306 = CIRCLE('',#17164,1.4) ;
#4307 = CIRCLE('',#17165,0.539999999999986) ;
#4308 = CIRCLE('',#17167,0.539999999999986) ;
#4309 = CIRCLE('',#17168,1.4) ;
#4310 = CIRCLE('',#17169,0.539999999999996) ;
#4311 = CIRCLE('',#17174,0.539999999999996) ;
#4312 = CIRCLE('',#17175,1.4) ;
#4313 = CIRCLE('',#17176,0.539999999999986) ;
#4314 = CIRCLE('',#17178,0.539999999999986) ;
#4315 = CIRCLE('',#17179,1.4) ;
#4316 = CIRCLE('',#17180,0.539999999999996) ;
#4317 = CIRCLE('',#17185,0.539999999999996) ;
#4318 = CIRCLE('',#17186,1.4) ;
#4319 = CIRCLE('',#17187,0.539999999999986) ;
#4320 = CIRCLE('',#17189,0.539999999999986) ;
#4321 = CIRCLE('',#17190,1.4) ;
#4322 = CIRCLE('',#17191,0.539999999999996) ;
#4323 = CIRCLE('',#17196,0.539999999999996) ;
#4324 = CIRCLE('',#17197,1.4) ;
#4325 = CIRCLE('',#17198,0.539999999999986) ;
#4326 = CIRCLE('',#17200,0.539999999999986) ;
#4327 = CIRCLE('',#17201,1.4) ;
#4328 = CIRCLE('',#17202,0.539999999999996) ;
#4329 = CIRCLE('',#17209,20.) ;
#4330 = CIRCLE('',#17210,20.) ;
#4331 = CIRCLE('',#17211,20.) ;
#4332 = CIRCLE('',#17213,20.5) ;
#4333 = CIRCLE('',#17215,24.5) ;
#4334 = CIRCLE('',#17217,25.) ;
#4335 = CIRCLE('',#17218,25.) ;
#4336 = CIRCLE('',#17220,25.) ;
#4337 = CIRCLE('',#17222,24.5) ;
#4338 = CIRCLE('',#17224,20.5) ;
#4339 = CIRCLE('',#17230,25.) ;
#4340 = CIRCLE('',#17231,25.) ;
#4341 = CIRCLE('',#17233,29.) ;
#4342 = CIRCLE('',#17234,25.) ;
#4343 = CIRCLE('',#17235,29.) ;
#4344 = CIRCLE('',#17236,25.) ;
#4345 = CIRCLE('',#17237,29.) ;
#4346 = CIRCLE('',#17238,25.) ;
#4347 = CIRCLE('',#17239,29.) ;
#4348 = CIRCLE('',#17240,18.7631) ;
#4349 = CIRCLE('',#17242,29.) ;
#4350 = CIRCLE('',#17244,25.) ;
#4351 = CIRCLE('',#17248,25.) ;
#4352 = CIRCLE('',#17250,29.) ;
#4353 = CIRCLE('',#17252,25.) ;
#4354 = CIRCLE('',#17256,25.) ;
#4355 = CIRCLE('',#17258,29.) ;
#4356 = CIRCLE('',#17260,25.) ;
#4357 = CIRCLE('',#17264,25.) ;
#4358 = CIRCLE('',#17266,29.) ;
#4359 = CIRCLE('',#17267,25.) ;
#4360 = CIRCLE('',#17270,18.7631) ;
#4361 = CIRCLE('',#17274,27.7395230264339) ;
#4362 = CIRCLE('',#17275,29.3077933083081) ;
#4363 = CIRCLE('',#17276,29.3077933083081) ;
#4364 = CIRCLE('',#17277,29.3077933083081) ;
#4365 = CIRCLE('',#17278,29.3077933083081) ;
#4366 = CIRCLE('',#17279,29.3077933083081) ;
#4367 = CIRCLE('',#17280,29.3077933083081) ;
#4368 = CIRCLE('',#17281,29.3077933083081) ;
#4369 = CIRCLE('',#17282,29.3077933083081) ;
#4370 = CIRCLE('',#17283,29.3077933083081) ;
#4371 = CIRCLE('',#17284,29.3077933083081) ;
#4372 = CIRCLE('',#17285,29.3077933083081) ;
#4373 = CIRCLE('',#17286,29.3077933083081) ;
#4374 = CIRCLE('',#17287,29.3077933083081) ;
#4375 = CIRCLE('',#17288,29.3077933083081) ;
#4376 = CIRCLE('',#17289,29.3077933083081) ;
#4377 = CIRCLE('',#17290,29.3077933083081) ;
#4378 = CIRCLE('',#17291,29.3077933083081) ;
#4379 = CIRCLE('',#17292,29.3077933083081) ;
#4380 = CIRCLE('',#17293,29.3077933083081) ;
#4381 = CIRCLE('',#17294,29.3077933083081) ;
#4382 = CIRCLE('',#17295,29.3077933083081) ;
#4383 = CIRCLE('',#17296,29.3077933083081) ;
#4384 = CIRCLE('',#17297,29.3077933083081) ;
#4385 = CIRCLE('',#17298,29.3077933083081) ;
#4386 = CIRCLE('',#17299,29.3077933083081) ;
#4387 = CIRCLE('',#17300,29.3077933083081) ;
#4388 = CIRCLE('',#17301,29.3077933083081) ;
#4389 = CIRCLE('',#17302,29.3077933083081) ;
#4390 = CIRCLE('',#17303,29.3077933083081) ;
#4391 = CIRCLE('',#17304,29.3077933083081) ;
#4392 = CIRCLE('',#17305,29.3077933083081) ;
#4393 = CIRCLE('',#17306,29.3077933083081) ;
#4394 = CIRCLE('',#17307,29.3077933083081) ;
#4395 = CIRCLE('',#17308,29.3077933083081) ;
#4396 = CIRCLE('',#17309,29.3077933083081) ;
#4397 = CIRCLE('',#17310,29.3077933083081) ;
#4398 = CIRCLE('',#17311,29.3077933083081) ;
#4399 = CIRCLE('',#17312,29.3077933083081) ;
#4400 = CIRCLE('',#17313,29.3077933083081) ;
#4401 = CIRCLE('',#17314,29.3077933083081) ;
#4402 = CIRCLE('',#17315,29.3077933083081) ;
#4403 = CIRCLE('',#17316,29.3077933083081) ;
#4404 = CIRCLE('',#17317,29.3077933083081) ;
#4405 = CIRCLE('',#17318,29.3077933083081) ;
#4406 = CIRCLE('',#17319,29.3077933083081) ;
#4407 = CIRCLE('',#17320,29.3077933083081) ;
#4408 = CIRCLE('',#17321,29.3077933083081) ;
#4409 = CIRCLE('',#17322,29.3077933083081) ;
#4410 = CIRCLE('',#17323,29.3077933083081) ;
#4411 = CIRCLE('',#17324,29.3077933083081) ;
#4412 = CIRCLE('',#17325,29.3077933083081) ;
#4413 = CIRCLE('',#17326,29.3077933083081) ;
#4414 = CIRCLE('',#17327,29.3077933083081) ;
#4415 = CIRCLE('',#17328,29.3077933083081) ;
#4416 = CIRCLE('',#17329,29.3077933083081) ;
#4417 = CIRCLE('',#17330,29.3077933083081) ;
#4418 = CIRCLE('',#17331,29.3077933083081) ;
#4419 = CIRCLE('',#17332,29.3077933083081) ;
#4420 = CIRCLE('',#17333,29.3077933083081) ;
#4421 = CIRCLE('',#17335,25.5228270063586) ;
#4422 = CIRCLE('',#17337,25.5228270063586) ;
#4423 = CIRCLE('',#17339,25.5228270063586) ;
#4424 = CIRCLE('',#17341,25.5228270063586) ;
#4425 = CIRCLE('',#17343,25.5228270063586) ;
#4426 = CIRCLE('',#17345,25.5228270063586) ;
#4427 = CIRCLE('',#17347,25.5228270063586) ;
#4428 = CIRCLE('',#17349,25.5228270063586) ;
#4429 = CIRCLE('',#17351,25.5228270063586) ;
#4430 = CIRCLE('',#17352,25.5228270063586) ;
#4431 = CIRCLE('',#17354,25.5228270063586) ;
#4432 = CIRCLE('',#17356,25.5228270063586) ;
#4433 = CIRCLE('',#17358,25.5228270063586) ;
#4434 = CIRCLE('',#17360,25.5228270063586) ;
#4435 = CIRCLE('',#17361,25.5228270063586) ;
#4436 = CIRCLE('',#17363,25.5228270063586) ;
#4437 = CIRCLE('',#17365,25.5228270063586) ;
#4438 = CIRCLE('',#17367,25.5228270063586) ;
#4439 = CIRCLE('',#17369,25.5228270063586) ;
#4440 = CIRCLE('',#17371,25.5228270063586) ;
#4441 = CIRCLE('',#17373,25.5228270063586) ;
#4442 = CIRCLE('',#17375,25.5228270063586) ;
#4443 = CIRCLE('',#17377,25.5228270063586) ;
#4444 = CIRCLE('',#17379,25.5228270063586) ;
#4445 = CIRCLE('',#17381,25.5228270063586) ;
#4446 = CIRCLE('',#17383,25.5228270063586) ;
#4447 = CIRCLE('',#17385,25.5228270063586) ;
#4448 = CIRCLE('',#17387,25.5228270063586) ;
#4449 = CIRCLE('',#17389,25.5228270063586) ;
#4450 = CIRCLE('',#17391,25.5228270063586) ;
#4451 = CIRCLE('',#17453,29.3077933083081) ;
#4452 = CIRCLE('',#17455,30.8653235080594) ;
#4453 = CIRCLE('',#17456,34.0685435652414) ;
#4454 = CIRCLE('',#17487,27.082990178354) ;
#4455 = CIRCLE('',#17488,27.082990178354) ;
#4456 = CIRCLE('',#17490,23.5) ;
#4457 = CIRCLE('',#17491,1.) ;
#4458 = CIRCLE('',#17492,22.5) ;
#4459 = CIRCLE('',#17494,36.5) ;
#4460 = CIRCLE('',#17495,1.) ;
#4461 = CIRCLE('',#17496,37.5) ;
#4462 = CIRCLE('',#17498,37.5) ;
#4463 = CIRCLE('',#17499,0.25) ;
#4464 = CIRCLE('',#17500,37.25) ;
#4465 = CIRCLE('',#17502,22.5) ;
#4466 = CIRCLE('',#17504,0.249999999999998) ;
#4467 = CIRCLE('',#17505,22.75) ;
#4468 = CIRCLE('',#17511,2.91746266896347) ;
#4469 = CIRCLE('',#17512,2.91746266896347) ;
#4470 = CIRCLE('',#17514,2.91746266896347) ;
#4471 = CIRCLE('',#17515,2.91746266896347) ;
#4472 = CIRCLE('',#17517,2.91746266896347) ;
#4473 = CIRCLE('',#17518,2.91746266896347) ;
#4474 = CIRCLE('',#17520,2.91746266896347) ;
#4475 = CIRCLE('',#17521,2.91746266896347) ;
#4476 = CIRCLE('',#17523,2.91746266896347) ;
#4477 = CIRCLE('',#17524,2.91746266896347) ;
#4478 = CIRCLE('',#17526,2.91746266896347) ;
#4479 = CIRCLE('',#17527,2.91746266896347) ;
#4480 = CIRCLE('',#17529,2.91746266896347) ;
#4481 = CIRCLE('',#17530,2.91746266896347) ;
#4482 = CIRCLE('',#17532,2.91746266896347) ;
#4483 = CIRCLE('',#17533,2.91746266896347) ;
#4484 = CIRCLE('',#17535,2.91746266896347) ;
#4485 = CIRCLE('',#17536,2.91746266896347) ;
#4486 = CIRCLE('',#17538,2.91746266896347) ;
#4487 = CIRCLE('',#17539,2.91746266896347) ;
#4488 = CIRCLE('',#17541,2.91746266896347) ;
#4489 = CIRCLE('',#17542,2.91746266896347) ;
#4490 = CIRCLE('',#17544,2.91746266896347) ;
#4491 = CIRCLE('',#17545,2.91746266896347) ;
#4492 = CIRCLE('',#17547,2.91746266896347) ;
#4493 = CIRCLE('',#17548,2.91746266896347) ;
#4494 = CIRCLE('',#17550,2.91746266896347) ;
#4495 = CIRCLE('',#17551,2.91746266896347) ;
#4496 = CIRCLE('',#17553,2.91746266896347) ;
#4497 = CIRCLE('',#17554,2.91746266896347) ;
#4498 = CIRCLE('',#17556,2.91746266896347) ;
#4499 = CIRCLE('',#17557,2.91746266896347) ;
#4500 = CIRCLE('',#17559,2.91746266896347) ;
#4501 = CIRCLE('',#17560,2.91746266896347) ;
#4502 = CIRCLE('',#17562,2.91746266896347) ;
#4503 = CIRCLE('',#17563,2.91746266896347) ;
#4504 = CIRCLE('',#17565,2.91746266896347) ;
#4505 = CIRCLE('',#17566,2.91746266896347) ;
#4506 = CIRCLE('',#17568,2.91746266896347) ;
#4507 = CIRCLE('',#17569,2.91746266896347) ;
#4508 = CIRCLE('',#17571,2.91746266896347) ;
#4509 = CIRCLE('',#17572,2.91746266896347) ;
#4510 = CIRCLE('',#17574,2.91746266896347) ;
#4511 = CIRCLE('',#17575,2.91746266896347) ;
#4512 = CIRCLE('',#17577,2.91746266896347) ;
#4513 = CIRCLE('',#17578,2.91746266896347) ;
#4514 = CIRCLE('',#17580,2.91746266896347) ;
#4515 = CIRCLE('',#17581,2.91746266896347) ;
#4516 = CIRCLE('',#17583,2.91746266896347) ;
#4517 = CIRCLE('',#17584,2.91746266896347) ;
#4518 = CIRCLE('',#17586,2.91746266896347) ;
#4519 = CIRCLE('',#17587,2.91746266896347) ;
#4520 = CIRCLE('',#17589,2.91746266896347) ;
#4521 = CIRCLE('',#17590,2.91746266896347) ;
#4522 = CIRCLE('',#17592,2.91746266896347) ;
#4523 = CIRCLE('',#17593,2.91746266896347) ;
#4524 = CIRCLE('',#17596,2.91746266896347) ;
#4525 = CIRCLE('',#17597,2.91746266896347) ;
#4526 = CIRCLE('',#17600,3.17084870199964) ;
#4527 = CIRCLE('',#17601,3.17084870199964) ;
#4528 = CIRCLE('',#17603,3.17084870199964) ;
#4529 = CIRCLE('',#17604,3.17084870199964) ;
#4530 = CIRCLE('',#17607,3.17084870199964) ;
#4531 = CIRCLE('',#17608,3.17084870199964) ;
#4532 = CIRCLE('',#17610,3.17084870199964) ;
#4533 = CIRCLE('',#17611,3.17084870199964) ;
#4534 = CIRCLE('',#17614,3.17084870199964) ;
#4535 = CIRCLE('',#17615,3.17084870199964) ;
#4536 = CIRCLE('',#17617,3.17084870199964) ;
#4537 = CIRCLE('',#17618,3.17084870199964) ;
#4538 = CIRCLE('',#17621,3.17084870199964) ;
#4539 = CIRCLE('',#17622,3.17084870199964) ;
#4540 = CIRCLE('',#17624,3.17084870199964) ;
#4541 = CIRCLE('',#17625,3.17084870199964) ;
#4542 = CIRCLE('',#17628,3.17084870199964) ;
#4543 = CIRCLE('',#17629,3.17084870199964) ;
#4544 = CIRCLE('',#17631,3.17084870199964) ;
#4545 = CIRCLE('',#17632,3.17084870199964) ;
#4546 = CIRCLE('',#17635,3.17084870199964) ;
#4547 = CIRCLE('',#17636,3.17084870199964) ;
#4548 = CIRCLE('',#17638,3.17084870199964) ;
#4549 = CIRCLE('',#17639,3.17084870199964) ;
#4550 = CIRCLE('',#17642,3.17084870199964) ;
#4551 = CIRCLE('',#17643,3.17084870199964) ;
#4552 = CIRCLE('',#17645,3.17084870199964) ;
#4553 = CIRCLE('',#17646,3.17084870199964) ;
#4554 = CIRCLE('',#17649,3.17084870199964) ;
#4555 = CIRCLE('',#17650,3.17084870199964) ;
#4556 = CIRCLE('',#17652,3.17084870199964) ;
#4557 = CIRCLE('',#17653,3.17084870199964) ;
#4558 = CIRCLE('',#17656,3.17084870199964) ;
#4559 = CIRCLE('',#17657,3.17084870199964) ;
#4560 = CIRCLE('',#17659,3.17084870199964) ;
#4561 = CIRCLE('',#17660,3.17084870199964) ;
#4562 = CIRCLE('',#17663,3.17084870199964) ;
#4563 = CIRCLE('',#17664,3.17084870199964) ;
#4564 = CIRCLE('',#17666,3.17084870199964) ;
#4565 = CIRCLE('',#17667,3.17084870199964) ;
#4566 = CIRCLE('',#17670,3.17084870199964) ;
#4567 = CIRCLE('',#17671,3.17084870199964) ;
#4568 = CIRCLE('',#17673,3.17084870199964) ;
#4569 = CIRCLE('',#17674,3.17084870199964) ;
#4570 = CIRCLE('',#17677,3.17084870199964) ;
#4571 = CIRCLE('',#17678,3.17084870199964) ;
#4572 = CIRCLE('',#17680,3.17084870199964) ;
#4573 = CIRCLE('',#17681,3.17084870199964) ;
#4574 = CIRCLE('',#17684,3.17084870199964) ;
#4575 = CIRCLE('',#17685,3.17084870199964) ;
#4576 = CIRCLE('',#17687,3.17084870199964) ;
#4577 = CIRCLE('',#17688,3.17084870199964) ;
#4578 = CIRCLE('',#17691,3.17084870199964) ;
#4579 = CIRCLE('',#17692,3.17084870199964) ;
#4580 = CIRCLE('',#17694,3.17084870199964) ;
#4581 = CIRCLE('',#17695,3.17084870199964) ;
#4582 = CIRCLE('',#17698,3.17084870199964) ;
#4583 = CIRCLE('',#17699,3.17084870199964) ;
#4584 = CIRCLE('',#17701,3.17084870199964) ;
#4585 = CIRCLE('',#17702,3.17084870199964) ;
#4586 = CIRCLE('',#17705,3.17084870199964) ;
#4587 = CIRCLE('',#17706,3.17084870199964) ;
#4588 = CIRCLE('',#17708,3.17084870199964) ;
#4589 = CIRCLE('',#17709,3.17084870199964) ;
#4590 = CIRCLE('',#17712,3.17084870199964) ;
#4591 = CIRCLE('',#17713,3.17084870199964) ;
#4592 = CIRCLE('',#17715,3.17084870199964) ;
#4593 = CIRCLE('',#17716,3.17084870199964) ;
#4594 = CIRCLE('',#17719,3.17084870199964) ;
#4595 = CIRCLE('',#17720,3.17084870199964) ;
#4596 = CIRCLE('',#17722,3.17084870199964) ;
#4597 = CIRCLE('',#17723,3.17084870199964) ;
#4598 = CIRCLE('',#17726,3.17084870199964) ;
#4599 = CIRCLE('',#17727,3.17084870199964) ;
#4600 = CIRCLE('',#17729,3.17084870199964) ;
#4601 = CIRCLE('',#17730,3.17084870199964) ;
#4602 = CIRCLE('',#17733,3.17084870199964) ;
#4603 = CIRCLE('',#17734,3.17084870199964) ;
#4604 = CIRCLE('',#17736,3.17084870199964) ;
#4605 = CIRCLE('',#17737,3.17084870199964) ;
#4606 = CIRCLE('',#17740,3.17084870199964) ;
#4607 = CIRCLE('',#17741,3.17084870199964) ;
#4608 = CIRCLE('',#17743,3.17084870199964) ;
#4609 = CIRCLE('',#17744,3.17084870199964) ;
#4610 = CIRCLE('',#17747,3.17084870199964) ;
#4611 = CIRCLE('',#17748,3.17084870199964) ;
#4612 = CIRCLE('',#17750,3.17084870199964) ;
#4613 = CIRCLE('',#17751,3.17084870199964) ;
#4614 = CIRCLE('',#17754,3.17084870199964) ;
#4615 = CIRCLE('',#17755,3.17084870199964) ;
#4616 = CIRCLE('',#17757,3.17084870199964) ;
#4617 = CIRCLE('',#17758,3.17084870199964) ;
#4618 = CIRCLE('',#17761,3.17084870199964) ;
#4619 = CIRCLE('',#17762,3.17084870199964) ;
#4620 = CIRCLE('',#17764,3.17084870199964) ;
#4621 = CIRCLE('',#17765,3.17084870199964) ;
#4622 = CIRCLE('',#17768,3.17084870199964) ;
#4623 = CIRCLE('',#17769,3.17084870199964) ;
#4624 = CIRCLE('',#17771,3.17084870199964) ;
#4625 = CIRCLE('',#17772,3.17084870199964) ;
#4626 = CIRCLE('',#17775,3.17084870199964) ;
#4627 = CIRCLE('',#17776,3.17084870199964) ;
#4628 = CIRCLE('',#17778,3.17084870199964) ;
#4629 = CIRCLE('',#17779,3.17084870199964) ;
#4630 = CIRCLE('',#17782,3.17084870199964) ;
#4631 = CIRCLE('',#17783,3.17084870199964) ;
#4632 = CIRCLE('',#17785,3.17084870199964) ;
#4633 = CIRCLE('',#17786,3.17084870199964) ;
#4634 = CIRCLE('',#17789,3.17084870199964) ;
#4635 = CIRCLE('',#17790,3.17084870199964) ;
#4636 = CIRCLE('',#17792,3.17084870199964) ;
#4637 = CIRCLE('',#17793,3.17084870199964) ;
#4638 = CIRCLE('',#17796,3.17084870199964) ;
#4639 = CIRCLE('',#17797,3.17084870199964) ;
#4640 = CIRCLE('',#17799,3.17084870199964) ;
#4641 = CIRCLE('',#17800,3.17084870199964) ;
#4642 = CIRCLE('',#17804,36.5) ;
#4643 = CIRCLE('',#17805,36.3) ;
#4644 = CIRCLE('',#17807,22.7) ;
#4645 = CIRCLE('',#17809,36.5) ;
#4646 = CIRCLE('',#17811,22.5) ;
#4647 = CIRCLE('',#17813,22.5) ;
#4648 = CIRCLE('',#17815,36.3) ;
#4649 = CIRCLE('',#17817,22.7) ;
#4650 = CIRCLE('',#17821,3.3) ;
#4651 = CIRCLE('',#17822,3.3) ;
#4652 = CIRCLE('',#17824,3.3) ;
#4653 = CIRCLE('',#17825,3.3) ;
#4654 = CIRCLE('',#17827,3.3) ;
#4655 = CIRCLE('',#17828,3.3) ;
#4656 = CIRCLE('',#17830,3.3) ;
#4657 = CIRCLE('',#17831,3.3) ;
#4658 = CIRCLE('',#17833,3.3) ;
#4659 = CIRCLE('',#17834,3.3) ;
#4660 = CIRCLE('',#17836,3.3) ;
#4661 = CIRCLE('',#17837,3.3) ;
#4662 = CIRCLE('',#17839,3.3) ;
#4663 = CIRCLE('',#17840,3.3) ;
#4664 = CIRCLE('',#17842,3.3) ;
#4665 = CIRCLE('',#17843,3.3) ;
#4666 = CIRCLE('',#17845,33.5) ;
#4667 = CIRCLE('',#17846,33.5) ;
#4668 = CIRCLE('',#17848,50.) ;
#4669 = CIRCLE('',#17849,50.) ;
#4670 = CIRCLE('',#17854,3.3) ;
#4671 = CIRCLE('',#17855,3.3) ;
#4672 = CIRCLE('',#17857,3.3) ;
#4673 = CIRCLE('',#17858,3.3) ;
#4674 = CIRCLE('',#17860,3.3) ;
#4675 = CIRCLE('',#17861,3.3) ;
#4676 = CIRCLE('',#17863,3.3) ;
#4677 = CIRCLE('',#17864,3.3) ;
#4678 = CIRCLE('',#17866,3.3) ;
#4679 = CIRCLE('',#17867,3.3) ;
#4680 = CIRCLE('',#17869,3.3) ;
#4681 = CIRCLE('',#17870,3.3) ;
#4682 = CIRCLE('',#17872,3.3) ;
#4683 = CIRCLE('',#17873,3.3) ;
#4684 = CIRCLE('',#17875,3.3) ;
#4685 = CIRCLE('',#17876,3.3) ;
#4686 = CIRCLE('',#17878,33.5) ;
#4687 = CIRCLE('',#17879,33.5) ;
#4688 = CIRCLE('',#17881,50.) ;
#4689 = CIRCLE('',#17882,50.) ;
#4690 = LINE('',#23017,#5346) ;
#4691 = LINE('',#23022,#5347) ;
#4692 = LINE('',#23026,#5348) ;
#4693 = LINE('',#23031,#5349) ;
#4694 = LINE('',#23035,#5350) ;
#4695 = LINE('',#23040,#5351) ;
#4696 = LINE('',#23044,#5352) ;
#4697 = LINE('',#23049,#5353) ;
#4698 = LINE('',#23058,#5354) ;
#4699 = LINE('',#23061,#5355) ;
#4700 = LINE('',#23071,#5356) ;
#4701 = LINE('',#23074,#5357) ;
#4702 = LINE('',#23084,#5358) ;
#4703 = LINE('',#23087,#5359) ;
#4704 = LINE('',#23097,#5360) ;
#4705 = LINE('',#23100,#5361) ;
#4706 = LINE('',#23105,#5362) ;
#4707 = LINE('',#23110,#5363) ;
#4708 = LINE('',#23114,#5364) ;
#4709 = LINE('',#23119,#5365) ;
#4710 = LINE('',#23123,#5366) ;
#4711 = LINE('',#23128,#5367) ;
#4712 = LINE('',#23132,#5368) ;
#4713 = LINE('',#23137,#5369) ;
#4714 = LINE('',#23141,#5370) ;
#4715 = LINE('',#23146,#5371) ;
#4716 = LINE('',#23150,#5372) ;
#4717 = LINE('',#23155,#5373) ;
#4718 = LINE('',#23159,#5374) ;
#4719 = LINE('',#23164,#5375) ;
#4720 = LINE('',#23168,#5376) ;
#4721 = LINE('',#23173,#5377) ;
#4722 = LINE('',#23178,#5378) ;
#4723 = LINE('',#23183,#5379) ;
#4724 = LINE('',#23185,#5380) ;
#4725 = LINE('',#23187,#5381) ;
#4726 = LINE('',#23188,#5382) ;
#4727 = LINE('',#23191,#5383) ;
#4728 = LINE('',#23193,#5384) ;
#4729 = LINE('',#23194,#5385) ;
#4730 = LINE('',#23197,#5386) ;
#4731 = LINE('',#23199,#5387) ;
#4732 = LINE('',#23200,#5388) ;
#4733 = LINE('',#23202,#5389) ;
#4734 = LINE('',#23203,#5390) ;
#4735 = LINE('',#23215,#5391) ;
#4736 = LINE('',#23218,#5392) ;
#4737 = LINE('',#23228,#5393) ;
#4738 = LINE('',#23231,#5394) ;
#4739 = LINE('',#23241,#5395) ;
#4740 = LINE('',#23244,#5396) ;
#4741 = LINE('',#23254,#5397) ;
#4742 = LINE('',#23257,#5398) ;
#4743 = LINE('',#23267,#5399) ;
#4744 = LINE('',#23270,#5400) ;
#4745 = LINE('',#23280,#5401) ;
#4746 = LINE('',#23283,#5402) ;
#4747 = LINE('',#23293,#5403) ;
#4748 = LINE('',#23296,#5404) ;
#4749 = LINE('',#23306,#5405) ;
#4750 = LINE('',#23309,#5406) ;
#4751 = LINE('',#23319,#5407) ;
#4752 = LINE('',#23322,#5408) ;
#4753 = LINE('',#23332,#5409) ;
#4754 = LINE('',#23335,#5410) ;
#4755 = LINE('',#23345,#5411) ;
#4756 = LINE('',#23348,#5412) ;
#4757 = LINE('',#23358,#5413) ;
#4758 = LINE('',#23361,#5414) ;
#4759 = LINE('',#23366,#5415) ;
#4760 = LINE('',#23368,#5416) ;
#4761 = LINE('',#23370,#5417) ;
#4762 = LINE('',#23371,#5418) ;
#4763 = LINE('',#23374,#5419) ;
#4764 = LINE('',#23376,#5420) ;
#4765 = LINE('',#23377,#5421) ;
#4766 = LINE('',#23380,#5422) ;
#4767 = LINE('',#23382,#5423) ;
#4768 = LINE('',#23383,#5424) ;
#4769 = LINE('',#23385,#5425) ;
#4770 = LINE('',#23386,#5426) ;
#4771 = LINE('',#23393,#5427) ;
#4772 = LINE('',#23398,#5428) ;
#4773 = LINE('',#23402,#5429) ;
#4774 = LINE('',#23407,#5430) ;
#4775 = LINE('',#23411,#5431) ;
#4776 = LINE('',#23416,#5432) ;
#4777 = LINE('',#23420,#5433) ;
#4778 = LINE('',#23425,#5434) ;
#4779 = LINE('',#23429,#5435) ;
#4780 = LINE('',#23433,#5436) ;
#4781 = LINE('',#23438,#5437) ;
#4782 = LINE('',#23442,#5438) ;
#4783 = LINE('',#23447,#5439) ;
#4784 = LINE('',#23449,#5440) ;
#4785 = LINE('',#23451,#5441) ;
#4786 = LINE('',#23452,#5442) ;
#4787 = LINE('',#23456,#5443) ;
#4788 = LINE('',#23461,#5444) ;
#4789 = LINE('',#23465,#5445) ;
#4790 = LINE('',#23470,#5446) ;
#4791 = LINE('',#23474,#5447) ;
#4792 = LINE('',#23475,#5448) ;
#4793 = LINE('',#23476,#5449) ;
#4794 = LINE('',#23479,#5450) ;
#4795 = LINE('',#23480,#5451) ;
#4796 = LINE('',#23483,#5452) ;
#4797 = LINE('',#23484,#5453) ;
#4798 = LINE('',#23486,#5454) ;
#4799 = LINE('',#23492,#5455) ;
#4800 = LINE('',#23497,#5456) ;
#4801 = LINE('',#23501,#5457) ;
#4802 = LINE('',#23506,#5458) ;
#4803 = LINE('',#23510,#5459) ;
#4804 = LINE('',#23515,#5460) ;
#4805 = LINE('',#23519,#5461) ;
#4806 = LINE('',#23524,#5462) ;
#4807 = LINE('',#23528,#5463) ;
#4808 = LINE('',#23533,#5464) ;
#4809 = LINE('',#23537,#5465) ;
#4810 = LINE('',#23542,#5466) ;
#4811 = LINE('',#23550,#5467) ;
#4812 = LINE('',#23555,#5468) ;
#4813 = LINE('',#23563,#5469) ;
#4814 = LINE('',#23568,#5470) ;
#4815 = LINE('',#23576,#5471) ;
#4816 = LINE('',#23581,#5472) ;
#4817 = LINE('',#23589,#5473) ;
#4818 = LINE('',#23594,#5474) ;
#4819 = LINE('',#23598,#5475) ;
#4820 = LINE('',#23602,#5476) ;
#4821 = LINE('',#23607,#5477) ;
#4822 = LINE('',#23611,#5478) ;
#4823 = LINE('',#23616,#5479) ;
#4824 = LINE('',#23620,#5480) ;
#4825 = LINE('',#23625,#5481) ;
#4826 = LINE('',#23629,#5482) ;
#4827 = LINE('',#23634,#5483) ;
#4828 = LINE('',#23638,#5484) ;
#4829 = LINE('',#23643,#5485) ;
#4830 = LINE('',#23647,#5486) ;
#4831 = LINE('',#23652,#5487) ;
#4832 = LINE('',#23656,#5488) ;
#4833 = LINE('',#23661,#5489) ;
#4834 = LINE('',#23665,#5490) ;
#4835 = LINE('',#23671,#5491) ;
#4836 = LINE('',#23676,#5492) ;
#4837 = LINE('',#23678,#5493) ;
#4838 = LINE('',#23680,#5494) ;
#4839 = LINE('',#23681,#5495) ;
#4840 = LINE('',#23684,#5496) ;
#4841 = LINE('',#23686,#5497) ;
#4842 = LINE('',#23687,#5498) ;
#4843 = LINE('',#23690,#5499) ;
#4844 = LINE('',#23692,#5500) ;
#4845 = LINE('',#23693,#5501) ;
#4846 = LINE('',#23695,#5502) ;
#4847 = LINE('',#23696,#5503) ;
#4848 = LINE('',#23703,#5504) ;
#4849 = LINE('',#23708,#5505) ;
#4850 = LINE('',#23712,#5506) ;
#4851 = LINE('',#23717,#5507) ;
#4852 = LINE('',#23721,#5508) ;
#4853 = LINE('',#23726,#5509) ;
#4854 = LINE('',#23730,#5510) ;
#4855 = LINE('',#23735,#5511) ;
#4856 = LINE('',#23739,#5512) ;
#4857 = LINE('',#23744,#5513) ;
#4858 = LINE('',#23748,#5514) ;
#4859 = LINE('',#23753,#5515) ;
#4860 = LINE('',#23757,#5516) ;
#4861 = LINE('',#23759,#5517) ;
#4862 = LINE('',#23761,#5518) ;
#4863 = LINE('',#23762,#5519) ;
#4864 = LINE('',#23766,#5520) ;
#4865 = LINE('',#23770,#5521) ;
#4866 = LINE('',#23775,#5522) ;
#4867 = LINE('',#23779,#5523) ;
#4868 = LINE('',#23784,#5524) ;
#4869 = LINE('',#23785,#5525) ;
#4870 = LINE('',#23786,#5526) ;
#4871 = LINE('',#23789,#5527) ;
#4872 = LINE('',#23790,#5528) ;
#4873 = LINE('',#23793,#5529) ;
#4874 = LINE('',#23794,#5530) ;
#4875 = LINE('',#23796,#5531) ;
#4876 = LINE('',#23802,#5532) ;
#4877 = LINE('',#24013,#5533) ;
#4878 = LINE('',#24711,#5534) ;
#4879 = LINE('',#25409,#5535) ;
#4880 = LINE('',#26239,#5536) ;
#4881 = LINE('',#27007,#5537) ;
#4882 = LINE('',#27737,#5538) ;
#4883 = LINE('',#28443,#5539) ;
#4884 = LINE('',#29111,#5540) ;
#4885 = LINE('',#29813,#5541) ;
#4886 = LINE('',#30599,#5542) ;
#4887 = LINE('',#31377,#5543) ;
#4888 = LINE('',#32055,#5544) ;
#4889 = LINE('',#32747,#5545) ;
#4890 = LINE('',#32836,#5546) ;
#4891 = LINE('',#33146,#5547) ;
#4892 = LINE('',#33462,#5548) ;
#4893 = LINE('',#33776,#5549) ;
#4894 = LINE('',#34460,#5550) ;
#4895 = LINE('',#35156,#5551) ;
#4896 = LINE('',#35839,#5552) ;
#4897 = LINE('',#36016,#5553) ;
#4898 = LINE('',#36316,#5554) ;
#4899 = LINE('',#36616,#5555) ;
#4900 = LINE('',#36906,#5556) ;
#4901 = LINE('',#37206,#5557) ;
#4902 = LINE('',#37512,#5558) ;
#4903 = LINE('',#38595,#5559) ;
#4904 = LINE('',#38599,#5560) ;
#4905 = LINE('',#39387,#5561) ;
#4906 = LINE('',#40182,#5562) ;
#4907 = LINE('',#40872,#5563) ;
#4908 = LINE('',#41620,#5564) ;
#4909 = LINE('',#42336,#5565) ;
#4910 = LINE('',#43028,#5566) ;
#4911 = LINE('',#43888,#5567) ;
#4912 = LINE('',#44572,#5568) ;
#4913 = LINE('',#45321,#5569) ;
#4914 = LINE('',#46025,#5570) ;
#4915 = LINE('',#48143,#5571) ;
#4916 = LINE('',#48152,#5572) ;
#4917 = LINE('',#48157,#5573) ;
#4918 = LINE('',#48161,#5574) ;
#4919 = LINE('',#48168,#5575) ;
#4920 = LINE('',#48173,#5576) ;
#4921 = LINE('',#48177,#5577) ;
#4922 = LINE('',#48198,#5578) ;
#4923 = LINE('',#48225,#5579) ;
#4924 = LINE('',#48230,#5580) ;
#4925 = LINE('',#48238,#5581) ;
#4926 = LINE('',#48245,#5582) ;
#4927 = LINE('',#48251,#5583) ;
#4928 = LINE('',#48255,#5584) ;
#4929 = LINE('',#48265,#5585) ;
#4930 = LINE('',#48269,#5586) ;
#4931 = LINE('',#48420,#5587) ;
#4932 = LINE('',#48425,#5588) ;
#4933 = LINE('',#48539,#5589) ;
#4934 = LINE('',#51824,#5590) ;
#4935 = LINE('',#51826,#5591) ;
#4936 = LINE('',#51827,#5592) ;
#4937 = LINE('',#51831,#5593) ;
#4938 = LINE('',#51834,#5594) ;
#4939 = LINE('',#51835,#5595) ;
#4940 = LINE('',#51842,#5596) ;
#4941 = LINE('',#51847,#5597) ;
#4942 = LINE('',#51849,#5598) ;
#4943 = LINE('',#51853,#5599) ;
#4944 = LINE('',#51860,#5600) ;
#4945 = LINE('',#51865,#5601) ;
#4946 = LINE('',#51875,#5602) ;
#4947 = LINE('',#51883,#5603) ;
#4948 = LINE('',#51887,#5604) ;
#4949 = LINE('',#51889,#5605) ;
#4950 = LINE('',#51890,#5606) ;
#4951 = LINE('',#51894,#5607) ;
#4952 = LINE('',#51906,#5608) ;
#4953 = LINE('',#51907,#5609) ;
#4954 = LINE('',#51909,#5610) ;
#4955 = LINE('',#51910,#5611) ;
#4956 = LINE('',#51912,#5612) ;
#4957 = LINE('',#51913,#5613) ;
#4958 = LINE('',#51923,#5614) ;
#4959 = LINE('',#51931,#5615) ;
#4960 = LINE('',#51935,#5616) ;
#4961 = LINE('',#51938,#5617) ;
#4962 = LINE('',#51942,#5618) ;
#4963 = LINE('',#51948,#5619) ;
#4964 = LINE('',#51953,#5620) ;
#4965 = LINE('',#51955,#5621) ;
#4966 = LINE('',#51957,#5622) ;
#4967 = LINE('',#51958,#5623) ;
#4968 = LINE('',#51961,#5624) ;
#4969 = LINE('',#51963,#5625) ;
#4970 = LINE('',#51964,#5626) ;
#4971 = LINE('',#51968,#5627) ;
#4972 = LINE('',#51969,#5628) ;
#4973 = LINE('',#51970,#5629) ;
#4974 = LINE('',#51978,#5630) ;
#4975 = LINE('',#51982,#5631) ;
#4976 = LINE('',#51989,#5632) ;
#4977 = LINE('',#51992,#5633) ;
#4978 = LINE('',#51998,#5634) ;
#4979 = LINE('',#52001,#5635) ;
#4980 = LINE('',#52007,#5636) ;
#4981 = LINE('',#52010,#5637) ;
#4982 = LINE('',#52014,#5638) ;
#4983 = LINE('',#52018,#5639) ;
#4984 = LINE('',#52023,#5640) ;
#4985 = LINE('',#52027,#5641) ;
#4986 = LINE('',#52032,#5642) ;
#4987 = LINE('',#52036,#5643) ;
#4988 = LINE('',#52043,#5644) ;
#4989 = LINE('',#52046,#5645) ;
#4990 = LINE('',#52052,#5646) ;
#4991 = LINE('',#52055,#5647) ;
#4992 = LINE('',#52061,#5648) ;
#4993 = LINE('',#52064,#5649) ;
#4994 = LINE('',#52070,#5650) ;
#4995 = LINE('',#52073,#5651) ;
#4996 = LINE('',#52079,#5652) ;
#4997 = LINE('',#52082,#5653) ;
#4998 = LINE('',#52088,#5654) ;
#4999 = LINE('',#52091,#5655) ;
#5000 = LINE('',#52097,#5656) ;
#5001 = LINE('',#52100,#5657) ;
#5002 = LINE('',#52106,#5658) ;
#5003 = LINE('',#52109,#5659) ;
#5004 = LINE('',#52115,#5660) ;
#5005 = LINE('',#52118,#5661) ;
#5006 = LINE('',#52124,#5662) ;
#5007 = LINE('',#52127,#5663) ;
#5008 = LINE('',#52133,#5664) ;
#5009 = LINE('',#52136,#5665) ;
#5010 = LINE('',#52142,#5666) ;
#5011 = LINE('',#52145,#5667) ;
#5012 = LINE('',#52151,#5668) ;
#5013 = LINE('',#52154,#5669) ;
#5014 = LINE('',#52158,#5670) ;
#5015 = LINE('',#52162,#5671) ;
#5016 = LINE('',#52169,#5672) ;
#5017 = LINE('',#52172,#5673) ;
#5018 = LINE('',#52178,#5674) ;
#5019 = LINE('',#52181,#5675) ;
#5020 = LINE('',#52187,#5676) ;
#5021 = LINE('',#52190,#5677) ;
#5022 = LINE('',#52196,#5678) ;
#5023 = LINE('',#52199,#5679) ;
#5024 = LINE('',#52205,#5680) ;
#5025 = LINE('',#52208,#5681) ;
#5026 = LINE('',#52214,#5682) ;
#5027 = LINE('',#52217,#5683) ;
#5028 = LINE('',#52223,#5684) ;
#5029 = LINE('',#52226,#5685) ;
#5030 = LINE('',#52232,#5686) ;
#5031 = LINE('',#52235,#5687) ;
#5032 = LINE('',#52241,#5688) ;
#5033 = LINE('',#52244,#5689) ;
#5034 = LINE('',#52250,#5690) ;
#5035 = LINE('',#52253,#5691) ;
#5036 = LINE('',#52259,#5692) ;
#5037 = LINE('',#52262,#5693) ;
#5038 = LINE('',#52266,#5694) ;
#5039 = LINE('',#52270,#5695) ;
#5040 = LINE('',#52275,#5696) ;
#5041 = LINE('',#52279,#5697) ;
#5042 = LINE('',#52284,#5698) ;
#5043 = LINE('',#52288,#5699) ;
#5044 = LINE('',#52293,#5700) ;
#5045 = LINE('',#52297,#5701) ;
#5046 = LINE('',#52302,#5702) ;
#5047 = LINE('',#52306,#5703) ;
#5048 = LINE('',#52311,#5704) ;
#5049 = LINE('',#52315,#5705) ;
#5050 = LINE('',#52320,#5706) ;
#5051 = LINE('',#52324,#5707) ;
#5052 = LINE('',#52331,#5708) ;
#5053 = LINE('',#52334,#5709) ;
#5054 = LINE('',#52340,#5710) ;
#5055 = LINE('',#52343,#5711) ;
#5056 = LINE('',#52349,#5712) ;
#5057 = LINE('',#52352,#5713) ;
#5058 = LINE('',#52358,#5714) ;
#5059 = LINE('',#52361,#5715) ;
#5060 = LINE('',#52367,#5716) ;
#5061 = LINE('',#52370,#5717) ;
#5062 = LINE('',#52376,#5718) ;
#5063 = LINE('',#52379,#5719) ;
#5064 = LINE('',#52385,#5720) ;
#5065 = LINE('',#52388,#5721) ;
#5066 = LINE('',#52394,#5722) ;
#5067 = LINE('',#52397,#5723) ;
#5068 = LINE('',#52403,#5724) ;
#5069 = LINE('',#52406,#5725) ;
#5070 = LINE('',#52412,#5726) ;
#5071 = LINE('',#52415,#5727) ;
#5072 = LINE('',#52421,#5728) ;
#5073 = LINE('',#52424,#5729) ;
#5074 = LINE('',#52428,#5730) ;
#5075 = LINE('',#52432,#5731) ;
#5076 = LINE('',#52439,#5732) ;
#5077 = LINE('',#52442,#5733) ;
#5078 = LINE('',#52448,#5734) ;
#5079 = LINE('',#52451,#5735) ;
#5080 = LINE('',#52457,#5736) ;
#5081 = LINE('',#52460,#5737) ;
#5082 = LINE('',#52466,#5738) ;
#5083 = LINE('',#52469,#5739) ;
#5084 = LINE('',#52475,#5740) ;
#5085 = LINE('',#52478,#5741) ;
#5086 = LINE('',#52484,#5742) ;
#5087 = LINE('',#52487,#5743) ;
#5088 = LINE('',#52493,#5744) ;
#5089 = LINE('',#52496,#5745) ;
#5090 = LINE('',#52500,#5746) ;
#5091 = LINE('',#52504,#5747) ;
#5092 = LINE('',#52511,#5748) ;
#5093 = LINE('',#52514,#5749) ;
#5094 = LINE('',#52518,#5750) ;
#5095 = LINE('',#52524,#5751) ;
#5096 = LINE('',#52533,#5752) ;
#5097 = LINE('',#52536,#5753) ;
#5098 = LINE('',#52604,#5754) ;
#5099 = LINE('',#52668,#5755) ;
#5100 = LINE('',#52675,#5756) ;
#5101 = LINE('',#52682,#5757) ;
#5102 = LINE('',#52689,#5758) ;
#5103 = LINE('',#52705,#5759) ;
#5104 = LINE('',#52707,#5760) ;
#5105 = LINE('',#52722,#5761) ;
#5106 = LINE('',#52724,#5762) ;
#5107 = LINE('',#52739,#5763) ;
#5108 = LINE('',#52741,#5764) ;
#5109 = LINE('',#52756,#5765) ;
#5110 = LINE('',#52758,#5766) ;
#5111 = LINE('',#52773,#5767) ;
#5112 = LINE('',#52775,#5768) ;
#5113 = LINE('',#52790,#5769) ;
#5114 = LINE('',#52792,#5770) ;
#5115 = LINE('',#52807,#5771) ;
#5116 = LINE('',#52809,#5772) ;
#5117 = LINE('',#52824,#5773) ;
#5118 = LINE('',#52826,#5774) ;
#5119 = LINE('',#52841,#5775) ;
#5120 = LINE('',#52843,#5776) ;
#5121 = LINE('',#52858,#5777) ;
#5122 = LINE('',#52860,#5778) ;
#5123 = LINE('',#52875,#5779) ;
#5124 = LINE('',#52877,#5780) ;
#5125 = LINE('',#52892,#5781) ;
#5126 = LINE('',#52894,#5782) ;
#5127 = LINE('',#52909,#5783) ;
#5128 = LINE('',#52911,#5784) ;
#5129 = LINE('',#52926,#5785) ;
#5130 = LINE('',#52928,#5786) ;
#5131 = LINE('',#52943,#5787) ;
#5132 = LINE('',#52945,#5788) ;
#5133 = LINE('',#52960,#5789) ;
#5134 = LINE('',#52962,#5790) ;
#5135 = LINE('',#52977,#5791) ;
#5136 = LINE('',#52979,#5792) ;
#5137 = LINE('',#52994,#5793) ;
#5138 = LINE('',#52996,#5794) ;
#5139 = LINE('',#53011,#5795) ;
#5140 = LINE('',#53013,#5796) ;
#5141 = LINE('',#53028,#5797) ;
#5142 = LINE('',#53030,#5798) ;
#5143 = LINE('',#53045,#5799) ;
#5144 = LINE('',#53047,#5800) ;
#5145 = LINE('',#53062,#5801) ;
#5146 = LINE('',#53064,#5802) ;
#5147 = LINE('',#53079,#5803) ;
#5148 = LINE('',#53081,#5804) ;
#5149 = LINE('',#53096,#5805) ;
#5150 = LINE('',#53098,#5806) ;
#5151 = LINE('',#53113,#5807) ;
#5152 = LINE('',#53115,#5808) ;
#5153 = LINE('',#53130,#5809) ;
#5154 = LINE('',#53132,#5810) ;
#5155 = LINE('',#53147,#5811) ;
#5156 = LINE('',#53149,#5812) ;
#5157 = LINE('',#53164,#5813) ;
#5158 = LINE('',#53166,#5814) ;
#5159 = LINE('',#53181,#5815) ;
#5160 = LINE('',#53183,#5816) ;
#5161 = LINE('',#53198,#5817) ;
#5162 = LINE('',#53200,#5818) ;
#5163 = LINE('',#53215,#5819) ;
#5164 = LINE('',#53217,#5820) ;
#5165 = LINE('',#53232,#5821) ;
#5166 = LINE('',#53234,#5822) ;
#5167 = LINE('',#53249,#5823) ;
#5168 = LINE('',#53251,#5824) ;
#5169 = LINE('',#53266,#5825) ;
#5170 = LINE('',#53268,#5826) ;
#5171 = LINE('',#53283,#5827) ;
#5172 = LINE('',#53285,#5828) ;
#5173 = LINE('',#53300,#5829) ;
#5174 = LINE('',#53302,#5830) ;
#5175 = LINE('',#53317,#5831) ;
#5176 = LINE('',#53319,#5832) ;
#5177 = LINE('',#53334,#5833) ;
#5178 = LINE('',#53336,#5834) ;
#5179 = LINE('',#53351,#5835) ;
#5180 = LINE('',#53353,#5836) ;
#5181 = LINE('',#53368,#5837) ;
#5182 = LINE('',#53370,#5838) ;
#5183 = LINE('',#53385,#5839) ;
#5184 = LINE('',#53387,#5840) ;
#5185 = LINE('',#53402,#5841) ;
#5186 = LINE('',#53404,#5842) ;
#5187 = LINE('',#53419,#5843) ;
#5188 = LINE('',#53421,#5844) ;
#5189 = LINE('',#53436,#5845) ;
#5190 = LINE('',#53438,#5846) ;
#5191 = LINE('',#53453,#5847) ;
#5192 = LINE('',#53455,#5848) ;
#5193 = LINE('',#53470,#5849) ;
#5194 = LINE('',#53472,#5850) ;
#5195 = LINE('',#53487,#5851) ;
#5196 = LINE('',#53489,#5852) ;
#5197 = LINE('',#53504,#5853) ;
#5198 = LINE('',#53506,#5854) ;
#5199 = LINE('',#53521,#5855) ;
#5200 = LINE('',#53523,#5856) ;
#5201 = LINE('',#53538,#5857) ;
#5202 = LINE('',#53540,#5858) ;
#5203 = LINE('',#53555,#5859) ;
#5204 = LINE('',#53557,#5860) ;
#5205 = LINE('',#53572,#5861) ;
#5206 = LINE('',#53574,#5862) ;
#5207 = LINE('',#53589,#5863) ;
#5208 = LINE('',#53591,#5864) ;
#5209 = LINE('',#53606,#5865) ;
#5210 = LINE('',#53608,#5866) ;
#5211 = LINE('',#53623,#5867) ;
#5212 = LINE('',#53625,#5868) ;
#5213 = LINE('',#53640,#5869) ;
#5214 = LINE('',#53642,#5870) ;
#5215 = LINE('',#53657,#5871) ;
#5216 = LINE('',#53659,#5872) ;
#5217 = LINE('',#53674,#5873) ;
#5218 = LINE('',#53676,#5874) ;
#5219 = LINE('',#53691,#5875) ;
#5220 = LINE('',#53693,#5876) ;
#5221 = LINE('',#53708,#5877) ;
#5222 = LINE('',#53710,#5878) ;
#5223 = LINE('',#53720,#5879) ;
#5224 = LINE('',#53724,#5880) ;
#5225 = LINE('',#53733,#5881) ;
#5226 = LINE('',#53737,#5882) ;
#5227 = LINE('',#53741,#5883) ;
#5228 = LINE('',#53747,#5884) ;
#5229 = LINE('',#53756,#5885) ;
#5230 = LINE('',#53758,#5886) ;
#5231 = LINE('',#53759,#5887) ;
#5232 = LINE('',#53767,#5888) ;
#5233 = LINE('',#53769,#5889) ;
#5234 = LINE('',#53770,#5890) ;
#5235 = LINE('',#53778,#5891) ;
#5236 = LINE('',#53782,#5892) ;
#5237 = LINE('',#53786,#5893) ;
#5238 = LINE('',#53790,#5894) ;
#5239 = LINE('',#53794,#5895) ;
#5240 = LINE('',#53798,#5896) ;
#5241 = LINE('',#53805,#5897) ;
#5242 = LINE('',#53818,#5898) ;
#5243 = LINE('',#53819,#5899) ;
#5244 = LINE('',#53821,#5900) ;
#5245 = LINE('',#53827,#5901) ;
#5246 = LINE('',#53840,#5902) ;
#5247 = LINE('',#53841,#5903) ;
#5248 = LINE('',#53843,#5904) ;
#5249 = LINE('',#53849,#5905) ;
#5250 = LINE('',#53862,#5906) ;
#5251 = LINE('',#53863,#5907) ;
#5252 = LINE('',#53865,#5908) ;
#5253 = LINE('',#53876,#5909) ;
#5254 = LINE('',#53882,#5910) ;
#5255 = LINE('',#56612,#5911) ;
#5256 = LINE('',#57803,#5912) ;
#5257 = LINE('',#57807,#5913) ;
#5258 = LINE('',#57809,#5914) ;
#5259 = LINE('',#57813,#5915) ;
#5260 = LINE('',#57815,#5916) ;
#5261 = LINE('',#57819,#5917) ;
#5262 = LINE('',#57821,#5918) ;
#5263 = LINE('',#57825,#5919) ;
#5264 = LINE('',#57827,#5920) ;
#5265 = LINE('',#57831,#5921) ;
#5266 = LINE('',#57833,#5922) ;
#5267 = LINE('',#57837,#5923) ;
#5268 = LINE('',#57839,#5924) ;
#5269 = LINE('',#57843,#5925) ;
#5270 = LINE('',#57845,#5926) ;
#5271 = LINE('',#57849,#5927) ;
#5272 = LINE('',#57851,#5928) ;
#5273 = LINE('',#57855,#5929) ;
#5274 = LINE('',#57857,#5930) ;
#5275 = LINE('',#57861,#5931) ;
#5276 = LINE('',#57863,#5932) ;
#5277 = LINE('',#57867,#5933) ;
#5278 = LINE('',#57869,#5934) ;
#5279 = LINE('',#57873,#5935) ;
#5280 = LINE('',#57875,#5936) ;
#5281 = LINE('',#57879,#5937) ;
#5282 = LINE('',#57881,#5938) ;
#5283 = LINE('',#57885,#5939) ;
#5284 = LINE('',#57887,#5940) ;
#5285 = LINE('',#57891,#5941) ;
#5286 = LINE('',#57893,#5942) ;
#5287 = LINE('',#57897,#5943) ;
#5288 = LINE('',#57899,#5944) ;
#5289 = LINE('',#57903,#5945) ;
#5290 = LINE('',#57905,#5946) ;
#5291 = LINE('',#57909,#5947) ;
#5292 = LINE('',#57911,#5948) ;
#5293 = LINE('',#57915,#5949) ;
#5294 = LINE('',#57917,#5950) ;
#5295 = LINE('',#57921,#5951) ;
#5296 = LINE('',#57923,#5952) ;
#5297 = LINE('',#57927,#5953) ;
#5298 = LINE('',#57929,#5954) ;
#5299 = LINE('',#57933,#5955) ;
#5300 = LINE('',#57935,#5956) ;
#5301 = LINE('',#57939,#5957) ;
#5302 = LINE('',#57941,#5958) ;
#5303 = LINE('',#57945,#5959) ;
#5304 = LINE('',#57947,#5960) ;
#5305 = LINE('',#57951,#5961) ;
#5306 = LINE('',#57953,#5962) ;
#5307 = LINE('',#57957,#5963) ;
#5308 = LINE('',#57959,#5964) ;
#5309 = LINE('',#57963,#5965) ;
#5310 = LINE('',#57965,#5966) ;
#5311 = LINE('',#57969,#5967) ;
#5312 = LINE('',#57971,#5968) ;
#5313 = LINE('',#57975,#5969) ;
#5314 = LINE('',#57977,#5970) ;
#5315 = LINE('',#57983,#5971) ;
#5316 = LINE('',#63291,#5972) ;
#5317 = LINE('',#63313,#5973) ;
#5318 = LINE('',#63320,#5974) ;
#5319 = LINE('',#63413,#5975) ;
#5320 = LINE('',#63622,#5976) ;
#5321 = LINE('',#63630,#5977) ;
#5322 = LINE('',#63634,#5978) ;
#5323 = LINE('',#63637,#5979) ;
#5324 = LINE('',#63641,#5980) ;
#5325 = LINE('',#63647,#5981) ;
#5326 = LINE('',#63653,#5982) ;
#5327 = LINE('',#63659,#5983) ;
#5328 = LINE('',#63665,#5984) ;
#5329 = LINE('',#63671,#5985) ;
#5330 = LINE('',#63677,#5986) ;
#5331 = LINE('',#63683,#5987) ;
#5332 = LINE('',#63689,#5988) ;
#5333 = LINE('',#63695,#5989) ;
#5334 = LINE('',#63701,#5990) ;
#5335 = LINE('',#63707,#5991) ;
#5336 = LINE('',#63716,#5992) ;
#5337 = LINE('',#63722,#5993) ;
#5338 = LINE('',#63728,#5994) ;
#5339 = LINE('',#63734,#5995) ;
#5340 = LINE('',#63740,#5996) ;
#5341 = LINE('',#63746,#5997) ;
#5342 = LINE('',#63752,#5998) ;
#5343 = LINE('',#63758,#5999) ;
#5344 = LINE('',#63764,#6000) ;
#5345 = LINE('',#63770,#6001) ;
#5346 = VECTOR('',#17908,2.42186816158307) ;
#5347 = VECTOR('',#17915,4.263) ;
#5348 = VECTOR('',#17918,2.42186816158307) ;
#5349 = VECTOR('',#17925,4.263) ;
#5350 = VECTOR('',#17928,2.42186816158307) ;
#5351 = VECTOR('',#17935,4.263) ;
#5352 = VECTOR('',#17938,2.42186816158307) ;
#5353 = VECTOR('',#17945,4.263) ;
#5354 = VECTOR('',#17956,9.) ;
#5355 = VECTOR('',#17959,5.5) ;
#5356 = VECTOR('',#17972,9.) ;
#5357 = VECTOR('',#17975,5.5) ;
#5358 = VECTOR('',#17988,9.) ;
#5359 = VECTOR('',#17991,5.5) ;
#5360 = VECTOR('',#18004,9.) ;
#5361 = VECTOR('',#18007,5.5) ;
#5362 = VECTOR('',#18012,1.65) ;
#5363 = VECTOR('',#18019,3.3) ;
#5364 = VECTOR('',#18022,1.44243074893998) ;
#5365 = VECTOR('',#18029,2.5175) ;
#5366 = VECTOR('',#18032,1.44243074893998) ;
#5367 = VECTOR('',#18039,2.5175) ;
#5368 = VECTOR('',#18042,1.44243074893998) ;
#5369 = VECTOR('',#18049,2.5175) ;
#5370 = VECTOR('',#18052,1.44243074893998) ;
#5371 = VECTOR('',#18059,2.5175) ;
#5372 = VECTOR('',#18062,1.44243074893998) ;
#5373 = VECTOR('',#18069,2.5175) ;
#5374 = VECTOR('',#18072,1.44243074893998) ;
#5375 = VECTOR('',#18079,2.5175) ;
#5376 = VECTOR('',#18082,1.65) ;
#5377 = VECTOR('',#18089,3.3) ;
#5378 = VECTOR('',#18094,37.5) ;
#5379 = VECTOR('',#18099,10.) ;
#5380 = VECTOR('',#18100,10.) ;
#5381 = VECTOR('',#18101,10.) ;
#5382 = VECTOR('',#18102,10.) ;
#5383 = VECTOR('',#18105,10.) ;
#5384 = VECTOR('',#18106,10.) ;
#5385 = VECTOR('',#18107,10.) ;
#5386 = VECTOR('',#18110,10.) ;
#5387 = VECTOR('',#18111,10.) ;
#5388 = VECTOR('',#18112,10.) ;
#5389 = VECTOR('',#18115,10.) ;
#5390 = VECTOR('',#18116,10.) ;
#5391 = VECTOR('',#18133,9.) ;
#5392 = VECTOR('',#18136,5.5) ;
#5393 = VECTOR('',#18149,9.) ;
#5394 = VECTOR('',#18152,5.5) ;
#5395 = VECTOR('',#18165,9.) ;
#5396 = VECTOR('',#18168,5.5) ;
#5397 = VECTOR('',#18181,9.) ;
#5398 = VECTOR('',#18184,5.5) ;
#5399 = VECTOR('',#18197,9.) ;
#5400 = VECTOR('',#18200,5.5) ;
#5401 = VECTOR('',#18213,9.) ;
#5402 = VECTOR('',#18216,5.5) ;
#5403 = VECTOR('',#18229,9.) ;
#5404 = VECTOR('',#18232,5.5) ;
#5405 = VECTOR('',#18245,9.) ;
#5406 = VECTOR('',#18248,5.5) ;
#5407 = VECTOR('',#18261,9.) ;
#5408 = VECTOR('',#18264,5.5) ;
#5409 = VECTOR('',#18277,9.) ;
#5410 = VECTOR('',#18280,5.5) ;
#5411 = VECTOR('',#18293,9.) ;
#5412 = VECTOR('',#18296,5.5) ;
#5413 = VECTOR('',#18309,9.) ;
#5414 = VECTOR('',#18312,5.5) ;
#5415 = VECTOR('',#18317,10.) ;
#5416 = VECTOR('',#18318,10.) ;
#5417 = VECTOR('',#18319,10.) ;
#5418 = VECTOR('',#18320,10.) ;
#5419 = VECTOR('',#18323,10.) ;
#5420 = VECTOR('',#18324,10.) ;
#5421 = VECTOR('',#18325,10.) ;
#5422 = VECTOR('',#18328,10.) ;
#5423 = VECTOR('',#18329,10.) ;
#5424 = VECTOR('',#18330,10.) ;
#5425 = VECTOR('',#18333,10.) ;
#5426 = VECTOR('',#18334,10.) ;
#5427 = VECTOR('',#18343,2.42186816158307) ;
#5428 = VECTOR('',#18350,4.263) ;
#5429 = VECTOR('',#18353,2.42186816158307) ;
#5430 = VECTOR('',#18360,4.263) ;
#5431 = VECTOR('',#18363,2.42186816158307) ;
#5432 = VECTOR('',#18370,4.263) ;
#5433 = VECTOR('',#18373,2.42186816158307) ;
#5434 = VECTOR('',#18380,4.263) ;
#5435 = VECTOR('',#18383,2.42186816158307) ;
#5436 = VECTOR('',#18388,4.263) ;
#5437 = VECTOR('',#18393,2.42186816158307) ;
#5438 = VECTOR('',#18398,4.263) ;
#5439 = VECTOR('',#18403,10.) ;
#5440 = VECTOR('',#18404,10.) ;
#5441 = VECTOR('',#18405,10.) ;
#5442 = VECTOR('',#18406,10.) ;
#5443 = VECTOR('',#18409,2.42186816158307) ;
#5444 = VECTOR('',#18416,4.263) ;
#5445 = VECTOR('',#18419,2.42186816158307) ;
#5446 = VECTOR('',#18426,4.263) ;
#5447 = VECTOR('',#18429,10.) ;
#5448 = VECTOR('',#18430,10.) ;
#5449 = VECTOR('',#18431,10.) ;
#5450 = VECTOR('',#18434,10.) ;
#5451 = VECTOR('',#18435,10.) ;
#5452 = VECTOR('',#18438,10.) ;
#5453 = VECTOR('',#18439,10.) ;
#5454 = VECTOR('',#18442,10.) ;
#5455 = VECTOR('',#18449,1.20708774962173) ;
#5456 = VECTOR('',#18456,2.117) ;
#5457 = VECTOR('',#18459,1.20708774962173) ;
#5458 = VECTOR('',#18466,2.117) ;
#5459 = VECTOR('',#18469,2.42186816158307) ;
#5460 = VECTOR('',#18476,4.263) ;
#5461 = VECTOR('',#18479,2.42186816158307) ;
#5462 = VECTOR('',#18486,4.263) ;
#5463 = VECTOR('',#18489,2.42186816158307) ;
#5464 = VECTOR('',#18496,4.263) ;
#5465 = VECTOR('',#18499,2.42186816158307) ;
#5466 = VECTOR('',#18506,4.263) ;
#5467 = VECTOR('',#18515,9.) ;
#5468 = VECTOR('',#18522,5.5) ;
#5469 = VECTOR('',#18531,9.) ;
#5470 = VECTOR('',#18538,5.5) ;
#5471 = VECTOR('',#18547,9.) ;
#5472 = VECTOR('',#18554,5.5) ;
#5473 = VECTOR('',#18563,9.) ;
#5474 = VECTOR('',#18570,5.5) ;
#5475 = VECTOR('',#18573,1.65) ;
#5476 = VECTOR('',#18578,3.3) ;
#5477 = VECTOR('',#18583,1.44243074893998) ;
#5478 = VECTOR('',#18588,2.5175) ;
#5479 = VECTOR('',#18593,1.44243074893998) ;
#5480 = VECTOR('',#18598,2.5175) ;
#5481 = VECTOR('',#18603,1.44243074893998) ;
#5482 = VECTOR('',#18608,2.5175) ;
#5483 = VECTOR('',#18613,1.44243074893998) ;
#5484 = VECTOR('',#18618,2.5175) ;
#5485 = VECTOR('',#18623,1.44243074893998) ;
#5486 = VECTOR('',#18628,2.5175) ;
#5487 = VECTOR('',#18633,1.44243074893998) ;
#5488 = VECTOR('',#18638,2.5175) ;
#5489 = VECTOR('',#18643,1.65) ;
#5490 = VECTOR('',#18648,3.3) ;
#5491 = VECTOR('',#18655,37.5) ;
#5492 = VECTOR('',#18660,10.) ;
#5493 = VECTOR('',#18661,10.) ;
#5494 = VECTOR('',#18662,10.) ;
#5495 = VECTOR('',#18663,10.) ;
#5496 = VECTOR('',#18666,10.) ;
#5497 = VECTOR('',#18667,10.) ;
#5498 = VECTOR('',#18668,10.) ;
#5499 = VECTOR('',#18671,10.) ;
#5500 = VECTOR('',#18672,10.) ;
#5501 = VECTOR('',#18673,10.) ;
#5502 = VECTOR('',#18676,10.) ;
#5503 = VECTOR('',#18677,10.) ;
#5504 = VECTOR('',#18686,2.42186816158307) ;
#5505 = VECTOR('',#18693,4.263) ;
#5506 = VECTOR('',#18696,2.42186816158307) ;
#5507 = VECTOR('',#18703,4.263) ;
#5508 = VECTOR('',#18706,2.42186816158307) ;
#5509 = VECTOR('',#18713,4.263) ;
#5510 = VECTOR('',#18716,2.42186816158307) ;
#5511 = VECTOR('',#18723,4.263) ;
#5512 = VECTOR('',#18726,2.42186816158307) ;
#5513 = VECTOR('',#18733,4.263) ;
#5514 = VECTOR('',#18736,2.42186816158307) ;
#5515 = VECTOR('',#18743,4.263) ;
#5516 = VECTOR('',#18746,10.) ;
#5517 = VECTOR('',#18747,10.) ;
#5518 = VECTOR('',#18748,10.) ;
#5519 = VECTOR('',#18749,10.) ;
#5520 = VECTOR('',#18752,2.42186816158307) ;
#5521 = VECTOR('',#18757,4.263) ;
#5522 = VECTOR('',#18762,2.42186816158307) ;
#5523 = VECTOR('',#18767,4.263) ;
#5524 = VECTOR('',#18772,10.) ;
#5525 = VECTOR('',#18773,10.) ;
#5526 = VECTOR('',#18774,10.) ;
#5527 = VECTOR('',#18777,10.) ;
#5528 = VECTOR('',#18778,10.) ;
#5529 = VECTOR('',#18781,10.) ;
#5530 = VECTOR('',#18782,10.) ;
#5531 = VECTOR('',#18785,10.) ;
#5532 = VECTOR('',#18792,19.425) ;
#5533 = VECTOR('',#18797,19.425) ;
#5534 = VECTOR('',#18800,19.425) ;
#5535 = VECTOR('',#18803,19.425) ;
#5536 = VECTOR('',#18806,19.425) ;
#5537 = VECTOR('',#18809,19.425) ;
#5538 = VECTOR('',#18812,19.425) ;
#5539 = VECTOR('',#18815,19.425) ;
#5540 = VECTOR('',#18818,19.425) ;
#5541 = VECTOR('',#18821,19.425) ;
#5542 = VECTOR('',#18824,19.425) ;
#5543 = VECTOR('',#18827,19.425) ;
#5544 = VECTOR('',#18830,19.425) ;
#5545 = VECTOR('',#18833,22.12975) ;
#5546 = VECTOR('',#18838,22.12975) ;
#5547 = VECTOR('',#18841,22.12975) ;
#5548 = VECTOR('',#18844,22.12975) ;
#5549 = VECTOR('',#18847,22.12975) ;
#5550 = VECTOR('',#18850,22.12975) ;
#5551 = VECTOR('',#18853,22.12975) ;
#5552 = VECTOR('',#18858,20.33524) ;
#5553 = VECTOR('',#18863,20.33524) ;
#5554 = VECTOR('',#18866,20.33524) ;
#5555 = VECTOR('',#18869,20.33524) ;
#5556 = VECTOR('',#18872,20.33524) ;
#5557 = VECTOR('',#18875,20.33524) ;
#5558 = VECTOR('',#18878,18.56595) ;
#5559 = VECTOR('',#18883,18.56595) ;
#5560 = VECTOR('',#18886,18.56595) ;
#5561 = VECTOR('',#18889,18.56595) ;
#5562 = VECTOR('',#18892,18.56595) ;
#5563 = VECTOR('',#18895,18.56595) ;
#5564 = VECTOR('',#18898,18.56595) ;
#5565 = VECTOR('',#18901,18.56595) ;
#5566 = VECTOR('',#18904,18.56595) ;
#5567 = VECTOR('',#18907,18.56595) ;
#5568 = VECTOR('',#18910,18.56595) ;
#5569 = VECTOR('',#18913,18.56595) ;
#5570 = VECTOR('',#18916,18.56595) ;
#5571 = VECTOR('',#18937,13.3250000000001) ;
#5572 = VECTOR('',#18950,13.2000000000001) ;
#5573 = VECTOR('',#18955,17.375) ;
#5574 = VECTOR('',#18960,17.5) ;
#5575 = VECTOR('',#18967,19.8749999999998) ;
#5576 = VECTOR('',#18974,19.9999999999999) ;
#5577 = VECTOR('',#18977,10.) ;
#5578 = VECTOR('',#18978,10.) ;
#5579 = VECTOR('',#18987,22.375) ;
#5580 = VECTOR('',#18994,22.5) ;
#5581 = VECTOR('',#19003,33.3824824663842) ;
#5582 = VECTOR('',#19012,33.5) ;
#5583 = VECTOR('',#19019,26.7825) ;
#5584 = VECTOR('',#19024,33.375) ;
#5585 = VECTOR('',#19035,15.7556101392397) ;
#5586 = VECTOR('',#19042,14.41685) ;
#5587 = VECTOR('',#19049,33.375) ;
#5588 = VECTOR('',#19056,33.5) ;
#5589 = VECTOR('',#19067,33.375) ;
#5590 = VECTOR('',#19088,10.) ;
#5591 = VECTOR('',#19089,10.) ;
#5592 = VECTOR('',#19090,10.) ;
#5593 = VECTOR('',#19095,10.) ;
#5594 = VECTOR('',#19098,10.) ;
#5595 = VECTOR('',#19099,10.) ;
#5596 = VECTOR('',#19110,20.065) ;
#5597 = VECTOR('',#19117,23.) ;
#5598 = VECTOR('',#19120,20.065) ;
#5599 = VECTOR('',#19125,22.5) ;
#5600 = VECTOR('',#19134,22.25) ;
#5601 = VECTOR('',#19141,18.) ;
#5602 = VECTOR('',#19152,1000.) ;
#5603 = VECTOR('',#19159,1000.) ;
#5604 = VECTOR('',#19164,1000.) ;
#5605 = VECTOR('',#19165,1000.) ;
#5606 = VECTOR('',#19166,1000.) ;
#5607 = VECTOR('',#19169,1000.) ;
#5608 = VECTOR('',#19184,1000.) ;
#5609 = VECTOR('',#19185,1000.) ;
#5610 = VECTOR('',#19188,1000.) ;
#5611 = VECTOR('',#19189,1000.) ;
#5612 = VECTOR('',#19192,1000.) ;
#5613 = VECTOR('',#19193,1000.) ;
#5614 = VECTOR('',#19208,26.9) ;
#5615 = VECTOR('',#19219,27.) ;
#5616 = VECTOR('',#19224,22.6) ;
#5617 = VECTOR('',#19227,22.5) ;
#5618 = VECTOR('',#19232,26.9) ;
#5619 = VECTOR('',#19241,22.6) ;
#5620 = VECTOR('',#19246,10.) ;
#5621 = VECTOR('',#19247,10.) ;
#5622 = VECTOR('',#19248,10.) ;
#5623 = VECTOR('',#19249,10.) ;
#5624 = VECTOR('',#19252,10.) ;
#5625 = VECTOR('',#19253,10.) ;
#5626 = VECTOR('',#19254,10.) ;
#5627 = VECTOR('',#19257,10.) ;
#5628 = VECTOR('',#19258,10.) ;
#5629 = VECTOR('',#19259,10.) ;
#5630 = VECTOR('',#19268,1000.) ;
#5631 = VECTOR('',#19271,1000.) ;
#5632 = VECTOR('',#19278,1000.) ;
#5633 = VECTOR('',#19281,1000.) ;
#5634 = VECTOR('',#19286,1000.) ;
#5635 = VECTOR('',#19289,1000.) ;
#5636 = VECTOR('',#19294,1000.) ;
#5637 = VECTOR('',#19297,1000.) ;
#5638 = VECTOR('',#19300,1000.) ;
#5639 = VECTOR('',#19303,1000.) ;
#5640 = VECTOR('',#19308,1000.) ;
#5641 = VECTOR('',#19311,1000.) ;
#5642 = VECTOR('',#19316,1000.) ;
#5643 = VECTOR('',#19319,1000.) ;
#5644 = VECTOR('',#19326,1000.) ;
#5645 = VECTOR('',#19329,1000.) ;
#5646 = VECTOR('',#19334,1000.) ;
#5647 = VECTOR('',#19337,1000.) ;
#5648 = VECTOR('',#19342,1000.) ;
#5649 = VECTOR('',#19345,1000.) ;
#5650 = VECTOR('',#19350,1000.) ;
#5651 = VECTOR('',#19353,1000.) ;
#5652 = VECTOR('',#19358,1000.) ;
#5653 = VECTOR('',#19361,1000.) ;
#5654 = VECTOR('',#19366,1000.) ;
#5655 = VECTOR('',#19369,1000.) ;
#5656 = VECTOR('',#19374,1000.) ;
#5657 = VECTOR('',#19377,1000.) ;
#5658 = VECTOR('',#19382,1000.) ;
#5659 = VECTOR('',#19385,1000.) ;
#5660 = VECTOR('',#19390,1000.) ;
#5661 = VECTOR('',#19393,1000.) ;
#5662 = VECTOR('',#19398,1000.) ;
#5663 = VECTOR('',#19401,1000.) ;
#5664 = VECTOR('',#19406,1000.) ;
#5665 = VECTOR('',#19409,1000.) ;
#5666 = VECTOR('',#19414,1000.) ;
#5667 = VECTOR('',#19417,1000.) ;
#5668 = VECTOR('',#19422,1000.) ;
#5669 = VECTOR('',#19425,1000.) ;
#5670 = VECTOR('',#19428,1000.) ;
#5671 = VECTOR('',#19431,1000.) ;
#5672 = VECTOR('',#19438,1000.) ;
#5673 = VECTOR('',#19441,1000.) ;
#5674 = VECTOR('',#19446,1000.) ;
#5675 = VECTOR('',#19449,1000.) ;
#5676 = VECTOR('',#19454,1000.) ;
#5677 = VECTOR('',#19457,1000.) ;
#5678 = VECTOR('',#19462,1000.) ;
#5679 = VECTOR('',#19465,1000.) ;
#5680 = VECTOR('',#19470,1000.) ;
#5681 = VECTOR('',#19473,1000.) ;
#5682 = VECTOR('',#19478,1000.) ;
#5683 = VECTOR('',#19481,1000.) ;
#5684 = VECTOR('',#19486,1000.) ;
#5685 = VECTOR('',#19489,1000.) ;
#5686 = VECTOR('',#19494,1000.) ;
#5687 = VECTOR('',#19497,1000.) ;
#5688 = VECTOR('',#19502,1000.) ;
#5689 = VECTOR('',#19505,1000.) ;
#5690 = VECTOR('',#19510,1000.) ;
#5691 = VECTOR('',#19513,1000.) ;
#5692 = VECTOR('',#19518,1000.) ;
#5693 = VECTOR('',#19521,1000.) ;
#5694 = VECTOR('',#19524,1000.) ;
#5695 = VECTOR('',#19527,1000.) ;
#5696 = VECTOR('',#19532,1000.) ;
#5697 = VECTOR('',#19535,1000.) ;
#5698 = VECTOR('',#19540,1000.) ;
#5699 = VECTOR('',#19543,1000.) ;
#5700 = VECTOR('',#19548,1000.) ;
#5701 = VECTOR('',#19551,1000.) ;
#5702 = VECTOR('',#19556,1000.) ;
#5703 = VECTOR('',#19559,1000.) ;
#5704 = VECTOR('',#19564,1000.) ;
#5705 = VECTOR('',#19567,1000.) ;
#5706 = VECTOR('',#19572,1000.) ;
#5707 = VECTOR('',#19575,1000.) ;
#5708 = VECTOR('',#19582,1000.) ;
#5709 = VECTOR('',#19585,1000.) ;
#5710 = VECTOR('',#19590,1000.) ;
#5711 = VECTOR('',#19593,1000.) ;
#5712 = VECTOR('',#19598,1000.) ;
#5713 = VECTOR('',#19601,1000.) ;
#5714 = VECTOR('',#19606,1000.) ;
#5715 = VECTOR('',#19609,1000.) ;
#5716 = VECTOR('',#19614,1000.) ;
#5717 = VECTOR('',#19617,1000.) ;
#5718 = VECTOR('',#19622,1000.) ;
#5719 = VECTOR('',#19625,1000.) ;
#5720 = VECTOR('',#19630,1000.) ;
#5721 = VECTOR('',#19633,1000.) ;
#5722 = VECTOR('',#19638,1000.) ;
#5723 = VECTOR('',#19641,1000.) ;
#5724 = VECTOR('',#19646,1000.) ;
#5725 = VECTOR('',#19649,1000.) ;
#5726 = VECTOR('',#19654,1000.) ;
#5727 = VECTOR('',#19657,1000.) ;
#5728 = VECTOR('',#19662,1000.) ;
#5729 = VECTOR('',#19665,1000.) ;
#5730 = VECTOR('',#19668,1000.) ;
#5731 = VECTOR('',#19671,1000.) ;
#5732 = VECTOR('',#19678,1000.) ;
#5733 = VECTOR('',#19681,1000.) ;
#5734 = VECTOR('',#19686,1000.) ;
#5735 = VECTOR('',#19689,1000.) ;
#5736 = VECTOR('',#19694,1000.) ;
#5737 = VECTOR('',#19697,1000.) ;
#5738 = VECTOR('',#19702,1000.) ;
#5739 = VECTOR('',#19705,1000.) ;
#5740 = VECTOR('',#19710,1000.) ;
#5741 = VECTOR('',#19713,1000.) ;
#5742 = VECTOR('',#19718,1000.) ;
#5743 = VECTOR('',#19721,1000.) ;
#5744 = VECTOR('',#19726,1000.) ;
#5745 = VECTOR('',#19729,1000.) ;
#5746 = VECTOR('',#19732,1000.) ;
#5747 = VECTOR('',#19735,1000.) ;
#5748 = VECTOR('',#19742,1000.) ;
#5749 = VECTOR('',#19745,1000.) ;
#5750 = VECTOR('',#19750,40.) ;
#5751 = VECTOR('',#19757,47.0433475024125) ;
#5752 = VECTOR('',#19768,49.2411809548974) ;
#5753 = VECTOR('',#19771,49.5) ;
#5754 = VECTOR('',#19900,47.175) ;
#5755 = VECTOR('',#20025,49.5) ;
#5756 = VECTOR('',#20034,49.2411809548975) ;
#5757 = VECTOR('',#20043,40.) ;
#5758 = VECTOR('',#20052,37.5) ;
#5759 = VECTOR('',#20075,1000.) ;
#5760 = VECTOR('',#20078,1000.) ;
#5761 = VECTOR('',#20099,1000.) ;
#5762 = VECTOR('',#20102,1000.) ;
#5763 = VECTOR('',#20123,1000.) ;
#5764 = VECTOR('',#20126,1000.) ;
#5765 = VECTOR('',#20147,1000.) ;
#5766 = VECTOR('',#20150,1000.) ;
#5767 = VECTOR('',#20171,1000.) ;
#5768 = VECTOR('',#20174,1000.) ;
#5769 = VECTOR('',#20195,1000.) ;
#5770 = VECTOR('',#20198,1000.) ;
#5771 = VECTOR('',#20219,1000.) ;
#5772 = VECTOR('',#20222,1000.) ;
#5773 = VECTOR('',#20243,1000.) ;
#5774 = VECTOR('',#20246,1000.) ;
#5775 = VECTOR('',#20267,1000.) ;
#5776 = VECTOR('',#20270,1000.) ;
#5777 = VECTOR('',#20291,1000.) ;
#5778 = VECTOR('',#20294,1000.) ;
#5779 = VECTOR('',#20315,1000.) ;
#5780 = VECTOR('',#20318,1000.) ;
#5781 = VECTOR('',#20339,1000.) ;
#5782 = VECTOR('',#20342,1000.) ;
#5783 = VECTOR('',#20363,1000.) ;
#5784 = VECTOR('',#20366,1000.) ;
#5785 = VECTOR('',#20387,1000.) ;
#5786 = VECTOR('',#20390,1000.) ;
#5787 = VECTOR('',#20411,1000.) ;
#5788 = VECTOR('',#20414,1000.) ;
#5789 = VECTOR('',#20435,1000.) ;
#5790 = VECTOR('',#20438,1000.) ;
#5791 = VECTOR('',#20459,1000.) ;
#5792 = VECTOR('',#20462,1000.) ;
#5793 = VECTOR('',#20483,1000.) ;
#5794 = VECTOR('',#20486,1000.) ;
#5795 = VECTOR('',#20507,1000.) ;
#5796 = VECTOR('',#20510,1000.) ;
#5797 = VECTOR('',#20531,1000.) ;
#5798 = VECTOR('',#20534,1000.) ;
#5799 = VECTOR('',#20555,1000.) ;
#5800 = VECTOR('',#20558,1000.) ;
#5801 = VECTOR('',#20579,1000.) ;
#5802 = VECTOR('',#20582,1000.) ;
#5803 = VECTOR('',#20603,1000.) ;
#5804 = VECTOR('',#20606,1000.) ;
#5805 = VECTOR('',#20627,1000.) ;
#5806 = VECTOR('',#20630,1000.) ;
#5807 = VECTOR('',#20651,1000.) ;
#5808 = VECTOR('',#20654,1000.) ;
#5809 = VECTOR('',#20675,1000.) ;
#5810 = VECTOR('',#20678,1000.) ;
#5811 = VECTOR('',#20699,1000.) ;
#5812 = VECTOR('',#20702,1000.) ;
#5813 = VECTOR('',#20723,1000.) ;
#5814 = VECTOR('',#20726,1000.) ;
#5815 = VECTOR('',#20747,1000.) ;
#5816 = VECTOR('',#20750,1000.) ;
#5817 = VECTOR('',#20771,1000.) ;
#5818 = VECTOR('',#20774,1000.) ;
#5819 = VECTOR('',#20795,1000.) ;
#5820 = VECTOR('',#20798,1000.) ;
#5821 = VECTOR('',#20819,1000.) ;
#5822 = VECTOR('',#20822,1000.) ;
#5823 = VECTOR('',#20843,1000.) ;
#5824 = VECTOR('',#20846,1000.) ;
#5825 = VECTOR('',#20867,1000.) ;
#5826 = VECTOR('',#20870,1000.) ;
#5827 = VECTOR('',#20891,1000.) ;
#5828 = VECTOR('',#20894,1000.) ;
#5829 = VECTOR('',#20915,1000.) ;
#5830 = VECTOR('',#20918,1000.) ;
#5831 = VECTOR('',#20939,1000.) ;
#5832 = VECTOR('',#20942,1000.) ;
#5833 = VECTOR('',#20963,1000.) ;
#5834 = VECTOR('',#20966,1000.) ;
#5835 = VECTOR('',#20987,1000.) ;
#5836 = VECTOR('',#20990,1000.) ;
#5837 = VECTOR('',#21011,1000.) ;
#5838 = VECTOR('',#21014,1000.) ;
#5839 = VECTOR('',#21035,1000.) ;
#5840 = VECTOR('',#21038,1000.) ;
#5841 = VECTOR('',#21059,1000.) ;
#5842 = VECTOR('',#21062,1000.) ;
#5843 = VECTOR('',#21083,1000.) ;
#5844 = VECTOR('',#21086,1000.) ;
#5845 = VECTOR('',#21107,1000.) ;
#5846 = VECTOR('',#21110,1000.) ;
#5847 = VECTOR('',#21131,1000.) ;
#5848 = VECTOR('',#21134,1000.) ;
#5849 = VECTOR('',#21155,1000.) ;
#5850 = VECTOR('',#21158,1000.) ;
#5851 = VECTOR('',#21179,1000.) ;
#5852 = VECTOR('',#21182,1000.) ;
#5853 = VECTOR('',#21203,1000.) ;
#5854 = VECTOR('',#21206,1000.) ;
#5855 = VECTOR('',#21227,1000.) ;
#5856 = VECTOR('',#21230,1000.) ;
#5857 = VECTOR('',#21251,1000.) ;
#5858 = VECTOR('',#21254,1000.) ;
#5859 = VECTOR('',#21275,1000.) ;
#5860 = VECTOR('',#21278,1000.) ;
#5861 = VECTOR('',#21299,1000.) ;
#5862 = VECTOR('',#21302,1000.) ;
#5863 = VECTOR('',#21323,1000.) ;
#5864 = VECTOR('',#21326,1000.) ;
#5865 = VECTOR('',#21347,1000.) ;
#5866 = VECTOR('',#21350,1000.) ;
#5867 = VECTOR('',#21371,1000.) ;
#5868 = VECTOR('',#21374,1000.) ;
#5869 = VECTOR('',#21395,1000.) ;
#5870 = VECTOR('',#21398,1000.) ;
#5871 = VECTOR('',#21419,1000.) ;
#5872 = VECTOR('',#21422,1000.) ;
#5873 = VECTOR('',#21443,1000.) ;
#5874 = VECTOR('',#21446,1000.) ;
#5875 = VECTOR('',#21467,1000.) ;
#5876 = VECTOR('',#21470,1000.) ;
#5877 = VECTOR('',#21491,1000.) ;
#5878 = VECTOR('',#21494,1000.) ;
#5879 = VECTOR('',#21507,20.) ;
#5880 = VECTOR('',#21512,20.) ;
#5881 = VECTOR('',#21523,24.5) ;
#5882 = VECTOR('',#21528,25.) ;
#5883 = VECTOR('',#21533,25.) ;
#5884 = VECTOR('',#21542,20.5) ;
#5885 = VECTOR('',#21547,10.) ;
#5886 = VECTOR('',#21548,10.) ;
#5887 = VECTOR('',#21549,10.) ;
#5888 = VECTOR('',#21552,10.) ;
#5889 = VECTOR('',#21553,10.) ;
#5890 = VECTOR('',#21554,10.) ;
#5891 = VECTOR('',#21565,10.) ;
#5892 = VECTOR('',#21568,10.) ;
#5893 = VECTOR('',#21571,10.) ;
#5894 = VECTOR('',#21574,10.) ;
#5895 = VECTOR('',#21577,10.) ;
#5896 = VECTOR('',#21580,10.) ;
#5897 = VECTOR('',#21589,10.) ;
#5898 = VECTOR('',#21596,10.) ;
#5899 = VECTOR('',#21597,10.) ;
#5900 = VECTOR('',#21600,10.) ;
#5901 = VECTOR('',#21609,10.) ;
#5902 = VECTOR('',#21616,10.) ;
#5903 = VECTOR('',#21617,10.) ;
#5904 = VECTOR('',#21620,10.) ;
#5905 = VECTOR('',#21629,10.) ;
#5906 = VECTOR('',#21636,10.) ;
#5907 = VECTOR('',#21637,10.) ;
#5908 = VECTOR('',#21640,10.) ;
#5909 = VECTOR('',#21659,18.7631) ;
#5910 = VECTOR('',#21666,28.523658167371) ;
#5911 = VECTOR('',#21787,26.6311750163962) ;
#5912 = VECTOR('',#21908,10.) ;
#5913 = VECTOR('',#21913,10.) ;
#5914 = VECTOR('',#21914,9.99999999999998) ;
#5915 = VECTOR('',#21919,10.) ;
#5916 = VECTOR('',#21920,10.) ;
#5917 = VECTOR('',#21925,10.) ;
#5918 = VECTOR('',#21926,10.) ;
#5919 = VECTOR('',#21931,10.) ;
#5920 = VECTOR('',#21932,10.) ;
#5921 = VECTOR('',#21937,10.) ;
#5922 = VECTOR('',#21938,10.) ;
#5923 = VECTOR('',#21943,10.) ;
#5924 = VECTOR('',#21944,9.99999999999999) ;
#5925 = VECTOR('',#21949,10.) ;
#5926 = VECTOR('',#21950,10.) ;
#5927 = VECTOR('',#21955,10.) ;
#5928 = VECTOR('',#21956,10.) ;
#5929 = VECTOR('',#21961,10.) ;
#5930 = VECTOR('',#21962,10.) ;
#5931 = VECTOR('',#21967,10.) ;
#5932 = VECTOR('',#21968,10.) ;
#5933 = VECTOR('',#21973,10.) ;
#5934 = VECTOR('',#21974,10.) ;
#5935 = VECTOR('',#21979,10.) ;
#5936 = VECTOR('',#21980,10.) ;
#5937 = VECTOR('',#21985,10.) ;
#5938 = VECTOR('',#21986,10.) ;
#5939 = VECTOR('',#21991,10.) ;
#5940 = VECTOR('',#21992,10.) ;
#5941 = VECTOR('',#21997,10.) ;
#5942 = VECTOR('',#21998,10.) ;
#5943 = VECTOR('',#22003,9.99999999999998) ;
#5944 = VECTOR('',#22004,10.) ;
#5945 = VECTOR('',#22009,10.) ;
#5946 = VECTOR('',#22010,10.) ;
#5947 = VECTOR('',#22015,10.) ;
#5948 = VECTOR('',#22016,10.) ;
#5949 = VECTOR('',#22021,10.) ;
#5950 = VECTOR('',#22022,10.) ;
#5951 = VECTOR('',#22027,10.) ;
#5952 = VECTOR('',#22028,10.) ;
#5953 = VECTOR('',#22033,10.) ;
#5954 = VECTOR('',#22034,10.) ;
#5955 = VECTOR('',#22039,10.) ;
#5956 = VECTOR('',#22040,10.) ;
#5957 = VECTOR('',#22045,10.) ;
#5958 = VECTOR('',#22046,10.) ;
#5959 = VECTOR('',#22051,10.) ;
#5960 = VECTOR('',#22052,10.) ;
#5961 = VECTOR('',#22057,10.) ;
#5962 = VECTOR('',#22058,10.) ;
#5963 = VECTOR('',#22063,10.) ;
#5964 = VECTOR('',#22064,10.) ;
#5965 = VECTOR('',#22069,10.) ;
#5966 = VECTOR('',#22070,10.) ;
#5967 = VECTOR('',#22075,10.) ;
#5968 = VECTOR('',#22076,10.) ;
#5969 = VECTOR('',#22081,10.) ;
#5970 = VECTOR('',#22082,29.3077933083081) ;
#5971 = VECTOR('',#22089,32.4669335366504) ;
#5972 = VECTOR('',#22154,27.082990178354) ;
#5973 = VECTOR('',#22183,22.5) ;
#5974 = VECTOR('',#22194,37.5) ;
#5975 = VECTOR('',#22379,26.3029085923563) ;
#5976 = VECTOR('',#22792,36.4) ;
#5977 = VECTOR('',#22803,36.5) ;
#5978 = VECTOR('',#22808,22.6) ;
#5979 = VECTOR('',#22811,22.5) ;
#5980 = VECTOR('',#22816,36.4) ;
#5981 = VECTOR('',#22825,22.6) ;
#5982 = VECTOR('',#22832,3.3) ;
#5983 = VECTOR('',#22839,3.3) ;
#5984 = VECTOR('',#22846,3.3) ;
#5985 = VECTOR('',#22853,3.3) ;
#5986 = VECTOR('',#22860,3.3) ;
#5987 = VECTOR('',#22867,3.3) ;
#5988 = VECTOR('',#22874,3.3) ;
#5989 = VECTOR('',#22881,3.3) ;
#5990 = VECTOR('',#22888,33.5) ;
#5991 = VECTOR('',#22895,50.) ;
#5992 = VECTOR('',#22908,3.3) ;
#5993 = VECTOR('',#22915,3.3) ;
#5994 = VECTOR('',#22922,3.3) ;
#5995 = VECTOR('',#22929,3.3) ;
#5996 = VECTOR('',#22936,3.3) ;
#5997 = VECTOR('',#22943,3.3) ;
#5998 = VECTOR('',#22950,3.3) ;
#5999 = VECTOR('',#22957,3.3) ;
#6000 = VECTOR('',#22964,33.5) ;
#6001 = VECTOR('',#22971,50.) ;
#6002 = VERTEX_POINT('',#23015) ;
#6003 = VERTEX_POINT('',#23016) ;
#6004 = VERTEX_POINT('',#23020) ;
#6005 = VERTEX_POINT('',#23024) ;
#6006 = VERTEX_POINT('',#23025) ;
#6007 = VERTEX_POINT('',#23029) ;
#6008 = VERTEX_POINT('',#23033) ;
#6009 = VERTEX_POINT('',#23034) ;
#6010 = VERTEX_POINT('',#23038) ;
#6011 = VERTEX_POINT('',#23042) ;
#6012 = VERTEX_POINT('',#23043) ;
#6013 = VERTEX_POINT('',#23047) ;
#6014 = VERTEX_POINT('',#23051) ;
#6015 = VERTEX_POINT('',#23053) ;
#6016 = VERTEX_POINT('',#23056) ;
#6017 = VERTEX_POINT('',#23060) ;
#6018 = VERTEX_POINT('',#23064) ;
#6019 = VERTEX_POINT('',#23066) ;
#6020 = VERTEX_POINT('',#23069) ;
#6021 = VERTEX_POINT('',#23073) ;
#6022 = VERTEX_POINT('',#23077) ;
#6023 = VERTEX_POINT('',#23079) ;
#6024 = VERTEX_POINT('',#23082) ;
#6025 = VERTEX_POINT('',#23086) ;
#6026 = VERTEX_POINT('',#23090) ;
#6027 = VERTEX_POINT('',#23092) ;
#6028 = VERTEX_POINT('',#23095) ;
#6029 = VERTEX_POINT('',#23099) ;
#6030 = VERTEX_POINT('',#23103) ;
#6031 = VERTEX_POINT('',#23104) ;
#6032 = VERTEX_POINT('',#23108) ;
#6033 = VERTEX_POINT('',#23112) ;
#6034 = VERTEX_POINT('',#23113) ;
#6035 = VERTEX_POINT('',#23117) ;
#6036 = VERTEX_POINT('',#23121) ;
#6037 = VERTEX_POINT('',#23122) ;
#6038 = VERTEX_POINT('',#23126) ;
#6039 = VERTEX_POINT('',#23130) ;
#6040 = VERTEX_POINT('',#23131) ;
#6041 = VERTEX_POINT('',#23135) ;
#6042 = VERTEX_POINT('',#23139) ;
#6043 = VERTEX_POINT('',#23140) ;
#6044 = VERTEX_POINT('',#23144) ;
#6045 = VERTEX_POINT('',#23148) ;
#6046 = VERTEX_POINT('',#23149) ;
#6047 = VERTEX_POINT('',#23153) ;
#6048 = VERTEX_POINT('',#23157) ;
#6049 = VERTEX_POINT('',#23158) ;
#6050 = VERTEX_POINT('',#23162) ;
#6051 = VERTEX_POINT('',#23166) ;
#6052 = VERTEX_POINT('',#23167) ;
#6053 = VERTEX_POINT('',#23171) ;
#6054 = VERTEX_POINT('',#23175) ;
#6055 = VERTEX_POINT('',#23177) ;
#6056 = VERTEX_POINT('',#23181) ;
#6057 = VERTEX_POINT('',#23182) ;
#6058 = VERTEX_POINT('',#23184) ;
#6059 = VERTEX_POINT('',#23186) ;
#6060 = VERTEX_POINT('',#23190) ;
#6061 = VERTEX_POINT('',#23192) ;
#6062 = VERTEX_POINT('',#23196) ;
#6063 = VERTEX_POINT('',#23198) ;
#6064 = VERTEX_POINT('',#23208) ;
#6065 = VERTEX_POINT('',#23210) ;
#6066 = VERTEX_POINT('',#23213) ;
#6067 = VERTEX_POINT('',#23217) ;
#6068 = VERTEX_POINT('',#23221) ;
#6069 = VERTEX_POINT('',#23223) ;
#6070 = VERTEX_POINT('',#23226) ;
#6071 = VERTEX_POINT('',#23230) ;
#6072 = VERTEX_POINT('',#23234) ;
#6073 = VERTEX_POINT('',#23236) ;
#6074 = VERTEX_POINT('',#23239) ;
#6075 = VERTEX_POINT('',#23243) ;
#6076 = VERTEX_POINT('',#23247) ;
#6077 = VERTEX_POINT('',#23249) ;
#6078 = VERTEX_POINT('',#23252) ;
#6079 = VERTEX_POINT('',#23256) ;
#6080 = VERTEX_POINT('',#23260) ;
#6081 = VERTEX_POINT('',#23262) ;
#6082 = VERTEX_POINT('',#23265) ;
#6083 = VERTEX_POINT('',#23269) ;
#6084 = VERTEX_POINT('',#23273) ;
#6085 = VERTEX_POINT('',#23275) ;
#6086 = VERTEX_POINT('',#23278) ;
#6087 = VERTEX_POINT('',#23282) ;
#6088 = VERTEX_POINT('',#23286) ;
#6089 = VERTEX_POINT('',#23288) ;
#6090 = VERTEX_POINT('',#23291) ;
#6091 = VERTEX_POINT('',#23295) ;
#6092 = VERTEX_POINT('',#23299) ;
#6093 = VERTEX_POINT('',#23301) ;
#6094 = VERTEX_POINT('',#23304) ;
#6095 = VERTEX_POINT('',#23308) ;
#6096 = VERTEX_POINT('',#23312) ;
#6097 = VERTEX_POINT('',#23314) ;
#6098 = VERTEX_POINT('',#23317) ;
#6099 = VERTEX_POINT('',#23321) ;
#6100 = VERTEX_POINT('',#23325) ;
#6101 = VERTEX_POINT('',#23327) ;
#6102 = VERTEX_POINT('',#23330) ;
#6103 = VERTEX_POINT('',#23334) ;
#6104 = VERTEX_POINT('',#23338) ;
#6105 = VERTEX_POINT('',#23340) ;
#6106 = VERTEX_POINT('',#23343) ;
#6107 = VERTEX_POINT('',#23347) ;
#6108 = VERTEX_POINT('',#23351) ;
#6109 = VERTEX_POINT('',#23353) ;
#6110 = VERTEX_POINT('',#23356) ;
#6111 = VERTEX_POINT('',#23360) ;
#6112 = VERTEX_POINT('',#23364) ;
#6113 = VERTEX_POINT('',#23365) ;
#6114 = VERTEX_POINT('',#23367) ;
#6115 = VERTEX_POINT('',#23369) ;
#6116 = VERTEX_POINT('',#23373) ;
#6117 = VERTEX_POINT('',#23375) ;
#6118 = VERTEX_POINT('',#23379) ;
#6119 = VERTEX_POINT('',#23381) ;
#6120 = VERTEX_POINT('',#23391) ;
#6121 = VERTEX_POINT('',#23392) ;
#6122 = VERTEX_POINT('',#23396) ;
#6123 = VERTEX_POINT('',#23400) ;
#6124 = VERTEX_POINT('',#23401) ;
#6125 = VERTEX_POINT('',#23405) ;
#6126 = VERTEX_POINT('',#23409) ;
#6127 = VERTEX_POINT('',#23410) ;
#6128 = VERTEX_POINT('',#23414) ;
#6129 = VERTEX_POINT('',#23418) ;
#6130 = VERTEX_POINT('',#23419) ;
#6131 = VERTEX_POINT('',#23423) ;
#6132 = VERTEX_POINT('',#23427) ;
#6133 = VERTEX_POINT('',#23428) ;
#6134 = VERTEX_POINT('',#23432) ;
#6135 = VERTEX_POINT('',#23436) ;
#6136 = VERTEX_POINT('',#23437) ;
#6137 = VERTEX_POINT('',#23441) ;
#6138 = VERTEX_POINT('',#23445) ;
#6139 = VERTEX_POINT('',#23446) ;
#6140 = VERTEX_POINT('',#23448) ;
#6141 = VERTEX_POINT('',#23450) ;
#6142 = VERTEX_POINT('',#23454) ;
#6143 = VERTEX_POINT('',#23455) ;
#6144 = VERTEX_POINT('',#23459) ;
#6145 = VERTEX_POINT('',#23463) ;
#6146 = VERTEX_POINT('',#23464) ;
#6147 = VERTEX_POINT('',#23468) ;
#6148 = VERTEX_POINT('',#23472) ;
#6149 = VERTEX_POINT('',#23473) ;
#6150 = VERTEX_POINT('',#23478) ;
#6151 = VERTEX_POINT('',#23482) ;
#6152 = VERTEX_POINT('',#23490) ;
#6153 = VERTEX_POINT('',#23491) ;
#6154 = VERTEX_POINT('',#23495) ;
#6155 = VERTEX_POINT('',#23499) ;
#6156 = VERTEX_POINT('',#23500) ;
#6157 = VERTEX_POINT('',#23504) ;
#6158 = VERTEX_POINT('',#23508) ;
#6159 = VERTEX_POINT('',#23509) ;
#6160 = VERTEX_POINT('',#23513) ;
#6161 = VERTEX_POINT('',#23517) ;
#6162 = VERTEX_POINT('',#23518) ;
#6163 = VERTEX_POINT('',#23522) ;
#6164 = VERTEX_POINT('',#23526) ;
#6165 = VERTEX_POINT('',#23527) ;
#6166 = VERTEX_POINT('',#23531) ;
#6167 = VERTEX_POINT('',#23535) ;
#6168 = VERTEX_POINT('',#23536) ;
#6169 = VERTEX_POINT('',#23540) ;
#6170 = VERTEX_POINT('',#23544) ;
#6171 = VERTEX_POINT('',#23546) ;
#6172 = VERTEX_POINT('',#23549) ;
#6173 = VERTEX_POINT('',#23553) ;
#6174 = VERTEX_POINT('',#23557) ;
#6175 = VERTEX_POINT('',#23559) ;
#6176 = VERTEX_POINT('',#23562) ;
#6177 = VERTEX_POINT('',#23566) ;
#6178 = VERTEX_POINT('',#23570) ;
#6179 = VERTEX_POINT('',#23572) ;
#6180 = VERTEX_POINT('',#23575) ;
#6181 = VERTEX_POINT('',#23579) ;
#6182 = VERTEX_POINT('',#23583) ;
#6183 = VERTEX_POINT('',#23585) ;
#6184 = VERTEX_POINT('',#23588) ;
#6185 = VERTEX_POINT('',#23592) ;
#6186 = VERTEX_POINT('',#23596) ;
#6187 = VERTEX_POINT('',#23597) ;
#6188 = VERTEX_POINT('',#23601) ;
#6189 = VERTEX_POINT('',#23605) ;
#6190 = VERTEX_POINT('',#23606) ;
#6191 = VERTEX_POINT('',#23610) ;
#6192 = VERTEX_POINT('',#23614) ;
#6193 = VERTEX_POINT('',#23615) ;
#6194 = VERTEX_POINT('',#23619) ;
#6195 = VERTEX_POINT('',#23623) ;
#6196 = VERTEX_POINT('',#23624) ;
#6197 = VERTEX_POINT('',#23628) ;
#6198 = VERTEX_POINT('',#23632) ;
#6199 = VERTEX_POINT('',#23633) ;
#6200 = VERTEX_POINT('',#23637) ;
#6201 = VERTEX_POINT('',#23641) ;
#6202 = VERTEX_POINT('',#23642) ;
#6203 = VERTEX_POINT('',#23646) ;
#6204 = VERTEX_POINT('',#23650) ;
#6205 = VERTEX_POINT('',#23651) ;
#6206 = VERTEX_POINT('',#23655) ;
#6207 = VERTEX_POINT('',#23659) ;
#6208 = VERTEX_POINT('',#23660) ;
#6209 = VERTEX_POINT('',#23664) ;
#6210 = VERTEX_POINT('',#23668) ;
#6211 = VERTEX_POINT('',#23670) ;
#6212 = VERTEX_POINT('',#23674) ;
#6213 = VERTEX_POINT('',#23675) ;
#6214 = VERTEX_POINT('',#23677) ;
#6215 = VERTEX_POINT('',#23679) ;
#6216 = VERTEX_POINT('',#23683) ;
#6217 = VERTEX_POINT('',#23685) ;
#6218 = VERTEX_POINT('',#23689) ;
#6219 = VERTEX_POINT('',#23691) ;
#6220 = VERTEX_POINT('',#23701) ;
#6221 = VERTEX_POINT('',#23702) ;
#6222 = VERTEX_POINT('',#23706) ;
#6223 = VERTEX_POINT('',#23710) ;
#6224 = VERTEX_POINT('',#23711) ;
#6225 = VERTEX_POINT('',#23715) ;
#6226 = VERTEX_POINT('',#23719) ;
#6227 = VERTEX_POINT('',#23720) ;
#6228 = VERTEX_POINT('',#23724) ;
#6229 = VERTEX_POINT('',#23728) ;
#6230 = VERTEX_POINT('',#23729) ;
#6231 = VERTEX_POINT('',#23733) ;
#6232 = VERTEX_POINT('',#23737) ;
#6233 = VERTEX_POINT('',#23738) ;
#6234 = VERTEX_POINT('',#23742) ;
#6235 = VERTEX_POINT('',#23746) ;
#6236 = VERTEX_POINT('',#23747) ;
#6237 = VERTEX_POINT('',#23751) ;
#6238 = VERTEX_POINT('',#23755) ;
#6239 = VERTEX_POINT('',#23756) ;
#6240 = VERTEX_POINT('',#23758) ;
#6241 = VERTEX_POINT('',#23760) ;
#6242 = VERTEX_POINT('',#23764) ;
#6243 = VERTEX_POINT('',#23765) ;
#6244 = VERTEX_POINT('',#23769) ;
#6245 = VERTEX_POINT('',#23773) ;
#6246 = VERTEX_POINT('',#23774) ;
#6247 = VERTEX_POINT('',#23778) ;
#6248 = VERTEX_POINT('',#23782) ;
#6249 = VERTEX_POINT('',#23783) ;
#6250 = VERTEX_POINT('',#23788) ;
#6251 = VERTEX_POINT('',#23792) ;
#6252 = VERTEX_POINT('',#23800) ;
#6253 = VERTEX_POINT('',#23801) ;
#6254 = VERTEX_POINT('',#23803) ;
#6255 = VERTEX_POINT('',#23936) ;
#6256 = VERTEX_POINT('',#24011) ;
#6257 = VERTEX_POINT('',#24012) ;
#6258 = VERTEX_POINT('',#24709) ;
#6259 = VERTEX_POINT('',#24710) ;
#6260 = VERTEX_POINT('',#25407) ;
#6261 = VERTEX_POINT('',#25408) ;
#6262 = VERTEX_POINT('',#26237) ;
#6263 = VERTEX_POINT('',#26238) ;
#6264 = VERTEX_POINT('',#27005) ;
#6265 = VERTEX_POINT('',#27006) ;
#6266 = VERTEX_POINT('',#27735) ;
#6267 = VERTEX_POINT('',#27736) ;
#6268 = VERTEX_POINT('',#28441) ;
#6269 = VERTEX_POINT('',#28442) ;
#6270 = VERTEX_POINT('',#29109) ;
#6271 = VERTEX_POINT('',#29110) ;
#6272 = VERTEX_POINT('',#29811) ;
#6273 = VERTEX_POINT('',#29812) ;
#6274 = VERTEX_POINT('',#30597) ;
#6275 = VERTEX_POINT('',#30598) ;
#6276 = VERTEX_POINT('',#31375) ;
#6277 = VERTEX_POINT('',#31376) ;
#6278 = VERTEX_POINT('',#32053) ;
#6279 = VERTEX_POINT('',#32054) ;
#6280 = VERTEX_POINT('',#32745) ;
#6281 = VERTEX_POINT('',#32746) ;
#6282 = VERTEX_POINT('',#32748) ;
#6283 = VERTEX_POINT('',#32799) ;
#6284 = VERTEX_POINT('',#32834) ;
#6285 = VERTEX_POINT('',#32835) ;
#6286 = VERTEX_POINT('',#33144) ;
#6287 = VERTEX_POINT('',#33145) ;
#6288 = VERTEX_POINT('',#33460) ;
#6289 = VERTEX_POINT('',#33461) ;
#6290 = VERTEX_POINT('',#33774) ;
#6291 = VERTEX_POINT('',#33775) ;
#6292 = VERTEX_POINT('',#34458) ;
#6293 = VERTEX_POINT('',#34459) ;
#6294 = VERTEX_POINT('',#35154) ;
#6295 = VERTEX_POINT('',#35155) ;
#6296 = VERTEX_POINT('',#35157) ;
#6297 = VERTEX_POINT('',#35837) ;
#6298 = VERTEX_POINT('',#35838) ;
#6299 = VERTEX_POINT('',#35840) ;
#6300 = VERTEX_POINT('',#35939) ;
#6301 = VERTEX_POINT('',#36014) ;
#6302 = VERTEX_POINT('',#36015) ;
#6303 = VERTEX_POINT('',#36314) ;
#6304 = VERTEX_POINT('',#36315) ;
#6305 = VERTEX_POINT('',#36614) ;
#6306 = VERTEX_POINT('',#36615) ;
#6307 = VERTEX_POINT('',#36904) ;
#6308 = VERTEX_POINT('',#36905) ;
#6309 = VERTEX_POINT('',#37204) ;
#6310 = VERTEX_POINT('',#37205) ;
#6311 = VERTEX_POINT('',#37510) ;
#6312 = VERTEX_POINT('',#37511) ;
#6313 = VERTEX_POINT('',#37513) ;
#6314 = VERTEX_POINT('',#37754) ;
#6315 = VERTEX_POINT('',#37905) ;
#6316 = VERTEX_POINT('',#38254) ;
#6317 = VERTEX_POINT('',#38597) ;
#6318 = VERTEX_POINT('',#38598) ;
#6319 = VERTEX_POINT('',#39385) ;
#6320 = VERTEX_POINT('',#39386) ;
#6321 = VERTEX_POINT('',#39780) ;
#6322 = VERTEX_POINT('',#40180) ;
#6323 = VERTEX_POINT('',#40181) ;
#6324 = VERTEX_POINT('',#40870) ;
#6325 = VERTEX_POINT('',#40871) ;
#6326 = VERTEX_POINT('',#41618) ;
#6327 = VERTEX_POINT('',#41619) ;
#6328 = VERTEX_POINT('',#42334) ;
#6329 = VERTEX_POINT('',#42335) ;
#6330 = VERTEX_POINT('',#43026) ;
#6331 = VERTEX_POINT('',#43027) ;
#6332 = VERTEX_POINT('',#43029) ;
#6333 = VERTEX_POINT('',#43410) ;
#6334 = VERTEX_POINT('',#43886) ;
#6335 = VERTEX_POINT('',#43887) ;
#6336 = VERTEX_POINT('',#44570) ;
#6337 = VERTEX_POINT('',#44571) ;
#6338 = VERTEX_POINT('',#44919) ;
#6339 = VERTEX_POINT('',#45319) ;
#6340 = VERTEX_POINT('',#45320) ;
#6341 = VERTEX_POINT('',#46023) ;
#6342 = VERTEX_POINT('',#46024) ;
#6343 = VERTEX_POINT('',#46707) ;
#6344 = VERTEX_POINT('',#47048) ;
#6345 = VERTEX_POINT('',#47253) ;
#6346 = VERTEX_POINT('',#47366) ;
#6347 = VERTEX_POINT('',#47459) ;
#6348 = VERTEX_POINT('',#47502) ;
#6349 = VERTEX_POINT('',#47877) ;
#6350 = VERTEX_POINT('',#48139) ;
#6351 = VERTEX_POINT('',#48140) ;
#6352 = VERTEX_POINT('',#48142) ;
#6353 = VERTEX_POINT('',#48147) ;
#6354 = VERTEX_POINT('',#48150) ;
#6355 = VERTEX_POINT('',#48154) ;
#6356 = VERTEX_POINT('',#48155) ;
#6357 = VERTEX_POINT('',#48160) ;
#6358 = VERTEX_POINT('',#48164) ;
#6359 = VERTEX_POINT('',#48165) ;
#6360 = VERTEX_POINT('',#48167) ;
#6361 = VERTEX_POINT('',#48172) ;
#6362 = VERTEX_POINT('',#48175) ;
#6363 = VERTEX_POINT('',#48176) ;
#6364 = VERTEX_POINT('',#48178) ;
#6365 = VERTEX_POINT('',#48197) ;
#6366 = VERTEX_POINT('',#48218) ;
#6367 = VERTEX_POINT('',#48221) ;
#6368 = VERTEX_POINT('',#48222) ;
#6369 = VERTEX_POINT('',#48224) ;
#6370 = VERTEX_POINT('',#48229) ;
#6371 = VERTEX_POINT('',#48234) ;
#6372 = VERTEX_POINT('',#48235) ;
#6373 = VERTEX_POINT('',#48237) ;
#6374 = VERTEX_POINT('',#48239) ;
#6375 = VERTEX_POINT('',#48244) ;
#6376 = VERTEX_POINT('',#48246) ;
#6377 = VERTEX_POINT('',#48250) ;
#6378 = VERTEX_POINT('',#48254) ;
#6379 = VERTEX_POINT('',#48258) ;
#6380 = VERTEX_POINT('',#48261) ;
#6381 = VERTEX_POINT('',#48262) ;
#6382 = VERTEX_POINT('',#48264) ;
#6383 = VERTEX_POINT('',#48416) ;
#6384 = VERTEX_POINT('',#48417) ;
#6385 = VERTEX_POINT('',#48419) ;
#6386 = VERTEX_POINT('',#48424) ;
#6387 = VERTEX_POINT('',#48426) ;
#6388 = VERTEX_POINT('',#48429) ;
#6389 = VERTEX_POINT('',#48464) ;
#6390 = VERTEX_POINT('',#48499) ;
#6391 = VERTEX_POINT('',#48535) ;
#6392 = VERTEX_POINT('',#48538) ;
#6393 = VERTEX_POINT('',#48542) ;
#6394 = VERTEX_POINT('',#48612) ;
#6395 = VERTEX_POINT('',#48739) ;
#6396 = VERTEX_POINT('',#48866) ;
#6397 = VERTEX_POINT('',#49753) ;
#6398 = VERTEX_POINT('',#50589) ;
#6399 = VERTEX_POINT('',#51684) ;
#6400 = VERTEX_POINT('',#51820) ;
#6401 = VERTEX_POINT('',#51823) ;
#6402 = VERTEX_POINT('',#51825) ;
#6403 = VERTEX_POINT('',#51829) ;
#6404 = VERTEX_POINT('',#51833) ;
#6405 = VERTEX_POINT('',#51840) ;
#6406 = VERTEX_POINT('',#51844) ;
#6407 = VERTEX_POINT('',#51851) ;
#6408 = VERTEX_POINT('',#51855) ;
#6409 = VERTEX_POINT('',#51858) ;
#6410 = VERTEX_POINT('',#51863) ;
#6411 = VERTEX_POINT('',#51869) ;
#6412 = VERTEX_POINT('',#51870) ;
#6413 = VERTEX_POINT('',#51872) ;
#6414 = VERTEX_POINT('',#51874) ;
#6415 = VERTEX_POINT('',#51876) ;
#6416 = VERTEX_POINT('',#51878) ;
#6417 = VERTEX_POINT('',#51880) ;
#6418 = VERTEX_POINT('',#51882) ;
#6419 = VERTEX_POINT('',#51886) ;
#6420 = VERTEX_POINT('',#51888) ;
#6421 = VERTEX_POINT('',#51892) ;
#6422 = VERTEX_POINT('',#51893) ;
#6423 = VERTEX_POINT('',#51895) ;
#6424 = VERTEX_POINT('',#51897) ;
#6425 = VERTEX_POINT('',#51900) ;
#6426 = VERTEX_POINT('',#51902) ;
#6427 = VERTEX_POINT('',#51920) ;
#6428 = VERTEX_POINT('',#51922) ;
#6429 = VERTEX_POINT('',#51926) ;
#6430 = VERTEX_POINT('',#51929) ;
#6431 = VERTEX_POINT('',#51933) ;
#6432 = VERTEX_POINT('',#51937) ;
#6433 = VERTEX_POINT('',#51941) ;
#6434 = VERTEX_POINT('',#51945) ;
#6435 = VERTEX_POINT('',#51951) ;
#6436 = VERTEX_POINT('',#51952) ;
#6437 = VERTEX_POINT('',#51954) ;
#6438 = VERTEX_POINT('',#51956) ;
#6439 = VERTEX_POINT('',#51960) ;
#6440 = VERTEX_POINT('',#51962) ;
#6441 = VERTEX_POINT('',#51966) ;
#6442 = VERTEX_POINT('',#51967) ;
#6443 = VERTEX_POINT('',#51972) ;
#6444 = VERTEX_POINT('',#51976) ;
#6445 = VERTEX_POINT('',#51977) ;
#6446 = VERTEX_POINT('',#51979) ;
#6447 = VERTEX_POINT('',#51981) ;
#6448 = VERTEX_POINT('',#51985) ;
#6449 = VERTEX_POINT('',#51986) ;
#6450 = VERTEX_POINT('',#51988) ;
#6451 = VERTEX_POINT('',#51990) ;
#6452 = VERTEX_POINT('',#51994) ;
#6453 = VERTEX_POINT('',#51995) ;
#6454 = VERTEX_POINT('',#51997) ;
#6455 = VERTEX_POINT('',#51999) ;
#6456 = VERTEX_POINT('',#52003) ;
#6457 = VERTEX_POINT('',#52004) ;
#6458 = VERTEX_POINT('',#52006) ;
#6459 = VERTEX_POINT('',#52008) ;
#6460 = VERTEX_POINT('',#52012) ;
#6461 = VERTEX_POINT('',#52013) ;
#6462 = VERTEX_POINT('',#52015) ;
#6463 = VERTEX_POINT('',#52017) ;
#6464 = VERTEX_POINT('',#52021) ;
#6465 = VERTEX_POINT('',#52022) ;
#6466 = VERTEX_POINT('',#52024) ;
#6467 = VERTEX_POINT('',#52026) ;
#6468 = VERTEX_POINT('',#52030) ;
#6469 = VERTEX_POINT('',#52031) ;
#6470 = VERTEX_POINT('',#52033) ;
#6471 = VERTEX_POINT('',#52035) ;
#6472 = VERTEX_POINT('',#52039) ;
#6473 = VERTEX_POINT('',#52040) ;
#6474 = VERTEX_POINT('',#52042) ;
#6475 = VERTEX_POINT('',#52044) ;
#6476 = VERTEX_POINT('',#52048) ;
#6477 = VERTEX_POINT('',#52049) ;
#6478 = VERTEX_POINT('',#52051) ;
#6479 = VERTEX_POINT('',#52053) ;
#6480 = VERTEX_POINT('',#52057) ;
#6481 = VERTEX_POINT('',#52058) ;
#6482 = VERTEX_POINT('',#52060) ;
#6483 = VERTEX_POINT('',#52062) ;
#6484 = VERTEX_POINT('',#52066) ;
#6485 = VERTEX_POINT('',#52067) ;
#6486 = VERTEX_POINT('',#52069) ;
#6487 = VERTEX_POINT('',#52071) ;
#6488 = VERTEX_POINT('',#52075) ;
#6489 = VERTEX_POINT('',#52076) ;
#6490 = VERTEX_POINT('',#52078) ;
#6491 = VERTEX_POINT('',#52080) ;
#6492 = VERTEX_POINT('',#52084) ;
#6493 = VERTEX_POINT('',#52085) ;
#6494 = VERTEX_POINT('',#52087) ;
#6495 = VERTEX_POINT('',#52089) ;
#6496 = VERTEX_POINT('',#52093) ;
#6497 = VERTEX_POINT('',#52094) ;
#6498 = VERTEX_POINT('',#52096) ;
#6499 = VERTEX_POINT('',#52098) ;
#6500 = VERTEX_POINT('',#52102) ;
#6501 = VERTEX_POINT('',#52103) ;
#6502 = VERTEX_POINT('',#52105) ;
#6503 = VERTEX_POINT('',#52107) ;
#6504 = VERTEX_POINT('',#52111) ;
#6505 = VERTEX_POINT('',#52112) ;
#6506 = VERTEX_POINT('',#52114) ;
#6507 = VERTEX_POINT('',#52116) ;
#6508 = VERTEX_POINT('',#52120) ;
#6509 = VERTEX_POINT('',#52121) ;
#6510 = VERTEX_POINT('',#52123) ;
#6511 = VERTEX_POINT('',#52125) ;
#6512 = VERTEX_POINT('',#52129) ;
#6513 = VERTEX_POINT('',#52130) ;
#6514 = VERTEX_POINT('',#52132) ;
#6515 = VERTEX_POINT('',#52134) ;
#6516 = VERTEX_POINT('',#52138) ;
#6517 = VERTEX_POINT('',#52139) ;
#6518 = VERTEX_POINT('',#52141) ;
#6519 = VERTEX_POINT('',#52143) ;
#6520 = VERTEX_POINT('',#52147) ;
#6521 = VERTEX_POINT('',#52148) ;
#6522 = VERTEX_POINT('',#52150) ;
#6523 = VERTEX_POINT('',#52152) ;
#6524 = VERTEX_POINT('',#52156) ;
#6525 = VERTEX_POINT('',#52157) ;
#6526 = VERTEX_POINT('',#52159) ;
#6527 = VERTEX_POINT('',#52161) ;
#6528 = VERTEX_POINT('',#52165) ;
#6529 = VERTEX_POINT('',#52166) ;
#6530 = VERTEX_POINT('',#52168) ;
#6531 = VERTEX_POINT('',#52170) ;
#6532 = VERTEX_POINT('',#52174) ;
#6533 = VERTEX_POINT('',#52175) ;
#6534 = VERTEX_POINT('',#52177) ;
#6535 = VERTEX_POINT('',#52179) ;
#6536 = VERTEX_POINT('',#52183) ;
#6537 = VERTEX_POINT('',#52184) ;
#6538 = VERTEX_POINT('',#52186) ;
#6539 = VERTEX_POINT('',#52188) ;
#6540 = VERTEX_POINT('',#52192) ;
#6541 = VERTEX_POINT('',#52193) ;
#6542 = VERTEX_POINT('',#52195) ;
#6543 = VERTEX_POINT('',#52197) ;
#6544 = VERTEX_POINT('',#52201) ;
#6545 = VERTEX_POINT('',#52202) ;
#6546 = VERTEX_POINT('',#52204) ;
#6547 = VERTEX_POINT('',#52206) ;
#6548 = VERTEX_POINT('',#52210) ;
#6549 = VERTEX_POINT('',#52211) ;
#6550 = VERTEX_POINT('',#52213) ;
#6551 = VERTEX_POINT('',#52215) ;
#6552 = VERTEX_POINT('',#52219) ;
#6553 = VERTEX_POINT('',#52220) ;
#6554 = VERTEX_POINT('',#52222) ;
#6555 = VERTEX_POINT('',#52224) ;
#6556 = VERTEX_POINT('',#52228) ;
#6557 = VERTEX_POINT('',#52229) ;
#6558 = VERTEX_POINT('',#52231) ;
#6559 = VERTEX_POINT('',#52233) ;
#6560 = VERTEX_POINT('',#52237) ;
#6561 = VERTEX_POINT('',#52238) ;
#6562 = VERTEX_POINT('',#52240) ;
#6563 = VERTEX_POINT('',#52242) ;
#6564 = VERTEX_POINT('',#52246) ;
#6565 = VERTEX_POINT('',#52247) ;
#6566 = VERTEX_POINT('',#52249) ;
#6567 = VERTEX_POINT('',#52251) ;
#6568 = VERTEX_POINT('',#52255) ;
#6569 = VERTEX_POINT('',#52256) ;
#6570 = VERTEX_POINT('',#52258) ;
#6571 = VERTEX_POINT('',#52260) ;
#6572 = VERTEX_POINT('',#52264) ;
#6573 = VERTEX_POINT('',#52265) ;
#6574 = VERTEX_POINT('',#52267) ;
#6575 = VERTEX_POINT('',#52269) ;
#6576 = VERTEX_POINT('',#52273) ;
#6577 = VERTEX_POINT('',#52274) ;
#6578 = VERTEX_POINT('',#52276) ;
#6579 = VERTEX_POINT('',#52278) ;
#6580 = VERTEX_POINT('',#52282) ;
#6581 = VERTEX_POINT('',#52283) ;
#6582 = VERTEX_POINT('',#52285) ;
#6583 = VERTEX_POINT('',#52287) ;
#6584 = VERTEX_POINT('',#52291) ;
#6585 = VERTEX_POINT('',#52292) ;
#6586 = VERTEX_POINT('',#52294) ;
#6587 = VERTEX_POINT('',#52296) ;
#6588 = VERTEX_POINT('',#52300) ;
#6589 = VERTEX_POINT('',#52301) ;
#6590 = VERTEX_POINT('',#52303) ;
#6591 = VERTEX_POINT('',#52305) ;
#6592 = VERTEX_POINT('',#52309) ;
#6593 = VERTEX_POINT('',#52310) ;
#6594 = VERTEX_POINT('',#52312) ;
#6595 = VERTEX_POINT('',#52314) ;
#6596 = VERTEX_POINT('',#52318) ;
#6597 = VERTEX_POINT('',#52319) ;
#6598 = VERTEX_POINT('',#52321) ;
#6599 = VERTEX_POINT('',#52323) ;
#6600 = VERTEX_POINT('',#52327) ;
#6601 = VERTEX_POINT('',#52328) ;
#6602 = VERTEX_POINT('',#52330) ;
#6603 = VERTEX_POINT('',#52332) ;
#6604 = VERTEX_POINT('',#52336) ;
#6605 = VERTEX_POINT('',#52337) ;
#6606 = VERTEX_POINT('',#52339) ;
#6607 = VERTEX_POINT('',#52341) ;
#6608 = VERTEX_POINT('',#52345) ;
#6609 = VERTEX_POINT('',#52346) ;
#6610 = VERTEX_POINT('',#52348) ;
#6611 = VERTEX_POINT('',#52350) ;
#6612 = VERTEX_POINT('',#52354) ;
#6613 = VERTEX_POINT('',#52355) ;
#6614 = VERTEX_POINT('',#52357) ;
#6615 = VERTEX_POINT('',#52359) ;
#6616 = VERTEX_POINT('',#52363) ;
#6617 = VERTEX_POINT('',#52364) ;
#6618 = VERTEX_POINT('',#52366) ;
#6619 = VERTEX_POINT('',#52368) ;
#6620 = VERTEX_POINT('',#52372) ;
#6621 = VERTEX_POINT('',#52373) ;
#6622 = VERTEX_POINT('',#52375) ;
#6623 = VERTEX_POINT('',#52377) ;
#6624 = VERTEX_POINT('',#52381) ;
#6625 = VERTEX_POINT('',#52382) ;
#6626 = VERTEX_POINT('',#52384) ;
#6627 = VERTEX_POINT('',#52386) ;
#6628 = VERTEX_POINT('',#52390) ;
#6629 = VERTEX_POINT('',#52391) ;
#6630 = VERTEX_POINT('',#52393) ;
#6631 = VERTEX_POINT('',#52395) ;
#6632 = VERTEX_POINT('',#52399) ;
#6633 = VERTEX_POINT('',#52400) ;
#6634 = VERTEX_POINT('',#52402) ;
#6635 = VERTEX_POINT('',#52404) ;
#6636 = VERTEX_POINT('',#52408) ;
#6637 = VERTEX_POINT('',#52409) ;
#6638 = VERTEX_POINT('',#52411) ;
#6639 = VERTEX_POINT('',#52413) ;
#6640 = VERTEX_POINT('',#52417) ;
#6641 = VERTEX_POINT('',#52418) ;
#6642 = VERTEX_POINT('',#52420) ;
#6643 = VERTEX_POINT('',#52422) ;
#6644 = VERTEX_POINT('',#52426) ;
#6645 = VERTEX_POINT('',#52427) ;
#6646 = VERTEX_POINT('',#52429) ;
#6647 = VERTEX_POINT('',#52431) ;
#6648 = VERTEX_POINT('',#52435) ;
#6649 = VERTEX_POINT('',#52436) ;
#6650 = VERTEX_POINT('',#52438) ;
#6651 = VERTEX_POINT('',#52440) ;
#6652 = VERTEX_POINT('',#52444) ;
#6653 = VERTEX_POINT('',#52445) ;
#6654 = VERTEX_POINT('',#52447) ;
#6655 = VERTEX_POINT('',#52449) ;
#6656 = VERTEX_POINT('',#52453) ;
#6657 = VERTEX_POINT('',#52454) ;
#6658 = VERTEX_POINT('',#52456) ;
#6659 = VERTEX_POINT('',#52458) ;
#6660 = VERTEX_POINT('',#52462) ;
#6661 = VERTEX_POINT('',#52463) ;
#6662 = VERTEX_POINT('',#52465) ;
#6663 = VERTEX_POINT('',#52467) ;
#6664 = VERTEX_POINT('',#52471) ;
#6665 = VERTEX_POINT('',#52472) ;
#6666 = VERTEX_POINT('',#52474) ;
#6667 = VERTEX_POINT('',#52476) ;
#6668 = VERTEX_POINT('',#52480) ;
#6669 = VERTEX_POINT('',#52481) ;
#6670 = VERTEX_POINT('',#52483) ;
#6671 = VERTEX_POINT('',#52485) ;
#6672 = VERTEX_POINT('',#52489) ;
#6673 = VERTEX_POINT('',#52490) ;
#6674 = VERTEX_POINT('',#52492) ;
#6675 = VERTEX_POINT('',#52494) ;
#6676 = VERTEX_POINT('',#52498) ;
#6677 = VERTEX_POINT('',#52499) ;
#6678 = VERTEX_POINT('',#52501) ;
#6679 = VERTEX_POINT('',#52503) ;
#6680 = VERTEX_POINT('',#52507) ;
#6681 = VERTEX_POINT('',#52508) ;
#6682 = VERTEX_POINT('',#52510) ;
#6683 = VERTEX_POINT('',#52512) ;
#6684 = VERTEX_POINT('',#52516) ;
#6685 = VERTEX_POINT('',#52520) ;
#6686 = VERTEX_POINT('',#52523) ;
#6687 = VERTEX_POINT('',#52525) ;
#6688 = VERTEX_POINT('',#52529) ;
#6689 = VERTEX_POINT('',#52530) ;
#6690 = VERTEX_POINT('',#52535) ;
#6691 = VERTEX_POINT('',#52599) ;
#6692 = VERTEX_POINT('',#52600) ;
#6693 = VERTEX_POINT('',#52603) ;
#6694 = VERTEX_POINT('',#52667) ;
#6695 = VERTEX_POINT('',#52669) ;
#6696 = VERTEX_POINT('',#52673) ;
#6697 = VERTEX_POINT('',#52677) ;
#6698 = VERTEX_POINT('',#52680) ;
#6699 = VERTEX_POINT('',#52684) ;
#6700 = VERTEX_POINT('',#52687) ;
#6701 = VERTEX_POINT('',#52693) ;
#6702 = VERTEX_POINT('',#52695) ;
#6703 = VERTEX_POINT('',#52699) ;
#6704 = VERTEX_POINT('',#52701) ;
#6705 = VERTEX_POINT('',#52710) ;
#6706 = VERTEX_POINT('',#52712) ;
#6707 = VERTEX_POINT('',#52716) ;
#6708 = VERTEX_POINT('',#52718) ;
#6709 = VERTEX_POINT('',#52727) ;
#6710 = VERTEX_POINT('',#52729) ;
#6711 = VERTEX_POINT('',#52733) ;
#6712 = VERTEX_POINT('',#52735) ;
#6713 = VERTEX_POINT('',#52744) ;
#6714 = VERTEX_POINT('',#52746) ;
#6715 = VERTEX_POINT('',#52750) ;
#6716 = VERTEX_POINT('',#52752) ;
#6717 = VERTEX_POINT('',#52761) ;
#6718 = VERTEX_POINT('',#52763) ;
#6719 = VERTEX_POINT('',#52767) ;
#6720 = VERTEX_POINT('',#52769) ;
#6721 = VERTEX_POINT('',#52778) ;
#6722 = VERTEX_POINT('',#52780) ;
#6723 = VERTEX_POINT('',#52784) ;
#6724 = VERTEX_POINT('',#52786) ;
#6725 = VERTEX_POINT('',#52795) ;
#6726 = VERTEX_POINT('',#52797) ;
#6727 = VERTEX_POINT('',#52801) ;
#6728 = VERTEX_POINT('',#52803) ;
#6729 = VERTEX_POINT('',#52812) ;
#6730 = VERTEX_POINT('',#52814) ;
#6731 = VERTEX_POINT('',#52818) ;
#6732 = VERTEX_POINT('',#52820) ;
#6733 = VERTEX_POINT('',#52829) ;
#6734 = VERTEX_POINT('',#52831) ;
#6735 = VERTEX_POINT('',#52835) ;
#6736 = VERTEX_POINT('',#52837) ;
#6737 = VERTEX_POINT('',#52846) ;
#6738 = VERTEX_POINT('',#52848) ;
#6739 = VERTEX_POINT('',#52852) ;
#6740 = VERTEX_POINT('',#52854) ;
#6741 = VERTEX_POINT('',#52863) ;
#6742 = VERTEX_POINT('',#52865) ;
#6743 = VERTEX_POINT('',#52869) ;
#6744 = VERTEX_POINT('',#52871) ;
#6745 = VERTEX_POINT('',#52880) ;
#6746 = VERTEX_POINT('',#52882) ;
#6747 = VERTEX_POINT('',#52886) ;
#6748 = VERTEX_POINT('',#52888) ;
#6749 = VERTEX_POINT('',#52897) ;
#6750 = VERTEX_POINT('',#52899) ;
#6751 = VERTEX_POINT('',#52903) ;
#6752 = VERTEX_POINT('',#52905) ;
#6753 = VERTEX_POINT('',#52914) ;
#6754 = VERTEX_POINT('',#52916) ;
#6755 = VERTEX_POINT('',#52920) ;
#6756 = VERTEX_POINT('',#52922) ;
#6757 = VERTEX_POINT('',#52931) ;
#6758 = VERTEX_POINT('',#52933) ;
#6759 = VERTEX_POINT('',#52937) ;
#6760 = VERTEX_POINT('',#52939) ;
#6761 = VERTEX_POINT('',#52948) ;
#6762 = VERTEX_POINT('',#52950) ;
#6763 = VERTEX_POINT('',#52954) ;
#6764 = VERTEX_POINT('',#52956) ;
#6765 = VERTEX_POINT('',#52965) ;
#6766 = VERTEX_POINT('',#52967) ;
#6767 = VERTEX_POINT('',#52971) ;
#6768 = VERTEX_POINT('',#52973) ;
#6769 = VERTEX_POINT('',#52982) ;
#6770 = VERTEX_POINT('',#52984) ;
#6771 = VERTEX_POINT('',#52988) ;
#6772 = VERTEX_POINT('',#52990) ;
#6773 = VERTEX_POINT('',#52999) ;
#6774 = VERTEX_POINT('',#53001) ;
#6775 = VERTEX_POINT('',#53005) ;
#6776 = VERTEX_POINT('',#53007) ;
#6777 = VERTEX_POINT('',#53016) ;
#6778 = VERTEX_POINT('',#53018) ;
#6779 = VERTEX_POINT('',#53022) ;
#6780 = VERTEX_POINT('',#53024) ;
#6781 = VERTEX_POINT('',#53033) ;
#6782 = VERTEX_POINT('',#53035) ;
#6783 = VERTEX_POINT('',#53039) ;
#6784 = VERTEX_POINT('',#53041) ;
#6785 = VERTEX_POINT('',#53050) ;
#6786 = VERTEX_POINT('',#53052) ;
#6787 = VERTEX_POINT('',#53056) ;
#6788 = VERTEX_POINT('',#53058) ;
#6789 = VERTEX_POINT('',#53067) ;
#6790 = VERTEX_POINT('',#53069) ;
#6791 = VERTEX_POINT('',#53073) ;
#6792 = VERTEX_POINT('',#53075) ;
#6793 = VERTEX_POINT('',#53084) ;
#6794 = VERTEX_POINT('',#53086) ;
#6795 = VERTEX_POINT('',#53090) ;
#6796 = VERTEX_POINT('',#53092) ;
#6797 = VERTEX_POINT('',#53101) ;
#6798 = VERTEX_POINT('',#53103) ;
#6799 = VERTEX_POINT('',#53107) ;
#6800 = VERTEX_POINT('',#53109) ;
#6801 = VERTEX_POINT('',#53118) ;
#6802 = VERTEX_POINT('',#53120) ;
#6803 = VERTEX_POINT('',#53124) ;
#6804 = VERTEX_POINT('',#53126) ;
#6805 = VERTEX_POINT('',#53135) ;
#6806 = VERTEX_POINT('',#53137) ;
#6807 = VERTEX_POINT('',#53141) ;
#6808 = VERTEX_POINT('',#53143) ;
#6809 = VERTEX_POINT('',#53152) ;
#6810 = VERTEX_POINT('',#53154) ;
#6811 = VERTEX_POINT('',#53158) ;
#6812 = VERTEX_POINT('',#53160) ;
#6813 = VERTEX_POINT('',#53169) ;
#6814 = VERTEX_POINT('',#53171) ;
#6815 = VERTEX_POINT('',#53175) ;
#6816 = VERTEX_POINT('',#53177) ;
#6817 = VERTEX_POINT('',#53186) ;
#6818 = VERTEX_POINT('',#53188) ;
#6819 = VERTEX_POINT('',#53192) ;
#6820 = VERTEX_POINT('',#53194) ;
#6821 = VERTEX_POINT('',#53203) ;
#6822 = VERTEX_POINT('',#53205) ;
#6823 = VERTEX_POINT('',#53209) ;
#6824 = VERTEX_POINT('',#53211) ;
#6825 = VERTEX_POINT('',#53220) ;
#6826 = VERTEX_POINT('',#53222) ;
#6827 = VERTEX_POINT('',#53226) ;
#6828 = VERTEX_POINT('',#53228) ;
#6829 = VERTEX_POINT('',#53237) ;
#6830 = VERTEX_POINT('',#53239) ;
#6831 = VERTEX_POINT('',#53243) ;
#6832 = VERTEX_POINT('',#53245) ;
#6833 = VERTEX_POINT('',#53254) ;
#6834 = VERTEX_POINT('',#53256) ;
#6835 = VERTEX_POINT('',#53260) ;
#6836 = VERTEX_POINT('',#53262) ;
#6837 = VERTEX_POINT('',#53271) ;
#6838 = VERTEX_POINT('',#53273) ;
#6839 = VERTEX_POINT('',#53277) ;
#6840 = VERTEX_POINT('',#53279) ;
#6841 = VERTEX_POINT('',#53288) ;
#6842 = VERTEX_POINT('',#53290) ;
#6843 = VERTEX_POINT('',#53294) ;
#6844 = VERTEX_POINT('',#53296) ;
#6845 = VERTEX_POINT('',#53305) ;
#6846 = VERTEX_POINT('',#53307) ;
#6847 = VERTEX_POINT('',#53311) ;
#6848 = VERTEX_POINT('',#53313) ;
#6849 = VERTEX_POINT('',#53322) ;
#6850 = VERTEX_POINT('',#53324) ;
#6851 = VERTEX_POINT('',#53328) ;
#6852 = VERTEX_POINT('',#53330) ;
#6853 = VERTEX_POINT('',#53339) ;
#6854 = VERTEX_POINT('',#53341) ;
#6855 = VERTEX_POINT('',#53345) ;
#6856 = VERTEX_POINT('',#53347) ;
#6857 = VERTEX_POINT('',#53356) ;
#6858 = VERTEX_POINT('',#53358) ;
#6859 = VERTEX_POINT('',#53362) ;
#6860 = VERTEX_POINT('',#53364) ;
#6861 = VERTEX_POINT('',#53373) ;
#6862 = VERTEX_POINT('',#53375) ;
#6863 = VERTEX_POINT('',#53379) ;
#6864 = VERTEX_POINT('',#53381) ;
#6865 = VERTEX_POINT('',#53390) ;
#6866 = VERTEX_POINT('',#53392) ;
#6867 = VERTEX_POINT('',#53396) ;
#6868 = VERTEX_POINT('',#53398) ;
#6869 = VERTEX_POINT('',#53407) ;
#6870 = VERTEX_POINT('',#53409) ;
#6871 = VERTEX_POINT('',#53413) ;
#6872 = VERTEX_POINT('',#53415) ;
#6873 = VERTEX_POINT('',#53424) ;
#6874 = VERTEX_POINT('',#53426) ;
#6875 = VERTEX_POINT('',#53430) ;
#6876 = VERTEX_POINT('',#53432) ;
#6877 = VERTEX_POINT('',#53441) ;
#6878 = VERTEX_POINT('',#53443) ;
#6879 = VERTEX_POINT('',#53447) ;
#6880 = VERTEX_POINT('',#53449) ;
#6881 = VERTEX_POINT('',#53458) ;
#6882 = VERTEX_POINT('',#53460) ;
#6883 = VERTEX_POINT('',#53464) ;
#6884 = VERTEX_POINT('',#53466) ;
#6885 = VERTEX_POINT('',#53475) ;
#6886 = VERTEX_POINT('',#53477) ;
#6887 = VERTEX_POINT('',#53481) ;
#6888 = VERTEX_POINT('',#53483) ;
#6889 = VERTEX_POINT('',#53492) ;
#6890 = VERTEX_POINT('',#53494) ;
#6891 = VERTEX_POINT('',#53498) ;
#6892 = VERTEX_POINT('',#53500) ;
#6893 = VERTEX_POINT('',#53509) ;
#6894 = VERTEX_POINT('',#53511) ;
#6895 = VERTEX_POINT('',#53515) ;
#6896 = VERTEX_POINT('',#53517) ;
#6897 = VERTEX_POINT('',#53526) ;
#6898 = VERTEX_POINT('',#53528) ;
#6899 = VERTEX_POINT('',#53532) ;
#6900 = VERTEX_POINT('',#53534) ;
#6901 = VERTEX_POINT('',#53543) ;
#6902 = VERTEX_POINT('',#53545) ;
#6903 = VERTEX_POINT('',#53549) ;
#6904 = VERTEX_POINT('',#53551) ;
#6905 = VERTEX_POINT('',#53560) ;
#6906 = VERTEX_POINT('',#53562) ;
#6907 = VERTEX_POINT('',#53566) ;
#6908 = VERTEX_POINT('',#53568) ;
#6909 = VERTEX_POINT('',#53577) ;
#6910 = VERTEX_POINT('',#53579) ;
#6911 = VERTEX_POINT('',#53583) ;
#6912 = VERTEX_POINT('',#53585) ;
#6913 = VERTEX_POINT('',#53594) ;
#6914 = VERTEX_POINT('',#53596) ;
#6915 = VERTEX_POINT('',#53600) ;
#6916 = VERTEX_POINT('',#53602) ;
#6917 = VERTEX_POINT('',#53611) ;
#6918 = VERTEX_POINT('',#53613) ;
#6919 = VERTEX_POINT('',#53617) ;
#6920 = VERTEX_POINT('',#53619) ;
#6921 = VERTEX_POINT('',#53628) ;
#6922 = VERTEX_POINT('',#53630) ;
#6923 = VERTEX_POINT('',#53634) ;
#6924 = VERTEX_POINT('',#53636) ;
#6925 = VERTEX_POINT('',#53645) ;
#6926 = VERTEX_POINT('',#53647) ;
#6927 = VERTEX_POINT('',#53651) ;
#6928 = VERTEX_POINT('',#53653) ;
#6929 = VERTEX_POINT('',#53662) ;
#6930 = VERTEX_POINT('',#53664) ;
#6931 = VERTEX_POINT('',#53668) ;
#6932 = VERTEX_POINT('',#53670) ;
#6933 = VERTEX_POINT('',#53679) ;
#6934 = VERTEX_POINT('',#53681) ;
#6935 = VERTEX_POINT('',#53685) ;
#6936 = VERTEX_POINT('',#53687) ;
#6937 = VERTEX_POINT('',#53696) ;
#6938 = VERTEX_POINT('',#53698) ;
#6939 = VERTEX_POINT('',#53702) ;
#6940 = VERTEX_POINT('',#53704) ;
#6941 = VERTEX_POINT('',#53715) ;
#6942 = VERTEX_POINT('',#53716) ;
#6943 = VERTEX_POINT('',#53719) ;
#6944 = VERTEX_POINT('',#53723) ;
#6945 = VERTEX_POINT('',#53727) ;
#6946 = VERTEX_POINT('',#53730) ;
#6947 = VERTEX_POINT('',#53731) ;
#6948 = VERTEX_POINT('',#53736) ;
#6949 = VERTEX_POINT('',#53740) ;
#6950 = VERTEX_POINT('',#53744) ;
#6951 = VERTEX_POINT('',#53750) ;
#6952 = VERTEX_POINT('',#53751) ;
#6953 = VERTEX_POINT('',#53755) ;
#6954 = VERTEX_POINT('',#53757) ;
#6955 = VERTEX_POINT('',#53761) ;
#6956 = VERTEX_POINT('',#53762) ;
#6957 = VERTEX_POINT('',#53766) ;
#6958 = VERTEX_POINT('',#53768) ;
#6959 = VERTEX_POINT('',#53775) ;
#6960 = VERTEX_POINT('',#53777) ;
#6961 = VERTEX_POINT('',#53779) ;
#6962 = VERTEX_POINT('',#53781) ;
#6963 = VERTEX_POINT('',#53783) ;
#6964 = VERTEX_POINT('',#53785) ;
#6965 = VERTEX_POINT('',#53787) ;
#6966 = VERTEX_POINT('',#53789) ;
#6967 = VERTEX_POINT('',#53791) ;
#6968 = VERTEX_POINT('',#53793) ;
#6969 = VERTEX_POINT('',#53795) ;
#6970 = VERTEX_POINT('',#53797) ;
#6971 = VERTEX_POINT('',#53800) ;
#6972 = VERTEX_POINT('',#53803) ;
#6973 = VERTEX_POINT('',#53807) ;
#6974 = VERTEX_POINT('',#53813) ;
#6975 = VERTEX_POINT('',#53814) ;
#6976 = VERTEX_POINT('',#53825) ;
#6977 = VERTEX_POINT('',#53829) ;
#6978 = VERTEX_POINT('',#53835) ;
#6979 = VERTEX_POINT('',#53836) ;
#6980 = VERTEX_POINT('',#53847) ;
#6981 = VERTEX_POINT('',#53851) ;
#6982 = VERTEX_POINT('',#53857) ;
#6983 = VERTEX_POINT('',#53858) ;
#6984 = VERTEX_POINT('',#53873) ;
#6985 = VERTEX_POINT('',#53879) ;
#6986 = VERTEX_POINT('',#53881) ;
#6987 = VERTEX_POINT('',#53883) ;
#6988 = VERTEX_POINT('',#53885) ;
#6989 = VERTEX_POINT('',#53926) ;
#6990 = VERTEX_POINT('',#53930) ;
#6991 = VERTEX_POINT('',#53932) ;
#6992 = VERTEX_POINT('',#53936) ;
#6993 = VERTEX_POINT('',#53977) ;
#6994 = VERTEX_POINT('',#53979) ;
#6995 = VERTEX_POINT('',#54020) ;
#6996 = VERTEX_POINT('',#54024) ;
#6997 = VERTEX_POINT('',#54026) ;
#6998 = VERTEX_POINT('',#54030) ;
#6999 = VERTEX_POINT('',#54071) ;
#7000 = VERTEX_POINT('',#54073) ;
#7001 = VERTEX_POINT('',#54114) ;
#7002 = VERTEX_POINT('',#54118) ;
#7003 = VERTEX_POINT('',#54120) ;
#7004 = VERTEX_POINT('',#54124) ;
#7005 = VERTEX_POINT('',#54165) ;
#7006 = VERTEX_POINT('',#54167) ;
#7007 = VERTEX_POINT('',#54208) ;
#7008 = VERTEX_POINT('',#54212) ;
#7009 = VERTEX_POINT('',#54214) ;
#7010 = VERTEX_POINT('',#54218) ;
#7011 = VERTEX_POINT('',#54259) ;
#7012 = VERTEX_POINT('',#54261) ;
#7013 = VERTEX_POINT('',#54302) ;
#7014 = VERTEX_POINT('',#54306) ;
#7015 = VERTEX_POINT('',#54308) ;
#7016 = VERTEX_POINT('',#54312) ;
#7017 = VERTEX_POINT('',#54353) ;
#7018 = VERTEX_POINT('',#54355) ;
#7019 = VERTEX_POINT('',#54396) ;
#7020 = VERTEX_POINT('',#54400) ;
#7021 = VERTEX_POINT('',#54402) ;
#7022 = VERTEX_POINT('',#54406) ;
#7023 = VERTEX_POINT('',#54447) ;
#7024 = VERTEX_POINT('',#54449) ;
#7025 = VERTEX_POINT('',#54490) ;
#7026 = VERTEX_POINT('',#54494) ;
#7027 = VERTEX_POINT('',#54496) ;
#7028 = VERTEX_POINT('',#54500) ;
#7029 = VERTEX_POINT('',#54541) ;
#7030 = VERTEX_POINT('',#54543) ;
#7031 = VERTEX_POINT('',#54584) ;
#7032 = VERTEX_POINT('',#54588) ;
#7033 = VERTEX_POINT('',#54590) ;
#7034 = VERTEX_POINT('',#54594) ;
#7035 = VERTEX_POINT('',#54635) ;
#7036 = VERTEX_POINT('',#54637) ;
#7037 = VERTEX_POINT('',#54678) ;
#7038 = VERTEX_POINT('',#54682) ;
#7039 = VERTEX_POINT('',#54684) ;
#7040 = VERTEX_POINT('',#54688) ;
#7041 = VERTEX_POINT('',#54729) ;
#7042 = VERTEX_POINT('',#54731) ;
#7043 = VERTEX_POINT('',#54772) ;
#7044 = VERTEX_POINT('',#54776) ;
#7045 = VERTEX_POINT('',#54778) ;
#7046 = VERTEX_POINT('',#54782) ;
#7047 = VERTEX_POINT('',#54823) ;
#7048 = VERTEX_POINT('',#54825) ;
#7049 = VERTEX_POINT('',#54866) ;
#7050 = VERTEX_POINT('',#54870) ;
#7051 = VERTEX_POINT('',#54872) ;
#7052 = VERTEX_POINT('',#54876) ;
#7053 = VERTEX_POINT('',#54917) ;
#7054 = VERTEX_POINT('',#54919) ;
#7055 = VERTEX_POINT('',#54960) ;
#7056 = VERTEX_POINT('',#54964) ;
#7057 = VERTEX_POINT('',#54966) ;
#7058 = VERTEX_POINT('',#54970) ;
#7059 = VERTEX_POINT('',#55011) ;
#7060 = VERTEX_POINT('',#55013) ;
#7061 = VERTEX_POINT('',#55054) ;
#7062 = VERTEX_POINT('',#55058) ;
#7063 = VERTEX_POINT('',#55060) ;
#7064 = VERTEX_POINT('',#55064) ;
#7065 = VERTEX_POINT('',#55105) ;
#7066 = VERTEX_POINT('',#55107) ;
#7067 = VERTEX_POINT('',#55148) ;
#7068 = VERTEX_POINT('',#55152) ;
#7069 = VERTEX_POINT('',#55154) ;
#7070 = VERTEX_POINT('',#55158) ;
#7071 = VERTEX_POINT('',#55199) ;
#7072 = VERTEX_POINT('',#55201) ;
#7073 = VERTEX_POINT('',#55242) ;
#7074 = VERTEX_POINT('',#55246) ;
#7075 = VERTEX_POINT('',#55248) ;
#7076 = VERTEX_POINT('',#55252) ;
#7077 = VERTEX_POINT('',#55293) ;
#7078 = VERTEX_POINT('',#55295) ;
#7079 = VERTEX_POINT('',#55336) ;
#7080 = VERTEX_POINT('',#55340) ;
#7081 = VERTEX_POINT('',#55342) ;
#7082 = VERTEX_POINT('',#55346) ;
#7083 = VERTEX_POINT('',#55387) ;
#7084 = VERTEX_POINT('',#55389) ;
#7085 = VERTEX_POINT('',#55430) ;
#7086 = VERTEX_POINT('',#55434) ;
#7087 = VERTEX_POINT('',#55436) ;
#7088 = VERTEX_POINT('',#55440) ;
#7089 = VERTEX_POINT('',#55481) ;
#7090 = VERTEX_POINT('',#55483) ;
#7091 = VERTEX_POINT('',#55524) ;
#7092 = VERTEX_POINT('',#55528) ;
#7093 = VERTEX_POINT('',#55530) ;
#7094 = VERTEX_POINT('',#55534) ;
#7095 = VERTEX_POINT('',#55575) ;
#7096 = VERTEX_POINT('',#55577) ;
#7097 = VERTEX_POINT('',#55618) ;
#7098 = VERTEX_POINT('',#55622) ;
#7099 = VERTEX_POINT('',#55624) ;
#7100 = VERTEX_POINT('',#55628) ;
#7101 = VERTEX_POINT('',#55669) ;
#7102 = VERTEX_POINT('',#55671) ;
#7103 = VERTEX_POINT('',#55712) ;
#7104 = VERTEX_POINT('',#55716) ;
#7105 = VERTEX_POINT('',#55718) ;
#7106 = VERTEX_POINT('',#55722) ;
#7107 = VERTEX_POINT('',#55763) ;
#7108 = VERTEX_POINT('',#55765) ;
#7109 = VERTEX_POINT('',#55806) ;
#7110 = VERTEX_POINT('',#55810) ;
#7111 = VERTEX_POINT('',#55812) ;
#7112 = VERTEX_POINT('',#55816) ;
#7113 = VERTEX_POINT('',#55857) ;
#7114 = VERTEX_POINT('',#55859) ;
#7115 = VERTEX_POINT('',#55900) ;
#7116 = VERTEX_POINT('',#55904) ;
#7117 = VERTEX_POINT('',#55906) ;
#7118 = VERTEX_POINT('',#55910) ;
#7119 = VERTEX_POINT('',#55951) ;
#7120 = VERTEX_POINT('',#55953) ;
#7121 = VERTEX_POINT('',#55994) ;
#7122 = VERTEX_POINT('',#55998) ;
#7123 = VERTEX_POINT('',#56000) ;
#7124 = VERTEX_POINT('',#56004) ;
#7125 = VERTEX_POINT('',#56045) ;
#7126 = VERTEX_POINT('',#56047) ;
#7127 = VERTEX_POINT('',#56088) ;
#7128 = VERTEX_POINT('',#56092) ;
#7129 = VERTEX_POINT('',#56094) ;
#7130 = VERTEX_POINT('',#56098) ;
#7131 = VERTEX_POINT('',#56139) ;
#7132 = VERTEX_POINT('',#56141) ;
#7133 = VERTEX_POINT('',#56182) ;
#7134 = VERTEX_POINT('',#56186) ;
#7135 = VERTEX_POINT('',#56188) ;
#7136 = VERTEX_POINT('',#56192) ;
#7137 = VERTEX_POINT('',#56233) ;
#7138 = VERTEX_POINT('',#56235) ;
#7139 = VERTEX_POINT('',#56276) ;
#7140 = VERTEX_POINT('',#56280) ;
#7141 = VERTEX_POINT('',#56282) ;
#7142 = VERTEX_POINT('',#56286) ;
#7143 = VERTEX_POINT('',#56327) ;
#7144 = VERTEX_POINT('',#56329) ;
#7145 = VERTEX_POINT('',#56370) ;
#7146 = VERTEX_POINT('',#56374) ;
#7147 = VERTEX_POINT('',#56376) ;
#7148 = VERTEX_POINT('',#56380) ;
#7149 = VERTEX_POINT('',#56421) ;
#7150 = VERTEX_POINT('',#56423) ;
#7151 = VERTEX_POINT('',#56464) ;
#7152 = VERTEX_POINT('',#56468) ;
#7153 = VERTEX_POINT('',#56470) ;
#7154 = VERTEX_POINT('',#56474) ;
#7155 = VERTEX_POINT('',#56515) ;
#7156 = VERTEX_POINT('',#56517) ;
#7157 = VERTEX_POINT('',#56558) ;
#7158 = VERTEX_POINT('',#56562) ;
#7159 = VERTEX_POINT('',#56564) ;
#7160 = VERTEX_POINT('',#56568) ;
#7161 = VERTEX_POINT('',#56611) ;
#7162 = VERTEX_POINT('',#56613) ;
#7163 = VERTEX_POINT('',#56615) ;
#7164 = VERTEX_POINT('',#56638) ;
#7165 = VERTEX_POINT('',#56650) ;
#7166 = VERTEX_POINT('',#56652) ;
#7167 = VERTEX_POINT('',#56675) ;
#7168 = VERTEX_POINT('',#56689) ;
#7169 = VERTEX_POINT('',#56691) ;
#7170 = VERTEX_POINT('',#56714) ;
#7171 = VERTEX_POINT('',#56726) ;
#7172 = VERTEX_POINT('',#56728) ;
#7173 = VERTEX_POINT('',#56751) ;
#7174 = VERTEX_POINT('',#56765) ;
#7175 = VERTEX_POINT('',#56767) ;
#7176 = VERTEX_POINT('',#56790) ;
#7177 = VERTEX_POINT('',#56802) ;
#7178 = VERTEX_POINT('',#56804) ;
#7179 = VERTEX_POINT('',#56827) ;
#7180 = VERTEX_POINT('',#56857) ;
#7181 = VERTEX_POINT('',#56859) ;
#7182 = VERTEX_POINT('',#56882) ;
#7183 = VERTEX_POINT('',#56894) ;
#7184 = VERTEX_POINT('',#56896) ;
#7185 = VERTEX_POINT('',#56919) ;
#7186 = VERTEX_POINT('',#56933) ;
#7187 = VERTEX_POINT('',#56935) ;
#7188 = VERTEX_POINT('',#56937) ;
#7189 = VERTEX_POINT('',#56960) ;
#7190 = VERTEX_POINT('',#56972) ;
#7191 = VERTEX_POINT('',#56974) ;
#7192 = VERTEX_POINT('',#56997) ;
#7193 = VERTEX_POINT('',#57015) ;
#7194 = VERTEX_POINT('',#57017) ;
#7195 = VERTEX_POINT('',#57040) ;
#7196 = VERTEX_POINT('',#57054) ;
#7197 = VERTEX_POINT('',#57056) ;
#7198 = VERTEX_POINT('',#57079) ;
#7199 = VERTEX_POINT('',#57091) ;
#7200 = VERTEX_POINT('',#57093) ;
#7201 = VERTEX_POINT('',#57095) ;
#7202 = VERTEX_POINT('',#57118) ;
#7203 = VERTEX_POINT('',#57132) ;
#7204 = VERTEX_POINT('',#57134) ;
#7205 = VERTEX_POINT('',#57161) ;
#7206 = VERTEX_POINT('',#57183) ;
#7207 = VERTEX_POINT('',#57185) ;
#7208 = VERTEX_POINT('',#57208) ;
#7209 = VERTEX_POINT('',#57220) ;
#7210 = VERTEX_POINT('',#57222) ;
#7211 = VERTEX_POINT('',#57245) ;
#7212 = VERTEX_POINT('',#57259) ;
#7213 = VERTEX_POINT('',#57261) ;
#7214 = VERTEX_POINT('',#57284) ;
#7215 = VERTEX_POINT('',#57298) ;
#7216 = VERTEX_POINT('',#57300) ;
#7217 = VERTEX_POINT('',#57323) ;
#7218 = VERTEX_POINT('',#57343) ;
#7219 = VERTEX_POINT('',#57345) ;
#7220 = VERTEX_POINT('',#57374) ;
#7221 = VERTEX_POINT('',#57394) ;
#7222 = VERTEX_POINT('',#57396) ;
#7223 = VERTEX_POINT('',#57419) ;
#7224 = VERTEX_POINT('',#57433) ;
#7225 = VERTEX_POINT('',#57435) ;
#7226 = VERTEX_POINT('',#57458) ;
#7227 = VERTEX_POINT('',#57470) ;
#7228 = VERTEX_POINT('',#57472) ;
#7229 = VERTEX_POINT('',#57495) ;
#7230 = VERTEX_POINT('',#57509) ;
#7231 = VERTEX_POINT('',#57511) ;
#7232 = VERTEX_POINT('',#57534) ;
#7233 = VERTEX_POINT('',#57546) ;
#7234 = VERTEX_POINT('',#57548) ;
#7235 = VERTEX_POINT('',#57571) ;
#7236 = VERTEX_POINT('',#57585) ;
#7237 = VERTEX_POINT('',#57587) ;
#7238 = VERTEX_POINT('',#57610) ;
#7239 = VERTEX_POINT('',#57622) ;
#7240 = VERTEX_POINT('',#57624) ;
#7241 = VERTEX_POINT('',#57647) ;
#7242 = VERTEX_POINT('',#57661) ;
#7243 = VERTEX_POINT('',#57663) ;
#7244 = VERTEX_POINT('',#57686) ;
#7245 = VERTEX_POINT('',#57701) ;
#7246 = VERTEX_POINT('',#57728) ;
#7247 = VERTEX_POINT('',#57750) ;
#7248 = VERTEX_POINT('',#57779) ;
#7249 = VERTEX_POINT('',#57802) ;
#7250 = VERTEX_POINT('',#57805) ;
#7251 = VERTEX_POINT('',#57808) ;
#7252 = VERTEX_POINT('',#57811) ;
#7253 = VERTEX_POINT('',#57814) ;
#7254 = VERTEX_POINT('',#57817) ;
#7255 = VERTEX_POINT('',#57820) ;
#7256 = VERTEX_POINT('',#57823) ;
#7257 = VERTEX_POINT('',#57826) ;
#7258 = VERTEX_POINT('',#57829) ;
#7259 = VERTEX_POINT('',#57832) ;
#7260 = VERTEX_POINT('',#57835) ;
#7261 = VERTEX_POINT('',#57838) ;
#7262 = VERTEX_POINT('',#57841) ;
#7263 = VERTEX_POINT('',#57844) ;
#7264 = VERTEX_POINT('',#57847) ;
#7265 = VERTEX_POINT('',#57850) ;
#7266 = VERTEX_POINT('',#57853) ;
#7267 = VERTEX_POINT('',#57856) ;
#7268 = VERTEX_POINT('',#57859) ;
#7269 = VERTEX_POINT('',#57862) ;
#7270 = VERTEX_POINT('',#57865) ;
#7271 = VERTEX_POINT('',#57868) ;
#7272 = VERTEX_POINT('',#57871) ;
#7273 = VERTEX_POINT('',#57874) ;
#7274 = VERTEX_POINT('',#57877) ;
#7275 = VERTEX_POINT('',#57880) ;
#7276 = VERTEX_POINT('',#57883) ;
#7277 = VERTEX_POINT('',#57886) ;
#7278 = VERTEX_POINT('',#57889) ;
#7279 = VERTEX_POINT('',#57892) ;
#7280 = VERTEX_POINT('',#57895) ;
#7281 = VERTEX_POINT('',#57898) ;
#7282 = VERTEX_POINT('',#57901) ;
#7283 = VERTEX_POINT('',#57904) ;
#7284 = VERTEX_POINT('',#57907) ;
#7285 = VERTEX_POINT('',#57910) ;
#7286 = VERTEX_POINT('',#57913) ;
#7287 = VERTEX_POINT('',#57916) ;
#7288 = VERTEX_POINT('',#57919) ;
#7289 = VERTEX_POINT('',#57922) ;
#7290 = VERTEX_POINT('',#57925) ;
#7291 = VERTEX_POINT('',#57928) ;
#7292 = VERTEX_POINT('',#57931) ;
#7293 = VERTEX_POINT('',#57934) ;
#7294 = VERTEX_POINT('',#57937) ;
#7295 = VERTEX_POINT('',#57940) ;
#7296 = VERTEX_POINT('',#57943) ;
#7297 = VERTEX_POINT('',#57946) ;
#7298 = VERTEX_POINT('',#57949) ;
#7299 = VERTEX_POINT('',#57952) ;
#7300 = VERTEX_POINT('',#57955) ;
#7301 = VERTEX_POINT('',#57958) ;
#7302 = VERTEX_POINT('',#57961) ;
#7303 = VERTEX_POINT('',#57964) ;
#7304 = VERTEX_POINT('',#57967) ;
#7305 = VERTEX_POINT('',#57970) ;
#7306 = VERTEX_POINT('',#57973) ;
#7307 = VERTEX_POINT('',#57976) ;
#7308 = VERTEX_POINT('',#57980) ;
#7309 = VERTEX_POINT('',#57982) ;
#7310 = VERTEX_POINT('',#57985) ;
#7311 = VERTEX_POINT('',#57986) ;
#7312 = VERTEX_POINT('',#58077) ;
#7313 = VERTEX_POINT('',#58169) ;
#7314 = VERTEX_POINT('',#58170) ;
#7315 = VERTEX_POINT('',#58172) ;
#7316 = VERTEX_POINT('',#58351) ;
#7317 = VERTEX_POINT('',#58352) ;
#7318 = VERTEX_POINT('',#58354) ;
#7319 = VERTEX_POINT('',#58533) ;
#7320 = VERTEX_POINT('',#58534) ;
#7321 = VERTEX_POINT('',#58536) ;
#7322 = VERTEX_POINT('',#58716) ;
#7323 = VERTEX_POINT('',#58717) ;
#7324 = VERTEX_POINT('',#58719) ;
#7325 = VERTEX_POINT('',#58900) ;
#7326 = VERTEX_POINT('',#58901) ;
#7327 = VERTEX_POINT('',#58903) ;
#7328 = VERTEX_POINT('',#59082) ;
#7329 = VERTEX_POINT('',#59083) ;
#7330 = VERTEX_POINT('',#59085) ;
#7331 = VERTEX_POINT('',#59264) ;
#7332 = VERTEX_POINT('',#59265) ;
#7333 = VERTEX_POINT('',#59267) ;
#7334 = VERTEX_POINT('',#59448) ;
#7335 = VERTEX_POINT('',#59449) ;
#7336 = VERTEX_POINT('',#59451) ;
#7337 = VERTEX_POINT('',#59631) ;
#7338 = VERTEX_POINT('',#59632) ;
#7339 = VERTEX_POINT('',#59634) ;
#7340 = VERTEX_POINT('',#59813) ;
#7341 = VERTEX_POINT('',#59814) ;
#7342 = VERTEX_POINT('',#59816) ;
#7343 = VERTEX_POINT('',#59996) ;
#7344 = VERTEX_POINT('',#59997) ;
#7345 = VERTEX_POINT('',#59999) ;
#7346 = VERTEX_POINT('',#60180) ;
#7347 = VERTEX_POINT('',#60181) ;
#7348 = VERTEX_POINT('',#60183) ;
#7349 = VERTEX_POINT('',#60362) ;
#7350 = VERTEX_POINT('',#60363) ;
#7351 = VERTEX_POINT('',#60365) ;
#7352 = VERTEX_POINT('',#60544) ;
#7353 = VERTEX_POINT('',#60545) ;
#7354 = VERTEX_POINT('',#60547) ;
#7355 = VERTEX_POINT('',#60728) ;
#7356 = VERTEX_POINT('',#60729) ;
#7357 = VERTEX_POINT('',#60731) ;
#7358 = VERTEX_POINT('',#60910) ;
#7359 = VERTEX_POINT('',#60911) ;
#7360 = VERTEX_POINT('',#60913) ;
#7361 = VERTEX_POINT('',#61092) ;
#7362 = VERTEX_POINT('',#61093) ;
#7363 = VERTEX_POINT('',#61095) ;
#7364 = VERTEX_POINT('',#61275) ;
#7365 = VERTEX_POINT('',#61276) ;
#7366 = VERTEX_POINT('',#61278) ;
#7367 = VERTEX_POINT('',#61459) ;
#7368 = VERTEX_POINT('',#61460) ;
#7369 = VERTEX_POINT('',#61462) ;
#7370 = VERTEX_POINT('',#61641) ;
#7371 = VERTEX_POINT('',#61642) ;
#7372 = VERTEX_POINT('',#61644) ;
#7373 = VERTEX_POINT('',#61823) ;
#7374 = VERTEX_POINT('',#61824) ;
#7375 = VERTEX_POINT('',#61826) ;
#7376 = VERTEX_POINT('',#62007) ;
#7377 = VERTEX_POINT('',#62008) ;
#7378 = VERTEX_POINT('',#62010) ;
#7379 = VERTEX_POINT('',#62190) ;
#7380 = VERTEX_POINT('',#62191) ;
#7381 = VERTEX_POINT('',#62193) ;
#7382 = VERTEX_POINT('',#62372) ;
#7383 = VERTEX_POINT('',#62373) ;
#7384 = VERTEX_POINT('',#62375) ;
#7385 = VERTEX_POINT('',#62555) ;
#7386 = VERTEX_POINT('',#62556) ;
#7387 = VERTEX_POINT('',#62558) ;
#7388 = VERTEX_POINT('',#62739) ;
#7389 = VERTEX_POINT('',#62740) ;
#7390 = VERTEX_POINT('',#62742) ;
#7391 = VERTEX_POINT('',#62921) ;
#7392 = VERTEX_POINT('',#62922) ;
#7393 = VERTEX_POINT('',#62924) ;
#7394 = VERTEX_POINT('',#63103) ;
#7395 = VERTEX_POINT('',#63104) ;
#7396 = VERTEX_POINT('',#63106) ;
#7397 = VERTEX_POINT('',#63288) ;
#7398 = VERTEX_POINT('',#63290) ;
#7399 = VERTEX_POINT('',#63294) ;
#7400 = VERTEX_POINT('',#63296) ;
#7401 = VERTEX_POINT('',#63300) ;
#7402 = VERTEX_POINT('',#63302) ;
#7403 = VERTEX_POINT('',#63306) ;
#7404 = VERTEX_POINT('',#63308) ;
#7405 = VERTEX_POINT('',#63312) ;
#7406 = VERTEX_POINT('',#63316) ;
#7407 = VERTEX_POINT('',#63619) ;
#7408 = VERTEX_POINT('',#63621) ;
#7409 = VERTEX_POINT('',#63625) ;
#7410 = VERTEX_POINT('',#63628) ;
#7411 = VERTEX_POINT('',#63632) ;
#7412 = VERTEX_POINT('',#63636) ;
#7413 = VERTEX_POINT('',#63640) ;
#7414 = VERTEX_POINT('',#63644) ;
#7415 = VERTEX_POINT('',#63650) ;
#7416 = VERTEX_POINT('',#63652) ;
#7417 = VERTEX_POINT('',#63656) ;
#7418 = VERTEX_POINT('',#63658) ;
#7419 = VERTEX_POINT('',#63662) ;
#7420 = VERTEX_POINT('',#63664) ;
#7421 = VERTEX_POINT('',#63668) ;
#7422 = VERTEX_POINT('',#63670) ;
#7423 = VERTEX_POINT('',#63674) ;
#7424 = VERTEX_POINT('',#63676) ;
#7425 = VERTEX_POINT('',#63680) ;
#7426 = VERTEX_POINT('',#63682) ;
#7427 = VERTEX_POINT('',#63686) ;
#7428 = VERTEX_POINT('',#63688) ;
#7429 = VERTEX_POINT('',#63692) ;
#7430 = VERTEX_POINT('',#63694) ;
#7431 = VERTEX_POINT('',#63698) ;
#7432 = VERTEX_POINT('',#63700) ;
#7433 = VERTEX_POINT('',#63704) ;
#7434 = VERTEX_POINT('',#63706) ;
#7435 = VERTEX_POINT('',#63713) ;
#7436 = VERTEX_POINT('',#63715) ;
#7437 = VERTEX_POINT('',#63719) ;
#7438 = VERTEX_POINT('',#63721) ;
#7439 = VERTEX_POINT('',#63725) ;
#7440 = VERTEX_POINT('',#63727) ;
#7441 = VERTEX_POINT('',#63731) ;
#7442 = VERTEX_POINT('',#63733) ;
#7443 = VERTEX_POINT('',#63737) ;
#7444 = VERTEX_POINT('',#63739) ;
#7445 = VERTEX_POINT('',#63743) ;
#7446 = VERTEX_POINT('',#63745) ;
#7447 = VERTEX_POINT('',#63749) ;
#7448 = VERTEX_POINT('',#63751) ;
#7449 = VERTEX_POINT('',#63755) ;
#7450 = VERTEX_POINT('',#63757) ;
#7451 = VERTEX_POINT('',#63761) ;
#7452 = VERTEX_POINT('',#63763) ;
#7453 = VERTEX_POINT('',#63767) ;
#7454 = VERTEX_POINT('',#63769) ;
#7455 = EDGE_CURVE('',#6002,#6003,#4690,.T.) ;
#7456 = EDGE_CURVE('',#6003,#6003,#3474,.T.) ;
#7457 = EDGE_CURVE('',#6004,#6004,#3475,.T.) ;
#7458 = EDGE_CURVE('',#6004,#6003,#4691,.T.) ;
#7459 = EDGE_CURVE('',#6005,#6006,#4692,.T.) ;
#7460 = EDGE_CURVE('',#6006,#6006,#3476,.T.) ;
#7461 = EDGE_CURVE('',#6007,#6007,#3477,.T.) ;
#7462 = EDGE_CURVE('',#6007,#6006,#4693,.T.) ;
#7463 = EDGE_CURVE('',#6008,#6009,#4694,.T.) ;
#7464 = EDGE_CURVE('',#6009,#6009,#3478,.T.) ;
#7465 = EDGE_CURVE('',#6010,#6010,#3479,.T.) ;
#7466 = EDGE_CURVE('',#6010,#6009,#4695,.T.) ;
#7467 = EDGE_CURVE('',#6011,#6012,#4696,.T.) ;
#7468 = EDGE_CURVE('',#6012,#6012,#3480,.T.) ;
#7469 = EDGE_CURVE('',#6013,#6013,#3481,.T.) ;
#7470 = EDGE_CURVE('',#6013,#6012,#4697,.T.) ;
#7471 = EDGE_CURVE('',#6014,#6014,#3482,.T.) ;
#7472 = EDGE_CURVE('',#6015,#6015,#3483,.T.) ;
#7473 = EDGE_CURVE('',#6016,#6016,#3484,.T.) ;
#7474 = EDGE_CURVE('',#6016,#6014,#4698,.T.) ;
#7475 = EDGE_CURVE('',#6015,#6017,#4699,.T.) ;
#7476 = EDGE_CURVE('',#6017,#6017,#3485,.T.) ;
#7477 = EDGE_CURVE('',#6018,#6018,#3486,.T.) ;
#7478 = EDGE_CURVE('',#6019,#6019,#3487,.T.) ;
#7479 = EDGE_CURVE('',#6020,#6020,#3488,.T.) ;
#7480 = EDGE_CURVE('',#6020,#6018,#4700,.T.) ;
#7481 = EDGE_CURVE('',#6019,#6021,#4701,.T.) ;
#7482 = EDGE_CURVE('',#6021,#6021,#3489,.T.) ;
#7483 = EDGE_CURVE('',#6022,#6022,#3490,.T.) ;
#7484 = EDGE_CURVE('',#6023,#6023,#3491,.T.) ;
#7485 = EDGE_CURVE('',#6024,#6024,#3492,.T.) ;
#7486 = EDGE_CURVE('',#6024,#6022,#4702,.T.) ;
#7487 = EDGE_CURVE('',#6023,#6025,#4703,.T.) ;
#7488 = EDGE_CURVE('',#6025,#6025,#3493,.T.) ;
#7489 = EDGE_CURVE('',#6026,#6026,#3494,.T.) ;
#7490 = EDGE_CURVE('',#6027,#6027,#3495,.T.) ;
#7491 = EDGE_CURVE('',#6028,#6028,#3496,.T.) ;
#7492 = EDGE_CURVE('',#6028,#6026,#4704,.T.) ;
#7493 = EDGE_CURVE('',#6027,#6029,#4705,.T.) ;
#7494 = EDGE_CURVE('',#6029,#6029,#3497,.T.) ;
#7495 = EDGE_CURVE('',#6030,#6031,#4706,.T.) ;
#7496 = EDGE_CURVE('',#6031,#6031,#3498,.T.) ;
#7497 = EDGE_CURVE('',#6032,#6032,#3499,.T.) ;
#7498 = EDGE_CURVE('',#6032,#6031,#4707,.T.) ;
#7499 = EDGE_CURVE('',#6033,#6034,#4708,.T.) ;
#7500 = EDGE_CURVE('',#6034,#6034,#3500,.T.) ;
#7501 = EDGE_CURVE('',#6035,#6035,#3501,.F.) ;
#7502 = EDGE_CURVE('',#6035,#6034,#4709,.T.) ;
#7503 = EDGE_CURVE('',#6036,#6037,#4710,.T.) ;
#7504 = EDGE_CURVE('',#6037,#6037,#3502,.T.) ;
#7505 = EDGE_CURVE('',#6038,#6038,#3503,.F.) ;
#7506 = EDGE_CURVE('',#6038,#6037,#4711,.T.) ;
#7507 = EDGE_CURVE('',#6039,#6040,#4712,.T.) ;
#7508 = EDGE_CURVE('',#6040,#6040,#3504,.T.) ;
#7509 = EDGE_CURVE('',#6041,#6041,#3505,.F.) ;
#7510 = EDGE_CURVE('',#6041,#6040,#4713,.T.) ;
#7511 = EDGE_CURVE('',#6042,#6043,#4714,.T.) ;
#7512 = EDGE_CURVE('',#6043,#6043,#3506,.T.) ;
#7513 = EDGE_CURVE('',#6044,#6044,#3507,.F.) ;
#7514 = EDGE_CURVE('',#6044,#6043,#4715,.T.) ;
#7515 = EDGE_CURVE('',#6045,#6046,#4716,.T.) ;
#7516 = EDGE_CURVE('',#6046,#6046,#3508,.T.) ;
#7517 = EDGE_CURVE('',#6047,#6047,#3509,.F.) ;
#7518 = EDGE_CURVE('',#6047,#6046,#4717,.T.) ;
#7519 = EDGE_CURVE('',#6048,#6049,#4718,.T.) ;
#7520 = EDGE_CURVE('',#6049,#6049,#3510,.T.) ;
#7521 = EDGE_CURVE('',#6050,#6050,#3511,.F.) ;
#7522 = EDGE_CURVE('',#6050,#6049,#4719,.T.) ;
#7523 = EDGE_CURVE('',#6051,#6052,#4720,.T.) ;
#7524 = EDGE_CURVE('',#6052,#6052,#3512,.T.) ;
#7525 = EDGE_CURVE('',#6053,#6053,#3513,.T.) ;
#7526 = EDGE_CURVE('',#6053,#6052,#4721,.T.) ;
#7527 = EDGE_CURVE('',#6054,#6054,#3514,.T.) ;
#7528 = EDGE_CURVE('',#6054,#6055,#4722,.T.) ;
#7529 = EDGE_CURVE('',#6055,#6055,#3515,.T.) ;
#7530 = EDGE_CURVE('',#6056,#6057,#4723,.T.) ;
#7531 = EDGE_CURVE('',#6056,#6058,#4724,.T.) ;
#7532 = EDGE_CURVE('',#6059,#6058,#4725,.T.) ;
#7533 = EDGE_CURVE('',#6057,#6059,#4726,.T.) ;
#7534 = EDGE_CURVE('',#6057,#6060,#4727,.T.) ;
#7535 = EDGE_CURVE('',#6061,#6059,#4728,.T.) ;
#7536 = EDGE_CURVE('',#6060,#6061,#4729,.T.) ;
#7537 = EDGE_CURVE('',#6062,#6060,#4730,.T.) ;
#7538 = EDGE_CURVE('',#6063,#6061,#4731,.T.) ;
#7539 = EDGE_CURVE('',#6062,#6063,#4732,.T.) ;
#7540 = EDGE_CURVE('',#6062,#6056,#4733,.T.) ;
#7541 = EDGE_CURVE('',#6058,#6063,#4734,.T.) ;
#7542 = EDGE_CURVE('',#6064,#6064,#3516,.T.) ;
#7543 = EDGE_CURVE('',#6065,#6065,#3517,.T.) ;
#7544 = EDGE_CURVE('',#6066,#6066,#3518,.T.) ;
#7545 = EDGE_CURVE('',#6066,#6064,#4735,.T.) ;
#7546 = EDGE_CURVE('',#6065,#6067,#4736,.T.) ;
#7547 = EDGE_CURVE('',#6067,#6067,#3519,.T.) ;
#7548 = EDGE_CURVE('',#6068,#6068,#3520,.T.) ;
#7549 = EDGE_CURVE('',#6069,#6069,#3521,.T.) ;
#7550 = EDGE_CURVE('',#6070,#6070,#3522,.T.) ;
#7551 = EDGE_CURVE('',#6070,#6068,#4737,.T.) ;
#7552 = EDGE_CURVE('',#6069,#6071,#4738,.T.) ;
#7553 = EDGE_CURVE('',#6071,#6071,#3523,.T.) ;
#7554 = EDGE_CURVE('',#6072,#6072,#3524,.T.) ;
#7555 = EDGE_CURVE('',#6073,#6073,#3525,.T.) ;
#7556 = EDGE_CURVE('',#6074,#6074,#3526,.T.) ;
#7557 = EDGE_CURVE('',#6074,#6072,#4739,.T.) ;
#7558 = EDGE_CURVE('',#6073,#6075,#4740,.T.) ;
#7559 = EDGE_CURVE('',#6075,#6075,#3527,.T.) ;
#7560 = EDGE_CURVE('',#6076,#6076,#3528,.T.) ;
#7561 = EDGE_CURVE('',#6077,#6077,#3529,.T.) ;
#7562 = EDGE_CURVE('',#6078,#6078,#3530,.T.) ;
#7563 = EDGE_CURVE('',#6078,#6076,#4741,.T.) ;
#7564 = EDGE_CURVE('',#6077,#6079,#4742,.T.) ;
#7565 = EDGE_CURVE('',#6079,#6079,#3531,.T.) ;
#7566 = EDGE_CURVE('',#6080,#6080,#3532,.T.) ;
#7567 = EDGE_CURVE('',#6081,#6081,#3533,.T.) ;
#7568 = EDGE_CURVE('',#6082,#6082,#3534,.T.) ;
#7569 = EDGE_CURVE('',#6082,#6080,#4743,.T.) ;
#7570 = EDGE_CURVE('',#6081,#6083,#4744,.T.) ;
#7571 = EDGE_CURVE('',#6083,#6083,#3535,.T.) ;
#7572 = EDGE_CURVE('',#6084,#6084,#3536,.T.) ;
#7573 = EDGE_CURVE('',#6085,#6085,#3537,.T.) ;
#7574 = EDGE_CURVE('',#6086,#6086,#3538,.T.) ;
#7575 = EDGE_CURVE('',#6086,#6084,#4745,.T.) ;
#7576 = EDGE_CURVE('',#6085,#6087,#4746,.T.) ;
#7577 = EDGE_CURVE('',#6087,#6087,#3539,.T.) ;
#7578 = EDGE_CURVE('',#6088,#6088,#3540,.T.) ;
#7579 = EDGE_CURVE('',#6089,#6089,#3541,.T.) ;
#7580 = EDGE_CURVE('',#6090,#6090,#3542,.T.) ;
#7581 = EDGE_CURVE('',#6090,#6088,#4747,.T.) ;
#7582 = EDGE_CURVE('',#6089,#6091,#4748,.T.) ;
#7583 = EDGE_CURVE('',#6091,#6091,#3543,.T.) ;
#7584 = EDGE_CURVE('',#6092,#6092,#3544,.T.) ;
#7585 = EDGE_CURVE('',#6093,#6093,#3545,.T.) ;
#7586 = EDGE_CURVE('',#6094,#6094,#3546,.T.) ;
#7587 = EDGE_CURVE('',#6094,#6092,#4749,.T.) ;
#7588 = EDGE_CURVE('',#6093,#6095,#4750,.T.) ;
#7589 = EDGE_CURVE('',#6095,#6095,#3547,.T.) ;
#7590 = EDGE_CURVE('',#6096,#6096,#3548,.T.) ;
#7591 = EDGE_CURVE('',#6097,#6097,#3549,.T.) ;
#7592 = EDGE_CURVE('',#6098,#6098,#3550,.T.) ;
#7593 = EDGE_CURVE('',#6098,#6096,#4751,.T.) ;
#7594 = EDGE_CURVE('',#6097,#6099,#4752,.T.) ;
#7595 = EDGE_CURVE('',#6099,#6099,#3551,.T.) ;
#7596 = EDGE_CURVE('',#6100,#6100,#3552,.T.) ;
#7597 = EDGE_CURVE('',#6101,#6101,#3553,.T.) ;
#7598 = EDGE_CURVE('',#6102,#6102,#3554,.T.) ;
#7599 = EDGE_CURVE('',#6102,#6100,#4753,.T.) ;
#7600 = EDGE_CURVE('',#6101,#6103,#4754,.T.) ;
#7601 = EDGE_CURVE('',#6103,#6103,#3555,.T.) ;
#7602 = EDGE_CURVE('',#6104,#6104,#3556,.T.) ;
#7603 = EDGE_CURVE('',#6105,#6105,#3557,.T.) ;
#7604 = EDGE_CURVE('',#6106,#6106,#3558,.T.) ;
#7605 = EDGE_CURVE('',#6106,#6104,#4755,.T.) ;
#7606 = EDGE_CURVE('',#6105,#6107,#4756,.T.) ;
#7607 = EDGE_CURVE('',#6107,#6107,#3559,.T.) ;
#7608 = EDGE_CURVE('',#6108,#6108,#3560,.T.) ;
#7609 = EDGE_CURVE('',#6109,#6109,#3561,.T.) ;
#7610 = EDGE_CURVE('',#6110,#6110,#3562,.T.) ;
#7611 = EDGE_CURVE('',#6110,#6108,#4757,.T.) ;
#7612 = EDGE_CURVE('',#6109,#6111,#4758,.T.) ;
#7613 = EDGE_CURVE('',#6111,#6111,#3563,.T.) ;
#7614 = EDGE_CURVE('',#6112,#6113,#4759,.T.) ;
#7615 = EDGE_CURVE('',#6114,#6113,#4760,.T.) ;
#7616 = EDGE_CURVE('',#6114,#6115,#4761,.T.) ;
#7617 = EDGE_CURVE('',#6115,#6112,#4762,.T.) ;
#7618 = EDGE_CURVE('',#6113,#6116,#4763,.T.) ;
#7619 = EDGE_CURVE('',#6117,#6116,#4764,.T.) ;
#7620 = EDGE_CURVE('',#6117,#6114,#4765,.T.) ;
#7621 = EDGE_CURVE('',#6116,#6118,#4766,.T.) ;
#7622 = EDGE_CURVE('',#6119,#6118,#4767,.T.) ;
#7623 = EDGE_CURVE('',#6119,#6117,#4768,.T.) ;
#7624 = EDGE_CURVE('',#6118,#6112,#4769,.T.) ;
#7625 = EDGE_CURVE('',#6115,#6119,#4770,.T.) ;
#7626 = EDGE_CURVE('',#6120,#6121,#4771,.T.) ;
#7627 = EDGE_CURVE('',#6121,#6121,#3564,.T.) ;
#7628 = EDGE_CURVE('',#6122,#6122,#3565,.T.) ;
#7629 = EDGE_CURVE('',#6122,#6121,#4772,.T.) ;
#7630 = EDGE_CURVE('',#6123,#6124,#4773,.T.) ;
#7631 = EDGE_CURVE('',#6124,#6124,#3566,.T.) ;
#7632 = EDGE_CURVE('',#6125,#6125,#3567,.T.) ;
#7633 = EDGE_CURVE('',#6125,#6124,#4774,.T.) ;
#7634 = EDGE_CURVE('',#6126,#6127,#4775,.T.) ;
#7635 = EDGE_CURVE('',#6127,#6127,#3568,.T.) ;
#7636 = EDGE_CURVE('',#6128,#6128,#3569,.T.) ;
#7637 = EDGE_CURVE('',#6128,#6127,#4776,.T.) ;
#7638 = EDGE_CURVE('',#6129,#6130,#4777,.T.) ;
#7639 = EDGE_CURVE('',#6130,#6130,#3570,.T.) ;
#7640 = EDGE_CURVE('',#6131,#6131,#3571,.T.) ;
#7641 = EDGE_CURVE('',#6131,#6130,#4778,.T.) ;
#7642 = EDGE_CURVE('',#6132,#6133,#4779,.T.) ;
#7643 = EDGE_CURVE('',#6133,#6133,#3572,.T.) ;
#7644 = EDGE_CURVE('',#6133,#6134,#4780,.T.) ;
#7645 = EDGE_CURVE('',#6134,#6134,#3573,.F.) ;
#7646 = EDGE_CURVE('',#6135,#6136,#4781,.T.) ;
#7647 = EDGE_CURVE('',#6136,#6136,#3574,.T.) ;
#7648 = EDGE_CURVE('',#6136,#6137,#4782,.T.) ;
#7649 = EDGE_CURVE('',#6137,#6137,#3575,.F.) ;
#7650 = EDGE_CURVE('',#6138,#6139,#4783,.T.) ;
#7651 = EDGE_CURVE('',#6140,#6138,#4784,.T.) ;
#7652 = EDGE_CURVE('',#6141,#6140,#4785,.T.) ;
#7653 = EDGE_CURVE('',#6139,#6141,#4786,.T.) ;
#7654 = EDGE_CURVE('',#6142,#6143,#4787,.T.) ;
#7655 = EDGE_CURVE('',#6143,#6143,#3576,.T.) ;
#7656 = EDGE_CURVE('',#6144,#6144,#3577,.F.) ;
#7657 = EDGE_CURVE('',#6144,#6143,#4788,.T.) ;
#7658 = EDGE_CURVE('',#6145,#6146,#4789,.T.) ;
#7659 = EDGE_CURVE('',#6146,#6146,#3578,.T.) ;
#7660 = EDGE_CURVE('',#6147,#6147,#3579,.F.) ;
#7661 = EDGE_CURVE('',#6147,#6146,#4790,.T.) ;
#7662 = EDGE_CURVE('',#6148,#6149,#4791,.T.) ;
#7663 = EDGE_CURVE('',#6148,#6139,#4792,.T.) ;
#7664 = EDGE_CURVE('',#6149,#6141,#4793,.T.) ;
#7665 = EDGE_CURVE('',#6149,#6150,#4794,.T.) ;
#7666 = EDGE_CURVE('',#6150,#6140,#4795,.T.) ;
#7667 = EDGE_CURVE('',#6150,#6151,#4796,.T.) ;
#7668 = EDGE_CURVE('',#6151,#6138,#4797,.T.) ;
#7669 = EDGE_CURVE('',#6151,#6148,#4798,.T.) ;
#7670 = EDGE_CURVE('',#6152,#6153,#4799,.T.) ;
#7671 = EDGE_CURVE('',#6153,#6153,#3580,.T.) ;
#7672 = EDGE_CURVE('',#6154,#6154,#3581,.T.) ;
#7673 = EDGE_CURVE('',#6154,#6153,#4800,.T.) ;
#7674 = EDGE_CURVE('',#6155,#6156,#4801,.T.) ;
#7675 = EDGE_CURVE('',#6156,#6156,#3582,.T.) ;
#7676 = EDGE_CURVE('',#6157,#6157,#3583,.T.) ;
#7677 = EDGE_CURVE('',#6157,#6156,#4802,.T.) ;
#7678 = EDGE_CURVE('',#6158,#6159,#4803,.T.) ;
#7679 = EDGE_CURVE('',#6159,#6159,#3584,.T.) ;
#7680 = EDGE_CURVE('',#6160,#6160,#3585,.T.) ;
#7681 = EDGE_CURVE('',#6160,#6159,#4804,.T.) ;
#7682 = EDGE_CURVE('',#6161,#6162,#4805,.T.) ;
#7683 = EDGE_CURVE('',#6162,#6162,#3586,.T.) ;
#7684 = EDGE_CURVE('',#6163,#6163,#3587,.T.) ;
#7685 = EDGE_CURVE('',#6163,#6162,#4806,.T.) ;
#7686 = EDGE_CURVE('',#6164,#6165,#4807,.T.) ;
#7687 = EDGE_CURVE('',#6165,#6165,#3588,.T.) ;
#7688 = EDGE_CURVE('',#6166,#6166,#3589,.T.) ;
#7689 = EDGE_CURVE('',#6166,#6165,#4808,.T.) ;
#7690 = EDGE_CURVE('',#6167,#6168,#4809,.T.) ;
#7691 = EDGE_CURVE('',#6168,#6168,#3590,.T.) ;
#7692 = EDGE_CURVE('',#6169,#6169,#3591,.T.) ;
#7693 = EDGE_CURVE('',#6169,#6168,#4810,.T.) ;
#7694 = EDGE_CURVE('',#6170,#6170,#3592,.T.) ;
#7695 = EDGE_CURVE('',#6171,#6171,#3593,.T.) ;
#7696 = EDGE_CURVE('',#6170,#6172,#4811,.T.) ;
#7697 = EDGE_CURVE('',#6172,#6172,#3594,.T.) ;
#7698 = EDGE_CURVE('',#6173,#6173,#3595,.T.) ;
#7699 = EDGE_CURVE('',#6173,#6171,#4812,.T.) ;
#7700 = EDGE_CURVE('',#6174,#6174,#3596,.T.) ;
#7701 = EDGE_CURVE('',#6175,#6175,#3597,.T.) ;
#7702 = EDGE_CURVE('',#6174,#6176,#4813,.T.) ;
#7703 = EDGE_CURVE('',#6176,#6176,#3598,.T.) ;
#7704 = EDGE_CURVE('',#6177,#6177,#3599,.T.) ;
#7705 = EDGE_CURVE('',#6177,#6175,#4814,.T.) ;
#7706 = EDGE_CURVE('',#6178,#6178,#3600,.T.) ;
#7707 = EDGE_CURVE('',#6179,#6179,#3601,.T.) ;
#7708 = EDGE_CURVE('',#6178,#6180,#4815,.T.) ;
#7709 = EDGE_CURVE('',#6180,#6180,#3602,.T.) ;
#7710 = EDGE_CURVE('',#6181,#6181,#3603,.T.) ;
#7711 = EDGE_CURVE('',#6181,#6179,#4816,.T.) ;
#7712 = EDGE_CURVE('',#6182,#6182,#3604,.T.) ;
#7713 = EDGE_CURVE('',#6183,#6183,#3605,.T.) ;
#7714 = EDGE_CURVE('',#6182,#6184,#4817,.T.) ;
#7715 = EDGE_CURVE('',#6184,#6184,#3606,.T.) ;
#7716 = EDGE_CURVE('',#6185,#6185,#3607,.T.) ;
#7717 = EDGE_CURVE('',#6185,#6183,#4818,.T.) ;
#7718 = EDGE_CURVE('',#6186,#6187,#4819,.T.) ;
#7719 = EDGE_CURVE('',#6187,#6187,#3608,.T.) ;
#7720 = EDGE_CURVE('',#6187,#6188,#4820,.T.) ;
#7721 = EDGE_CURVE('',#6188,#6188,#3609,.T.) ;
#7722 = EDGE_CURVE('',#6189,#6190,#4821,.T.) ;
#7723 = EDGE_CURVE('',#6190,#6190,#3610,.T.) ;
#7724 = EDGE_CURVE('',#6190,#6191,#4822,.T.) ;
#7725 = EDGE_CURVE('',#6191,#6191,#3611,.F.) ;
#7726 = EDGE_CURVE('',#6192,#6193,#4823,.T.) ;
#7727 = EDGE_CURVE('',#6193,#6193,#3612,.T.) ;
#7728 = EDGE_CURVE('',#6193,#6194,#4824,.T.) ;
#7729 = EDGE_CURVE('',#6194,#6194,#3613,.F.) ;
#7730 = EDGE_CURVE('',#6195,#6196,#4825,.T.) ;
#7731 = EDGE_CURVE('',#6196,#6196,#3614,.T.) ;
#7732 = EDGE_CURVE('',#6196,#6197,#4826,.T.) ;
#7733 = EDGE_CURVE('',#6197,#6197,#3615,.F.) ;
#7734 = EDGE_CURVE('',#6198,#6199,#4827,.T.) ;
#7735 = EDGE_CURVE('',#6199,#6199,#3616,.T.) ;
#7736 = EDGE_CURVE('',#6199,#6200,#4828,.T.) ;
#7737 = EDGE_CURVE('',#6200,#6200,#3617,.F.) ;
#7738 = EDGE_CURVE('',#6201,#6202,#4829,.T.) ;
#7739 = EDGE_CURVE('',#6202,#6202,#3618,.T.) ;
#7740 = EDGE_CURVE('',#6202,#6203,#4830,.T.) ;
#7741 = EDGE_CURVE('',#6203,#6203,#3619,.F.) ;
#7742 = EDGE_CURVE('',#6204,#6205,#4831,.T.) ;
#7743 = EDGE_CURVE('',#6205,#6205,#3620,.T.) ;
#7744 = EDGE_CURVE('',#6205,#6206,#4832,.T.) ;
#7745 = EDGE_CURVE('',#6206,#6206,#3621,.F.) ;
#7746 = EDGE_CURVE('',#6207,#6208,#4833,.T.) ;
#7747 = EDGE_CURVE('',#6208,#6208,#3622,.T.) ;
#7748 = EDGE_CURVE('',#6208,#6209,#4834,.T.) ;
#7749 = EDGE_CURVE('',#6209,#6209,#3623,.T.) ;
#7750 = EDGE_CURVE('',#6210,#6210,#3624,.T.) ;
#7751 = EDGE_CURVE('',#6210,#6211,#4835,.T.) ;
#7752 = EDGE_CURVE('',#6211,#6211,#3625,.T.) ;
#7753 = EDGE_CURVE('',#6212,#6213,#4836,.T.) ;
#7754 = EDGE_CURVE('',#6213,#6214,#4837,.T.) ;
#7755 = EDGE_CURVE('',#6214,#6215,#4838,.T.) ;
#7756 = EDGE_CURVE('',#6212,#6215,#4839,.T.) ;
#7757 = EDGE_CURVE('',#6213,#6216,#4840,.T.) ;
#7758 = EDGE_CURVE('',#6216,#6217,#4841,.T.) ;
#7759 = EDGE_CURVE('',#6217,#6214,#4842,.T.) ;
#7760 = EDGE_CURVE('',#6218,#6216,#4843,.T.) ;
#7761 = EDGE_CURVE('',#6218,#6219,#4844,.T.) ;
#7762 = EDGE_CURVE('',#6219,#6217,#4845,.T.) ;
#7763 = EDGE_CURVE('',#6218,#6212,#4846,.T.) ;
#7764 = EDGE_CURVE('',#6215,#6219,#4847,.T.) ;
#7765 = EDGE_CURVE('',#6220,#6221,#4848,.T.) ;
#7766 = EDGE_CURVE('',#6221,#6221,#3626,.T.) ;
#7767 = EDGE_CURVE('',#6222,#6222,#3627,.T.) ;
#7768 = EDGE_CURVE('',#6222,#6221,#4849,.T.) ;
#7769 = EDGE_CURVE('',#6223,#6224,#4850,.T.) ;
#7770 = EDGE_CURVE('',#6224,#6224,#3628,.T.) ;
#7771 = EDGE_CURVE('',#6225,#6225,#3629,.T.) ;
#7772 = EDGE_CURVE('',#6225,#6224,#4851,.T.) ;
#7773 = EDGE_CURVE('',#6226,#6227,#4852,.T.) ;
#7774 = EDGE_CURVE('',#6227,#6227,#3630,.T.) ;
#7775 = EDGE_CURVE('',#6228,#6228,#3631,.T.) ;
#7776 = EDGE_CURVE('',#6228,#6227,#4853,.T.) ;
#7777 = EDGE_CURVE('',#6229,#6230,#4854,.T.) ;
#7778 = EDGE_CURVE('',#6230,#6230,#3632,.T.) ;
#7779 = EDGE_CURVE('',#6231,#6231,#3633,.T.) ;
#7780 = EDGE_CURVE('',#6231,#6230,#4855,.T.) ;
#7781 = EDGE_CURVE('',#6232,#6233,#4856,.T.) ;
#7782 = EDGE_CURVE('',#6233,#6233,#3634,.T.) ;
#7783 = EDGE_CURVE('',#6234,#6234,#3635,.F.) ;
#7784 = EDGE_CURVE('',#6234,#6233,#4857,.T.) ;
#7785 = EDGE_CURVE('',#6235,#6236,#4858,.T.) ;
#7786 = EDGE_CURVE('',#6236,#6236,#3636,.T.) ;
#7787 = EDGE_CURVE('',#6237,#6237,#3637,.F.) ;
#7788 = EDGE_CURVE('',#6237,#6236,#4859,.T.) ;
#7789 = EDGE_CURVE('',#6238,#6239,#4860,.T.) ;
#7790 = EDGE_CURVE('',#6239,#6240,#4861,.T.) ;
#7791 = EDGE_CURVE('',#6240,#6241,#4862,.T.) ;
#7792 = EDGE_CURVE('',#6241,#6238,#4863,.T.) ;
#7793 = EDGE_CURVE('',#6242,#6243,#4864,.T.) ;
#7794 = EDGE_CURVE('',#6243,#6243,#3638,.T.) ;
#7795 = EDGE_CURVE('',#6243,#6244,#4865,.T.) ;
#7796 = EDGE_CURVE('',#6244,#6244,#3639,.F.) ;
#7797 = EDGE_CURVE('',#6245,#6246,#4866,.T.) ;
#7798 = EDGE_CURVE('',#6246,#6246,#3640,.T.) ;
#7799 = EDGE_CURVE('',#6246,#6247,#4867,.T.) ;
#7800 = EDGE_CURVE('',#6247,#6247,#3641,.F.) ;
#7801 = EDGE_CURVE('',#6248,#6249,#4868,.T.) ;
#7802 = EDGE_CURVE('',#6249,#6240,#4869,.T.) ;
#7803 = EDGE_CURVE('',#6248,#6239,#4870,.T.) ;
#7804 = EDGE_CURVE('',#6249,#6250,#4871,.T.) ;
#7805 = EDGE_CURVE('',#6250,#6241,#4872,.T.) ;
#7806 = EDGE_CURVE('',#6250,#6251,#4873,.T.) ;
#7807 = EDGE_CURVE('',#6251,#6238,#4874,.T.) ;
#7808 = EDGE_CURVE('',#6251,#6248,#4875,.T.) ;
#7809 = EDGE_CURVE('',#6252,#6253,#4876,.T.) ;
#7810 = EDGE_CURVE('',#6252,#6254,#222,.F.) ;
#7811 = EDGE_CURVE('',#6254,#6255,#3642,.T.) ;
#7812 = EDGE_CURVE('',#6255,#6253,#223,.T.) ;
#7813 = EDGE_CURVE('',#6256,#6257,#4877,.T.) ;
#7814 = EDGE_CURVE('',#6256,#6252,#224,.F.) ;
#7815 = EDGE_CURVE('',#6253,#6257,#225,.T.) ;
#7816 = EDGE_CURVE('',#6258,#6259,#4878,.T.) ;
#7817 = EDGE_CURVE('',#6258,#6256,#226,.T.) ;
#7818 = EDGE_CURVE('',#6257,#6259,#227,.T.) ;
#7819 = EDGE_CURVE('',#6260,#6261,#4879,.T.) ;
#7820 = EDGE_CURVE('',#6260,#6258,#228,.T.) ;
#7821 = EDGE_CURVE('',#6259,#6261,#229,.T.) ;
#7822 = EDGE_CURVE('',#6262,#6263,#4880,.T.) ;
#7823 = EDGE_CURVE('',#6262,#6260,#230,.T.) ;
#7824 = EDGE_CURVE('',#6261,#6263,#231,.T.) ;
#7825 = EDGE_CURVE('',#6264,#6265,#4881,.T.) ;
#7826 = EDGE_CURVE('',#6264,#6262,#232,.T.) ;
#7827 = EDGE_CURVE('',#6263,#6265,#233,.T.) ;
#7828 = EDGE_CURVE('',#6266,#6267,#4882,.T.) ;
#7829 = EDGE_CURVE('',#6266,#6264,#234,.T.) ;
#7830 = EDGE_CURVE('',#6265,#6267,#235,.T.) ;
#7831 = EDGE_CURVE('',#6268,#6269,#4883,.T.) ;
#7832 = EDGE_CURVE('',#6268,#6266,#236,.T.) ;
#7833 = EDGE_CURVE('',#6267,#6269,#237,.T.) ;
#7834 = EDGE_CURVE('',#6270,#6271,#4884,.T.) ;
#7835 = EDGE_CURVE('',#6270,#6268,#238,.T.) ;
#7836 = EDGE_CURVE('',#6269,#6271,#239,.T.) ;
#7837 = EDGE_CURVE('',#6272,#6273,#4885,.T.) ;
#7838 = EDGE_CURVE('',#6272,#6270,#240,.T.) ;
#7839 = EDGE_CURVE('',#6271,#6273,#241,.T.) ;
#7840 = EDGE_CURVE('',#6274,#6275,#4886,.T.) ;
#7841 = EDGE_CURVE('',#6274,#6272,#242,.T.) ;
#7842 = EDGE_CURVE('',#6273,#6275,#243,.T.) ;
#7843 = EDGE_CURVE('',#6276,#6277,#4887,.T.) ;
#7844 = EDGE_CURVE('',#6276,#6274,#244,.T.) ;
#7845 = EDGE_CURVE('',#6275,#6277,#245,.T.) ;
#7846 = EDGE_CURVE('',#6278,#6279,#4888,.T.) ;
#7847 = EDGE_CURVE('',#6278,#6276,#246,.T.) ;
#7848 = EDGE_CURVE('',#6277,#6279,#247,.T.) ;
#7849 = EDGE_CURVE('',#6280,#6281,#4889,.T.) ;
#7850 = EDGE_CURVE('',#6280,#6282,#248,.T.) ;
#7851 = EDGE_CURVE('',#6282,#6283,#3643,.T.) ;
#7852 = EDGE_CURVE('',#6283,#6281,#249,.T.) ;
#7853 = EDGE_CURVE('',#6284,#6285,#4890,.T.) ;
#7854 = EDGE_CURVE('',#6284,#6280,#250,.T.) ;
#7855 = EDGE_CURVE('',#6281,#6285,#251,.T.) ;
#7856 = EDGE_CURVE('',#6286,#6287,#4891,.T.) ;
#7857 = EDGE_CURVE('',#6286,#6284,#252,.T.) ;
#7858 = EDGE_CURVE('',#6285,#6287,#253,.T.) ;
#7859 = EDGE_CURVE('',#6288,#6289,#4892,.T.) ;
#7860 = EDGE_CURVE('',#6288,#6286,#254,.T.) ;
#7861 = EDGE_CURVE('',#6287,#6289,#255,.T.) ;
#7862 = EDGE_CURVE('',#6290,#6291,#4893,.T.) ;
#7863 = EDGE_CURVE('',#6290,#6288,#256,.T.) ;
#7864 = EDGE_CURVE('',#6289,#6291,#257,.T.) ;
#7865 = EDGE_CURVE('',#6292,#6293,#4894,.T.) ;
#7866 = EDGE_CURVE('',#6292,#6290,#258,.T.) ;
#7867 = EDGE_CURVE('',#6291,#6293,#259,.T.) ;
#7868 = EDGE_CURVE('',#6294,#6295,#4895,.T.) ;
#7869 = EDGE_CURVE('',#6296,#6294,#3644,.F.) ;
#7870 = EDGE_CURVE('',#6296,#6292,#260,.T.) ;
#7871 = EDGE_CURVE('',#6293,#6295,#261,.T.) ;
#7872 = EDGE_CURVE('',#6297,#6298,#4896,.T.) ;
#7873 = EDGE_CURVE('',#6299,#6297,#262,.F.) ;
#7874 = EDGE_CURVE('',#6300,#6299,#3645,.T.) ;
#7875 = EDGE_CURVE('',#6300,#6298,#263,.T.) ;
#7876 = EDGE_CURVE('',#6301,#6302,#4897,.T.) ;
#7877 = EDGE_CURVE('',#6297,#6301,#264,.F.) ;
#7878 = EDGE_CURVE('',#6298,#6302,#265,.T.) ;
#7879 = EDGE_CURVE('',#6303,#6304,#4898,.T.) ;
#7880 = EDGE_CURVE('',#6301,#6303,#266,.F.) ;
#7881 = EDGE_CURVE('',#6302,#6304,#267,.T.) ;
#7882 = EDGE_CURVE('',#6305,#6306,#4899,.T.) ;
#7883 = EDGE_CURVE('',#6303,#6305,#268,.F.) ;
#7884 = EDGE_CURVE('',#6304,#6306,#269,.T.) ;
#7885 = EDGE_CURVE('',#6307,#6308,#4900,.T.) ;
#7886 = EDGE_CURVE('',#6305,#6307,#270,.F.) ;
#7887 = EDGE_CURVE('',#6306,#6308,#271,.T.) ;
#7888 = EDGE_CURVE('',#6309,#6310,#4901,.T.) ;
#7889 = EDGE_CURVE('',#6307,#6309,#272,.F.) ;
#7890 = EDGE_CURVE('',#6308,#6310,#273,.T.) ;
#7891 = EDGE_CURVE('',#6311,#6312,#4902,.T.) ;
#7892 = EDGE_CURVE('',#6313,#6311,#274,.F.) ;
#7893 = EDGE_CURVE('',#6314,#6313,#3646,.T.) ;
#7894 = EDGE_CURVE('',#6314,#6312,#275,.T.) ;
#7895 = EDGE_CURVE('',#6311,#6315,#276,.F.) ;
#7896 = EDGE_CURVE('',#6312,#6316,#277,.T.) ;
#7897 = EDGE_CURVE('',#6315,#6316,#4903,.T.) ;
#7898 = EDGE_CURVE('',#6317,#6318,#4904,.T.) ;
#7899 = EDGE_CURVE('',#6315,#6317,#278,.F.) ;
#7900 = EDGE_CURVE('',#6316,#6318,#279,.T.) ;
#7901 = EDGE_CURVE('',#6319,#6320,#4905,.T.) ;
#7902 = EDGE_CURVE('',#6317,#6319,#280,.F.) ;
#7903 = EDGE_CURVE('',#6318,#6321,#281,.T.) ;
#7904 = EDGE_CURVE('',#6321,#6320,#282,.T.) ;
#7905 = EDGE_CURVE('',#6322,#6323,#4906,.T.) ;
#7906 = EDGE_CURVE('',#6319,#6322,#283,.F.) ;
#7907 = EDGE_CURVE('',#6320,#6323,#284,.T.) ;
#7908 = EDGE_CURVE('',#6324,#6325,#4907,.T.) ;
#7909 = EDGE_CURVE('',#6322,#6324,#285,.F.) ;
#7910 = EDGE_CURVE('',#6323,#6325,#286,.T.) ;
#7911 = EDGE_CURVE('',#6326,#6327,#4908,.T.) ;
#7912 = EDGE_CURVE('',#6324,#6326,#287,.F.) ;
#7913 = EDGE_CURVE('',#6325,#6327,#288,.T.) ;
#7914 = EDGE_CURVE('',#6328,#6329,#4909,.T.) ;
#7915 = EDGE_CURVE('',#6326,#6328,#289,.F.) ;
#7916 = EDGE_CURVE('',#6327,#6329,#290,.T.) ;
#7917 = EDGE_CURVE('',#6330,#6331,#4910,.T.) ;
#7918 = EDGE_CURVE('',#6332,#6330,#291,.F.) ;
#7919 = EDGE_CURVE('',#6328,#6332,#292,.F.) ;
#7920 = EDGE_CURVE('',#6329,#6333,#293,.T.) ;
#7921 = EDGE_CURVE('',#6333,#6331,#294,.T.) ;
#7922 = EDGE_CURVE('',#6334,#6335,#4911,.T.) ;
#7923 = EDGE_CURVE('',#6330,#6334,#295,.F.) ;
#7924 = EDGE_CURVE('',#6331,#6335,#296,.T.) ;
#7925 = EDGE_CURVE('',#6336,#6337,#4912,.T.) ;
#7926 = EDGE_CURVE('',#6334,#6336,#297,.F.) ;
#7927 = EDGE_CURVE('',#6335,#6338,#298,.T.) ;
#7928 = EDGE_CURVE('',#6338,#6337,#299,.T.) ;
#7929 = EDGE_CURVE('',#6339,#6340,#4913,.T.) ;
#7930 = EDGE_CURVE('',#6336,#6339,#300,.F.) ;
#7931 = EDGE_CURVE('',#6337,#6340,#301,.T.) ;
#7932 = EDGE_CURVE('',#6341,#6342,#4914,.T.) ;
#7933 = EDGE_CURVE('',#6339,#6341,#302,.F.) ;
#7934 = EDGE_CURVE('',#6340,#6342,#303,.T.) ;
#7935 = EDGE_CURVE('',#6342,#6343,#304,.T.) ;
#7936 = EDGE_CURVE('',#6344,#6343,#3647,.T.) ;
#7937 = EDGE_CURVE('',#6341,#6344,#305,.F.) ;
#7938 = EDGE_CURVE('',#6310,#6345,#306,.T.) ;
#7939 = EDGE_CURVE('',#6346,#6345,#3648,.T.) ;
#7940 = EDGE_CURVE('',#6309,#6346,#307,.F.) ;
#7941 = EDGE_CURVE('',#6295,#6347,#308,.T.) ;
#7942 = EDGE_CURVE('',#6294,#6347,#3649,.F.) ;
#7943 = EDGE_CURVE('',#6279,#6348,#309,.T.) ;
#7944 = EDGE_CURVE('',#6349,#6348,#3650,.F.) ;
#7945 = EDGE_CURVE('',#6349,#6278,#310,.T.) ;
#7946 = EDGE_CURVE('',#6350,#6351,#3651,.T.) ;
#7947 = EDGE_CURVE('',#6351,#6352,#4915,.T.) ;
#7948 = EDGE_CURVE('',#6352,#6352,#3652,.T.) ;
#7949 = EDGE_CURVE('',#6351,#6350,#3653,.T.) ;
#7950 = EDGE_CURVE('',#6353,#6353,#3654,.T.) ;
#7951 = EDGE_CURVE('',#6354,#6354,#3655,.T.) ;
#7952 = EDGE_CURVE('',#6354,#6350,#4916,.T.) ;
#7953 = EDGE_CURVE('',#6355,#6356,#3656,.T.) ;
#7954 = EDGE_CURVE('',#6356,#6353,#4917,.T.) ;
#7955 = EDGE_CURVE('',#6356,#6355,#3657,.T.) ;
#7956 = EDGE_CURVE('',#6355,#6357,#4918,.T.) ;
#7957 = EDGE_CURVE('',#6357,#6357,#3658,.T.) ;
#7958 = EDGE_CURVE('',#6358,#6359,#3659,.T.) ;
#7959 = EDGE_CURVE('',#6359,#6360,#4919,.T.) ;
#7960 = EDGE_CURVE('',#6360,#6360,#3660,.T.) ;
#7961 = EDGE_CURVE('',#6359,#6358,#3661,.T.) ;
#7962 = EDGE_CURVE('',#6358,#6361,#4920,.T.) ;
#7963 = EDGE_CURVE('',#6361,#6361,#3662,.T.) ;
#7964 = EDGE_CURVE('',#6362,#6363,#4921,.T.) ;
#7965 = EDGE_CURVE('',#6363,#6364,#311,.T.) ;
#7966 = EDGE_CURVE('',#6364,#6365,#4922,.T.) ;
#7967 = EDGE_CURVE('',#6365,#6362,#312,.T.) ;
#7968 = EDGE_CURVE('',#6366,#6366,#3663,.T.) ;
#7969 = EDGE_CURVE('',#6367,#6368,#3664,.T.) ;
#7970 = EDGE_CURVE('',#6368,#6369,#4923,.T.) ;
#7971 = EDGE_CURVE('',#6369,#6369,#3665,.T.) ;
#7972 = EDGE_CURVE('',#6368,#6367,#3666,.T.) ;
#7973 = EDGE_CURVE('',#6367,#6370,#4924,.T.) ;
#7974 = EDGE_CURVE('',#6370,#6370,#3667,.T.) ;
#7975 = EDGE_CURVE('',#6371,#6372,#3668,.T.) ;
#7976 = EDGE_CURVE('',#6372,#6373,#4925,.T.) ;
#7977 = EDGE_CURVE('',#6373,#6374,#3669,.T.) ;
#7978 = EDGE_CURVE('',#6374,#6373,#3670,.T.) ;
#7979 = EDGE_CURVE('',#6372,#6371,#3671,.T.) ;
#7980 = EDGE_CURVE('',#6371,#6375,#4926,.T.) ;
#7981 = EDGE_CURVE('',#6376,#6375,#3672,.T.) ;
#7982 = EDGE_CURVE('',#6375,#6376,#3673,.T.) ;
#7983 = EDGE_CURVE('',#6374,#6377,#4927,.T.) ;
#7984 = EDGE_CURVE('',#6377,#6377,#3674,.T.) ;
#7985 = EDGE_CURVE('',#6376,#6378,#4928,.T.) ;
#7986 = EDGE_CURVE('',#6378,#6378,#3675,.T.) ;
#7987 = EDGE_CURVE('',#6379,#6379,#3676,.T.) ;
#7988 = EDGE_CURVE('',#6380,#6381,#3677,.T.) ;
#7989 = EDGE_CURVE('',#6381,#6382,#4929,.T.) ;
#7990 = EDGE_CURVE('',#6382,#6382,#3678,.T.) ;
#7991 = EDGE_CURVE('',#6381,#6380,#3679,.T.) ;
#7992 = EDGE_CURVE('',#6354,#6380,#4930,.T.) ;
#7993 = EDGE_CURVE('',#6299,#6283,#313,.F.) ;
#7994 = EDGE_CURVE('',#6282,#6300,#314,.T.) ;
#7995 = EDGE_CURVE('',#6383,#6384,#3680,.T.) ;
#7996 = EDGE_CURVE('',#6384,#6385,#4931,.T.) ;
#7997 = EDGE_CURVE('',#6385,#6385,#3681,.T.) ;
#7998 = EDGE_CURVE('',#6384,#6383,#3682,.T.) ;
#7999 = EDGE_CURVE('',#6383,#6386,#4932,.T.) ;
#8000 = EDGE_CURVE('',#6387,#6386,#3683,.T.) ;
#8001 = EDGE_CURVE('',#6386,#6387,#3684,.T.) ;
#8002 = EDGE_CURVE('',#6388,#6388,#315,.T.) ;
#8003 = EDGE_CURVE('',#6389,#6389,#316,.T.) ;
#8004 = EDGE_CURVE('',#6390,#6390,#317,.T.) ;
#8005 = EDGE_CURVE('',#6391,#6391,#3685,.T.) ;
#8006 = EDGE_CURVE('',#6387,#6392,#4933,.T.) ;
#8007 = EDGE_CURVE('',#6392,#6392,#3686,.T.) ;
#8008 = EDGE_CURVE('',#6393,#6393,#3687,.T.) ;
#8009 = EDGE_CURVE('',#6388,#6394,#318,.T.) ;
#8010 = EDGE_CURVE('',#6394,#6394,#319,.T.) ;
#8011 = EDGE_CURVE('',#6389,#6395,#320,.T.) ;
#8012 = EDGE_CURVE('',#6395,#6395,#321,.T.) ;
#8013 = EDGE_CURVE('',#6390,#6396,#322,.T.) ;
#8014 = EDGE_CURVE('',#6396,#6396,#323,.T.) ;
#8015 = EDGE_CURVE('',#6348,#6344,#324,.T.) ;
#8016 = EDGE_CURVE('',#6397,#6255,#325,.T.) ;
#8017 = EDGE_CURVE('',#6397,#6313,#326,.T.) ;
#8018 = EDGE_CURVE('',#6398,#6349,#327,.T.) ;
#8019 = EDGE_CURVE('',#6343,#6398,#328,.T.) ;
#8020 = EDGE_CURVE('',#6254,#6314,#329,.T.) ;
#8021 = EDGE_CURVE('',#6347,#6346,#330,.T.) ;
#8022 = EDGE_CURVE('',#6399,#6296,#331,.T.) ;
#8023 = EDGE_CURVE('',#6345,#6399,#332,.T.) ;
#8024 = EDGE_CURVE('',#6400,#6400,#3688,.T.) ;
#8025 = EDGE_CURVE('',#6401,#6362,#4934,.T.) ;
#8026 = EDGE_CURVE('',#6402,#6401,#4935,.T.) ;
#8027 = EDGE_CURVE('',#6402,#6363,#4936,.T.) ;
#8028 = EDGE_CURVE('',#6403,#6402,#3689,.T.) ;
#8029 = EDGE_CURVE('',#6403,#6364,#4937,.T.) ;
#8030 = EDGE_CURVE('',#6404,#6403,#4938,.T.) ;
#8031 = EDGE_CURVE('',#6404,#6365,#4939,.T.) ;
#8032 = EDGE_CURVE('',#6401,#6404,#3690,.T.) ;
#8033 = EDGE_CURVE('',#6405,#6405,#3691,.T.) ;
#8034 = EDGE_CURVE('',#6405,#6400,#4940,.T.) ;
#8035 = EDGE_CURVE('',#6406,#6406,#3692,.T.) ;
#8036 = EDGE_CURVE('',#6379,#6406,#4941,.T.) ;
#8037 = EDGE_CURVE('',#6393,#6377,#4942,.T.) ;
#8038 = EDGE_CURVE('',#6407,#6407,#3693,.T.) ;
#8039 = EDGE_CURVE('',#6407,#6391,#4943,.T.) ;
#8040 = EDGE_CURVE('',#6408,#6408,#3694,.T.) ;
#8041 = EDGE_CURVE('',#6409,#6409,#3695,.T.) ;
#8042 = EDGE_CURVE('',#6409,#6408,#4944,.T.) ;
#8043 = EDGE_CURVE('',#6410,#6410,#3696,.T.) ;
#8044 = EDGE_CURVE('',#6410,#6366,#4945,.T.) ;
#8045 = EDGE_CURVE('',#6411,#6412,#3697,.T.) ;
#8046 = EDGE_CURVE('',#6412,#6413,#91,.T.) ;
#8047 = EDGE_CURVE('',#6414,#6413,#4946,.T.) ;
#8048 = EDGE_CURVE('',#6414,#6415,#92,.T.) ;
#8049 = EDGE_CURVE('',#6416,#6415,#3698,.T.) ;
#8050 = EDGE_CURVE('',#6416,#6417,#93,.T.) ;
#8051 = EDGE_CURVE('',#6417,#6418,#4947,.T.) ;
#8052 = EDGE_CURVE('',#6418,#6411,#94,.T.) ;
#8053 = EDGE_CURVE('',#6419,#6413,#4948,.T.) ;
#8054 = EDGE_CURVE('',#6420,#6419,#4949,.T.) ;
#8055 = EDGE_CURVE('',#6420,#6414,#4950,.T.) ;
#8056 = EDGE_CURVE('',#6421,#6422,#4951,.T.) ;
#8057 = EDGE_CURVE('',#6421,#6423,#95,.T.) ;
#8058 = EDGE_CURVE('',#6424,#6423,#3699,.T.) ;
#8059 = EDGE_CURVE('',#6424,#6420,#96,.T.) ;
#8060 = EDGE_CURVE('',#6419,#6425,#97,.T.) ;
#8061 = EDGE_CURVE('',#6425,#6426,#3700,.T.) ;
#8062 = EDGE_CURVE('',#6426,#6422,#98,.T.) ;
#8063 = EDGE_CURVE('',#6421,#6417,#4952,.T.) ;
#8064 = EDGE_CURVE('',#6422,#6418,#4953,.T.) ;
#8065 = EDGE_CURVE('',#6416,#6423,#4954,.T.) ;
#8066 = EDGE_CURVE('',#6424,#6415,#4955,.T.) ;
#8067 = EDGE_CURVE('',#6411,#6426,#4956,.T.) ;
#8068 = EDGE_CURVE('',#6425,#6412,#4957,.T.) ;
#8069 = EDGE_CURVE('',#6427,#6427,#3701,.T.) ;
#8070 = EDGE_CURVE('',#6427,#6428,#4958,.T.) ;
#8071 = EDGE_CURVE('',#6428,#6428,#3702,.T.) ;
#8072 = EDGE_CURVE('',#6429,#6429,#3703,.T.) ;
#8073 = EDGE_CURVE('',#6430,#6430,#3704,.T.) ;
#8074 = EDGE_CURVE('',#6430,#6427,#4959,.T.) ;
#8075 = EDGE_CURVE('',#6431,#6431,#3705,.T.) ;
#8076 = EDGE_CURVE('',#6431,#6429,#4960,.T.) ;
#8077 = EDGE_CURVE('',#6431,#6432,#4961,.T.) ;
#8078 = EDGE_CURVE('',#6432,#6432,#3706,.T.) ;
#8079 = EDGE_CURVE('',#6430,#6433,#4962,.T.) ;
#8080 = EDGE_CURVE('',#6433,#6433,#3707,.T.) ;
#8081 = EDGE_CURVE('',#6434,#6434,#3708,.T.) ;
#8082 = EDGE_CURVE('',#6432,#6434,#4963,.T.) ;
#8083 = EDGE_CURVE('',#6435,#6436,#4964,.T.) ;
#8084 = EDGE_CURVE('',#6437,#6435,#4965,.T.) ;
#8085 = EDGE_CURVE('',#6437,#6438,#4966,.T.) ;
#8086 = EDGE_CURVE('',#6436,#6438,#4967,.T.) ;
#8087 = EDGE_CURVE('',#6439,#6437,#4968,.T.) ;
#8088 = EDGE_CURVE('',#6439,#6440,#4969,.T.) ;
#8089 = EDGE_CURVE('',#6438,#6440,#4970,.T.) ;
#8090 = EDGE_CURVE('',#6441,#6442,#4971,.T.) ;
#8091 = EDGE_CURVE('',#6440,#6441,#4972,.T.) ;
#8092 = EDGE_CURVE('',#6442,#6439,#4973,.T.) ;
#8093 = EDGE_CURVE('',#6443,#6443,#3709,.T.) ;
#8094 = EDGE_CURVE('',#6435,#6442,#3710,.T.) ;
#8095 = EDGE_CURVE('',#6444,#6445,#4974,.T.) ;
#8096 = EDGE_CURVE('',#6446,#6444,#3711,.T.) ;
#8097 = EDGE_CURVE('',#6446,#6447,#4975,.T.) ;
#8098 = EDGE_CURVE('',#6447,#6445,#3712,.T.) ;
#8099 = EDGE_CURVE('',#6448,#6449,#3713,.T.) ;
#8100 = EDGE_CURVE('',#6448,#6450,#4976,.T.) ;
#8101 = EDGE_CURVE('',#6450,#6451,#3714,.T.) ;
#8102 = EDGE_CURVE('',#6449,#6451,#4977,.T.) ;
#8103 = EDGE_CURVE('',#6452,#6453,#3715,.T.) ;
#8104 = EDGE_CURVE('',#6452,#6454,#4978,.T.) ;
#8105 = EDGE_CURVE('',#6454,#6455,#3716,.T.) ;
#8106 = EDGE_CURVE('',#6453,#6455,#4979,.T.) ;
#8107 = EDGE_CURVE('',#6456,#6457,#3717,.T.) ;
#8108 = EDGE_CURVE('',#6456,#6458,#4980,.T.) ;
#8109 = EDGE_CURVE('',#6458,#6459,#3718,.T.) ;
#8110 = EDGE_CURVE('',#6457,#6459,#4981,.T.) ;
#8111 = EDGE_CURVE('',#6460,#6461,#4982,.T.) ;
#8112 = EDGE_CURVE('',#6462,#6460,#3719,.T.) ;
#8113 = EDGE_CURVE('',#6462,#6463,#4983,.T.) ;
#8114 = EDGE_CURVE('',#6463,#6461,#3720,.T.) ;
#8115 = EDGE_CURVE('',#6464,#6465,#4984,.T.) ;
#8116 = EDGE_CURVE('',#6466,#6464,#3721,.T.) ;
#8117 = EDGE_CURVE('',#6466,#6467,#4985,.T.) ;
#8118 = EDGE_CURVE('',#6467,#6465,#3722,.T.) ;
#8119 = EDGE_CURVE('',#6468,#6469,#4986,.T.) ;
#8120 = EDGE_CURVE('',#6470,#6468,#3723,.T.) ;
#8121 = EDGE_CURVE('',#6470,#6471,#4987,.T.) ;
#8122 = EDGE_CURVE('',#6471,#6469,#3724,.T.) ;
#8123 = EDGE_CURVE('',#6472,#6473,#3725,.T.) ;
#8124 = EDGE_CURVE('',#6472,#6474,#4988,.T.) ;
#8125 = EDGE_CURVE('',#6474,#6475,#3726,.T.) ;
#8126 = EDGE_CURVE('',#6473,#6475,#4989,.T.) ;
#8127 = EDGE_CURVE('',#6476,#6477,#3727,.T.) ;
#8128 = EDGE_CURVE('',#6476,#6478,#4990,.T.) ;
#8129 = EDGE_CURVE('',#6478,#6479,#3728,.T.) ;
#8130 = EDGE_CURVE('',#6477,#6479,#4991,.T.) ;
#8131 = EDGE_CURVE('',#6480,#6481,#3729,.T.) ;
#8132 = EDGE_CURVE('',#6480,#6482,#4992,.T.) ;
#8133 = EDGE_CURVE('',#6482,#6483,#3730,.T.) ;
#8134 = EDGE_CURVE('',#6481,#6483,#4993,.T.) ;
#8135 = EDGE_CURVE('',#6484,#6485,#3731,.T.) ;
#8136 = EDGE_CURVE('',#6484,#6486,#4994,.T.) ;
#8137 = EDGE_CURVE('',#6486,#6487,#3732,.T.) ;
#8138 = EDGE_CURVE('',#6485,#6487,#4995,.T.) ;
#8139 = EDGE_CURVE('',#6488,#6489,#3733,.T.) ;
#8140 = EDGE_CURVE('',#6488,#6490,#4996,.T.) ;
#8141 = EDGE_CURVE('',#6490,#6491,#3734,.T.) ;
#8142 = EDGE_CURVE('',#6489,#6491,#4997,.T.) ;
#8143 = EDGE_CURVE('',#6492,#6493,#3735,.T.) ;
#8144 = EDGE_CURVE('',#6492,#6494,#4998,.T.) ;
#8145 = EDGE_CURVE('',#6494,#6495,#3736,.T.) ;
#8146 = EDGE_CURVE('',#6493,#6495,#4999,.T.) ;
#8147 = EDGE_CURVE('',#6496,#6497,#3737,.T.) ;
#8148 = EDGE_CURVE('',#6496,#6498,#5000,.T.) ;
#8149 = EDGE_CURVE('',#6498,#6499,#3738,.T.) ;
#8150 = EDGE_CURVE('',#6497,#6499,#5001,.T.) ;
#8151 = EDGE_CURVE('',#6500,#6501,#3739,.T.) ;
#8152 = EDGE_CURVE('',#6500,#6502,#5002,.T.) ;
#8153 = EDGE_CURVE('',#6502,#6503,#3740,.T.) ;
#8154 = EDGE_CURVE('',#6501,#6503,#5003,.T.) ;
#8155 = EDGE_CURVE('',#6504,#6505,#3741,.T.) ;
#8156 = EDGE_CURVE('',#6504,#6506,#5004,.T.) ;
#8157 = EDGE_CURVE('',#6506,#6507,#3742,.T.) ;
#8158 = EDGE_CURVE('',#6505,#6507,#5005,.T.) ;
#8159 = EDGE_CURVE('',#6508,#6509,#3743,.T.) ;
#8160 = EDGE_CURVE('',#6508,#6510,#5006,.T.) ;
#8161 = EDGE_CURVE('',#6510,#6511,#3744,.T.) ;
#8162 = EDGE_CURVE('',#6509,#6511,#5007,.T.) ;
#8163 = EDGE_CURVE('',#6512,#6513,#3745,.T.) ;
#8164 = EDGE_CURVE('',#6512,#6514,#5008,.T.) ;
#8165 = EDGE_CURVE('',#6514,#6515,#3746,.T.) ;
#8166 = EDGE_CURVE('',#6513,#6515,#5009,.T.) ;
#8167 = EDGE_CURVE('',#6516,#6517,#3747,.T.) ;
#8168 = EDGE_CURVE('',#6516,#6518,#5010,.T.) ;
#8169 = EDGE_CURVE('',#6518,#6519,#3748,.T.) ;
#8170 = EDGE_CURVE('',#6517,#6519,#5011,.T.) ;
#8171 = EDGE_CURVE('',#6520,#6521,#3749,.T.) ;
#8172 = EDGE_CURVE('',#6520,#6522,#5012,.T.) ;
#8173 = EDGE_CURVE('',#6522,#6523,#3750,.T.) ;
#8174 = EDGE_CURVE('',#6521,#6523,#5013,.T.) ;
#8175 = EDGE_CURVE('',#6524,#6525,#5014,.T.) ;
#8176 = EDGE_CURVE('',#6526,#6524,#3751,.T.) ;
#8177 = EDGE_CURVE('',#6526,#6527,#5015,.T.) ;
#8178 = EDGE_CURVE('',#6527,#6525,#3752,.T.) ;
#8179 = EDGE_CURVE('',#6528,#6529,#3753,.T.) ;
#8180 = EDGE_CURVE('',#6528,#6530,#5016,.T.) ;
#8181 = EDGE_CURVE('',#6530,#6531,#3754,.T.) ;
#8182 = EDGE_CURVE('',#6529,#6531,#5017,.T.) ;
#8183 = EDGE_CURVE('',#6532,#6533,#3755,.T.) ;
#8184 = EDGE_CURVE('',#6532,#6534,#5018,.T.) ;
#8185 = EDGE_CURVE('',#6534,#6535,#3756,.T.) ;
#8186 = EDGE_CURVE('',#6533,#6535,#5019,.T.) ;
#8187 = EDGE_CURVE('',#6536,#6537,#3757,.T.) ;
#8188 = EDGE_CURVE('',#6536,#6538,#5020,.T.) ;
#8189 = EDGE_CURVE('',#6538,#6539,#3758,.T.) ;
#8190 = EDGE_CURVE('',#6537,#6539,#5021,.T.) ;
#8191 = EDGE_CURVE('',#6540,#6541,#3759,.T.) ;
#8192 = EDGE_CURVE('',#6540,#6542,#5022,.T.) ;
#8193 = EDGE_CURVE('',#6542,#6543,#3760,.T.) ;
#8194 = EDGE_CURVE('',#6541,#6543,#5023,.T.) ;
#8195 = EDGE_CURVE('',#6544,#6545,#3761,.T.) ;
#8196 = EDGE_CURVE('',#6544,#6546,#5024,.T.) ;
#8197 = EDGE_CURVE('',#6546,#6547,#3762,.T.) ;
#8198 = EDGE_CURVE('',#6545,#6547,#5025,.T.) ;
#8199 = EDGE_CURVE('',#6548,#6549,#3763,.T.) ;
#8200 = EDGE_CURVE('',#6548,#6550,#5026,.T.) ;
#8201 = EDGE_CURVE('',#6550,#6551,#3764,.T.) ;
#8202 = EDGE_CURVE('',#6549,#6551,#5027,.T.) ;
#8203 = EDGE_CURVE('',#6552,#6553,#3765,.T.) ;
#8204 = EDGE_CURVE('',#6552,#6554,#5028,.T.) ;
#8205 = EDGE_CURVE('',#6554,#6555,#3766,.T.) ;
#8206 = EDGE_CURVE('',#6553,#6555,#5029,.T.) ;
#8207 = EDGE_CURVE('',#6556,#6557,#3767,.T.) ;
#8208 = EDGE_CURVE('',#6556,#6558,#5030,.T.) ;
#8209 = EDGE_CURVE('',#6558,#6559,#3768,.T.) ;
#8210 = EDGE_CURVE('',#6557,#6559,#5031,.T.) ;
#8211 = EDGE_CURVE('',#6560,#6561,#3769,.T.) ;
#8212 = EDGE_CURVE('',#6560,#6562,#5032,.T.) ;
#8213 = EDGE_CURVE('',#6562,#6563,#3770,.T.) ;
#8214 = EDGE_CURVE('',#6561,#6563,#5033,.T.) ;
#8215 = EDGE_CURVE('',#6564,#6565,#3771,.T.) ;
#8216 = EDGE_CURVE('',#6564,#6566,#5034,.T.) ;
#8217 = EDGE_CURVE('',#6566,#6567,#3772,.T.) ;
#8218 = EDGE_CURVE('',#6565,#6567,#5035,.T.) ;
#8219 = EDGE_CURVE('',#6568,#6569,#3773,.T.) ;
#8220 = EDGE_CURVE('',#6568,#6570,#5036,.T.) ;
#8221 = EDGE_CURVE('',#6570,#6571,#3774,.T.) ;
#8222 = EDGE_CURVE('',#6569,#6571,#5037,.T.) ;
#8223 = EDGE_CURVE('',#6572,#6573,#5038,.T.) ;
#8224 = EDGE_CURVE('',#6574,#6572,#3775,.T.) ;
#8225 = EDGE_CURVE('',#6574,#6575,#5039,.T.) ;
#8226 = EDGE_CURVE('',#6575,#6573,#3776,.T.) ;
#8227 = EDGE_CURVE('',#6576,#6577,#5040,.T.) ;
#8228 = EDGE_CURVE('',#6578,#6576,#3777,.T.) ;
#8229 = EDGE_CURVE('',#6578,#6579,#5041,.T.) ;
#8230 = EDGE_CURVE('',#6579,#6577,#3778,.T.) ;
#8231 = EDGE_CURVE('',#6580,#6581,#5042,.T.) ;
#8232 = EDGE_CURVE('',#6582,#6580,#3779,.T.) ;
#8233 = EDGE_CURVE('',#6582,#6583,#5043,.T.) ;
#8234 = EDGE_CURVE('',#6583,#6581,#3780,.T.) ;
#8235 = EDGE_CURVE('',#6584,#6585,#5044,.T.) ;
#8236 = EDGE_CURVE('',#6586,#6584,#3781,.T.) ;
#8237 = EDGE_CURVE('',#6586,#6587,#5045,.T.) ;
#8238 = EDGE_CURVE('',#6587,#6585,#3782,.T.) ;
#8239 = EDGE_CURVE('',#6588,#6589,#5046,.T.) ;
#8240 = EDGE_CURVE('',#6590,#6588,#3783,.T.) ;
#8241 = EDGE_CURVE('',#6590,#6591,#5047,.T.) ;
#8242 = EDGE_CURVE('',#6591,#6589,#3784,.T.) ;
#8243 = EDGE_CURVE('',#6592,#6593,#5048,.T.) ;
#8244 = EDGE_CURVE('',#6594,#6592,#3785,.T.) ;
#8245 = EDGE_CURVE('',#6594,#6595,#5049,.T.) ;
#8246 = EDGE_CURVE('',#6595,#6593,#3786,.T.) ;
#8247 = EDGE_CURVE('',#6596,#6597,#5050,.T.) ;
#8248 = EDGE_CURVE('',#6598,#6596,#3787,.T.) ;
#8249 = EDGE_CURVE('',#6598,#6599,#5051,.T.) ;
#8250 = EDGE_CURVE('',#6599,#6597,#3788,.T.) ;
#8251 = EDGE_CURVE('',#6600,#6601,#3789,.T.) ;
#8252 = EDGE_CURVE('',#6600,#6602,#5052,.T.) ;
#8253 = EDGE_CURVE('',#6602,#6603,#3790,.T.) ;
#8254 = EDGE_CURVE('',#6601,#6603,#5053,.T.) ;
#8255 = EDGE_CURVE('',#6604,#6605,#3791,.T.) ;
#8256 = EDGE_CURVE('',#6604,#6606,#5054,.T.) ;
#8257 = EDGE_CURVE('',#6606,#6607,#3792,.T.) ;
#8258 = EDGE_CURVE('',#6605,#6607,#5055,.T.) ;
#8259 = EDGE_CURVE('',#6608,#6609,#3793,.T.) ;
#8260 = EDGE_CURVE('',#6608,#6610,#5056,.T.) ;
#8261 = EDGE_CURVE('',#6610,#6611,#3794,.T.) ;
#8262 = EDGE_CURVE('',#6609,#6611,#5057,.T.) ;
#8263 = EDGE_CURVE('',#6612,#6613,#3795,.T.) ;
#8264 = EDGE_CURVE('',#6612,#6614,#5058,.T.) ;
#8265 = EDGE_CURVE('',#6614,#6615,#3796,.T.) ;
#8266 = EDGE_CURVE('',#6613,#6615,#5059,.T.) ;
#8267 = EDGE_CURVE('',#6616,#6617,#3797,.T.) ;
#8268 = EDGE_CURVE('',#6616,#6618,#5060,.T.) ;
#8269 = EDGE_CURVE('',#6618,#6619,#3798,.T.) ;
#8270 = EDGE_CURVE('',#6617,#6619,#5061,.T.) ;
#8271 = EDGE_CURVE('',#6620,#6621,#3799,.T.) ;
#8272 = EDGE_CURVE('',#6620,#6622,#5062,.T.) ;
#8273 = EDGE_CURVE('',#6622,#6623,#3800,.T.) ;
#8274 = EDGE_CURVE('',#6621,#6623,#5063,.T.) ;
#8275 = EDGE_CURVE('',#6624,#6625,#3801,.T.) ;
#8276 = EDGE_CURVE('',#6624,#6626,#5064,.T.) ;
#8277 = EDGE_CURVE('',#6626,#6627,#3802,.T.) ;
#8278 = EDGE_CURVE('',#6625,#6627,#5065,.T.) ;
#8279 = EDGE_CURVE('',#6628,#6629,#3803,.T.) ;
#8280 = EDGE_CURVE('',#6628,#6630,#5066,.T.) ;
#8281 = EDGE_CURVE('',#6630,#6631,#3804,.T.) ;
#8282 = EDGE_CURVE('',#6629,#6631,#5067,.T.) ;
#8283 = EDGE_CURVE('',#6632,#6633,#3805,.T.) ;
#8284 = EDGE_CURVE('',#6632,#6634,#5068,.T.) ;
#8285 = EDGE_CURVE('',#6634,#6635,#3806,.T.) ;
#8286 = EDGE_CURVE('',#6633,#6635,#5069,.T.) ;
#8287 = EDGE_CURVE('',#6636,#6637,#3807,.T.) ;
#8288 = EDGE_CURVE('',#6636,#6638,#5070,.T.) ;
#8289 = EDGE_CURVE('',#6638,#6639,#3808,.T.) ;
#8290 = EDGE_CURVE('',#6637,#6639,#5071,.T.) ;
#8291 = EDGE_CURVE('',#6640,#6641,#3809,.T.) ;
#8292 = EDGE_CURVE('',#6640,#6642,#5072,.T.) ;
#8293 = EDGE_CURVE('',#6642,#6643,#3810,.T.) ;
#8294 = EDGE_CURVE('',#6641,#6643,#5073,.T.) ;
#8295 = EDGE_CURVE('',#6644,#6645,#5074,.T.) ;
#8296 = EDGE_CURVE('',#6646,#6644,#3811,.T.) ;
#8297 = EDGE_CURVE('',#6646,#6647,#5075,.T.) ;
#8298 = EDGE_CURVE('',#6647,#6645,#3812,.T.) ;
#8299 = EDGE_CURVE('',#6648,#6649,#3813,.T.) ;
#8300 = EDGE_CURVE('',#6648,#6650,#5076,.T.) ;
#8301 = EDGE_CURVE('',#6650,#6651,#3814,.T.) ;
#8302 = EDGE_CURVE('',#6649,#6651,#5077,.T.) ;
#8303 = EDGE_CURVE('',#6652,#6653,#3815,.T.) ;
#8304 = EDGE_CURVE('',#6652,#6654,#5078,.T.) ;
#8305 = EDGE_CURVE('',#6654,#6655,#3816,.T.) ;
#8306 = EDGE_CURVE('',#6653,#6655,#5079,.T.) ;
#8307 = EDGE_CURVE('',#6656,#6657,#3817,.T.) ;
#8308 = EDGE_CURVE('',#6656,#6658,#5080,.T.) ;
#8309 = EDGE_CURVE('',#6658,#6659,#3818,.T.) ;
#8310 = EDGE_CURVE('',#6657,#6659,#5081,.T.) ;
#8311 = EDGE_CURVE('',#6660,#6661,#3819,.T.) ;
#8312 = EDGE_CURVE('',#6660,#6662,#5082,.T.) ;
#8313 = EDGE_CURVE('',#6662,#6663,#3820,.T.) ;
#8314 = EDGE_CURVE('',#6661,#6663,#5083,.T.) ;
#8315 = EDGE_CURVE('',#6664,#6665,#3821,.T.) ;
#8316 = EDGE_CURVE('',#6664,#6666,#5084,.T.) ;
#8317 = EDGE_CURVE('',#6666,#6667,#3822,.T.) ;
#8318 = EDGE_CURVE('',#6665,#6667,#5085,.T.) ;
#8319 = EDGE_CURVE('',#6668,#6669,#3823,.T.) ;
#8320 = EDGE_CURVE('',#6668,#6670,#5086,.T.) ;
#8321 = EDGE_CURVE('',#6670,#6671,#3824,.T.) ;
#8322 = EDGE_CURVE('',#6669,#6671,#5087,.T.) ;
#8323 = EDGE_CURVE('',#6672,#6673,#3825,.T.) ;
#8324 = EDGE_CURVE('',#6672,#6674,#5088,.T.) ;
#8325 = EDGE_CURVE('',#6674,#6675,#3826,.T.) ;
#8326 = EDGE_CURVE('',#6673,#6675,#5089,.T.) ;
#8327 = EDGE_CURVE('',#6676,#6677,#5090,.T.) ;
#8328 = EDGE_CURVE('',#6678,#6676,#3827,.T.) ;
#8329 = EDGE_CURVE('',#6678,#6679,#5091,.T.) ;
#8330 = EDGE_CURVE('',#6679,#6677,#3828,.T.) ;
#8331 = EDGE_CURVE('',#6680,#6681,#3829,.T.) ;
#8332 = EDGE_CURVE('',#6680,#6682,#5092,.T.) ;
#8333 = EDGE_CURVE('',#6682,#6683,#3830,.T.) ;
#8334 = EDGE_CURVE('',#6681,#6683,#5093,.T.) ;
#8335 = EDGE_CURVE('',#6684,#6684,#3831,.T.) ;
#8336 = EDGE_CURVE('',#6684,#6443,#5094,.T.) ;
#8337 = EDGE_CURVE('',#6685,#6685,#3832,.T.) ;
#8338 = EDGE_CURVE('',#6685,#6686,#5095,.T.) ;
#8339 = EDGE_CURVE('',#6687,#6686,#3833,.T.) ;
#8340 = EDGE_CURVE('',#6686,#6687,#3834,.T.) ;
#8341 = EDGE_CURVE('',#6688,#6689,#3835,.T.) ;
#8342 = EDGE_CURVE('',#6689,#6688,#3836,.T.) ;
#8343 = EDGE_CURVE('',#6689,#6687,#5096,.T.) ;
#8344 = EDGE_CURVE('',#6688,#6690,#5097,.T.) ;
#8345 = EDGE_CURVE('',#6619,#6690,#3837,.T.) ;
#8346 = EDGE_CURVE('',#6615,#6618,#3838,.T.) ;
#8347 = EDGE_CURVE('',#6611,#6614,#3839,.T.) ;
#8348 = EDGE_CURVE('',#6607,#6610,#3840,.T.) ;
#8349 = EDGE_CURVE('',#6573,#6606,#3841,.T.) ;
#8350 = EDGE_CURVE('',#6577,#6575,#3842,.T.) ;
#8351 = EDGE_CURVE('',#6581,#6579,#3843,.T.) ;
#8352 = EDGE_CURVE('',#6585,#6583,#3844,.T.) ;
#8353 = EDGE_CURVE('',#6589,#6587,#3845,.T.) ;
#8354 = EDGE_CURVE('',#6593,#6591,#3846,.T.) ;
#8355 = EDGE_CURVE('',#6597,#6595,#3847,.T.) ;
#8356 = EDGE_CURVE('',#6603,#6599,#3848,.T.) ;
#8357 = EDGE_CURVE('',#6571,#6602,#3849,.T.) ;
#8358 = EDGE_CURVE('',#6567,#6570,#3850,.T.) ;
#8359 = EDGE_CURVE('',#6563,#6566,#3851,.T.) ;
#8360 = EDGE_CURVE('',#6559,#6562,#3852,.T.) ;
#8361 = EDGE_CURVE('',#6555,#6558,#3853,.T.) ;
#8362 = EDGE_CURVE('',#6551,#6554,#3854,.T.) ;
#8363 = EDGE_CURVE('',#6547,#6550,#3855,.T.) ;
#8364 = EDGE_CURVE('',#6543,#6546,#3856,.T.) ;
#8365 = EDGE_CURVE('',#6539,#6542,#3857,.T.) ;
#8366 = EDGE_CURVE('',#6535,#6538,#3858,.T.) ;
#8367 = EDGE_CURVE('',#6525,#6534,#3859,.T.) ;
#8368 = EDGE_CURVE('',#6531,#6527,#3860,.T.) ;
#8369 = EDGE_CURVE('',#6523,#6530,#3861,.T.) ;
#8370 = EDGE_CURVE('',#6519,#6522,#3862,.T.) ;
#8371 = EDGE_CURVE('',#6515,#6518,#3863,.T.) ;
#8372 = EDGE_CURVE('',#6511,#6514,#3864,.T.) ;
#8373 = EDGE_CURVE('',#6507,#6510,#3865,.T.) ;
#8374 = EDGE_CURVE('',#6503,#6506,#3866,.T.) ;
#8375 = EDGE_CURVE('',#6499,#6502,#3867,.T.) ;
#8376 = EDGE_CURVE('',#6495,#6498,#3868,.T.) ;
#8377 = EDGE_CURVE('',#6491,#6494,#3869,.T.) ;
#8378 = EDGE_CURVE('',#6487,#6490,#3870,.T.) ;
#8379 = EDGE_CURVE('',#6483,#6486,#3871,.T.) ;
#8380 = EDGE_CURVE('',#6479,#6482,#3872,.T.) ;
#8381 = EDGE_CURVE('',#6461,#6478,#3873,.T.) ;
#8382 = EDGE_CURVE('',#6465,#6463,#3874,.T.) ;
#8383 = EDGE_CURVE('',#6469,#6467,#3875,.T.) ;
#8384 = EDGE_CURVE('',#6475,#6471,#3876,.T.) ;
#8385 = EDGE_CURVE('',#6459,#6474,#3877,.T.) ;
#8386 = EDGE_CURVE('',#6455,#6458,#3878,.T.) ;
#8387 = EDGE_CURVE('',#6451,#6454,#3879,.T.) ;
#8388 = EDGE_CURVE('',#6445,#6450,#3880,.T.) ;
#8389 = EDGE_CURVE('',#6677,#6447,#3881,.T.) ;
#8390 = EDGE_CURVE('',#6683,#6679,#3882,.T.) ;
#8391 = EDGE_CURVE('',#6675,#6682,#3883,.T.) ;
#8392 = EDGE_CURVE('',#6671,#6674,#3884,.T.) ;
#8393 = EDGE_CURVE('',#6667,#6670,#3885,.T.) ;
#8394 = EDGE_CURVE('',#6663,#6666,#3886,.T.) ;
#8395 = EDGE_CURVE('',#6659,#6662,#3887,.T.) ;
#8396 = EDGE_CURVE('',#6655,#6658,#3888,.T.) ;
#8397 = EDGE_CURVE('',#6645,#6654,#3889,.T.) ;
#8398 = EDGE_CURVE('',#6651,#6647,#3890,.T.) ;
#8399 = EDGE_CURVE('',#6643,#6650,#3891,.T.) ;
#8400 = EDGE_CURVE('',#6639,#6642,#3892,.T.) ;
#8401 = EDGE_CURVE('',#6635,#6638,#3893,.T.) ;
#8402 = EDGE_CURVE('',#6631,#6634,#3894,.T.) ;
#8403 = EDGE_CURVE('',#6627,#6630,#3895,.T.) ;
#8404 = EDGE_CURVE('',#6623,#6626,#3896,.T.) ;
#8405 = EDGE_CURVE('',#6690,#6622,#3897,.T.) ;
#8406 = EDGE_CURVE('',#6691,#6692,#3898,.T.) ;
#8407 = EDGE_CURVE('',#6692,#6691,#3899,.T.) ;
#8408 = EDGE_CURVE('',#6692,#6693,#5098,.T.) ;
#8409 = EDGE_CURVE('',#6693,#6500,#3900,.T.) ;
#8410 = EDGE_CURVE('',#6501,#6504,#3901,.T.) ;
#8411 = EDGE_CURVE('',#6505,#6508,#3902,.T.) ;
#8412 = EDGE_CURVE('',#6509,#6512,#3903,.T.) ;
#8413 = EDGE_CURVE('',#6513,#6516,#3904,.T.) ;
#8414 = EDGE_CURVE('',#6517,#6520,#3905,.T.) ;
#8415 = EDGE_CURVE('',#6521,#6528,#3906,.T.) ;
#8416 = EDGE_CURVE('',#6529,#6526,#3907,.T.) ;
#8417 = EDGE_CURVE('',#6524,#6532,#3908,.T.) ;
#8418 = EDGE_CURVE('',#6533,#6536,#3909,.T.) ;
#8419 = EDGE_CURVE('',#6537,#6540,#3910,.T.) ;
#8420 = EDGE_CURVE('',#6541,#6544,#3911,.T.) ;
#8421 = EDGE_CURVE('',#6545,#6548,#3912,.T.) ;
#8422 = EDGE_CURVE('',#6549,#6552,#3913,.T.) ;
#8423 = EDGE_CURVE('',#6553,#6556,#3914,.T.) ;
#8424 = EDGE_CURVE('',#6557,#6560,#3915,.T.) ;
#8425 = EDGE_CURVE('',#6561,#6564,#3916,.T.) ;
#8426 = EDGE_CURVE('',#6565,#6568,#3917,.T.) ;
#8427 = EDGE_CURVE('',#6569,#6600,#3918,.T.) ;
#8428 = EDGE_CURVE('',#6601,#6598,#3919,.T.) ;
#8429 = EDGE_CURVE('',#6596,#6594,#3920,.T.) ;
#8430 = EDGE_CURVE('',#6592,#6590,#3921,.T.) ;
#8431 = EDGE_CURVE('',#6588,#6586,#3922,.T.) ;
#8432 = EDGE_CURVE('',#6584,#6582,#3923,.T.) ;
#8433 = EDGE_CURVE('',#6580,#6578,#3924,.T.) ;
#8434 = EDGE_CURVE('',#6576,#6574,#3925,.T.) ;
#8435 = EDGE_CURVE('',#6572,#6604,#3926,.T.) ;
#8436 = EDGE_CURVE('',#6605,#6608,#3927,.T.) ;
#8437 = EDGE_CURVE('',#6609,#6612,#3928,.T.) ;
#8438 = EDGE_CURVE('',#6613,#6616,#3929,.T.) ;
#8439 = EDGE_CURVE('',#6617,#6620,#3930,.T.) ;
#8440 = EDGE_CURVE('',#6621,#6624,#3931,.T.) ;
#8441 = EDGE_CURVE('',#6625,#6628,#3932,.T.) ;
#8442 = EDGE_CURVE('',#6629,#6632,#3933,.T.) ;
#8443 = EDGE_CURVE('',#6633,#6636,#3934,.T.) ;
#8444 = EDGE_CURVE('',#6637,#6640,#3935,.T.) ;
#8445 = EDGE_CURVE('',#6641,#6648,#3936,.T.) ;
#8446 = EDGE_CURVE('',#6649,#6646,#3937,.T.) ;
#8447 = EDGE_CURVE('',#6644,#6652,#3938,.T.) ;
#8448 = EDGE_CURVE('',#6653,#6656,#3939,.T.) ;
#8449 = EDGE_CURVE('',#6657,#6660,#3940,.T.) ;
#8450 = EDGE_CURVE('',#6661,#6664,#3941,.T.) ;
#8451 = EDGE_CURVE('',#6665,#6668,#3942,.T.) ;
#8452 = EDGE_CURVE('',#6669,#6672,#3943,.T.) ;
#8453 = EDGE_CURVE('',#6673,#6680,#3944,.T.) ;
#8454 = EDGE_CURVE('',#6681,#6678,#3945,.T.) ;
#8455 = EDGE_CURVE('',#6676,#6446,#3946,.T.) ;
#8456 = EDGE_CURVE('',#6444,#6448,#3947,.T.) ;
#8457 = EDGE_CURVE('',#6449,#6452,#3948,.T.) ;
#8458 = EDGE_CURVE('',#6453,#6456,#3949,.T.) ;
#8459 = EDGE_CURVE('',#6457,#6472,#3950,.T.) ;
#8460 = EDGE_CURVE('',#6473,#6470,#3951,.T.) ;
#8461 = EDGE_CURVE('',#6468,#6466,#3952,.T.) ;
#8462 = EDGE_CURVE('',#6464,#6462,#3953,.T.) ;
#8463 = EDGE_CURVE('',#6460,#6476,#3954,.T.) ;
#8464 = EDGE_CURVE('',#6477,#6480,#3955,.T.) ;
#8465 = EDGE_CURVE('',#6481,#6484,#3956,.T.) ;
#8466 = EDGE_CURVE('',#6485,#6488,#3957,.T.) ;
#8467 = EDGE_CURVE('',#6489,#6492,#3958,.T.) ;
#8468 = EDGE_CURVE('',#6493,#6496,#3959,.T.) ;
#8469 = EDGE_CURVE('',#6497,#6693,#3960,.T.) ;
#8470 = EDGE_CURVE('',#6691,#6694,#5099,.T.) ;
#8471 = EDGE_CURVE('',#6695,#6694,#3961,.T.) ;
#8472 = EDGE_CURVE('',#6694,#6695,#3962,.T.) ;
#8473 = EDGE_CURVE('',#6696,#6696,#3963,.T.) ;
#8474 = EDGE_CURVE('',#6696,#6695,#5100,.T.) ;
#8475 = EDGE_CURVE('',#6697,#6697,#3964,.T.) ;
#8476 = EDGE_CURVE('',#6698,#6698,#3965,.T.) ;
#8477 = EDGE_CURVE('',#6698,#6697,#5101,.T.) ;
#8478 = EDGE_CURVE('',#6699,#6699,#3966,.T.) ;
#8479 = EDGE_CURVE('',#6700,#6700,#3967,.T.) ;
#8480 = EDGE_CURVE('',#6700,#6699,#5102,.T.) ;
#8481 = EDGE_CURVE('',#6436,#6441,#3968,.T.) ;
#8482 = EDGE_CURVE('',#6683,#6701,#3969,.T.) ;
#8483 = EDGE_CURVE('',#6702,#6679,#3970,.T.) ;
#8484 = EDGE_CURVE('',#6702,#6701,#3971,.T.) ;
#8485 = EDGE_CURVE('',#6681,#6703,#3972,.T.) ;
#8486 = EDGE_CURVE('',#6704,#6703,#3973,.T.) ;
#8487 = EDGE_CURVE('',#6704,#6678,#3974,.T.) ;
#8488 = EDGE_CURVE('',#6704,#6702,#5103,.T.) ;
#8489 = EDGE_CURVE('',#6703,#6701,#5104,.T.) ;
#8490 = EDGE_CURVE('',#6705,#6447,#3975,.T.) ;
#8491 = EDGE_CURVE('',#6705,#6706,#3976,.T.) ;
#8492 = EDGE_CURVE('',#6677,#6706,#3977,.T.) ;
#8493 = EDGE_CURVE('',#6676,#6707,#3978,.T.) ;
#8494 = EDGE_CURVE('',#6708,#6707,#3979,.T.) ;
#8495 = EDGE_CURVE('',#6708,#6446,#3980,.T.) ;
#8496 = EDGE_CURVE('',#6708,#6705,#5105,.T.) ;
#8497 = EDGE_CURVE('',#6707,#6706,#5106,.T.) ;
#8498 = EDGE_CURVE('',#6709,#6682,#3981,.T.) ;
#8499 = EDGE_CURVE('',#6709,#6710,#3982,.T.) ;
#8500 = EDGE_CURVE('',#6675,#6710,#3983,.T.) ;
#8501 = EDGE_CURVE('',#6673,#6711,#3984,.T.) ;
#8502 = EDGE_CURVE('',#6712,#6711,#3985,.T.) ;
#8503 = EDGE_CURVE('',#6712,#6680,#3986,.T.) ;
#8504 = EDGE_CURVE('',#6712,#6709,#5107,.T.) ;
#8505 = EDGE_CURVE('',#6711,#6710,#5108,.T.) ;
#8506 = EDGE_CURVE('',#6713,#6674,#3987,.T.) ;
#8507 = EDGE_CURVE('',#6713,#6714,#3988,.T.) ;
#8508 = EDGE_CURVE('',#6671,#6714,#3989,.T.) ;
#8509 = EDGE_CURVE('',#6669,#6715,#3990,.T.) ;
#8510 = EDGE_CURVE('',#6716,#6715,#3991,.T.) ;
#8511 = EDGE_CURVE('',#6716,#6672,#3992,.T.) ;
#8512 = EDGE_CURVE('',#6716,#6713,#5109,.T.) ;
#8513 = EDGE_CURVE('',#6715,#6714,#5110,.T.) ;
#8514 = EDGE_CURVE('',#6717,#6670,#3993,.T.) ;
#8515 = EDGE_CURVE('',#6717,#6718,#3994,.T.) ;
#8516 = EDGE_CURVE('',#6667,#6718,#3995,.T.) ;
#8517 = EDGE_CURVE('',#6665,#6719,#3996,.T.) ;
#8518 = EDGE_CURVE('',#6720,#6719,#3997,.T.) ;
#8519 = EDGE_CURVE('',#6720,#6668,#3998,.T.) ;
#8520 = EDGE_CURVE('',#6720,#6717,#5111,.T.) ;
#8521 = EDGE_CURVE('',#6719,#6718,#5112,.T.) ;
#8522 = EDGE_CURVE('',#6721,#6666,#3999,.T.) ;
#8523 = EDGE_CURVE('',#6721,#6722,#4000,.T.) ;
#8524 = EDGE_CURVE('',#6663,#6722,#4001,.T.) ;
#8525 = EDGE_CURVE('',#6661,#6723,#4002,.T.) ;
#8526 = EDGE_CURVE('',#6724,#6723,#4003,.T.) ;
#8527 = EDGE_CURVE('',#6724,#6664,#4004,.T.) ;
#8528 = EDGE_CURVE('',#6724,#6721,#5113,.T.) ;
#8529 = EDGE_CURVE('',#6723,#6722,#5114,.T.) ;
#8530 = EDGE_CURVE('',#6725,#6662,#4005,.T.) ;
#8531 = EDGE_CURVE('',#6725,#6726,#4006,.T.) ;
#8532 = EDGE_CURVE('',#6659,#6726,#4007,.T.) ;
#8533 = EDGE_CURVE('',#6657,#6727,#4008,.T.) ;
#8534 = EDGE_CURVE('',#6728,#6727,#4009,.T.) ;
#8535 = EDGE_CURVE('',#6728,#6660,#4010,.T.) ;
#8536 = EDGE_CURVE('',#6728,#6725,#5115,.T.) ;
#8537 = EDGE_CURVE('',#6727,#6726,#5116,.T.) ;
#8538 = EDGE_CURVE('',#6729,#6658,#4011,.T.) ;
#8539 = EDGE_CURVE('',#6729,#6730,#4012,.T.) ;
#8540 = EDGE_CURVE('',#6655,#6730,#4013,.T.) ;
#8541 = EDGE_CURVE('',#6653,#6731,#4014,.T.) ;
#8542 = EDGE_CURVE('',#6732,#6731,#4015,.T.) ;
#8543 = EDGE_CURVE('',#6732,#6656,#4016,.T.) ;
#8544 = EDGE_CURVE('',#6732,#6729,#5117,.T.) ;
#8545 = EDGE_CURVE('',#6731,#6730,#5118,.T.) ;
#8546 = EDGE_CURVE('',#6733,#6647,#4017,.T.) ;
#8547 = EDGE_CURVE('',#6733,#6734,#4018,.T.) ;
#8548 = EDGE_CURVE('',#6651,#6734,#4019,.T.) ;
#8549 = EDGE_CURVE('',#6649,#6735,#4020,.T.) ;
#8550 = EDGE_CURVE('',#6736,#6735,#4021,.T.) ;
#8551 = EDGE_CURVE('',#6736,#6646,#4022,.T.) ;
#8552 = EDGE_CURVE('',#6736,#6733,#5119,.T.) ;
#8553 = EDGE_CURVE('',#6735,#6734,#5120,.T.) ;
#8554 = EDGE_CURVE('',#6737,#6654,#4023,.T.) ;
#8555 = EDGE_CURVE('',#6737,#6738,#4024,.T.) ;
#8556 = EDGE_CURVE('',#6645,#6738,#4025,.T.) ;
#8557 = EDGE_CURVE('',#6644,#6739,#4026,.T.) ;
#8558 = EDGE_CURVE('',#6740,#6739,#4027,.T.) ;
#8559 = EDGE_CURVE('',#6740,#6652,#4028,.T.) ;
#8560 = EDGE_CURVE('',#6740,#6737,#5121,.T.) ;
#8561 = EDGE_CURVE('',#6739,#6738,#5122,.T.) ;
#8562 = EDGE_CURVE('',#6741,#6650,#4029,.T.) ;
#8563 = EDGE_CURVE('',#6741,#6742,#4030,.T.) ;
#8564 = EDGE_CURVE('',#6643,#6742,#4031,.T.) ;
#8565 = EDGE_CURVE('',#6641,#6743,#4032,.T.) ;
#8566 = EDGE_CURVE('',#6744,#6743,#4033,.T.) ;
#8567 = EDGE_CURVE('',#6744,#6648,#4034,.T.) ;
#8568 = EDGE_CURVE('',#6744,#6741,#5123,.T.) ;
#8569 = EDGE_CURVE('',#6743,#6742,#5124,.T.) ;
#8570 = EDGE_CURVE('',#6745,#6642,#4035,.T.) ;
#8571 = EDGE_CURVE('',#6745,#6746,#4036,.T.) ;
#8572 = EDGE_CURVE('',#6639,#6746,#4037,.T.) ;
#8573 = EDGE_CURVE('',#6637,#6747,#4038,.T.) ;
#8574 = EDGE_CURVE('',#6748,#6747,#4039,.T.) ;
#8575 = EDGE_CURVE('',#6748,#6640,#4040,.T.) ;
#8576 = EDGE_CURVE('',#6748,#6745,#5125,.T.) ;
#8577 = EDGE_CURVE('',#6747,#6746,#5126,.T.) ;
#8578 = EDGE_CURVE('',#6749,#6638,#4041,.T.) ;
#8579 = EDGE_CURVE('',#6749,#6750,#4042,.T.) ;
#8580 = EDGE_CURVE('',#6635,#6750,#4043,.T.) ;
#8581 = EDGE_CURVE('',#6633,#6751,#4044,.T.) ;
#8582 = EDGE_CURVE('',#6752,#6751,#4045,.T.) ;
#8583 = EDGE_CURVE('',#6752,#6636,#4046,.T.) ;
#8584 = EDGE_CURVE('',#6752,#6749,#5127,.T.) ;
#8585 = EDGE_CURVE('',#6751,#6750,#5128,.T.) ;
#8586 = EDGE_CURVE('',#6753,#6634,#4047,.T.) ;
#8587 = EDGE_CURVE('',#6753,#6754,#4048,.T.) ;
#8588 = EDGE_CURVE('',#6631,#6754,#4049,.T.) ;
#8589 = EDGE_CURVE('',#6629,#6755,#4050,.T.) ;
#8590 = EDGE_CURVE('',#6756,#6755,#4051,.T.) ;
#8591 = EDGE_CURVE('',#6756,#6632,#4052,.T.) ;
#8592 = EDGE_CURVE('',#6756,#6753,#5129,.T.) ;
#8593 = EDGE_CURVE('',#6755,#6754,#5130,.T.) ;
#8594 = EDGE_CURVE('',#6757,#6630,#4053,.T.) ;
#8595 = EDGE_CURVE('',#6757,#6758,#4054,.T.) ;
#8596 = EDGE_CURVE('',#6627,#6758,#4055,.T.) ;
#8597 = EDGE_CURVE('',#6625,#6759,#4056,.T.) ;
#8598 = EDGE_CURVE('',#6760,#6759,#4057,.T.) ;
#8599 = EDGE_CURVE('',#6760,#6628,#4058,.T.) ;
#8600 = EDGE_CURVE('',#6760,#6757,#5131,.T.) ;
#8601 = EDGE_CURVE('',#6759,#6758,#5132,.T.) ;
#8602 = EDGE_CURVE('',#6761,#6626,#4059,.T.) ;
#8603 = EDGE_CURVE('',#6761,#6762,#4060,.T.) ;
#8604 = EDGE_CURVE('',#6623,#6762,#4061,.T.) ;
#8605 = EDGE_CURVE('',#6621,#6763,#4062,.T.) ;
#8606 = EDGE_CURVE('',#6764,#6763,#4063,.T.) ;
#8607 = EDGE_CURVE('',#6764,#6624,#4064,.T.) ;
#8608 = EDGE_CURVE('',#6764,#6761,#5133,.T.) ;
#8609 = EDGE_CURVE('',#6763,#6762,#5134,.T.) ;
#8610 = EDGE_CURVE('',#6765,#6622,#4065,.T.) ;
#8611 = EDGE_CURVE('',#6765,#6766,#4066,.T.) ;
#8612 = EDGE_CURVE('',#6619,#6766,#4067,.T.) ;
#8613 = EDGE_CURVE('',#6617,#6767,#4068,.T.) ;
#8614 = EDGE_CURVE('',#6768,#6767,#4069,.T.) ;
#8615 = EDGE_CURVE('',#6768,#6620,#4070,.T.) ;
#8616 = EDGE_CURVE('',#6768,#6765,#5135,.T.) ;
#8617 = EDGE_CURVE('',#6767,#6766,#5136,.T.) ;
#8618 = EDGE_CURVE('',#6769,#6618,#4071,.T.) ;
#8619 = EDGE_CURVE('',#6769,#6770,#4072,.T.) ;
#8620 = EDGE_CURVE('',#6615,#6770,#4073,.T.) ;
#8621 = EDGE_CURVE('',#6613,#6771,#4074,.T.) ;
#8622 = EDGE_CURVE('',#6772,#6771,#4075,.T.) ;
#8623 = EDGE_CURVE('',#6772,#6616,#4076,.T.) ;
#8624 = EDGE_CURVE('',#6772,#6769,#5137,.T.) ;
#8625 = EDGE_CURVE('',#6771,#6770,#5138,.T.) ;
#8626 = EDGE_CURVE('',#6773,#6614,#4077,.T.) ;
#8627 = EDGE_CURVE('',#6773,#6774,#4078,.T.) ;
#8628 = EDGE_CURVE('',#6611,#6774,#4079,.T.) ;
#8629 = EDGE_CURVE('',#6609,#6775,#4080,.T.) ;
#8630 = EDGE_CURVE('',#6776,#6775,#4081,.T.) ;
#8631 = EDGE_CURVE('',#6776,#6612,#4082,.T.) ;
#8632 = EDGE_CURVE('',#6776,#6773,#5139,.T.) ;
#8633 = EDGE_CURVE('',#6775,#6774,#5140,.T.) ;
#8634 = EDGE_CURVE('',#6777,#6610,#4083,.T.) ;
#8635 = EDGE_CURVE('',#6777,#6778,#4084,.T.) ;
#8636 = EDGE_CURVE('',#6607,#6778,#4085,.T.) ;
#8637 = EDGE_CURVE('',#6605,#6779,#4086,.T.) ;
#8638 = EDGE_CURVE('',#6780,#6779,#4087,.T.) ;
#8639 = EDGE_CURVE('',#6780,#6608,#4088,.T.) ;
#8640 = EDGE_CURVE('',#6780,#6777,#5141,.T.) ;
#8641 = EDGE_CURVE('',#6779,#6778,#5142,.T.) ;
#8642 = EDGE_CURVE('',#6781,#6599,#4089,.T.) ;
#8643 = EDGE_CURVE('',#6781,#6782,#4090,.T.) ;
#8644 = EDGE_CURVE('',#6603,#6782,#4091,.T.) ;
#8645 = EDGE_CURVE('',#6601,#6783,#4092,.T.) ;
#8646 = EDGE_CURVE('',#6784,#6783,#4093,.T.) ;
#8647 = EDGE_CURVE('',#6784,#6598,#4094,.T.) ;
#8648 = EDGE_CURVE('',#6784,#6781,#5143,.T.) ;
#8649 = EDGE_CURVE('',#6783,#6782,#5144,.T.) ;
#8650 = EDGE_CURVE('',#6785,#6595,#4095,.T.) ;
#8651 = EDGE_CURVE('',#6785,#6786,#4096,.T.) ;
#8652 = EDGE_CURVE('',#6597,#6786,#4097,.T.) ;
#8653 = EDGE_CURVE('',#6596,#6787,#4098,.T.) ;
#8654 = EDGE_CURVE('',#6788,#6787,#4099,.T.) ;
#8655 = EDGE_CURVE('',#6788,#6594,#4100,.T.) ;
#8656 = EDGE_CURVE('',#6788,#6785,#5145,.T.) ;
#8657 = EDGE_CURVE('',#6787,#6786,#5146,.T.) ;
#8658 = EDGE_CURVE('',#6789,#6591,#4101,.T.) ;
#8659 = EDGE_CURVE('',#6789,#6790,#4102,.T.) ;
#8660 = EDGE_CURVE('',#6593,#6790,#4103,.T.) ;
#8661 = EDGE_CURVE('',#6592,#6791,#4104,.T.) ;
#8662 = EDGE_CURVE('',#6792,#6791,#4105,.T.) ;
#8663 = EDGE_CURVE('',#6792,#6590,#4106,.T.) ;
#8664 = EDGE_CURVE('',#6792,#6789,#5147,.T.) ;
#8665 = EDGE_CURVE('',#6791,#6790,#5148,.T.) ;
#8666 = EDGE_CURVE('',#6793,#6587,#4107,.T.) ;
#8667 = EDGE_CURVE('',#6793,#6794,#4108,.T.) ;
#8668 = EDGE_CURVE('',#6589,#6794,#4109,.T.) ;
#8669 = EDGE_CURVE('',#6588,#6795,#4110,.T.) ;
#8670 = EDGE_CURVE('',#6796,#6795,#4111,.T.) ;
#8671 = EDGE_CURVE('',#6796,#6586,#4112,.T.) ;
#8672 = EDGE_CURVE('',#6796,#6793,#5149,.T.) ;
#8673 = EDGE_CURVE('',#6795,#6794,#5150,.T.) ;
#8674 = EDGE_CURVE('',#6797,#6583,#4113,.T.) ;
#8675 = EDGE_CURVE('',#6797,#6798,#4114,.T.) ;
#8676 = EDGE_CURVE('',#6585,#6798,#4115,.T.) ;
#8677 = EDGE_CURVE('',#6584,#6799,#4116,.T.) ;
#8678 = EDGE_CURVE('',#6800,#6799,#4117,.T.) ;
#8679 = EDGE_CURVE('',#6800,#6582,#4118,.T.) ;
#8680 = EDGE_CURVE('',#6800,#6797,#5151,.T.) ;
#8681 = EDGE_CURVE('',#6799,#6798,#5152,.T.) ;
#8682 = EDGE_CURVE('',#6801,#6579,#4119,.T.) ;
#8683 = EDGE_CURVE('',#6801,#6802,#4120,.T.) ;
#8684 = EDGE_CURVE('',#6581,#6802,#4121,.T.) ;
#8685 = EDGE_CURVE('',#6580,#6803,#4122,.T.) ;
#8686 = EDGE_CURVE('',#6804,#6803,#4123,.T.) ;
#8687 = EDGE_CURVE('',#6804,#6578,#4124,.T.) ;
#8688 = EDGE_CURVE('',#6804,#6801,#5153,.T.) ;
#8689 = EDGE_CURVE('',#6803,#6802,#5154,.T.) ;
#8690 = EDGE_CURVE('',#6805,#6575,#4125,.T.) ;
#8691 = EDGE_CURVE('',#6805,#6806,#4126,.T.) ;
#8692 = EDGE_CURVE('',#6577,#6806,#4127,.T.) ;
#8693 = EDGE_CURVE('',#6576,#6807,#4128,.T.) ;
#8694 = EDGE_CURVE('',#6808,#6807,#4129,.T.) ;
#8695 = EDGE_CURVE('',#6808,#6574,#4130,.T.) ;
#8696 = EDGE_CURVE('',#6808,#6805,#5155,.T.) ;
#8697 = EDGE_CURVE('',#6807,#6806,#5156,.T.) ;
#8698 = EDGE_CURVE('',#6809,#6606,#4131,.T.) ;
#8699 = EDGE_CURVE('',#6809,#6810,#4132,.T.) ;
#8700 = EDGE_CURVE('',#6573,#6810,#4133,.T.) ;
#8701 = EDGE_CURVE('',#6572,#6811,#4134,.T.) ;
#8702 = EDGE_CURVE('',#6812,#6811,#4135,.T.) ;
#8703 = EDGE_CURVE('',#6812,#6604,#4136,.T.) ;
#8704 = EDGE_CURVE('',#6812,#6809,#5157,.T.) ;
#8705 = EDGE_CURVE('',#6811,#6810,#5158,.T.) ;
#8706 = EDGE_CURVE('',#6813,#6602,#4137,.T.) ;
#8707 = EDGE_CURVE('',#6813,#6814,#4138,.T.) ;
#8708 = EDGE_CURVE('',#6571,#6814,#4139,.T.) ;
#8709 = EDGE_CURVE('',#6569,#6815,#4140,.T.) ;
#8710 = EDGE_CURVE('',#6816,#6815,#4141,.T.) ;
#8711 = EDGE_CURVE('',#6816,#6600,#4142,.T.) ;
#8712 = EDGE_CURVE('',#6816,#6813,#5159,.T.) ;
#8713 = EDGE_CURVE('',#6815,#6814,#5160,.T.) ;
#8714 = EDGE_CURVE('',#6817,#6570,#4143,.T.) ;
#8715 = EDGE_CURVE('',#6817,#6818,#4144,.T.) ;
#8716 = EDGE_CURVE('',#6567,#6818,#4145,.T.) ;
#8717 = EDGE_CURVE('',#6565,#6819,#4146,.T.) ;
#8718 = EDGE_CURVE('',#6820,#6819,#4147,.T.) ;
#8719 = EDGE_CURVE('',#6820,#6568,#4148,.T.) ;
#8720 = EDGE_CURVE('',#6820,#6817,#5161,.T.) ;
#8721 = EDGE_CURVE('',#6819,#6818,#5162,.T.) ;
#8722 = EDGE_CURVE('',#6821,#6566,#4149,.T.) ;
#8723 = EDGE_CURVE('',#6821,#6822,#4150,.T.) ;
#8724 = EDGE_CURVE('',#6563,#6822,#4151,.T.) ;
#8725 = EDGE_CURVE('',#6561,#6823,#4152,.T.) ;
#8726 = EDGE_CURVE('',#6824,#6823,#4153,.T.) ;
#8727 = EDGE_CURVE('',#6824,#6564,#4154,.T.) ;
#8728 = EDGE_CURVE('',#6824,#6821,#5163,.T.) ;
#8729 = EDGE_CURVE('',#6823,#6822,#5164,.T.) ;
#8730 = EDGE_CURVE('',#6825,#6562,#4155,.T.) ;
#8731 = EDGE_CURVE('',#6825,#6826,#4156,.T.) ;
#8732 = EDGE_CURVE('',#6559,#6826,#4157,.T.) ;
#8733 = EDGE_CURVE('',#6557,#6827,#4158,.T.) ;
#8734 = EDGE_CURVE('',#6828,#6827,#4159,.T.) ;
#8735 = EDGE_CURVE('',#6828,#6560,#4160,.T.) ;
#8736 = EDGE_CURVE('',#6828,#6825,#5165,.T.) ;
#8737 = EDGE_CURVE('',#6827,#6826,#5166,.T.) ;
#8738 = EDGE_CURVE('',#6829,#6558,#4161,.T.) ;
#8739 = EDGE_CURVE('',#6829,#6830,#4162,.T.) ;
#8740 = EDGE_CURVE('',#6555,#6830,#4163,.T.) ;
#8741 = EDGE_CURVE('',#6553,#6831,#4164,.T.) ;
#8742 = EDGE_CURVE('',#6832,#6831,#4165,.T.) ;
#8743 = EDGE_CURVE('',#6832,#6556,#4166,.T.) ;
#8744 = EDGE_CURVE('',#6832,#6829,#5167,.T.) ;
#8745 = EDGE_CURVE('',#6831,#6830,#5168,.T.) ;
#8746 = EDGE_CURVE('',#6833,#6554,#4167,.T.) ;
#8747 = EDGE_CURVE('',#6833,#6834,#4168,.T.) ;
#8748 = EDGE_CURVE('',#6551,#6834,#4169,.T.) ;
#8749 = EDGE_CURVE('',#6549,#6835,#4170,.T.) ;
#8750 = EDGE_CURVE('',#6836,#6835,#4171,.T.) ;
#8751 = EDGE_CURVE('',#6836,#6552,#4172,.T.) ;
#8752 = EDGE_CURVE('',#6836,#6833,#5169,.T.) ;
#8753 = EDGE_CURVE('',#6835,#6834,#5170,.T.) ;
#8754 = EDGE_CURVE('',#6837,#6550,#4173,.T.) ;
#8755 = EDGE_CURVE('',#6837,#6838,#4174,.T.) ;
#8756 = EDGE_CURVE('',#6547,#6838,#4175,.T.) ;
#8757 = EDGE_CURVE('',#6545,#6839,#4176,.T.) ;
#8758 = EDGE_CURVE('',#6840,#6839,#4177,.T.) ;
#8759 = EDGE_CURVE('',#6840,#6548,#4178,.T.) ;
#8760 = EDGE_CURVE('',#6840,#6837,#5171,.T.) ;
#8761 = EDGE_CURVE('',#6839,#6838,#5172,.T.) ;
#8762 = EDGE_CURVE('',#6841,#6546,#4179,.T.) ;
#8763 = EDGE_CURVE('',#6841,#6842,#4180,.T.) ;
#8764 = EDGE_CURVE('',#6543,#6842,#4181,.T.) ;
#8765 = EDGE_CURVE('',#6541,#6843,#4182,.T.) ;
#8766 = EDGE_CURVE('',#6844,#6843,#4183,.T.) ;
#8767 = EDGE_CURVE('',#6844,#6544,#4184,.T.) ;
#8768 = EDGE_CURVE('',#6844,#6841,#5173,.T.) ;
#8769 = EDGE_CURVE('',#6843,#6842,#5174,.T.) ;
#8770 = EDGE_CURVE('',#6845,#6542,#4185,.T.) ;
#8771 = EDGE_CURVE('',#6845,#6846,#4186,.T.) ;
#8772 = EDGE_CURVE('',#6539,#6846,#4187,.T.) ;
#8773 = EDGE_CURVE('',#6537,#6847,#4188,.T.) ;
#8774 = EDGE_CURVE('',#6848,#6847,#4189,.T.) ;
#8775 = EDGE_CURVE('',#6848,#6540,#4190,.T.) ;
#8776 = EDGE_CURVE('',#6848,#6845,#5175,.T.) ;
#8777 = EDGE_CURVE('',#6847,#6846,#5176,.T.) ;
#8778 = EDGE_CURVE('',#6849,#6538,#4191,.T.) ;
#8779 = EDGE_CURVE('',#6849,#6850,#4192,.T.) ;
#8780 = EDGE_CURVE('',#6535,#6850,#4193,.T.) ;
#8781 = EDGE_CURVE('',#6533,#6851,#4194,.T.) ;
#8782 = EDGE_CURVE('',#6852,#6851,#4195,.T.) ;
#8783 = EDGE_CURVE('',#6852,#6536,#4196,.T.) ;
#8784 = EDGE_CURVE('',#6852,#6849,#5177,.T.) ;
#8785 = EDGE_CURVE('',#6851,#6850,#5178,.T.) ;
#8786 = EDGE_CURVE('',#6853,#6527,#4197,.T.) ;
#8787 = EDGE_CURVE('',#6853,#6854,#4198,.T.) ;
#8788 = EDGE_CURVE('',#6531,#6854,#4199,.T.) ;
#8789 = EDGE_CURVE('',#6529,#6855,#4200,.T.) ;
#8790 = EDGE_CURVE('',#6856,#6855,#4201,.T.) ;
#8791 = EDGE_CURVE('',#6856,#6526,#4202,.T.) ;
#8792 = EDGE_CURVE('',#6856,#6853,#5179,.T.) ;
#8793 = EDGE_CURVE('',#6855,#6854,#5180,.T.) ;
#8794 = EDGE_CURVE('',#6857,#6534,#4203,.T.) ;
#8795 = EDGE_CURVE('',#6857,#6858,#4204,.T.) ;
#8796 = EDGE_CURVE('',#6525,#6858,#4205,.T.) ;
#8797 = EDGE_CURVE('',#6524,#6859,#4206,.T.) ;
#8798 = EDGE_CURVE('',#6860,#6859,#4207,.T.) ;
#8799 = EDGE_CURVE('',#6860,#6532,#4208,.T.) ;
#8800 = EDGE_CURVE('',#6860,#6857,#5181,.T.) ;
#8801 = EDGE_CURVE('',#6859,#6858,#5182,.T.) ;
#8802 = EDGE_CURVE('',#6861,#6530,#4209,.T.) ;
#8803 = EDGE_CURVE('',#6861,#6862,#4210,.T.) ;
#8804 = EDGE_CURVE('',#6523,#6862,#4211,.T.) ;
#8805 = EDGE_CURVE('',#6521,#6863,#4212,.T.) ;
#8806 = EDGE_CURVE('',#6864,#6863,#4213,.T.) ;
#8807 = EDGE_CURVE('',#6864,#6528,#4214,.T.) ;
#8808 = EDGE_CURVE('',#6864,#6861,#5183,.T.) ;
#8809 = EDGE_CURVE('',#6863,#6862,#5184,.T.) ;
#8810 = EDGE_CURVE('',#6865,#6522,#4215,.T.) ;
#8811 = EDGE_CURVE('',#6865,#6866,#4216,.T.) ;
#8812 = EDGE_CURVE('',#6519,#6866,#4217,.T.) ;
#8813 = EDGE_CURVE('',#6517,#6867,#4218,.T.) ;
#8814 = EDGE_CURVE('',#6868,#6867,#4219,.T.) ;
#8815 = EDGE_CURVE('',#6868,#6520,#4220,.T.) ;
#8816 = EDGE_CURVE('',#6868,#6865,#5185,.T.) ;
#8817 = EDGE_CURVE('',#6867,#6866,#5186,.T.) ;
#8818 = EDGE_CURVE('',#6869,#6518,#4221,.T.) ;
#8819 = EDGE_CURVE('',#6869,#6870,#4222,.T.) ;
#8820 = EDGE_CURVE('',#6515,#6870,#4223,.T.) ;
#8821 = EDGE_CURVE('',#6513,#6871,#4224,.T.) ;
#8822 = EDGE_CURVE('',#6872,#6871,#4225,.T.) ;
#8823 = EDGE_CURVE('',#6872,#6516,#4226,.T.) ;
#8824 = EDGE_CURVE('',#6872,#6869,#5187,.T.) ;
#8825 = EDGE_CURVE('',#6871,#6870,#5188,.T.) ;
#8826 = EDGE_CURVE('',#6873,#6514,#4227,.T.) ;
#8827 = EDGE_CURVE('',#6873,#6874,#4228,.T.) ;
#8828 = EDGE_CURVE('',#6511,#6874,#4229,.T.) ;
#8829 = EDGE_CURVE('',#6509,#6875,#4230,.T.) ;
#8830 = EDGE_CURVE('',#6876,#6875,#4231,.T.) ;
#8831 = EDGE_CURVE('',#6876,#6512,#4232,.T.) ;
#8832 = EDGE_CURVE('',#6876,#6873,#5189,.T.) ;
#8833 = EDGE_CURVE('',#6875,#6874,#5190,.T.) ;
#8834 = EDGE_CURVE('',#6877,#6510,#4233,.T.) ;
#8835 = EDGE_CURVE('',#6877,#6878,#4234,.T.) ;
#8836 = EDGE_CURVE('',#6507,#6878,#4235,.T.) ;
#8837 = EDGE_CURVE('',#6505,#6879,#4236,.T.) ;
#8838 = EDGE_CURVE('',#6880,#6879,#4237,.T.) ;
#8839 = EDGE_CURVE('',#6880,#6508,#4238,.T.) ;
#8840 = EDGE_CURVE('',#6880,#6877,#5191,.T.) ;
#8841 = EDGE_CURVE('',#6879,#6878,#5192,.T.) ;
#8842 = EDGE_CURVE('',#6881,#6506,#4239,.T.) ;
#8843 = EDGE_CURVE('',#6881,#6882,#4240,.T.) ;
#8844 = EDGE_CURVE('',#6503,#6882,#4241,.T.) ;
#8845 = EDGE_CURVE('',#6501,#6883,#4242,.T.) ;
#8846 = EDGE_CURVE('',#6884,#6883,#4243,.T.) ;
#8847 = EDGE_CURVE('',#6884,#6504,#4244,.T.) ;
#8848 = EDGE_CURVE('',#6884,#6881,#5193,.T.) ;
#8849 = EDGE_CURVE('',#6883,#6882,#5194,.T.) ;
#8850 = EDGE_CURVE('',#6885,#6502,#4245,.T.) ;
#8851 = EDGE_CURVE('',#6885,#6886,#4246,.T.) ;
#8852 = EDGE_CURVE('',#6499,#6886,#4247,.T.) ;
#8853 = EDGE_CURVE('',#6497,#6887,#4248,.T.) ;
#8854 = EDGE_CURVE('',#6888,#6887,#4249,.T.) ;
#8855 = EDGE_CURVE('',#6888,#6500,#4250,.T.) ;
#8856 = EDGE_CURVE('',#6888,#6885,#5195,.T.) ;
#8857 = EDGE_CURVE('',#6887,#6886,#5196,.T.) ;
#8858 = EDGE_CURVE('',#6889,#6498,#4251,.T.) ;
#8859 = EDGE_CURVE('',#6889,#6890,#4252,.T.) ;
#8860 = EDGE_CURVE('',#6495,#6890,#4253,.T.) ;
#8861 = EDGE_CURVE('',#6493,#6891,#4254,.T.) ;
#8862 = EDGE_CURVE('',#6892,#6891,#4255,.T.) ;
#8863 = EDGE_CURVE('',#6892,#6496,#4256,.T.) ;
#8864 = EDGE_CURVE('',#6892,#6889,#5197,.T.) ;
#8865 = EDGE_CURVE('',#6891,#6890,#5198,.T.) ;
#8866 = EDGE_CURVE('',#6893,#6494,#4257,.T.) ;
#8867 = EDGE_CURVE('',#6893,#6894,#4258,.T.) ;
#8868 = EDGE_CURVE('',#6491,#6894,#4259,.T.) ;
#8869 = EDGE_CURVE('',#6489,#6895,#4260,.T.) ;
#8870 = EDGE_CURVE('',#6896,#6895,#4261,.T.) ;
#8871 = EDGE_CURVE('',#6896,#6492,#4262,.T.) ;
#8872 = EDGE_CURVE('',#6896,#6893,#5199,.T.) ;
#8873 = EDGE_CURVE('',#6895,#6894,#5200,.T.) ;
#8874 = EDGE_CURVE('',#6897,#6490,#4263,.T.) ;
#8875 = EDGE_CURVE('',#6897,#6898,#4264,.T.) ;
#8876 = EDGE_CURVE('',#6487,#6898,#4265,.T.) ;
#8877 = EDGE_CURVE('',#6485,#6899,#4266,.T.) ;
#8878 = EDGE_CURVE('',#6900,#6899,#4267,.T.) ;
#8879 = EDGE_CURVE('',#6900,#6488,#4268,.T.) ;
#8880 = EDGE_CURVE('',#6900,#6897,#5201,.T.) ;
#8881 = EDGE_CURVE('',#6899,#6898,#5202,.T.) ;
#8882 = EDGE_CURVE('',#6901,#6486,#4269,.T.) ;
#8883 = EDGE_CURVE('',#6901,#6902,#4270,.T.) ;
#8884 = EDGE_CURVE('',#6483,#6902,#4271,.T.) ;
#8885 = EDGE_CURVE('',#6481,#6903,#4272,.T.) ;
#8886 = EDGE_CURVE('',#6904,#6903,#4273,.T.) ;
#8887 = EDGE_CURVE('',#6904,#6484,#4274,.T.) ;
#8888 = EDGE_CURVE('',#6904,#6901,#5203,.T.) ;
#8889 = EDGE_CURVE('',#6903,#6902,#5204,.T.) ;
#8890 = EDGE_CURVE('',#6905,#6482,#4275,.T.) ;
#8891 = EDGE_CURVE('',#6905,#6906,#4276,.T.) ;
#8892 = EDGE_CURVE('',#6479,#6906,#4277,.T.) ;
#8893 = EDGE_CURVE('',#6477,#6907,#4278,.T.) ;
#8894 = EDGE_CURVE('',#6908,#6907,#4279,.T.) ;
#8895 = EDGE_CURVE('',#6908,#6480,#4280,.T.) ;
#8896 = EDGE_CURVE('',#6908,#6905,#5205,.T.) ;
#8897 = EDGE_CURVE('',#6907,#6906,#5206,.T.) ;
#8898 = EDGE_CURVE('',#6909,#6471,#4281,.T.) ;
#8899 = EDGE_CURVE('',#6909,#6910,#4282,.T.) ;
#8900 = EDGE_CURVE('',#6475,#6910,#4283,.T.) ;
#8901 = EDGE_CURVE('',#6473,#6911,#4284,.T.) ;
#8902 = EDGE_CURVE('',#6912,#6911,#4285,.T.) ;
#8903 = EDGE_CURVE('',#6912,#6470,#4286,.T.) ;
#8904 = EDGE_CURVE('',#6912,#6909,#5207,.T.) ;
#8905 = EDGE_CURVE('',#6911,#6910,#5208,.T.) ;
#8906 = EDGE_CURVE('',#6913,#6467,#4287,.T.) ;
#8907 = EDGE_CURVE('',#6913,#6914,#4288,.T.) ;
#8908 = EDGE_CURVE('',#6469,#6914,#4289,.T.) ;
#8909 = EDGE_CURVE('',#6468,#6915,#4290,.T.) ;
#8910 = EDGE_CURVE('',#6916,#6915,#4291,.T.) ;
#8911 = EDGE_CURVE('',#6916,#6466,#4292,.T.) ;
#8912 = EDGE_CURVE('',#6916,#6913,#5209,.T.) ;
#8913 = EDGE_CURVE('',#6915,#6914,#5210,.T.) ;
#8914 = EDGE_CURVE('',#6917,#6463,#4293,.T.) ;
#8915 = EDGE_CURVE('',#6917,#6918,#4294,.T.) ;
#8916 = EDGE_CURVE('',#6465,#6918,#4295,.T.) ;
#8917 = EDGE_CURVE('',#6464,#6919,#4296,.T.) ;
#8918 = EDGE_CURVE('',#6920,#6919,#4297,.T.) ;
#8919 = EDGE_CURVE('',#6920,#6462,#4298,.T.) ;
#8920 = EDGE_CURVE('',#6920,#6917,#5211,.T.) ;
#8921 = EDGE_CURVE('',#6919,#6918,#5212,.T.) ;
#8922 = EDGE_CURVE('',#6921,#6478,#4299,.T.) ;
#8923 = EDGE_CURVE('',#6921,#6922,#4300,.T.) ;
#8924 = EDGE_CURVE('',#6461,#6922,#4301,.T.) ;
#8925 = EDGE_CURVE('',#6460,#6923,#4302,.T.) ;
#8926 = EDGE_CURVE('',#6924,#6923,#4303,.T.) ;
#8927 = EDGE_CURVE('',#6924,#6476,#4304,.T.) ;
#8928 = EDGE_CURVE('',#6924,#6921,#5213,.T.) ;
#8929 = EDGE_CURVE('',#6923,#6922,#5214,.T.) ;
#8930 = EDGE_CURVE('',#6925,#6474,#4305,.T.) ;
#8931 = EDGE_CURVE('',#6925,#6926,#4306,.T.) ;
#8932 = EDGE_CURVE('',#6459,#6926,#4307,.T.) ;
#8933 = EDGE_CURVE('',#6457,#6927,#4308,.T.) ;
#8934 = EDGE_CURVE('',#6928,#6927,#4309,.T.) ;
#8935 = EDGE_CURVE('',#6928,#6472,#4310,.T.) ;
#8936 = EDGE_CURVE('',#6928,#6925,#5215,.T.) ;
#8937 = EDGE_CURVE('',#6927,#6926,#5216,.T.) ;
#8938 = EDGE_CURVE('',#6929,#6458,#4311,.T.) ;
#8939 = EDGE_CURVE('',#6929,#6930,#4312,.T.) ;
#8940 = EDGE_CURVE('',#6455,#6930,#4313,.T.) ;
#8941 = EDGE_CURVE('',#6453,#6931,#4314,.T.) ;
#8942 = EDGE_CURVE('',#6932,#6931,#4315,.T.) ;
#8943 = EDGE_CURVE('',#6932,#6456,#4316,.T.) ;
#8944 = EDGE_CURVE('',#6932,#6929,#5217,.T.) ;
#8945 = EDGE_CURVE('',#6931,#6930,#5218,.T.) ;
#8946 = EDGE_CURVE('',#6933,#6454,#4317,.T.) ;
#8947 = EDGE_CURVE('',#6933,#6934,#4318,.T.) ;
#8948 = EDGE_CURVE('',#6451,#6934,#4319,.T.) ;
#8949 = EDGE_CURVE('',#6449,#6935,#4320,.T.) ;
#8950 = EDGE_CURVE('',#6936,#6935,#4321,.T.) ;
#8951 = EDGE_CURVE('',#6936,#6452,#4322,.T.) ;
#8952 = EDGE_CURVE('',#6936,#6933,#5219,.T.) ;
#8953 = EDGE_CURVE('',#6935,#6934,#5220,.T.) ;
#8954 = EDGE_CURVE('',#6937,#6450,#4323,.T.) ;
#8955 = EDGE_CURVE('',#6937,#6938,#4324,.T.) ;
#8956 = EDGE_CURVE('',#6445,#6938,#4325,.T.) ;
#8957 = EDGE_CURVE('',#6444,#6939,#4326,.T.) ;
#8958 = EDGE_CURVE('',#6940,#6939,#4327,.T.) ;
#8959 = EDGE_CURVE('',#6940,#6448,#4328,.T.) ;
#8960 = EDGE_CURVE('',#6940,#6937,#5221,.T.) ;
#8961 = EDGE_CURVE('',#6939,#6938,#5222,.T.) ;
#8962 = EDGE_CURVE('',#6941,#6942,#4329,.T.) ;
#8963 = EDGE_CURVE('',#6942,#6941,#4330,.T.) ;
#8964 = EDGE_CURVE('',#6942,#6943,#5223,.T.) ;
#8965 = EDGE_CURVE('',#6943,#6943,#4331,.T.) ;
#8966 = EDGE_CURVE('',#6943,#6944,#5224,.T.) ;
#8967 = EDGE_CURVE('',#6944,#6944,#4332,.T.) ;
#8968 = EDGE_CURVE('',#6945,#6945,#4333,.T.) ;
#8969 = EDGE_CURVE('',#6946,#6947,#4334,.T.) ;
#8970 = EDGE_CURVE('',#6947,#6945,#5225,.T.) ;
#8971 = EDGE_CURVE('',#6947,#6946,#4335,.T.) ;
#8972 = EDGE_CURVE('',#6946,#6948,#5226,.T.) ;
#8973 = EDGE_CURVE('',#6948,#6948,#4336,.T.) ;
#8974 = EDGE_CURVE('',#6948,#6949,#5227,.T.) ;
#8975 = EDGE_CURVE('',#6949,#6949,#4337,.T.) ;
#8976 = EDGE_CURVE('',#6950,#6950,#4338,.T.) ;
#8977 = EDGE_CURVE('',#6941,#6950,#5228,.T.) ;
#8978 = EDGE_CURVE('',#6951,#6952,#83,.T.) ;
#8979 = EDGE_CURVE('',#6953,#6951,#5229,.T.) ;
#8980 = EDGE_CURVE('',#6954,#6953,#5230,.T.) ;
#8981 = EDGE_CURVE('',#6952,#6954,#5231,.T.) ;
#8982 = EDGE_CURVE('',#6955,#6956,#84,.T.) ;
#8983 = EDGE_CURVE('',#6955,#6957,#5232,.T.) ;
#8984 = EDGE_CURVE('',#6958,#6957,#5233,.T.) ;
#8985 = EDGE_CURVE('',#6956,#6958,#5234,.T.) ;
#8986 = EDGE_CURVE('',#6955,#6952,#4339,.T.) ;
#8987 = EDGE_CURVE('',#6957,#6954,#4340,.T.) ;
#8988 = EDGE_CURVE('',#6959,#6953,#4341,.T.) ;
#8989 = EDGE_CURVE('',#6959,#6960,#5235,.T.) ;
#8990 = EDGE_CURVE('',#6960,#6961,#4342,.T.) ;
#8991 = EDGE_CURVE('',#6961,#6962,#5236,.T.) ;
#8992 = EDGE_CURVE('',#6963,#6962,#4343,.T.) ;
#8993 = EDGE_CURVE('',#6963,#6964,#5237,.T.) ;
#8994 = EDGE_CURVE('',#6964,#6965,#4344,.T.) ;
#8995 = EDGE_CURVE('',#6965,#6966,#5238,.T.) ;
#8996 = EDGE_CURVE('',#6967,#6966,#4345,.T.) ;
#8997 = EDGE_CURVE('',#6967,#6968,#5239,.T.) ;
#8998 = EDGE_CURVE('',#6968,#6969,#4346,.T.) ;
#8999 = EDGE_CURVE('',#6969,#6970,#5240,.T.) ;
#9000 = EDGE_CURVE('',#6958,#6970,#4347,.T.) ;
#9001 = EDGE_CURVE('',#6971,#6971,#4348,.F.) ;
#9002 = EDGE_CURVE('',#6972,#6951,#4349,.T.) ;
#9003 = EDGE_CURVE('',#6972,#6959,#5241,.T.) ;
#9004 = EDGE_CURVE('',#6952,#6973,#4350,.T.) ;
#9005 = EDGE_CURVE('',#6973,#6972,#85,.T.) ;
#9006 = EDGE_CURVE('',#6974,#6975,#86,.T.) ;
#9007 = EDGE_CURVE('',#6962,#6974,#5242,.T.) ;
#9008 = EDGE_CURVE('',#6975,#6961,#5243,.T.) ;
#9009 = EDGE_CURVE('',#6973,#6960,#5244,.T.) ;
#9010 = EDGE_CURVE('',#6973,#6975,#4351,.T.) ;
#9011 = EDGE_CURVE('',#6976,#6974,#4352,.T.) ;
#9012 = EDGE_CURVE('',#6976,#6963,#5245,.T.) ;
#9013 = EDGE_CURVE('',#6975,#6977,#4353,.T.) ;
#9014 = EDGE_CURVE('',#6977,#6976,#87,.T.) ;
#9015 = EDGE_CURVE('',#6978,#6979,#88,.T.) ;
#9016 = EDGE_CURVE('',#6966,#6978,#5246,.T.) ;
#9017 = EDGE_CURVE('',#6979,#6965,#5247,.T.) ;
#9018 = EDGE_CURVE('',#6977,#6964,#5248,.T.) ;
#9019 = EDGE_CURVE('',#6977,#6979,#4354,.T.) ;
#9020 = EDGE_CURVE('',#6980,#6978,#4355,.T.) ;
#9021 = EDGE_CURVE('',#6980,#6967,#5249,.T.) ;
#9022 = EDGE_CURVE('',#6979,#6981,#4356,.T.) ;
#9023 = EDGE_CURVE('',#6981,#6980,#89,.T.) ;
#9024 = EDGE_CURVE('',#6982,#6983,#90,.T.) ;
#9025 = EDGE_CURVE('',#6970,#6982,#5250,.T.) ;
#9026 = EDGE_CURVE('',#6983,#6969,#5251,.T.) ;
#9027 = EDGE_CURVE('',#6981,#6968,#5252,.T.) ;
#9028 = EDGE_CURVE('',#6981,#6983,#4357,.T.) ;
#9029 = EDGE_CURVE('',#6956,#6982,#4358,.T.) ;
#9030 = EDGE_CURVE('',#6983,#6955,#4359,.T.) ;
#9031 = EDGE_CURVE('',#6984,#6984,#4360,.F.) ;
#9032 = EDGE_CURVE('',#6971,#6984,#5253,.T.) ;
#9033 = EDGE_CURVE('',#6985,#6985,#4361,.T.) ;
#9034 = EDGE_CURVE('',#6985,#6986,#5254,.T.) ;
#9035 = EDGE_CURVE('',#6986,#6987,#4362,.T.) ;
#9036 = EDGE_CURVE('',#6987,#6988,#333,.T.) ;
#9037 = EDGE_CURVE('',#6989,#6988,#334,.T.) ;
#9038 = EDGE_CURVE('',#6989,#6990,#4363,.T.) ;
#9039 = EDGE_CURVE('',#6991,#6990,#335,.T.) ;
#9040 = EDGE_CURVE('',#6991,#6992,#336,.T.) ;
#9041 = EDGE_CURVE('',#6992,#6993,#4364,.T.) ;
#9042 = EDGE_CURVE('',#6993,#6994,#337,.T.) ;
#9043 = EDGE_CURVE('',#6995,#6994,#338,.T.) ;
#9044 = EDGE_CURVE('',#6995,#6996,#4365,.T.) ;
#9045 = EDGE_CURVE('',#6997,#6996,#339,.T.) ;
#9046 = EDGE_CURVE('',#6997,#6998,#340,.T.) ;
#9047 = EDGE_CURVE('',#6998,#6999,#4366,.T.) ;
#9048 = EDGE_CURVE('',#6999,#7000,#341,.T.) ;
#9049 = EDGE_CURVE('',#7001,#7000,#342,.T.) ;
#9050 = EDGE_CURVE('',#7001,#7002,#4367,.T.) ;
#9051 = EDGE_CURVE('',#7003,#7002,#343,.T.) ;
#9052 = EDGE_CURVE('',#7003,#7004,#344,.T.) ;
#9053 = EDGE_CURVE('',#7004,#7005,#4368,.T.) ;
#9054 = EDGE_CURVE('',#7005,#7006,#345,.T.) ;
#9055 = EDGE_CURVE('',#7007,#7006,#346,.T.) ;
#9056 = EDGE_CURVE('',#7007,#7008,#4369,.T.) ;
#9057 = EDGE_CURVE('',#7009,#7008,#347,.T.) ;
#9058 = EDGE_CURVE('',#7009,#7010,#348,.T.) ;
#9059 = EDGE_CURVE('',#7010,#7011,#4370,.T.) ;
#9060 = EDGE_CURVE('',#7011,#7012,#349,.T.) ;
#9061 = EDGE_CURVE('',#7013,#7012,#350,.T.) ;
#9062 = EDGE_CURVE('',#7013,#7014,#4371,.T.) ;
#9063 = EDGE_CURVE('',#7015,#7014,#351,.T.) ;
#9064 = EDGE_CURVE('',#7015,#7016,#352,.T.) ;
#9065 = EDGE_CURVE('',#7016,#7017,#4372,.T.) ;
#9066 = EDGE_CURVE('',#7017,#7018,#353,.T.) ;
#9067 = EDGE_CURVE('',#7019,#7018,#354,.T.) ;
#9068 = EDGE_CURVE('',#7019,#7020,#4373,.T.) ;
#9069 = EDGE_CURVE('',#7021,#7020,#355,.T.) ;
#9070 = EDGE_CURVE('',#7021,#7022,#356,.T.) ;
#9071 = EDGE_CURVE('',#7022,#7023,#4374,.T.) ;
#9072 = EDGE_CURVE('',#7023,#7024,#357,.T.) ;
#9073 = EDGE_CURVE('',#7025,#7024,#358,.T.) ;
#9074 = EDGE_CURVE('',#7025,#7026,#4375,.T.) ;
#9075 = EDGE_CURVE('',#7027,#7026,#359,.T.) ;
#9076 = EDGE_CURVE('',#7027,#7028,#360,.T.) ;
#9077 = EDGE_CURVE('',#7028,#7029,#4376,.T.) ;
#9078 = EDGE_CURVE('',#7029,#7030,#361,.T.) ;
#9079 = EDGE_CURVE('',#7031,#7030,#362,.T.) ;
#9080 = EDGE_CURVE('',#7031,#7032,#4377,.T.) ;
#9081 = EDGE_CURVE('',#7033,#7032,#363,.T.) ;
#9082 = EDGE_CURVE('',#7033,#7034,#364,.T.) ;
#9083 = EDGE_CURVE('',#7034,#7035,#4378,.T.) ;
#9084 = EDGE_CURVE('',#7035,#7036,#365,.T.) ;
#9085 = EDGE_CURVE('',#7037,#7036,#366,.T.) ;
#9086 = EDGE_CURVE('',#7037,#7038,#4379,.T.) ;
#9087 = EDGE_CURVE('',#7039,#7038,#367,.T.) ;
#9088 = EDGE_CURVE('',#7039,#7040,#368,.T.) ;
#9089 = EDGE_CURVE('',#7040,#7041,#4380,.T.) ;
#9090 = EDGE_CURVE('',#7041,#7042,#369,.T.) ;
#9091 = EDGE_CURVE('',#7043,#7042,#370,.T.) ;
#9092 = EDGE_CURVE('',#7043,#7044,#4381,.T.) ;
#9093 = EDGE_CURVE('',#7045,#7044,#371,.T.) ;
#9094 = EDGE_CURVE('',#7045,#7046,#372,.T.) ;
#9095 = EDGE_CURVE('',#7046,#7047,#4382,.T.) ;
#9096 = EDGE_CURVE('',#7047,#7048,#373,.T.) ;
#9097 = EDGE_CURVE('',#7049,#7048,#374,.T.) ;
#9098 = EDGE_CURVE('',#7049,#7050,#4383,.T.) ;
#9099 = EDGE_CURVE('',#7051,#7050,#375,.T.) ;
#9100 = EDGE_CURVE('',#7051,#7052,#376,.T.) ;
#9101 = EDGE_CURVE('',#7052,#7053,#4384,.T.) ;
#9102 = EDGE_CURVE('',#7053,#7054,#377,.T.) ;
#9103 = EDGE_CURVE('',#7055,#7054,#378,.T.) ;
#9104 = EDGE_CURVE('',#7055,#7056,#4385,.T.) ;
#9105 = EDGE_CURVE('',#7057,#7056,#379,.T.) ;
#9106 = EDGE_CURVE('',#7057,#7058,#380,.T.) ;
#9107 = EDGE_CURVE('',#7058,#7059,#4386,.T.) ;
#9108 = EDGE_CURVE('',#7059,#7060,#381,.T.) ;
#9109 = EDGE_CURVE('',#7061,#7060,#382,.T.) ;
#9110 = EDGE_CURVE('',#7061,#7062,#4387,.T.) ;
#9111 = EDGE_CURVE('',#7063,#7062,#383,.T.) ;
#9112 = EDGE_CURVE('',#7063,#7064,#384,.T.) ;
#9113 = EDGE_CURVE('',#7064,#7065,#4388,.T.) ;
#9114 = EDGE_CURVE('',#7065,#7066,#385,.T.) ;
#9115 = EDGE_CURVE('',#7067,#7066,#386,.T.) ;
#9116 = EDGE_CURVE('',#7067,#7068,#4389,.T.) ;
#9117 = EDGE_CURVE('',#7069,#7068,#387,.T.) ;
#9118 = EDGE_CURVE('',#7069,#7070,#388,.T.) ;
#9119 = EDGE_CURVE('',#7070,#7071,#4390,.T.) ;
#9120 = EDGE_CURVE('',#7071,#7072,#389,.T.) ;
#9121 = EDGE_CURVE('',#7073,#7072,#390,.T.) ;
#9122 = EDGE_CURVE('',#7073,#7074,#4391,.T.) ;
#9123 = EDGE_CURVE('',#7075,#7074,#391,.T.) ;
#9124 = EDGE_CURVE('',#7075,#7076,#392,.T.) ;
#9125 = EDGE_CURVE('',#7076,#7077,#4392,.T.) ;
#9126 = EDGE_CURVE('',#7077,#7078,#393,.T.) ;
#9127 = EDGE_CURVE('',#7079,#7078,#394,.T.) ;
#9128 = EDGE_CURVE('',#7079,#7080,#4393,.T.) ;
#9129 = EDGE_CURVE('',#7081,#7080,#395,.T.) ;
#9130 = EDGE_CURVE('',#7081,#7082,#396,.T.) ;
#9131 = EDGE_CURVE('',#7082,#7083,#4394,.T.) ;
#9132 = EDGE_CURVE('',#7083,#7084,#397,.T.) ;
#9133 = EDGE_CURVE('',#7085,#7084,#398,.T.) ;
#9134 = EDGE_CURVE('',#7085,#7086,#4395,.T.) ;
#9135 = EDGE_CURVE('',#7087,#7086,#399,.T.) ;
#9136 = EDGE_CURVE('',#7087,#7088,#400,.T.) ;
#9137 = EDGE_CURVE('',#7088,#7089,#4396,.T.) ;
#9138 = EDGE_CURVE('',#7089,#7090,#401,.T.) ;
#9139 = EDGE_CURVE('',#7091,#7090,#402,.T.) ;
#9140 = EDGE_CURVE('',#7091,#7092,#4397,.T.) ;
#9141 = EDGE_CURVE('',#7093,#7092,#403,.T.) ;
#9142 = EDGE_CURVE('',#7093,#7094,#404,.T.) ;
#9143 = EDGE_CURVE('',#7094,#7095,#4398,.T.) ;
#9144 = EDGE_CURVE('',#7095,#7096,#405,.T.) ;
#9145 = EDGE_CURVE('',#7097,#7096,#406,.T.) ;
#9146 = EDGE_CURVE('',#7097,#7098,#4399,.T.) ;
#9147 = EDGE_CURVE('',#7099,#7098,#407,.T.) ;
#9148 = EDGE_CURVE('',#7099,#7100,#408,.T.) ;
#9149 = EDGE_CURVE('',#7100,#7101,#4400,.T.) ;
#9150 = EDGE_CURVE('',#7101,#7102,#409,.T.) ;
#9151 = EDGE_CURVE('',#7103,#7102,#410,.T.) ;
#9152 = EDGE_CURVE('',#7103,#7104,#4401,.T.) ;
#9153 = EDGE_CURVE('',#7105,#7104,#411,.T.) ;
#9154 = EDGE_CURVE('',#7105,#7106,#412,.T.) ;
#9155 = EDGE_CURVE('',#7106,#7107,#4402,.T.) ;
#9156 = EDGE_CURVE('',#7107,#7108,#413,.T.) ;
#9157 = EDGE_CURVE('',#7109,#7108,#414,.T.) ;
#9158 = EDGE_CURVE('',#7109,#7110,#4403,.T.) ;
#9159 = EDGE_CURVE('',#7111,#7110,#415,.T.) ;
#9160 = EDGE_CURVE('',#7111,#7112,#416,.T.) ;
#9161 = EDGE_CURVE('',#7112,#7113,#4404,.T.) ;
#9162 = EDGE_CURVE('',#7113,#7114,#417,.T.) ;
#9163 = EDGE_CURVE('',#7115,#7114,#418,.T.) ;
#9164 = EDGE_CURVE('',#7115,#7116,#4405,.T.) ;
#9165 = EDGE_CURVE('',#7117,#7116,#419,.T.) ;
#9166 = EDGE_CURVE('',#7117,#7118,#420,.T.) ;
#9167 = EDGE_CURVE('',#7118,#7119,#4406,.T.) ;
#9168 = EDGE_CURVE('',#7119,#7120,#421,.T.) ;
#9169 = EDGE_CURVE('',#7121,#7120,#422,.T.) ;
#9170 = EDGE_CURVE('',#7121,#7122,#4407,.T.) ;
#9171 = EDGE_CURVE('',#7123,#7122,#423,.T.) ;
#9172 = EDGE_CURVE('',#7123,#7124,#424,.T.) ;
#9173 = EDGE_CURVE('',#7124,#7125,#4408,.T.) ;
#9174 = EDGE_CURVE('',#7125,#7126,#425,.T.) ;
#9175 = EDGE_CURVE('',#7127,#7126,#426,.T.) ;
#9176 = EDGE_CURVE('',#7127,#7128,#4409,.T.) ;
#9177 = EDGE_CURVE('',#7129,#7128,#427,.T.) ;
#9178 = EDGE_CURVE('',#7129,#7130,#428,.T.) ;
#9179 = EDGE_CURVE('',#7130,#7131,#4410,.T.) ;
#9180 = EDGE_CURVE('',#7131,#7132,#429,.T.) ;
#9181 = EDGE_CURVE('',#7133,#7132,#430,.T.) ;
#9182 = EDGE_CURVE('',#7133,#7134,#4411,.T.) ;
#9183 = EDGE_CURVE('',#7135,#7134,#431,.T.) ;
#9184 = EDGE_CURVE('',#7135,#7136,#432,.T.) ;
#9185 = EDGE_CURVE('',#7136,#7137,#4412,.T.) ;
#9186 = EDGE_CURVE('',#7137,#7138,#433,.T.) ;
#9187 = EDGE_CURVE('',#7139,#7138,#434,.T.) ;
#9188 = EDGE_CURVE('',#7139,#7140,#4413,.T.) ;
#9189 = EDGE_CURVE('',#7141,#7140,#435,.T.) ;
#9190 = EDGE_CURVE('',#7141,#7142,#436,.T.) ;
#9191 = EDGE_CURVE('',#7142,#7143,#4414,.T.) ;
#9192 = EDGE_CURVE('',#7143,#7144,#437,.T.) ;
#9193 = EDGE_CURVE('',#7145,#7144,#438,.T.) ;
#9194 = EDGE_CURVE('',#7145,#7146,#4415,.T.) ;
#9195 = EDGE_CURVE('',#7147,#7146,#439,.T.) ;
#9196 = EDGE_CURVE('',#7147,#7148,#440,.T.) ;
#9197 = EDGE_CURVE('',#7148,#7149,#4416,.T.) ;
#9198 = EDGE_CURVE('',#7149,#7150,#441,.T.) ;
#9199 = EDGE_CURVE('',#7151,#7150,#442,.T.) ;
#9200 = EDGE_CURVE('',#7151,#7152,#4417,.T.) ;
#9201 = EDGE_CURVE('',#7153,#7152,#443,.T.) ;
#9202 = EDGE_CURVE('',#7153,#7154,#444,.T.) ;
#9203 = EDGE_CURVE('',#7154,#7155,#4418,.T.) ;
#9204 = EDGE_CURVE('',#7155,#7156,#445,.T.) ;
#9205 = EDGE_CURVE('',#7157,#7156,#446,.T.) ;
#9206 = EDGE_CURVE('',#7157,#7158,#4419,.T.) ;
#9207 = EDGE_CURVE('',#7159,#7158,#447,.T.) ;
#9208 = EDGE_CURVE('',#7159,#7160,#448,.T.) ;
#9209 = EDGE_CURVE('',#7160,#6986,#4420,.T.) ;
#9210 = EDGE_CURVE('',#6985,#7161,#5255,.T.) ;
#9211 = EDGE_CURVE('',#7162,#7161,#4421,.T.) ;
#9212 = EDGE_CURVE('',#7163,#7162,#449,.T.) ;
#9213 = EDGE_CURVE('',#7164,#7163,#99,.T.) ;
#9214 = EDGE_CURVE('',#7162,#7164,#450,.T.) ;
#9215 = EDGE_CURVE('',#7165,#7162,#4422,.T.) ;
#9216 = EDGE_CURVE('',#7166,#7165,#451,.T.) ;
#9217 = EDGE_CURVE('',#7167,#7166,#100,.T.) ;
#9218 = EDGE_CURVE('',#7165,#7167,#452,.T.) ;
#9219 = EDGE_CURVE('',#7168,#7165,#4423,.T.) ;
#9220 = EDGE_CURVE('',#7169,#7168,#453,.T.) ;
#9221 = EDGE_CURVE('',#7170,#7169,#101,.T.) ;
#9222 = EDGE_CURVE('',#7168,#7170,#454,.T.) ;
#9223 = EDGE_CURVE('',#7171,#7168,#4424,.T.) ;
#9224 = EDGE_CURVE('',#7172,#7171,#455,.T.) ;
#9225 = EDGE_CURVE('',#7173,#7172,#102,.T.) ;
#9226 = EDGE_CURVE('',#7171,#7173,#456,.T.) ;
#9227 = EDGE_CURVE('',#7174,#7171,#4425,.T.) ;
#9228 = EDGE_CURVE('',#7175,#7174,#457,.T.) ;
#9229 = EDGE_CURVE('',#7176,#7175,#103,.T.) ;
#9230 = EDGE_CURVE('',#7174,#7176,#458,.T.) ;
#9231 = EDGE_CURVE('',#7177,#7174,#4426,.T.) ;
#9232 = EDGE_CURVE('',#7178,#7177,#459,.T.) ;
#9233 = EDGE_CURVE('',#7179,#7178,#104,.T.) ;
#9234 = EDGE_CURVE('',#7177,#7179,#460,.T.) ;
#9235 = EDGE_CURVE('',#7180,#7177,#4427,.T.) ;
#9236 = EDGE_CURVE('',#7181,#7180,#461,.T.) ;
#9237 = EDGE_CURVE('',#7182,#7181,#105,.T.) ;
#9238 = EDGE_CURVE('',#7180,#7182,#462,.T.) ;
#9239 = EDGE_CURVE('',#7183,#7180,#4428,.T.) ;
#9240 = EDGE_CURVE('',#7184,#7183,#463,.T.) ;
#9241 = EDGE_CURVE('',#7185,#7184,#106,.T.) ;
#9242 = EDGE_CURVE('',#7183,#7185,#464,.T.) ;
#9243 = EDGE_CURVE('',#7186,#7183,#4429,.T.) ;
#9244 = EDGE_CURVE('',#7187,#7186,#4430,.T.) ;
#9245 = EDGE_CURVE('',#7188,#7187,#465,.T.) ;
#9246 = EDGE_CURVE('',#7189,#7188,#107,.T.) ;
#9247 = EDGE_CURVE('',#7187,#7189,#466,.T.) ;
#9248 = EDGE_CURVE('',#7190,#7187,#4431,.T.) ;
#9249 = EDGE_CURVE('',#7191,#7190,#467,.T.) ;
#9250 = EDGE_CURVE('',#7192,#7191,#108,.T.) ;
#9251 = EDGE_CURVE('',#7190,#7192,#468,.T.) ;
#9252 = EDGE_CURVE('',#7193,#7190,#4432,.T.) ;
#9253 = EDGE_CURVE('',#7194,#7193,#469,.T.) ;
#9254 = EDGE_CURVE('',#7195,#7194,#109,.T.) ;
#9255 = EDGE_CURVE('',#7193,#7195,#470,.T.) ;
#9256 = EDGE_CURVE('',#7196,#7193,#4433,.T.) ;
#9257 = EDGE_CURVE('',#7197,#7196,#471,.T.) ;
#9258 = EDGE_CURVE('',#7198,#7197,#110,.T.) ;
#9259 = EDGE_CURVE('',#7196,#7198,#472,.T.) ;
#9260 = EDGE_CURVE('',#7199,#7196,#4434,.T.) ;
#9261 = EDGE_CURVE('',#7200,#7199,#4435,.T.) ;
#9262 = EDGE_CURVE('',#7201,#7200,#473,.T.) ;
#9263 = EDGE_CURVE('',#7202,#7201,#111,.T.) ;
#9264 = EDGE_CURVE('',#7200,#7202,#474,.T.) ;
#9265 = EDGE_CURVE('',#7203,#7200,#4436,.T.) ;
#9266 = EDGE_CURVE('',#7204,#7203,#475,.T.) ;
#9267 = EDGE_CURVE('',#7205,#7204,#112,.T.) ;
#9268 = EDGE_CURVE('',#7203,#7205,#476,.T.) ;
#9269 = EDGE_CURVE('',#7206,#7203,#4437,.T.) ;
#9270 = EDGE_CURVE('',#7207,#7206,#477,.T.) ;
#9271 = EDGE_CURVE('',#7208,#7207,#113,.T.) ;
#9272 = EDGE_CURVE('',#7206,#7208,#478,.T.) ;
#9273 = EDGE_CURVE('',#7209,#7206,#4438,.T.) ;
#9274 = EDGE_CURVE('',#7210,#7209,#479,.T.) ;
#9275 = EDGE_CURVE('',#7211,#7210,#114,.T.) ;
#9276 = EDGE_CURVE('',#7209,#7211,#480,.T.) ;
#9277 = EDGE_CURVE('',#7212,#7209,#4439,.T.) ;
#9278 = EDGE_CURVE('',#7213,#7212,#481,.T.) ;
#9279 = EDGE_CURVE('',#7214,#7213,#115,.T.) ;
#9280 = EDGE_CURVE('',#7212,#7214,#482,.T.) ;
#9281 = EDGE_CURVE('',#7215,#7212,#4440,.T.) ;
#9282 = EDGE_CURVE('',#7216,#7215,#483,.T.) ;
#9283 = EDGE_CURVE('',#7217,#7216,#116,.T.) ;
#9284 = EDGE_CURVE('',#7215,#7217,#484,.T.) ;
#9285 = EDGE_CURVE('',#7218,#7215,#4441,.T.) ;
#9286 = EDGE_CURVE('',#7219,#7218,#485,.T.) ;
#9287 = EDGE_CURVE('',#7220,#7219,#117,.T.) ;
#9288 = EDGE_CURVE('',#7218,#7220,#486,.T.) ;
#9289 = EDGE_CURVE('',#7221,#7218,#4442,.T.) ;
#9290 = EDGE_CURVE('',#7222,#7221,#487,.T.) ;
#9291 = EDGE_CURVE('',#7223,#7222,#118,.T.) ;
#9292 = EDGE_CURVE('',#7221,#7223,#488,.T.) ;
#9293 = EDGE_CURVE('',#7224,#7221,#4443,.T.) ;
#9294 = EDGE_CURVE('',#7225,#7224,#489,.T.) ;
#9295 = EDGE_CURVE('',#7226,#7225,#119,.T.) ;
#9296 = EDGE_CURVE('',#7224,#7226,#490,.T.) ;
#9297 = EDGE_CURVE('',#7227,#7224,#4444,.T.) ;
#9298 = EDGE_CURVE('',#7228,#7227,#491,.T.) ;
#9299 = EDGE_CURVE('',#7229,#7228,#120,.T.) ;
#9300 = EDGE_CURVE('',#7227,#7229,#492,.T.) ;
#9301 = EDGE_CURVE('',#7230,#7227,#4445,.T.) ;
#9302 = EDGE_CURVE('',#7231,#7230,#493,.T.) ;
#9303 = EDGE_CURVE('',#7232,#7231,#121,.T.) ;
#9304 = EDGE_CURVE('',#7230,#7232,#494,.T.) ;
#9305 = EDGE_CURVE('',#7233,#7230,#4446,.T.) ;
#9306 = EDGE_CURVE('',#7234,#7233,#495,.T.) ;
#9307 = EDGE_CURVE('',#7235,#7234,#122,.T.) ;
#9308 = EDGE_CURVE('',#7233,#7235,#496,.T.) ;
#9309 = EDGE_CURVE('',#7236,#7233,#4447,.T.) ;
#9310 = EDGE_CURVE('',#7237,#7236,#497,.T.) ;
#9311 = EDGE_CURVE('',#7238,#7237,#123,.T.) ;
#9312 = EDGE_CURVE('',#7236,#7238,#498,.T.) ;
#9313 = EDGE_CURVE('',#7239,#7236,#4448,.T.) ;
#9314 = EDGE_CURVE('',#7240,#7239,#499,.T.) ;
#9315 = EDGE_CURVE('',#7241,#7240,#124,.T.) ;
#9316 = EDGE_CURVE('',#7239,#7241,#500,.T.) ;
#9317 = EDGE_CURVE('',#7242,#7239,#4449,.T.) ;
#9318 = EDGE_CURVE('',#7243,#7242,#501,.T.) ;
#9319 = EDGE_CURVE('',#7244,#7243,#125,.T.) ;
#9320 = EDGE_CURVE('',#7242,#7244,#502,.T.) ;
#9321 = EDGE_CURVE('',#7161,#7242,#4450,.T.) ;
#9322 = EDGE_CURVE('',#7245,#7186,#503,.T.) ;
#9323 = EDGE_CURVE('',#7246,#7245,#126,.T.) ;
#9324 = EDGE_CURVE('',#7186,#7246,#504,.T.) ;
#9325 = EDGE_CURVE('',#7247,#7199,#505,.T.) ;
#9326 = EDGE_CURVE('',#7248,#7247,#127,.T.) ;
#9327 = EDGE_CURVE('',#7199,#7248,#506,.T.) ;
#9328 = EDGE_CURVE('',#7160,#7249,#5256,.T.) ;
#9329 = EDGE_CURVE('',#7158,#7249,#128,.T.) ;
#9330 = EDGE_CURVE('',#7250,#7157,#129,.T.) ;
#9331 = EDGE_CURVE('',#7250,#7155,#5257,.T.) ;
#9332 = EDGE_CURVE('',#7154,#7251,#5258,.T.) ;
#9333 = EDGE_CURVE('',#7152,#7251,#130,.T.) ;
#9334 = EDGE_CURVE('',#7252,#7151,#131,.T.) ;
#9335 = EDGE_CURVE('',#7252,#7149,#5259,.T.) ;
#9336 = EDGE_CURVE('',#7148,#7253,#5260,.T.) ;
#9337 = EDGE_CURVE('',#7146,#7253,#132,.T.) ;
#9338 = EDGE_CURVE('',#7254,#7145,#133,.T.) ;
#9339 = EDGE_CURVE('',#7254,#7143,#5261,.T.) ;
#9340 = EDGE_CURVE('',#7142,#7255,#5262,.T.) ;
#9341 = EDGE_CURVE('',#7140,#7255,#134,.T.) ;
#9342 = EDGE_CURVE('',#7256,#7139,#135,.T.) ;
#9343 = EDGE_CURVE('',#7256,#7137,#5263,.T.) ;
#9344 = EDGE_CURVE('',#7136,#7257,#5264,.T.) ;
#9345 = EDGE_CURVE('',#7134,#7257,#136,.T.) ;
#9346 = EDGE_CURVE('',#7258,#7133,#137,.T.) ;
#9347 = EDGE_CURVE('',#7258,#7131,#5265,.T.) ;
#9348 = EDGE_CURVE('',#7130,#7259,#5266,.T.) ;
#9349 = EDGE_CURVE('',#7128,#7259,#138,.T.) ;
#9350 = EDGE_CURVE('',#7260,#7127,#139,.T.) ;
#9351 = EDGE_CURVE('',#7260,#7125,#5267,.T.) ;
#9352 = EDGE_CURVE('',#7124,#7261,#5268,.T.) ;
#9353 = EDGE_CURVE('',#7122,#7261,#140,.T.) ;
#9354 = EDGE_CURVE('',#7262,#7121,#141,.T.) ;
#9355 = EDGE_CURVE('',#7262,#7119,#5269,.T.) ;
#9356 = EDGE_CURVE('',#7118,#7263,#5270,.T.) ;
#9357 = EDGE_CURVE('',#7116,#7263,#142,.T.) ;
#9358 = EDGE_CURVE('',#7264,#7115,#143,.T.) ;
#9359 = EDGE_CURVE('',#7264,#7113,#5271,.T.) ;
#9360 = EDGE_CURVE('',#7112,#7265,#5272,.T.) ;
#9361 = EDGE_CURVE('',#7110,#7265,#144,.T.) ;
#9362 = EDGE_CURVE('',#7266,#7109,#145,.T.) ;
#9363 = EDGE_CURVE('',#7266,#7107,#5273,.T.) ;
#9364 = EDGE_CURVE('',#7106,#7267,#5274,.T.) ;
#9365 = EDGE_CURVE('',#7104,#7267,#146,.T.) ;
#9366 = EDGE_CURVE('',#7268,#7103,#147,.T.) ;
#9367 = EDGE_CURVE('',#7268,#7101,#5275,.T.) ;
#9368 = EDGE_CURVE('',#7100,#7269,#5276,.T.) ;
#9369 = EDGE_CURVE('',#7098,#7269,#148,.T.) ;
#9370 = EDGE_CURVE('',#7270,#7097,#149,.T.) ;
#9371 = EDGE_CURVE('',#7270,#7095,#5277,.T.) ;
#9372 = EDGE_CURVE('',#7094,#7271,#5278,.T.) ;
#9373 = EDGE_CURVE('',#7092,#7271,#150,.T.) ;
#9374 = EDGE_CURVE('',#7272,#7091,#151,.T.) ;
#9375 = EDGE_CURVE('',#7272,#7089,#5279,.T.) ;
#9376 = EDGE_CURVE('',#7088,#7273,#5280,.T.) ;
#9377 = EDGE_CURVE('',#7086,#7273,#152,.T.) ;
#9378 = EDGE_CURVE('',#7274,#7085,#153,.T.) ;
#9379 = EDGE_CURVE('',#7274,#7083,#5281,.T.) ;
#9380 = EDGE_CURVE('',#7082,#7275,#5282,.T.) ;
#9381 = EDGE_CURVE('',#7080,#7275,#154,.T.) ;
#9382 = EDGE_CURVE('',#7276,#7079,#155,.T.) ;
#9383 = EDGE_CURVE('',#7276,#7077,#5283,.T.) ;
#9384 = EDGE_CURVE('',#7076,#7277,#5284,.T.) ;
#9385 = EDGE_CURVE('',#7074,#7277,#156,.T.) ;
#9386 = EDGE_CURVE('',#7278,#7073,#157,.T.) ;
#9387 = EDGE_CURVE('',#7278,#7071,#5285,.T.) ;
#9388 = EDGE_CURVE('',#7070,#7279,#5286,.T.) ;
#9389 = EDGE_CURVE('',#7068,#7279,#158,.T.) ;
#9390 = EDGE_CURVE('',#7280,#7067,#159,.T.) ;
#9391 = EDGE_CURVE('',#7280,#7065,#5287,.T.) ;
#9392 = EDGE_CURVE('',#7064,#7281,#5288,.T.) ;
#9393 = EDGE_CURVE('',#7062,#7281,#160,.T.) ;
#9394 = EDGE_CURVE('',#7282,#7061,#161,.T.) ;
#9395 = EDGE_CURVE('',#7282,#7059,#5289,.T.) ;
#9396 = EDGE_CURVE('',#7058,#7283,#5290,.T.) ;
#9397 = EDGE_CURVE('',#7056,#7283,#162,.T.) ;
#9398 = EDGE_CURVE('',#7284,#7055,#163,.T.) ;
#9399 = EDGE_CURVE('',#7284,#7053,#5291,.T.) ;
#9400 = EDGE_CURVE('',#7052,#7285,#5292,.T.) ;
#9401 = EDGE_CURVE('',#7050,#7285,#164,.T.) ;
#9402 = EDGE_CURVE('',#7286,#7049,#165,.T.) ;
#9403 = EDGE_CURVE('',#7286,#7047,#5293,.T.) ;
#9404 = EDGE_CURVE('',#7046,#7287,#5294,.T.) ;
#9405 = EDGE_CURVE('',#7044,#7287,#166,.T.) ;
#9406 = EDGE_CURVE('',#7288,#7043,#167,.T.) ;
#9407 = EDGE_CURVE('',#7288,#7041,#5295,.T.) ;
#9408 = EDGE_CURVE('',#7040,#7289,#5296,.T.) ;
#9409 = EDGE_CURVE('',#7038,#7289,#168,.T.) ;
#9410 = EDGE_CURVE('',#7290,#7037,#169,.T.) ;
#9411 = EDGE_CURVE('',#7290,#7035,#5297,.T.) ;
#9412 = EDGE_CURVE('',#7034,#7291,#5298,.T.) ;
#9413 = EDGE_CURVE('',#7032,#7291,#170,.T.) ;
#9414 = EDGE_CURVE('',#7292,#7031,#171,.T.) ;
#9415 = EDGE_CURVE('',#7292,#7029,#5299,.T.) ;
#9416 = EDGE_CURVE('',#7028,#7293,#5300,.T.) ;
#9417 = EDGE_CURVE('',#7026,#7293,#172,.T.) ;
#9418 = EDGE_CURVE('',#7294,#7025,#173,.T.) ;
#9419 = EDGE_CURVE('',#7294,#7023,#5301,.T.) ;
#9420 = EDGE_CURVE('',#7022,#7295,#5302,.T.) ;
#9421 = EDGE_CURVE('',#7020,#7295,#174,.T.) ;
#9422 = EDGE_CURVE('',#7296,#7019,#175,.T.) ;
#9423 = EDGE_CURVE('',#7296,#7017,#5303,.T.) ;
#9424 = EDGE_CURVE('',#7016,#7297,#5304,.T.) ;
#9425 = EDGE_CURVE('',#7014,#7297,#176,.T.) ;
#9426 = EDGE_CURVE('',#7298,#7013,#177,.T.) ;
#9427 = EDGE_CURVE('',#7298,#7011,#5305,.T.) ;
#9428 = EDGE_CURVE('',#7010,#7299,#5306,.T.) ;
#9429 = EDGE_CURVE('',#7008,#7299,#178,.T.) ;
#9430 = EDGE_CURVE('',#7300,#7007,#179,.T.) ;
#9431 = EDGE_CURVE('',#7300,#7005,#5307,.T.) ;
#9432 = EDGE_CURVE('',#7004,#7301,#5308,.T.) ;
#9433 = EDGE_CURVE('',#7002,#7301,#180,.T.) ;
#9434 = EDGE_CURVE('',#7302,#7001,#181,.T.) ;
#9435 = EDGE_CURVE('',#7302,#6999,#5309,.T.) ;
#9436 = EDGE_CURVE('',#6998,#7303,#5310,.T.) ;
#9437 = EDGE_CURVE('',#6996,#7303,#182,.T.) ;
#9438 = EDGE_CURVE('',#7304,#6995,#183,.T.) ;
#9439 = EDGE_CURVE('',#7304,#6993,#5311,.T.) ;
#9440 = EDGE_CURVE('',#6992,#7305,#5312,.T.) ;
#9441 = EDGE_CURVE('',#6990,#7305,#184,.T.) ;
#9442 = EDGE_CURVE('',#7306,#6989,#185,.T.) ;
#9443 = EDGE_CURVE('',#7306,#6987,#5313,.T.) ;
#9444 = EDGE_CURVE('',#6986,#7307,#5314,.T.) ;
#9445 = EDGE_CURVE('',#7307,#7307,#4451,.T.) ;
#9446 = EDGE_CURVE('',#7308,#7308,#4452,.T.) ;
#9447 = EDGE_CURVE('',#7308,#7309,#5315,.T.) ;
#9448 = EDGE_CURVE('',#7309,#7309,#4453,.T.) ;
#9449 = EDGE_CURVE('',#7310,#7311,#507,.T.) ;
#9450 = EDGE_CURVE('',#7312,#7310,#186,.T.) ;
#9451 = EDGE_CURVE('',#7311,#7312,#508,.T.) ;
#9452 = EDGE_CURVE('',#7313,#7314,#187,.T.) ;
#9453 = EDGE_CURVE('',#7315,#7313,#509,.T.) ;
#9454 = EDGE_CURVE('',#7314,#7315,#510,.T.) ;
#9455 = EDGE_CURVE('',#7316,#7317,#188,.T.) ;
#9456 = EDGE_CURVE('',#7318,#7316,#511,.T.) ;
#9457 = EDGE_CURVE('',#7317,#7318,#512,.T.) ;
#9458 = EDGE_CURVE('',#7319,#7320,#189,.T.) ;
#9459 = EDGE_CURVE('',#7321,#7319,#513,.T.) ;
#9460 = EDGE_CURVE('',#7320,#7321,#514,.T.) ;
#9461 = EDGE_CURVE('',#7322,#7323,#190,.T.) ;
#9462 = EDGE_CURVE('',#7324,#7322,#515,.T.) ;
#9463 = EDGE_CURVE('',#7323,#7324,#516,.T.) ;
#9464 = EDGE_CURVE('',#7325,#7326,#191,.T.) ;
#9465 = EDGE_CURVE('',#7327,#7325,#517,.T.) ;
#9466 = EDGE_CURVE('',#7326,#7327,#518,.T.) ;
#9467 = EDGE_CURVE('',#7328,#7329,#192,.T.) ;
#9468 = EDGE_CURVE('',#7330,#7328,#519,.T.) ;
#9469 = EDGE_CURVE('',#7329,#7330,#520,.T.) ;
#9470 = EDGE_CURVE('',#7331,#7332,#193,.T.) ;
#9471 = EDGE_CURVE('',#7333,#7331,#521,.T.) ;
#9472 = EDGE_CURVE('',#7332,#7333,#522,.T.) ;
#9473 = EDGE_CURVE('',#7334,#7335,#194,.T.) ;
#9474 = EDGE_CURVE('',#7336,#7334,#523,.T.) ;
#9475 = EDGE_CURVE('',#7335,#7336,#524,.T.) ;
#9476 = EDGE_CURVE('',#7337,#7338,#195,.T.) ;
#9477 = EDGE_CURVE('',#7339,#7337,#525,.T.) ;
#9478 = EDGE_CURVE('',#7338,#7339,#526,.T.) ;
#9479 = EDGE_CURVE('',#7340,#7341,#196,.T.) ;
#9480 = EDGE_CURVE('',#7342,#7340,#527,.T.) ;
#9481 = EDGE_CURVE('',#7341,#7342,#528,.T.) ;
#9482 = EDGE_CURVE('',#7343,#7344,#197,.T.) ;
#9483 = EDGE_CURVE('',#7345,#7343,#529,.T.) ;
#9484 = EDGE_CURVE('',#7344,#7345,#530,.T.) ;
#9485 = EDGE_CURVE('',#7346,#7347,#198,.T.) ;
#9486 = EDGE_CURVE('',#7348,#7346,#531,.T.) ;
#9487 = EDGE_CURVE('',#7347,#7348,#532,.T.) ;
#9488 = EDGE_CURVE('',#7349,#7350,#199,.T.) ;
#9489 = EDGE_CURVE('',#7351,#7349,#533,.T.) ;
#9490 = EDGE_CURVE('',#7350,#7351,#534,.T.) ;
#9491 = EDGE_CURVE('',#7352,#7353,#200,.T.) ;
#9492 = EDGE_CURVE('',#7354,#7352,#535,.T.) ;
#9493 = EDGE_CURVE('',#7353,#7354,#536,.T.) ;
#9494 = EDGE_CURVE('',#7355,#7356,#201,.T.) ;
#9495 = EDGE_CURVE('',#7357,#7355,#537,.T.) ;
#9496 = EDGE_CURVE('',#7356,#7357,#538,.T.) ;
#9497 = EDGE_CURVE('',#7358,#7359,#202,.T.) ;
#9498 = EDGE_CURVE('',#7360,#7358,#539,.T.) ;
#9499 = EDGE_CURVE('',#7359,#7360,#540,.T.) ;
#9500 = EDGE_CURVE('',#7361,#7362,#203,.T.) ;
#9501 = EDGE_CURVE('',#7363,#7361,#541,.T.) ;
#9502 = EDGE_CURVE('',#7362,#7363,#542,.T.) ;
#9503 = EDGE_CURVE('',#7364,#7365,#204,.T.) ;
#9504 = EDGE_CURVE('',#7366,#7364,#543,.T.) ;
#9505 = EDGE_CURVE('',#7365,#7366,#544,.T.) ;
#9506 = EDGE_CURVE('',#7367,#7368,#205,.T.) ;
#9507 = EDGE_CURVE('',#7369,#7367,#545,.T.) ;
#9508 = EDGE_CURVE('',#7368,#7369,#546,.T.) ;
#9509 = EDGE_CURVE('',#7370,#7371,#206,.T.) ;
#9510 = EDGE_CURVE('',#7372,#7370,#547,.T.) ;
#9511 = EDGE_CURVE('',#7371,#7372,#548,.T.) ;
#9512 = EDGE_CURVE('',#7373,#7374,#207,.T.) ;
#9513 = EDGE_CURVE('',#7375,#7373,#549,.T.) ;
#9514 = EDGE_CURVE('',#7374,#7375,#550,.T.) ;
#9515 = EDGE_CURVE('',#7376,#7377,#208,.T.) ;
#9516 = EDGE_CURVE('',#7378,#7376,#551,.T.) ;
#9517 = EDGE_CURVE('',#7377,#7378,#552,.T.) ;
#9518 = EDGE_CURVE('',#7379,#7380,#209,.T.) ;
#9519 = EDGE_CURVE('',#7381,#7379,#553,.T.) ;
#9520 = EDGE_CURVE('',#7380,#7381,#554,.T.) ;
#9521 = EDGE_CURVE('',#7382,#7383,#210,.T.) ;
#9522 = EDGE_CURVE('',#7384,#7382,#555,.T.) ;
#9523 = EDGE_CURVE('',#7383,#7384,#556,.T.) ;
#9524 = EDGE_CURVE('',#7385,#7386,#211,.T.) ;
#9525 = EDGE_CURVE('',#7387,#7385,#557,.T.) ;
#9526 = EDGE_CURVE('',#7386,#7387,#558,.T.) ;
#9527 = EDGE_CURVE('',#7388,#7389,#212,.T.) ;
#9528 = EDGE_CURVE('',#7390,#7388,#559,.T.) ;
#9529 = EDGE_CURVE('',#7389,#7390,#560,.T.) ;
#9530 = EDGE_CURVE('',#7391,#7392,#213,.T.) ;
#9531 = EDGE_CURVE('',#7393,#7391,#561,.T.) ;
#9532 = EDGE_CURVE('',#7392,#7393,#562,.T.) ;
#9533 = EDGE_CURVE('',#7394,#7395,#214,.T.) ;
#9534 = EDGE_CURVE('',#7396,#7394,#563,.T.) ;
#9535 = EDGE_CURVE('',#7395,#7396,#564,.T.) ;
#9536 = EDGE_CURVE('',#7397,#7397,#4454,.T.) ;
#9537 = EDGE_CURVE('',#7397,#7398,#5316,.T.) ;
#9538 = EDGE_CURVE('',#7398,#7398,#4455,.T.) ;
#9539 = EDGE_CURVE('',#7399,#7399,#4456,.T.) ;
#9540 = EDGE_CURVE('',#7399,#7400,#4457,.T.) ;
#9541 = EDGE_CURVE('',#7400,#7400,#4458,.T.) ;
#9542 = EDGE_CURVE('',#7401,#7401,#4459,.T.) ;
#9543 = EDGE_CURVE('',#7401,#7402,#4460,.T.) ;
#9544 = EDGE_CURVE('',#7402,#7402,#4461,.T.) ;
#9545 = EDGE_CURVE('',#7403,#7403,#4462,.T.) ;
#9546 = EDGE_CURVE('',#7403,#7404,#4463,.T.) ;
#9547 = EDGE_CURVE('',#7404,#7404,#4464,.T.) ;
#9548 = EDGE_CURVE('',#7400,#7405,#5317,.T.) ;
#9549 = EDGE_CURVE('',#7405,#7405,#4465,.T.) ;
#9550 = EDGE_CURVE('',#7405,#7406,#4466,.T.) ;
#9551 = EDGE_CURVE('',#7406,#7406,#4467,.T.) ;
#9552 = EDGE_CURVE('',#7402,#7403,#5318,.T.) ;
#9553 = EDGE_CURVE('',#7311,#7200,#4468,.T.) ;
#9554 = EDGE_CURVE('',#7200,#7311,#4469,.T.) ;
#9555 = EDGE_CURVE('',#7396,#7203,#4470,.T.) ;
#9556 = EDGE_CURVE('',#7203,#7396,#4471,.T.) ;
#9557 = EDGE_CURVE('',#7357,#7206,#4472,.T.) ;
#9558 = EDGE_CURVE('',#7206,#7357,#4473,.T.) ;
#9559 = EDGE_CURVE('',#7393,#7209,#4474,.T.) ;
#9560 = EDGE_CURVE('',#7209,#7393,#4475,.T.) ;
#9561 = EDGE_CURVE('',#7360,#7212,#4476,.T.) ;
#9562 = EDGE_CURVE('',#7212,#7360,#4477,.T.) ;
#9563 = EDGE_CURVE('',#7390,#7215,#4478,.T.) ;
#9564 = EDGE_CURVE('',#7215,#7390,#4479,.T.) ;
#9565 = EDGE_CURVE('',#7363,#7218,#4480,.T.) ;
#9566 = EDGE_CURVE('',#7218,#7363,#4481,.T.) ;
#9567 = EDGE_CURVE('',#7387,#7221,#4482,.T.) ;
#9568 = EDGE_CURVE('',#7221,#7387,#4483,.T.) ;
#9569 = EDGE_CURVE('',#7366,#7224,#4484,.T.) ;
#9570 = EDGE_CURVE('',#7224,#7366,#4485,.T.) ;
#9571 = EDGE_CURVE('',#7384,#7227,#4486,.T.) ;
#9572 = EDGE_CURVE('',#7227,#7384,#4487,.T.) ;
#9573 = EDGE_CURVE('',#7369,#7230,#4488,.T.) ;
#9574 = EDGE_CURVE('',#7230,#7369,#4489,.T.) ;
#9575 = EDGE_CURVE('',#7381,#7233,#4490,.T.) ;
#9576 = EDGE_CURVE('',#7233,#7381,#4491,.T.) ;
#9577 = EDGE_CURVE('',#7372,#7236,#4492,.T.) ;
#9578 = EDGE_CURVE('',#7236,#7372,#4493,.T.) ;
#9579 = EDGE_CURVE('',#7378,#7239,#4494,.T.) ;
#9580 = EDGE_CURVE('',#7239,#7378,#4495,.T.) ;
#9581 = EDGE_CURVE('',#7375,#7242,#4496,.T.) ;
#9582 = EDGE_CURVE('',#7242,#7375,#4497,.T.) ;
#9583 = EDGE_CURVE('',#7333,#7162,#4498,.T.) ;
#9584 = EDGE_CURVE('',#7162,#7333,#4499,.T.) ;
#9585 = EDGE_CURVE('',#7336,#7165,#4500,.T.) ;
#9586 = EDGE_CURVE('',#7165,#7336,#4501,.T.) ;
#9587 = EDGE_CURVE('',#7330,#7168,#4502,.T.) ;
#9588 = EDGE_CURVE('',#7168,#7330,#4503,.T.) ;
#9589 = EDGE_CURVE('',#7339,#7171,#4504,.T.) ;
#9590 = EDGE_CURVE('',#7171,#7339,#4505,.T.) ;
#9591 = EDGE_CURVE('',#7327,#7174,#4506,.T.) ;
#9592 = EDGE_CURVE('',#7174,#7327,#4507,.T.) ;
#9593 = EDGE_CURVE('',#7342,#7177,#4508,.T.) ;
#9594 = EDGE_CURVE('',#7177,#7342,#4509,.T.) ;
#9595 = EDGE_CURVE('',#7324,#7180,#4510,.T.) ;
#9596 = EDGE_CURVE('',#7180,#7324,#4511,.T.) ;
#9597 = EDGE_CURVE('',#7345,#7183,#4512,.T.) ;
#9598 = EDGE_CURVE('',#7183,#7345,#4513,.T.) ;
#9599 = EDGE_CURVE('',#7321,#7186,#4514,.T.) ;
#9600 = EDGE_CURVE('',#7186,#7321,#4515,.T.) ;
#9601 = EDGE_CURVE('',#7348,#7187,#4516,.T.) ;
#9602 = EDGE_CURVE('',#7187,#7348,#4517,.T.) ;
#9603 = EDGE_CURVE('',#7318,#7190,#4518,.T.) ;
#9604 = EDGE_CURVE('',#7190,#7318,#4519,.T.) ;
#9605 = EDGE_CURVE('',#7351,#7193,#4520,.T.) ;
#9606 = EDGE_CURVE('',#7193,#7351,#4521,.T.) ;
#9607 = EDGE_CURVE('',#7315,#7196,#4522,.T.) ;
#9608 = EDGE_CURVE('',#7196,#7315,#4523,.T.) ;
#9609 = EDGE_CURVE('',#7354,#7199,#4524,.T.) ;
#9610 = EDGE_CURVE('',#7199,#7354,#4525,.T.) ;
#9611 = EDGE_CURVE('',#7398,#7161,#5319,.T.) ;
#9612 = EDGE_CURVE('',#7075,#7201,#4526,.T.) ;
#9613 = EDGE_CURVE('',#7312,#7277,#4527,.T.) ;
#9614 = EDGE_CURVE('',#7202,#7072,#4528,.T.) ;
#9615 = EDGE_CURVE('',#7278,#7310,#4529,.T.) ;
#9616 = EDGE_CURVE('',#7069,#7204,#4530,.T.) ;
#9617 = EDGE_CURVE('',#7394,#7279,#4531,.T.) ;
#9618 = EDGE_CURVE('',#7205,#7066,#4532,.T.) ;
#9619 = EDGE_CURVE('',#7280,#7395,#4533,.T.) ;
#9620 = EDGE_CURVE('',#7063,#7207,#4534,.T.) ;
#9621 = EDGE_CURVE('',#7355,#7281,#4535,.T.) ;
#9622 = EDGE_CURVE('',#7208,#7060,#4536,.T.) ;
#9623 = EDGE_CURVE('',#7282,#7356,#4537,.T.) ;
#9624 = EDGE_CURVE('',#7057,#7210,#4538,.T.) ;
#9625 = EDGE_CURVE('',#7391,#7283,#4539,.T.) ;
#9626 = EDGE_CURVE('',#7211,#7054,#4540,.T.) ;
#9627 = EDGE_CURVE('',#7284,#7392,#4541,.T.) ;
#9628 = EDGE_CURVE('',#7051,#7213,#4542,.T.) ;
#9629 = EDGE_CURVE('',#7358,#7285,#4543,.T.) ;
#9630 = EDGE_CURVE('',#7214,#7048,#4544,.T.) ;
#9631 = EDGE_CURVE('',#7286,#7359,#4545,.T.) ;
#9632 = EDGE_CURVE('',#7045,#7216,#4546,.T.) ;
#9633 = EDGE_CURVE('',#7388,#7287,#4547,.T.) ;
#9634 = EDGE_CURVE('',#7217,#7042,#4548,.T.) ;
#9635 = EDGE_CURVE('',#7288,#7389,#4549,.T.) ;
#9636 = EDGE_CURVE('',#7039,#7219,#4550,.T.) ;
#9637 = EDGE_CURVE('',#7361,#7289,#4551,.T.) ;
#9638 = EDGE_CURVE('',#7220,#7036,#4552,.T.) ;
#9639 = EDGE_CURVE('',#7290,#7362,#4553,.T.) ;
#9640 = EDGE_CURVE('',#7033,#7222,#4554,.T.) ;
#9641 = EDGE_CURVE('',#7385,#7291,#4555,.T.) ;
#9642 = EDGE_CURVE('',#7223,#7030,#4556,.T.) ;
#9643 = EDGE_CURVE('',#7292,#7386,#4557,.T.) ;
#9644 = EDGE_CURVE('',#7027,#7225,#4558,.T.) ;
#9645 = EDGE_CURVE('',#7364,#7293,#4559,.T.) ;
#9646 = EDGE_CURVE('',#7294,#7365,#4560,.T.) ;
#9647 = EDGE_CURVE('',#7226,#7024,#4561,.T.) ;
#9648 = EDGE_CURVE('',#7021,#7228,#4562,.T.) ;
#9649 = EDGE_CURVE('',#7382,#7295,#4563,.T.) ;
#9650 = EDGE_CURVE('',#7296,#7383,#4564,.T.) ;
#9651 = EDGE_CURVE('',#7229,#7018,#4565,.T.) ;
#9652 = EDGE_CURVE('',#7015,#7231,#4566,.T.) ;
#9653 = EDGE_CURVE('',#7367,#7297,#4567,.T.) ;
#9654 = EDGE_CURVE('',#7298,#7368,#4568,.T.) ;
#9655 = EDGE_CURVE('',#7232,#7012,#4569,.T.) ;
#9656 = EDGE_CURVE('',#7009,#7234,#4570,.T.) ;
#9657 = EDGE_CURVE('',#7379,#7299,#4571,.T.) ;
#9658 = EDGE_CURVE('',#7300,#7380,#4572,.T.) ;
#9659 = EDGE_CURVE('',#7235,#7006,#4573,.T.) ;
#9660 = EDGE_CURVE('',#7003,#7237,#4574,.T.) ;
#9661 = EDGE_CURVE('',#7370,#7301,#4575,.T.) ;
#9662 = EDGE_CURVE('',#7302,#7371,#4576,.T.) ;
#9663 = EDGE_CURVE('',#7238,#7000,#4577,.T.) ;
#9664 = EDGE_CURVE('',#6997,#7240,#4578,.T.) ;
#9665 = EDGE_CURVE('',#7376,#7303,#4579,.T.) ;
#9666 = EDGE_CURVE('',#7304,#7377,#4580,.T.) ;
#9667 = EDGE_CURVE('',#7241,#6994,#4581,.T.) ;
#9668 = EDGE_CURVE('',#6991,#7243,#4582,.T.) ;
#9669 = EDGE_CURVE('',#7373,#7305,#4583,.T.) ;
#9670 = EDGE_CURVE('',#7306,#7374,#4584,.T.) ;
#9671 = EDGE_CURVE('',#7244,#6988,#4585,.T.) ;
#9672 = EDGE_CURVE('',#7159,#7163,#4586,.T.) ;
#9673 = EDGE_CURVE('',#7331,#7249,#4587,.T.) ;
#9674 = EDGE_CURVE('',#7250,#7332,#4588,.T.) ;
#9675 = EDGE_CURVE('',#7164,#7156,#4589,.T.) ;
#9676 = EDGE_CURVE('',#7153,#7166,#4590,.T.) ;
#9677 = EDGE_CURVE('',#7334,#7251,#4591,.T.) ;
#9678 = EDGE_CURVE('',#7252,#7335,#4592,.T.) ;
#9679 = EDGE_CURVE('',#7167,#7150,#4593,.T.) ;
#9680 = EDGE_CURVE('',#7147,#7169,#4594,.T.) ;
#9681 = EDGE_CURVE('',#7328,#7253,#4595,.T.) ;
#9682 = EDGE_CURVE('',#7254,#7329,#4596,.T.) ;
#9683 = EDGE_CURVE('',#7170,#7144,#4597,.T.) ;
#9684 = EDGE_CURVE('',#7141,#7172,#4598,.T.) ;
#9685 = EDGE_CURVE('',#7337,#7255,#4599,.T.) ;
#9686 = EDGE_CURVE('',#7256,#7338,#4600,.T.) ;
#9687 = EDGE_CURVE('',#7173,#7138,#4601,.T.) ;
#9688 = EDGE_CURVE('',#7135,#7175,#4602,.T.) ;
#9689 = EDGE_CURVE('',#7325,#7257,#4603,.T.) ;
#9690 = EDGE_CURVE('',#7258,#7326,#4604,.T.) ;
#9691 = EDGE_CURVE('',#7176,#7132,#4605,.T.) ;
#9692 = EDGE_CURVE('',#7129,#7178,#4606,.T.) ;
#9693 = EDGE_CURVE('',#7340,#7259,#4607,.T.) ;
#9694 = EDGE_CURVE('',#7260,#7341,#4608,.T.) ;
#9695 = EDGE_CURVE('',#7179,#7126,#4609,.T.) ;
#9696 = EDGE_CURVE('',#7123,#7181,#4610,.T.) ;
#9697 = EDGE_CURVE('',#7322,#7261,#4611,.T.) ;
#9698 = EDGE_CURVE('',#7262,#7323,#4612,.T.) ;
#9699 = EDGE_CURVE('',#7182,#7120,#4613,.T.) ;
#9700 = EDGE_CURVE('',#7117,#7184,#4614,.T.) ;
#9701 = EDGE_CURVE('',#7343,#7263,#4615,.T.) ;
#9702 = EDGE_CURVE('',#7185,#7114,#4616,.T.) ;
#9703 = EDGE_CURVE('',#7264,#7344,#4617,.T.) ;
#9704 = EDGE_CURVE('',#7111,#7245,#4618,.T.) ;
#9705 = EDGE_CURVE('',#7319,#7265,#4619,.T.) ;
#9706 = EDGE_CURVE('',#7246,#7108,#4620,.T.) ;
#9707 = EDGE_CURVE('',#7266,#7320,#4621,.T.) ;
#9708 = EDGE_CURVE('',#7105,#7188,#4622,.T.) ;
#9709 = EDGE_CURVE('',#7346,#7267,#4623,.T.) ;
#9710 = EDGE_CURVE('',#7189,#7102,#4624,.T.) ;
#9711 = EDGE_CURVE('',#7268,#7347,#4625,.T.) ;
#9712 = EDGE_CURVE('',#7099,#7191,#4626,.T.) ;
#9713 = EDGE_CURVE('',#7316,#7269,#4627,.T.) ;
#9714 = EDGE_CURVE('',#7192,#7096,#4628,.T.) ;
#9715 = EDGE_CURVE('',#7270,#7317,#4629,.T.) ;
#9716 = EDGE_CURVE('',#7093,#7194,#4630,.T.) ;
#9717 = EDGE_CURVE('',#7349,#7271,#4631,.T.) ;
#9718 = EDGE_CURVE('',#7195,#7090,#4632,.T.) ;
#9719 = EDGE_CURVE('',#7272,#7350,#4633,.T.) ;
#9720 = EDGE_CURVE('',#7087,#7197,#4634,.T.) ;
#9721 = EDGE_CURVE('',#7313,#7273,#4635,.T.) ;
#9722 = EDGE_CURVE('',#7198,#7084,#4636,.T.) ;
#9723 = EDGE_CURVE('',#7274,#7314,#4637,.T.) ;
#9724 = EDGE_CURVE('',#7081,#7247,#4638,.T.) ;
#9725 = EDGE_CURVE('',#7352,#7275,#4639,.T.) ;
#9726 = EDGE_CURVE('',#7248,#7078,#4640,.T.) ;
#9727 = EDGE_CURVE('',#7276,#7353,#4641,.T.) ;
#9728 = EDGE_CURVE('',#7407,#7407,#4642,.T.) ;
#9729 = EDGE_CURVE('',#7407,#7408,#5320,.T.) ;
#9730 = EDGE_CURVE('',#7408,#7408,#4643,.T.) ;
#9731 = EDGE_CURVE('',#7409,#7409,#4644,.T.) ;
#9732 = EDGE_CURVE('',#7410,#7410,#4645,.T.) ;
#9733 = EDGE_CURVE('',#7410,#7407,#5321,.T.) ;
#9734 = EDGE_CURVE('',#7411,#7411,#4646,.T.) ;
#9735 = EDGE_CURVE('',#7411,#7409,#5322,.T.) ;
#9736 = EDGE_CURVE('',#7411,#7412,#5323,.T.) ;
#9737 = EDGE_CURVE('',#7412,#7412,#4647,.T.) ;
#9738 = EDGE_CURVE('',#7410,#7413,#5324,.T.) ;
#9739 = EDGE_CURVE('',#7413,#7413,#4648,.T.) ;
#9740 = EDGE_CURVE('',#7414,#7414,#4649,.T.) ;
#9741 = EDGE_CURVE('',#7412,#7414,#5325,.T.) ;
#9742 = EDGE_CURVE('',#7415,#7415,#4650,.T.) ;
#9743 = EDGE_CURVE('',#7415,#7416,#5326,.T.) ;
#9744 = EDGE_CURVE('',#7416,#7416,#4651,.T.) ;
#9745 = EDGE_CURVE('',#7417,#7417,#4652,.T.) ;
#9746 = EDGE_CURVE('',#7417,#7418,#5327,.T.) ;
#9747 = EDGE_CURVE('',#7418,#7418,#4653,.T.) ;
#9748 = EDGE_CURVE('',#7419,#7419,#4654,.T.) ;
#9749 = EDGE_CURVE('',#7419,#7420,#5328,.T.) ;
#9750 = EDGE_CURVE('',#7420,#7420,#4655,.T.) ;
#9751 = EDGE_CURVE('',#7421,#7421,#4656,.T.) ;
#9752 = EDGE_CURVE('',#7421,#7422,#5329,.T.) ;
#9753 = EDGE_CURVE('',#7422,#7422,#4657,.T.) ;
#9754 = EDGE_CURVE('',#7423,#7423,#4658,.T.) ;
#9755 = EDGE_CURVE('',#7423,#7424,#5330,.T.) ;
#9756 = EDGE_CURVE('',#7424,#7424,#4659,.T.) ;
#9757 = EDGE_CURVE('',#7425,#7425,#4660,.T.) ;
#9758 = EDGE_CURVE('',#7425,#7426,#5331,.T.) ;
#9759 = EDGE_CURVE('',#7426,#7426,#4661,.T.) ;
#9760 = EDGE_CURVE('',#7427,#7427,#4662,.T.) ;
#9761 = EDGE_CURVE('',#7427,#7428,#5332,.T.) ;
#9762 = EDGE_CURVE('',#7428,#7428,#4663,.T.) ;
#9763 = EDGE_CURVE('',#7429,#7429,#4664,.T.) ;
#9764 = EDGE_CURVE('',#7429,#7430,#5333,.T.) ;
#9765 = EDGE_CURVE('',#7430,#7430,#4665,.T.) ;
#9766 = EDGE_CURVE('',#7431,#7431,#4666,.T.) ;
#9767 = EDGE_CURVE('',#7431,#7432,#5334,.T.) ;
#9768 = EDGE_CURVE('',#7432,#7432,#4667,.T.) ;
#9769 = EDGE_CURVE('',#7433,#7433,#4668,.T.) ;
#9770 = EDGE_CURVE('',#7433,#7434,#5335,.T.) ;
#9771 = EDGE_CURVE('',#7434,#7434,#4669,.T.) ;
#9772 = EDGE_CURVE('',#7435,#7435,#4670,.T.) ;
#9773 = EDGE_CURVE('',#7435,#7436,#5336,.T.) ;
#9774 = EDGE_CURVE('',#7436,#7436,#4671,.T.) ;
#9775 = EDGE_CURVE('',#7437,#7437,#4672,.T.) ;
#9776 = EDGE_CURVE('',#7437,#7438,#5337,.T.) ;
#9777 = EDGE_CURVE('',#7438,#7438,#4673,.T.) ;
#9778 = EDGE_CURVE('',#7439,#7439,#4674,.T.) ;
#9779 = EDGE_CURVE('',#7439,#7440,#5338,.T.) ;
#9780 = EDGE_CURVE('',#7440,#7440,#4675,.T.) ;
#9781 = EDGE_CURVE('',#7441,#7441,#4676,.T.) ;
#9782 = EDGE_CURVE('',#7441,#7442,#5339,.T.) ;
#9783 = EDGE_CURVE('',#7442,#7442,#4677,.T.) ;
#9784 = EDGE_CURVE('',#7443,#7443,#4678,.T.) ;
#9785 = EDGE_CURVE('',#7443,#7444,#5340,.T.) ;
#9786 = EDGE_CURVE('',#7444,#7444,#4679,.T.) ;
#9787 = EDGE_CURVE('',#7445,#7445,#4680,.T.) ;
#9788 = EDGE_CURVE('',#7445,#7446,#5341,.T.) ;
#9789 = EDGE_CURVE('',#7446,#7446,#4681,.T.) ;
#9790 = EDGE_CURVE('',#7447,#7447,#4682,.T.) ;
#9791 = EDGE_CURVE('',#7447,#7448,#5342,.T.) ;
#9792 = EDGE_CURVE('',#7448,#7448,#4683,.T.) ;
#9793 = EDGE_CURVE('',#7449,#7449,#4684,.T.) ;
#9794 = EDGE_CURVE('',#7449,#7450,#5343,.T.) ;
#9795 = EDGE_CURVE('',#7450,#7450,#4685,.T.) ;
#9796 = EDGE_CURVE('',#7451,#7451,#4686,.T.) ;
#9797 = EDGE_CURVE('',#7451,#7452,#5344,.T.) ;
#9798 = EDGE_CURVE('',#7452,#7452,#4687,.T.) ;
#9799 = EDGE_CURVE('',#7453,#7453,#4688,.T.) ;
#9800 = EDGE_CURVE('',#7453,#7454,#5345,.T.) ;
#9801 = EDGE_CURVE('',#7454,#7454,#4689,.T.) ;
#9802 = ORIENTED_EDGE('',*,*,#7455,.T.) ;
#9803 = ORIENTED_EDGE('',*,*,#7456,.F.) ;
#9804 = ORIENTED_EDGE('',*,*,#7455,.F.) ;
#9805 = ORIENTED_EDGE('',*,*,#7457,.F.) ;
#9806 = ORIENTED_EDGE('',*,*,#7458,.T.) ;
#9807 = ORIENTED_EDGE('',*,*,#7456,.T.) ;
#9808 = ORIENTED_EDGE('',*,*,#7458,.F.) ;
#9809 = ORIENTED_EDGE('',*,*,#7459,.T.) ;
#9810 = ORIENTED_EDGE('',*,*,#7460,.F.) ;
#9811 = ORIENTED_EDGE('',*,*,#7459,.F.) ;
#9812 = ORIENTED_EDGE('',*,*,#7461,.F.) ;
#9813 = ORIENTED_EDGE('',*,*,#7462,.T.) ;
#9814 = ORIENTED_EDGE('',*,*,#7460,.T.) ;
#9815 = ORIENTED_EDGE('',*,*,#7462,.F.) ;
#9816 = ORIENTED_EDGE('',*,*,#7463,.T.) ;
#9817 = ORIENTED_EDGE('',*,*,#7464,.F.) ;
#9818 = ORIENTED_EDGE('',*,*,#7463,.F.) ;
#9819 = ORIENTED_EDGE('',*,*,#7465,.F.) ;
#9820 = ORIENTED_EDGE('',*,*,#7466,.T.) ;
#9821 = ORIENTED_EDGE('',*,*,#7464,.T.) ;
#9822 = ORIENTED_EDGE('',*,*,#7466,.F.) ;
#9823 = ORIENTED_EDGE('',*,*,#7467,.T.) ;
#9824 = ORIENTED_EDGE('',*,*,#7468,.F.) ;
#9825 = ORIENTED_EDGE('',*,*,#7467,.F.) ;
#9826 = ORIENTED_EDGE('',*,*,#7469,.F.) ;
#9827 = ORIENTED_EDGE('',*,*,#7470,.T.) ;
#9828 = ORIENTED_EDGE('',*,*,#7468,.T.) ;
#9829 = ORIENTED_EDGE('',*,*,#7470,.F.) ;
#9830 = ORIENTED_EDGE('',*,*,#7471,.F.) ;
#9831 = ORIENTED_EDGE('',*,*,#7472,.T.) ;
#9832 = ORIENTED_EDGE('',*,*,#7473,.F.) ;
#9833 = ORIENTED_EDGE('',*,*,#7474,.T.) ;
#9834 = ORIENTED_EDGE('',*,*,#7471,.T.) ;
#9835 = ORIENTED_EDGE('',*,*,#7474,.F.) ;
#9836 = ORIENTED_EDGE('',*,*,#7472,.F.) ;
#9837 = ORIENTED_EDGE('',*,*,#7475,.T.) ;
#9838 = ORIENTED_EDGE('',*,*,#7476,.F.) ;
#9839 = ORIENTED_EDGE('',*,*,#7475,.F.) ;
#9840 = ORIENTED_EDGE('',*,*,#7477,.F.) ;
#9841 = ORIENTED_EDGE('',*,*,#7478,.T.) ;
#9842 = ORIENTED_EDGE('',*,*,#7479,.F.) ;
#9843 = ORIENTED_EDGE('',*,*,#7480,.T.) ;
#9844 = ORIENTED_EDGE('',*,*,#7477,.T.) ;
#9845 = ORIENTED_EDGE('',*,*,#7480,.F.) ;
#9846 = ORIENTED_EDGE('',*,*,#7478,.F.) ;
#9847 = ORIENTED_EDGE('',*,*,#7481,.T.) ;
#9848 = ORIENTED_EDGE('',*,*,#7482,.F.) ;
#9849 = ORIENTED_EDGE('',*,*,#7481,.F.) ;
#9850 = ORIENTED_EDGE('',*,*,#7483,.F.) ;
#9851 = ORIENTED_EDGE('',*,*,#7484,.T.) ;
#9852 = ORIENTED_EDGE('',*,*,#7485,.F.) ;
#9853 = ORIENTED_EDGE('',*,*,#7486,.T.) ;
#9854 = ORIENTED_EDGE('',*,*,#7483,.T.) ;
#9855 = ORIENTED_EDGE('',*,*,#7486,.F.) ;
#9856 = ORIENTED_EDGE('',*,*,#7484,.F.) ;
#9857 = ORIENTED_EDGE('',*,*,#7487,.T.) ;
#9858 = ORIENTED_EDGE('',*,*,#7488,.F.) ;
#9859 = ORIENTED_EDGE('',*,*,#7487,.F.) ;
#9860 = ORIENTED_EDGE('',*,*,#7489,.F.) ;
#9861 = ORIENTED_EDGE('',*,*,#7490,.T.) ;
#9862 = ORIENTED_EDGE('',*,*,#7491,.F.) ;
#9863 = ORIENTED_EDGE('',*,*,#7492,.T.) ;
#9864 = ORIENTED_EDGE('',*,*,#7489,.T.) ;
#9865 = ORIENTED_EDGE('',*,*,#7492,.F.) ;
#9866 = ORIENTED_EDGE('',*,*,#7490,.F.) ;
#9867 = ORIENTED_EDGE('',*,*,#7493,.T.) ;
#9868 = ORIENTED_EDGE('',*,*,#7494,.F.) ;
#9869 = ORIENTED_EDGE('',*,*,#7493,.F.) ;
#9870 = ORIENTED_EDGE('',*,*,#7495,.T.) ;
#9871 = ORIENTED_EDGE('',*,*,#7496,.F.) ;
#9872 = ORIENTED_EDGE('',*,*,#7495,.F.) ;
#9873 = ORIENTED_EDGE('',*,*,#7497,.F.) ;
#9874 = ORIENTED_EDGE('',*,*,#7498,.T.) ;
#9875 = ORIENTED_EDGE('',*,*,#7496,.T.) ;
#9876 = ORIENTED_EDGE('',*,*,#7498,.F.) ;
#9877 = ORIENTED_EDGE('',*,*,#7499,.T.) ;
#9878 = ORIENTED_EDGE('',*,*,#7500,.F.) ;
#9879 = ORIENTED_EDGE('',*,*,#7499,.F.) ;
#9880 = ORIENTED_EDGE('',*,*,#7501,.F.) ;
#9881 = ORIENTED_EDGE('',*,*,#7502,.T.) ;
#9882 = ORIENTED_EDGE('',*,*,#7500,.T.) ;
#9883 = ORIENTED_EDGE('',*,*,#7502,.F.) ;
#9884 = ORIENTED_EDGE('',*,*,#7503,.T.) ;
#9885 = ORIENTED_EDGE('',*,*,#7504,.F.) ;
#9886 = ORIENTED_EDGE('',*,*,#7503,.F.) ;
#9887 = ORIENTED_EDGE('',*,*,#7505,.F.) ;
#9888 = ORIENTED_EDGE('',*,*,#7506,.T.) ;
#9889 = ORIENTED_EDGE('',*,*,#7504,.T.) ;
#9890 = ORIENTED_EDGE('',*,*,#7506,.F.) ;
#9891 = ORIENTED_EDGE('',*,*,#7507,.T.) ;
#9892 = ORIENTED_EDGE('',*,*,#7508,.F.) ;
#9893 = ORIENTED_EDGE('',*,*,#7507,.F.) ;
#9894 = ORIENTED_EDGE('',*,*,#7509,.F.) ;
#9895 = ORIENTED_EDGE('',*,*,#7510,.T.) ;
#9896 = ORIENTED_EDGE('',*,*,#7508,.T.) ;
#9897 = ORIENTED_EDGE('',*,*,#7510,.F.) ;
#9898 = ORIENTED_EDGE('',*,*,#7511,.T.) ;
#9899 = ORIENTED_EDGE('',*,*,#7512,.F.) ;
#9900 = ORIENTED_EDGE('',*,*,#7511,.F.) ;
#9901 = ORIENTED_EDGE('',*,*,#7513,.F.) ;
#9902 = ORIENTED_EDGE('',*,*,#7514,.T.) ;
#9903 = ORIENTED_EDGE('',*,*,#7512,.T.) ;
#9904 = ORIENTED_EDGE('',*,*,#7514,.F.) ;
#9905 = ORIENTED_EDGE('',*,*,#7515,.T.) ;
#9906 = ORIENTED_EDGE('',*,*,#7516,.F.) ;
#9907 = ORIENTED_EDGE('',*,*,#7515,.F.) ;
#9908 = ORIENTED_EDGE('',*,*,#7517,.F.) ;
#9909 = ORIENTED_EDGE('',*,*,#7518,.T.) ;
#9910 = ORIENTED_EDGE('',*,*,#7516,.T.) ;
#9911 = ORIENTED_EDGE('',*,*,#7518,.F.) ;
#9912 = ORIENTED_EDGE('',*,*,#7519,.T.) ;
#9913 = ORIENTED_EDGE('',*,*,#7520,.F.) ;
#9914 = ORIENTED_EDGE('',*,*,#7519,.F.) ;
#9915 = ORIENTED_EDGE('',*,*,#7521,.F.) ;
#9916 = ORIENTED_EDGE('',*,*,#7522,.T.) ;
#9917 = ORIENTED_EDGE('',*,*,#7520,.T.) ;
#9918 = ORIENTED_EDGE('',*,*,#7522,.F.) ;
#9919 = ORIENTED_EDGE('',*,*,#7523,.T.) ;
#9920 = ORIENTED_EDGE('',*,*,#7524,.F.) ;
#9921 = ORIENTED_EDGE('',*,*,#7523,.F.) ;
#9922 = ORIENTED_EDGE('',*,*,#7525,.F.) ;
#9923 = ORIENTED_EDGE('',*,*,#7526,.T.) ;
#9924 = ORIENTED_EDGE('',*,*,#7524,.T.) ;
#9925 = ORIENTED_EDGE('',*,*,#7526,.F.) ;
#9926 = ORIENTED_EDGE('',*,*,#7527,.F.) ;
#9927 = ORIENTED_EDGE('',*,*,#7528,.T.) ;
#9928 = ORIENTED_EDGE('',*,*,#7529,.F.) ;
#9929 = ORIENTED_EDGE('',*,*,#7528,.F.) ;
#9930 = ORIENTED_EDGE('',*,*,#7530,.F.) ;
#9931 = ORIENTED_EDGE('',*,*,#7531,.T.) ;
#9932 = ORIENTED_EDGE('',*,*,#7532,.F.) ;
#9933 = ORIENTED_EDGE('',*,*,#7533,.F.) ;
#9934 = ORIENTED_EDGE('',*,*,#7465,.T.) ;
#9935 = ORIENTED_EDGE('',*,*,#7469,.T.) ;
#9936 = ORIENTED_EDGE('',*,*,#7534,.F.) ;
#9937 = ORIENTED_EDGE('',*,*,#7533,.T.) ;
#9938 = ORIENTED_EDGE('',*,*,#7535,.F.) ;
#9939 = ORIENTED_EDGE('',*,*,#7536,.F.) ;
#9940 = ORIENTED_EDGE('',*,*,#7537,.T.) ;
#9941 = ORIENTED_EDGE('',*,*,#7536,.T.) ;
#9942 = ORIENTED_EDGE('',*,*,#7538,.F.) ;
#9943 = ORIENTED_EDGE('',*,*,#7539,.F.) ;
#9944 = ORIENTED_EDGE('',*,*,#7457,.T.) ;
#9945 = ORIENTED_EDGE('',*,*,#7461,.T.) ;
#9946 = ORIENTED_EDGE('',*,*,#7540,.F.) ;
#9947 = ORIENTED_EDGE('',*,*,#7539,.T.) ;
#9948 = ORIENTED_EDGE('',*,*,#7541,.F.) ;
#9949 = ORIENTED_EDGE('',*,*,#7531,.F.) ;
#9950 = ORIENTED_EDGE('',*,*,#7540,.T.) ;
#9951 = ORIENTED_EDGE('',*,*,#7530,.T.) ;
#9952 = ORIENTED_EDGE('',*,*,#7534,.T.) ;
#9953 = ORIENTED_EDGE('',*,*,#7537,.F.) ;
#9954 = ORIENTED_EDGE('',*,*,#7473,.T.) ;
#9955 = ORIENTED_EDGE('',*,*,#7479,.T.) ;
#9956 = ORIENTED_EDGE('',*,*,#7485,.T.) ;
#9957 = ORIENTED_EDGE('',*,*,#7491,.T.) ;
#9958 = ORIENTED_EDGE('',*,*,#7527,.T.) ;
#9959 = ORIENTED_EDGE('',*,*,#7541,.T.) ;
#9960 = ORIENTED_EDGE('',*,*,#7538,.T.) ;
#9961 = ORIENTED_EDGE('',*,*,#7535,.T.) ;
#9962 = ORIENTED_EDGE('',*,*,#7532,.T.) ;
#9963 = ORIENTED_EDGE('',*,*,#7476,.T.) ;
#9964 = ORIENTED_EDGE('',*,*,#7482,.T.) ;
#9965 = ORIENTED_EDGE('',*,*,#7488,.T.) ;
#9966 = ORIENTED_EDGE('',*,*,#7494,.T.) ;
#9967 = ORIENTED_EDGE('',*,*,#7497,.T.) ;
#9968 = ORIENTED_EDGE('',*,*,#7501,.T.) ;
#9969 = ORIENTED_EDGE('',*,*,#7505,.T.) ;
#9970 = ORIENTED_EDGE('',*,*,#7509,.T.) ;
#9971 = ORIENTED_EDGE('',*,*,#7513,.T.) ;
#9972 = ORIENTED_EDGE('',*,*,#7517,.T.) ;
#9973 = ORIENTED_EDGE('',*,*,#7521,.T.) ;
#9974 = ORIENTED_EDGE('',*,*,#7525,.T.) ;
#9975 = ORIENTED_EDGE('',*,*,#7529,.T.) ;
#9976 = ORIENTED_EDGE('',*,*,#7542,.F.) ;
#9977 = ORIENTED_EDGE('',*,*,#7543,.T.) ;
#9978 = ORIENTED_EDGE('',*,*,#7544,.F.) ;
#9979 = ORIENTED_EDGE('',*,*,#7545,.T.) ;
#9980 = ORIENTED_EDGE('',*,*,#7542,.T.) ;
#9981 = ORIENTED_EDGE('',*,*,#7545,.F.) ;
#9982 = ORIENTED_EDGE('',*,*,#7543,.F.) ;
#9983 = ORIENTED_EDGE('',*,*,#7546,.T.) ;
#9984 = ORIENTED_EDGE('',*,*,#7547,.F.) ;
#9985 = ORIENTED_EDGE('',*,*,#7546,.F.) ;
#9986 = ORIENTED_EDGE('',*,*,#7548,.F.) ;
#9987 = ORIENTED_EDGE('',*,*,#7549,.T.) ;
#9988 = ORIENTED_EDGE('',*,*,#7550,.F.) ;
#9989 = ORIENTED_EDGE('',*,*,#7551,.T.) ;
#9990 = ORIENTED_EDGE('',*,*,#7548,.T.) ;
#9991 = ORIENTED_EDGE('',*,*,#7551,.F.) ;
#9992 = ORIENTED_EDGE('',*,*,#7549,.F.) ;
#9993 = ORIENTED_EDGE('',*,*,#7552,.T.) ;
#9994 = ORIENTED_EDGE('',*,*,#7553,.F.) ;
#9995 = ORIENTED_EDGE('',*,*,#7552,.F.) ;
#9996 = ORIENTED_EDGE('',*,*,#7554,.F.) ;
#9997 = ORIENTED_EDGE('',*,*,#7555,.T.) ;
#9998 = ORIENTED_EDGE('',*,*,#7556,.F.) ;
#9999 = ORIENTED_EDGE('',*,*,#7557,.T.) ;
#10000 = ORIENTED_EDGE('',*,*,#7554,.T.) ;
#10001 = ORIENTED_EDGE('',*,*,#7557,.F.) ;
#10002 = ORIENTED_EDGE('',*,*,#7555,.F.) ;
#10003 = ORIENTED_EDGE('',*,*,#7558,.T.) ;
#10004 = ORIENTED_EDGE('',*,*,#7559,.F.) ;
#10005 = ORIENTED_EDGE('',*,*,#7558,.F.) ;
#10006 = ORIENTED_EDGE('',*,*,#7560,.F.) ;
#10007 = ORIENTED_EDGE('',*,*,#7561,.T.) ;
#10008 = ORIENTED_EDGE('',*,*,#7562,.F.) ;
#10009 = ORIENTED_EDGE('',*,*,#7563,.T.) ;
#10010 = ORIENTED_EDGE('',*,*,#7560,.T.) ;
#10011 = ORIENTED_EDGE('',*,*,#7563,.F.) ;
#10012 = ORIENTED_EDGE('',*,*,#7561,.F.) ;
#10013 = ORIENTED_EDGE('',*,*,#7564,.T.) ;
#10014 = ORIENTED_EDGE('',*,*,#7565,.F.) ;
#10015 = ORIENTED_EDGE('',*,*,#7564,.F.) ;
#10016 = ORIENTED_EDGE('',*,*,#7566,.F.) ;
#10017 = ORIENTED_EDGE('',*,*,#7567,.T.) ;
#10018 = ORIENTED_EDGE('',*,*,#7568,.F.) ;
#10019 = ORIENTED_EDGE('',*,*,#7569,.T.) ;
#10020 = ORIENTED_EDGE('',*,*,#7566,.T.) ;
#10021 = ORIENTED_EDGE('',*,*,#7569,.F.) ;
#10022 = ORIENTED_EDGE('',*,*,#7567,.F.) ;
#10023 = ORIENTED_EDGE('',*,*,#7570,.T.) ;
#10024 = ORIENTED_EDGE('',*,*,#7571,.F.) ;
#10025 = ORIENTED_EDGE('',*,*,#7570,.F.) ;
#10026 = ORIENTED_EDGE('',*,*,#7572,.F.) ;
#10027 = ORIENTED_EDGE('',*,*,#7573,.T.) ;
#10028 = ORIENTED_EDGE('',*,*,#7574,.F.) ;
#10029 = ORIENTED_EDGE('',*,*,#7575,.T.) ;
#10030 = ORIENTED_EDGE('',*,*,#7572,.T.) ;
#10031 = ORIENTED_EDGE('',*,*,#7575,.F.) ;
#10032 = ORIENTED_EDGE('',*,*,#7573,.F.) ;
#10033 = ORIENTED_EDGE('',*,*,#7576,.T.) ;
#10034 = ORIENTED_EDGE('',*,*,#7577,.F.) ;
#10035 = ORIENTED_EDGE('',*,*,#7576,.F.) ;
#10036 = ORIENTED_EDGE('',*,*,#7578,.F.) ;
#10037 = ORIENTED_EDGE('',*,*,#7579,.T.) ;
#10038 = ORIENTED_EDGE('',*,*,#7580,.F.) ;
#10039 = ORIENTED_EDGE('',*,*,#7581,.T.) ;
#10040 = ORIENTED_EDGE('',*,*,#7578,.T.) ;
#10041 = ORIENTED_EDGE('',*,*,#7581,.F.) ;
#10042 = ORIENTED_EDGE('',*,*,#7579,.F.) ;
#10043 = ORIENTED_EDGE('',*,*,#7582,.T.) ;
#10044 = ORIENTED_EDGE('',*,*,#7583,.F.) ;
#10045 = ORIENTED_EDGE('',*,*,#7582,.F.) ;
#10046 = ORIENTED_EDGE('',*,*,#7584,.F.) ;
#10047 = ORIENTED_EDGE('',*,*,#7585,.T.) ;
#10048 = ORIENTED_EDGE('',*,*,#7586,.F.) ;
#10049 = ORIENTED_EDGE('',*,*,#7587,.T.) ;
#10050 = ORIENTED_EDGE('',*,*,#7584,.T.) ;
#10051 = ORIENTED_EDGE('',*,*,#7587,.F.) ;
#10052 = ORIENTED_EDGE('',*,*,#7585,.F.) ;
#10053 = ORIENTED_EDGE('',*,*,#7588,.T.) ;
#10054 = ORIENTED_EDGE('',*,*,#7589,.F.) ;
#10055 = ORIENTED_EDGE('',*,*,#7588,.F.) ;
#10056 = ORIENTED_EDGE('',*,*,#7590,.F.) ;
#10057 = ORIENTED_EDGE('',*,*,#7591,.T.) ;
#10058 = ORIENTED_EDGE('',*,*,#7592,.F.) ;
#10059 = ORIENTED_EDGE('',*,*,#7593,.T.) ;
#10060 = ORIENTED_EDGE('',*,*,#7590,.T.) ;
#10061 = ORIENTED_EDGE('',*,*,#7593,.F.) ;
#10062 = ORIENTED_EDGE('',*,*,#7591,.F.) ;
#10063 = ORIENTED_EDGE('',*,*,#7594,.T.) ;
#10064 = ORIENTED_EDGE('',*,*,#7595,.F.) ;
#10065 = ORIENTED_EDGE('',*,*,#7594,.F.) ;
#10066 = ORIENTED_EDGE('',*,*,#7596,.F.) ;
#10067 = ORIENTED_EDGE('',*,*,#7597,.T.) ;
#10068 = ORIENTED_EDGE('',*,*,#7598,.F.) ;
#10069 = ORIENTED_EDGE('',*,*,#7599,.T.) ;
#10070 = ORIENTED_EDGE('',*,*,#7596,.T.) ;
#10071 = ORIENTED_EDGE('',*,*,#7599,.F.) ;
#10072 = ORIENTED_EDGE('',*,*,#7597,.F.) ;
#10073 = ORIENTED_EDGE('',*,*,#7600,.T.) ;
#10074 = ORIENTED_EDGE('',*,*,#7601,.F.) ;
#10075 = ORIENTED_EDGE('',*,*,#7600,.F.) ;
#10076 = ORIENTED_EDGE('',*,*,#7602,.F.) ;
#10077 = ORIENTED_EDGE('',*,*,#7603,.T.) ;
#10078 = ORIENTED_EDGE('',*,*,#7604,.F.) ;
#10079 = ORIENTED_EDGE('',*,*,#7605,.T.) ;
#10080 = ORIENTED_EDGE('',*,*,#7602,.T.) ;
#10081 = ORIENTED_EDGE('',*,*,#7605,.F.) ;
#10082 = ORIENTED_EDGE('',*,*,#7603,.F.) ;
#10083 = ORIENTED_EDGE('',*,*,#7606,.T.) ;
#10084 = ORIENTED_EDGE('',*,*,#7607,.F.) ;
#10085 = ORIENTED_EDGE('',*,*,#7606,.F.) ;
#10086 = ORIENTED_EDGE('',*,*,#7608,.F.) ;
#10087 = ORIENTED_EDGE('',*,*,#7609,.T.) ;
#10088 = ORIENTED_EDGE('',*,*,#7610,.F.) ;
#10089 = ORIENTED_EDGE('',*,*,#7611,.T.) ;
#10090 = ORIENTED_EDGE('',*,*,#7608,.T.) ;
#10091 = ORIENTED_EDGE('',*,*,#7611,.F.) ;
#10092 = ORIENTED_EDGE('',*,*,#7609,.F.) ;
#10093 = ORIENTED_EDGE('',*,*,#7612,.T.) ;
#10094 = ORIENTED_EDGE('',*,*,#7613,.F.) ;
#10095 = ORIENTED_EDGE('',*,*,#7612,.F.) ;
#10096 = ORIENTED_EDGE('',*,*,#7614,.T.) ;
#10097 = ORIENTED_EDGE('',*,*,#7615,.F.) ;
#10098 = ORIENTED_EDGE('',*,*,#7616,.T.) ;
#10099 = ORIENTED_EDGE('',*,*,#7617,.T.) ;
#10100 = ORIENTED_EDGE('',*,*,#7547,.T.) ;
#10101 = ORIENTED_EDGE('',*,*,#7553,.T.) ;
#10102 = ORIENTED_EDGE('',*,*,#7559,.T.) ;
#10103 = ORIENTED_EDGE('',*,*,#7565,.T.) ;
#10104 = ORIENTED_EDGE('',*,*,#7571,.T.) ;
#10105 = ORIENTED_EDGE('',*,*,#7577,.T.) ;
#10106 = ORIENTED_EDGE('',*,*,#7583,.T.) ;
#10107 = ORIENTED_EDGE('',*,*,#7589,.T.) ;
#10108 = ORIENTED_EDGE('',*,*,#7592,.T.) ;
#10109 = ORIENTED_EDGE('',*,*,#7598,.T.) ;
#10110 = ORIENTED_EDGE('',*,*,#7604,.T.) ;
#10111 = ORIENTED_EDGE('',*,*,#7610,.T.) ;
#10112 = ORIENTED_EDGE('',*,*,#7618,.T.) ;
#10113 = ORIENTED_EDGE('',*,*,#7619,.F.) ;
#10114 = ORIENTED_EDGE('',*,*,#7620,.T.) ;
#10115 = ORIENTED_EDGE('',*,*,#7615,.T.) ;
#10116 = ORIENTED_EDGE('',*,*,#7621,.T.) ;
#10117 = ORIENTED_EDGE('',*,*,#7622,.F.) ;
#10118 = ORIENTED_EDGE('',*,*,#7623,.T.) ;
#10119 = ORIENTED_EDGE('',*,*,#7619,.T.) ;
#10120 = ORIENTED_EDGE('',*,*,#7544,.T.) ;
#10121 = ORIENTED_EDGE('',*,*,#7550,.T.) ;
#10122 = ORIENTED_EDGE('',*,*,#7556,.T.) ;
#10123 = ORIENTED_EDGE('',*,*,#7562,.T.) ;
#10124 = ORIENTED_EDGE('',*,*,#7568,.T.) ;
#10125 = ORIENTED_EDGE('',*,*,#7574,.T.) ;
#10126 = ORIENTED_EDGE('',*,*,#7580,.T.) ;
#10127 = ORIENTED_EDGE('',*,*,#7586,.T.) ;
#10128 = ORIENTED_EDGE('',*,*,#7595,.T.) ;
#10129 = ORIENTED_EDGE('',*,*,#7601,.T.) ;
#10130 = ORIENTED_EDGE('',*,*,#7607,.T.) ;
#10131 = ORIENTED_EDGE('',*,*,#7613,.T.) ;
#10132 = ORIENTED_EDGE('',*,*,#7624,.T.) ;
#10133 = ORIENTED_EDGE('',*,*,#7617,.F.) ;
#10134 = ORIENTED_EDGE('',*,*,#7625,.T.) ;
#10135 = ORIENTED_EDGE('',*,*,#7622,.T.) ;
#10136 = ORIENTED_EDGE('',*,*,#7620,.F.) ;
#10137 = ORIENTED_EDGE('',*,*,#7623,.F.) ;
#10138 = ORIENTED_EDGE('',*,*,#7625,.F.) ;
#10139 = ORIENTED_EDGE('',*,*,#7616,.F.) ;
#10140 = ORIENTED_EDGE('',*,*,#7621,.F.) ;
#10141 = ORIENTED_EDGE('',*,*,#7618,.F.) ;
#10142 = ORIENTED_EDGE('',*,*,#7614,.F.) ;
#10143 = ORIENTED_EDGE('',*,*,#7624,.F.) ;
#10144 = ORIENTED_EDGE('',*,*,#7626,.T.) ;
#10145 = ORIENTED_EDGE('',*,*,#7627,.F.) ;
#10146 = ORIENTED_EDGE('',*,*,#7626,.F.) ;
#10147 = ORIENTED_EDGE('',*,*,#7628,.F.) ;
#10148 = ORIENTED_EDGE('',*,*,#7629,.T.) ;
#10149 = ORIENTED_EDGE('',*,*,#7627,.T.) ;
#10150 = ORIENTED_EDGE('',*,*,#7629,.F.) ;
#10151 = ORIENTED_EDGE('',*,*,#7630,.T.) ;
#10152 = ORIENTED_EDGE('',*,*,#7631,.F.) ;
#10153 = ORIENTED_EDGE('',*,*,#7630,.F.) ;
#10154 = ORIENTED_EDGE('',*,*,#7632,.F.) ;
#10155 = ORIENTED_EDGE('',*,*,#7633,.T.) ;
#10156 = ORIENTED_EDGE('',*,*,#7631,.T.) ;
#10157 = ORIENTED_EDGE('',*,*,#7633,.F.) ;
#10158 = ORIENTED_EDGE('',*,*,#7634,.T.) ;
#10159 = ORIENTED_EDGE('',*,*,#7635,.F.) ;
#10160 = ORIENTED_EDGE('',*,*,#7634,.F.) ;
#10161 = ORIENTED_EDGE('',*,*,#7636,.F.) ;
#10162 = ORIENTED_EDGE('',*,*,#7637,.T.) ;
#10163 = ORIENTED_EDGE('',*,*,#7635,.T.) ;
#10164 = ORIENTED_EDGE('',*,*,#7637,.F.) ;
#10165 = ORIENTED_EDGE('',*,*,#7638,.T.) ;
#10166 = ORIENTED_EDGE('',*,*,#7639,.F.) ;
#10167 = ORIENTED_EDGE('',*,*,#7638,.F.) ;
#10168 = ORIENTED_EDGE('',*,*,#7640,.F.) ;
#10169 = ORIENTED_EDGE('',*,*,#7641,.T.) ;
#10170 = ORIENTED_EDGE('',*,*,#7639,.T.) ;
#10171 = ORIENTED_EDGE('',*,*,#7641,.F.) ;
#10172 = ORIENTED_EDGE('',*,*,#7642,.T.) ;
#10173 = ORIENTED_EDGE('',*,*,#7643,.T.) ;
#10174 = ORIENTED_EDGE('',*,*,#7642,.F.) ;
#10175 = ORIENTED_EDGE('',*,*,#7643,.F.) ;
#10176 = ORIENTED_EDGE('',*,*,#7644,.T.) ;
#10177 = ORIENTED_EDGE('',*,*,#7645,.T.) ;
#10178 = ORIENTED_EDGE('',*,*,#7644,.F.) ;
#10179 = ORIENTED_EDGE('',*,*,#7646,.T.) ;
#10180 = ORIENTED_EDGE('',*,*,#7647,.T.) ;
#10181 = ORIENTED_EDGE('',*,*,#7646,.F.) ;
#10182 = ORIENTED_EDGE('',*,*,#7647,.F.) ;
#10183 = ORIENTED_EDGE('',*,*,#7648,.T.) ;
#10184 = ORIENTED_EDGE('',*,*,#7649,.T.) ;
#10185 = ORIENTED_EDGE('',*,*,#7648,.F.) ;
#10186 = ORIENTED_EDGE('',*,*,#7650,.F.) ;
#10187 = ORIENTED_EDGE('',*,*,#7651,.F.) ;
#10188 = ORIENTED_EDGE('',*,*,#7652,.F.) ;
#10189 = ORIENTED_EDGE('',*,*,#7653,.F.) ;
#10190 = ORIENTED_EDGE('',*,*,#7645,.F.) ;
#10191 = ORIENTED_EDGE('',*,*,#7649,.F.) ;
#10192 = ORIENTED_EDGE('',*,*,#7654,.T.) ;
#10193 = ORIENTED_EDGE('',*,*,#7655,.F.) ;
#10194 = ORIENTED_EDGE('',*,*,#7654,.F.) ;
#10195 = ORIENTED_EDGE('',*,*,#7656,.F.) ;
#10196 = ORIENTED_EDGE('',*,*,#7657,.T.) ;
#10197 = ORIENTED_EDGE('',*,*,#7655,.T.) ;
#10198 = ORIENTED_EDGE('',*,*,#7657,.F.) ;
#10199 = ORIENTED_EDGE('',*,*,#7658,.T.) ;
#10200 = ORIENTED_EDGE('',*,*,#7659,.F.) ;
#10201 = ORIENTED_EDGE('',*,*,#7658,.F.) ;
#10202 = ORIENTED_EDGE('',*,*,#7660,.F.) ;
#10203 = ORIENTED_EDGE('',*,*,#7661,.T.) ;
#10204 = ORIENTED_EDGE('',*,*,#7659,.T.) ;
#10205 = ORIENTED_EDGE('',*,*,#7661,.F.) ;
#10206 = ORIENTED_EDGE('',*,*,#7662,.F.) ;
#10207 = ORIENTED_EDGE('',*,*,#7663,.T.) ;
#10208 = ORIENTED_EDGE('',*,*,#7653,.T.) ;
#10209 = ORIENTED_EDGE('',*,*,#7664,.F.) ;
#10210 = ORIENTED_EDGE('',*,*,#7665,.F.) ;
#10211 = ORIENTED_EDGE('',*,*,#7664,.T.) ;
#10212 = ORIENTED_EDGE('',*,*,#7652,.T.) ;
#10213 = ORIENTED_EDGE('',*,*,#7666,.F.) ;
#10214 = ORIENTED_EDGE('',*,*,#7628,.T.) ;
#10215 = ORIENTED_EDGE('',*,*,#7632,.T.) ;
#10216 = ORIENTED_EDGE('',*,*,#7667,.F.) ;
#10217 = ORIENTED_EDGE('',*,*,#7666,.T.) ;
#10218 = ORIENTED_EDGE('',*,*,#7651,.T.) ;
#10219 = ORIENTED_EDGE('',*,*,#7668,.F.) ;
#10220 = ORIENTED_EDGE('',*,*,#7669,.F.) ;
#10221 = ORIENTED_EDGE('',*,*,#7668,.T.) ;
#10222 = ORIENTED_EDGE('',*,*,#7650,.T.) ;
#10223 = ORIENTED_EDGE('',*,*,#7663,.F.) ;
#10224 = ORIENTED_EDGE('',*,*,#7636,.T.) ;
#10225 = ORIENTED_EDGE('',*,*,#7640,.T.) ;
#10226 = ORIENTED_EDGE('',*,*,#7669,.T.) ;
#10227 = ORIENTED_EDGE('',*,*,#7662,.T.) ;
#10228 = ORIENTED_EDGE('',*,*,#7665,.T.) ;
#10229 = ORIENTED_EDGE('',*,*,#7667,.T.) ;
#10230 = ORIENTED_EDGE('',*,*,#7656,.T.) ;
#10231 = ORIENTED_EDGE('',*,*,#7660,.T.) ;
#10232 = ORIENTED_EDGE('',*,*,#7670,.T.) ;
#10233 = ORIENTED_EDGE('',*,*,#7671,.F.) ;
#10234 = ORIENTED_EDGE('',*,*,#7670,.F.) ;
#10235 = ORIENTED_EDGE('',*,*,#7672,.F.) ;
#10236 = ORIENTED_EDGE('',*,*,#7673,.T.) ;
#10237 = ORIENTED_EDGE('',*,*,#7671,.T.) ;
#10238 = ORIENTED_EDGE('',*,*,#7673,.F.) ;
#10239 = ORIENTED_EDGE('',*,*,#7674,.T.) ;
#10240 = ORIENTED_EDGE('',*,*,#7675,.F.) ;
#10241 = ORIENTED_EDGE('',*,*,#7674,.F.) ;
#10242 = ORIENTED_EDGE('',*,*,#7676,.F.) ;
#10243 = ORIENTED_EDGE('',*,*,#7677,.T.) ;
#10244 = ORIENTED_EDGE('',*,*,#7675,.T.) ;
#10245 = ORIENTED_EDGE('',*,*,#7677,.F.) ;
#10246 = ORIENTED_EDGE('',*,*,#7678,.T.) ;
#10247 = ORIENTED_EDGE('',*,*,#7679,.F.) ;
#10248 = ORIENTED_EDGE('',*,*,#7678,.F.) ;
#10249 = ORIENTED_EDGE('',*,*,#7680,.F.) ;
#10250 = ORIENTED_EDGE('',*,*,#7681,.T.) ;
#10251 = ORIENTED_EDGE('',*,*,#7679,.T.) ;
#10252 = ORIENTED_EDGE('',*,*,#7681,.F.) ;
#10253 = ORIENTED_EDGE('',*,*,#7682,.T.) ;
#10254 = ORIENTED_EDGE('',*,*,#7683,.F.) ;
#10255 = ORIENTED_EDGE('',*,*,#7682,.F.) ;
#10256 = ORIENTED_EDGE('',*,*,#7684,.F.) ;
#10257 = ORIENTED_EDGE('',*,*,#7685,.T.) ;
#10258 = ORIENTED_EDGE('',*,*,#7683,.T.) ;
#10259 = ORIENTED_EDGE('',*,*,#7685,.F.) ;
#10260 = ORIENTED_EDGE('',*,*,#7686,.T.) ;
#10261 = ORIENTED_EDGE('',*,*,#7687,.F.) ;
#10262 = ORIENTED_EDGE('',*,*,#7686,.F.) ;
#10263 = ORIENTED_EDGE('',*,*,#7688,.F.) ;
#10264 = ORIENTED_EDGE('',*,*,#7689,.T.) ;
#10265 = ORIENTED_EDGE('',*,*,#7687,.T.) ;
#10266 = ORIENTED_EDGE('',*,*,#7689,.F.) ;
#10267 = ORIENTED_EDGE('',*,*,#7690,.T.) ;
#10268 = ORIENTED_EDGE('',*,*,#7691,.F.) ;
#10269 = ORIENTED_EDGE('',*,*,#7690,.F.) ;
#10270 = ORIENTED_EDGE('',*,*,#7692,.F.) ;
#10271 = ORIENTED_EDGE('',*,*,#7693,.T.) ;
#10272 = ORIENTED_EDGE('',*,*,#7691,.T.) ;
#10273 = ORIENTED_EDGE('',*,*,#7693,.F.) ;
#10274 = ORIENTED_EDGE('',*,*,#7694,.T.) ;
#10275 = ORIENTED_EDGE('',*,*,#7695,.F.) ;
#10276 = ORIENTED_EDGE('',*,*,#7694,.F.) ;
#10277 = ORIENTED_EDGE('',*,*,#7696,.T.) ;
#10278 = ORIENTED_EDGE('',*,*,#7697,.T.) ;
#10279 = ORIENTED_EDGE('',*,*,#7696,.F.) ;
#10280 = ORIENTED_EDGE('',*,*,#7698,.T.) ;
#10281 = ORIENTED_EDGE('',*,*,#7699,.T.) ;
#10282 = ORIENTED_EDGE('',*,*,#7695,.T.) ;
#10283 = ORIENTED_EDGE('',*,*,#7699,.F.) ;
#10284 = ORIENTED_EDGE('',*,*,#7700,.T.) ;
#10285 = ORIENTED_EDGE('',*,*,#7701,.F.) ;
#10286 = ORIENTED_EDGE('',*,*,#7700,.F.) ;
#10287 = ORIENTED_EDGE('',*,*,#7702,.T.) ;
#10288 = ORIENTED_EDGE('',*,*,#7703,.T.) ;
#10289 = ORIENTED_EDGE('',*,*,#7702,.F.) ;
#10290 = ORIENTED_EDGE('',*,*,#7704,.T.) ;
#10291 = ORIENTED_EDGE('',*,*,#7705,.T.) ;
#10292 = ORIENTED_EDGE('',*,*,#7701,.T.) ;
#10293 = ORIENTED_EDGE('',*,*,#7705,.F.) ;
#10294 = ORIENTED_EDGE('',*,*,#7706,.T.) ;
#10295 = ORIENTED_EDGE('',*,*,#7707,.F.) ;
#10296 = ORIENTED_EDGE('',*,*,#7706,.F.) ;
#10297 = ORIENTED_EDGE('',*,*,#7708,.T.) ;
#10298 = ORIENTED_EDGE('',*,*,#7709,.T.) ;
#10299 = ORIENTED_EDGE('',*,*,#7708,.F.) ;
#10300 = ORIENTED_EDGE('',*,*,#7710,.T.) ;
#10301 = ORIENTED_EDGE('',*,*,#7711,.T.) ;
#10302 = ORIENTED_EDGE('',*,*,#7707,.T.) ;
#10303 = ORIENTED_EDGE('',*,*,#7711,.F.) ;
#10304 = ORIENTED_EDGE('',*,*,#7712,.T.) ;
#10305 = ORIENTED_EDGE('',*,*,#7713,.F.) ;
#10306 = ORIENTED_EDGE('',*,*,#7712,.F.) ;
#10307 = ORIENTED_EDGE('',*,*,#7714,.T.) ;
#10308 = ORIENTED_EDGE('',*,*,#7715,.T.) ;
#10309 = ORIENTED_EDGE('',*,*,#7714,.F.) ;
#10310 = ORIENTED_EDGE('',*,*,#7716,.T.) ;
#10311 = ORIENTED_EDGE('',*,*,#7717,.T.) ;
#10312 = ORIENTED_EDGE('',*,*,#7713,.T.) ;
#10313 = ORIENTED_EDGE('',*,*,#7717,.F.) ;
#10314 = ORIENTED_EDGE('',*,*,#7718,.T.) ;
#10315 = ORIENTED_EDGE('',*,*,#7719,.T.) ;
#10316 = ORIENTED_EDGE('',*,*,#7718,.F.) ;
#10317 = ORIENTED_EDGE('',*,*,#7719,.F.) ;
#10318 = ORIENTED_EDGE('',*,*,#7720,.T.) ;
#10319 = ORIENTED_EDGE('',*,*,#7721,.T.) ;
#10320 = ORIENTED_EDGE('',*,*,#7720,.F.) ;
#10321 = ORIENTED_EDGE('',*,*,#7722,.T.) ;
#10322 = ORIENTED_EDGE('',*,*,#7723,.T.) ;
#10323 = ORIENTED_EDGE('',*,*,#7722,.F.) ;
#10324 = ORIENTED_EDGE('',*,*,#7723,.F.) ;
#10325 = ORIENTED_EDGE('',*,*,#7724,.T.) ;
#10326 = ORIENTED_EDGE('',*,*,#7725,.T.) ;
#10327 = ORIENTED_EDGE('',*,*,#7724,.F.) ;
#10328 = ORIENTED_EDGE('',*,*,#7726,.T.) ;
#10329 = ORIENTED_EDGE('',*,*,#7727,.T.) ;
#10330 = ORIENTED_EDGE('',*,*,#7726,.F.) ;
#10331 = ORIENTED_EDGE('',*,*,#7727,.F.) ;
#10332 = ORIENTED_EDGE('',*,*,#7728,.T.) ;
#10333 = ORIENTED_EDGE('',*,*,#7729,.T.) ;
#10334 = ORIENTED_EDGE('',*,*,#7728,.F.) ;
#10335 = ORIENTED_EDGE('',*,*,#7730,.T.) ;
#10336 = ORIENTED_EDGE('',*,*,#7731,.T.) ;
#10337 = ORIENTED_EDGE('',*,*,#7730,.F.) ;
#10338 = ORIENTED_EDGE('',*,*,#7731,.F.) ;
#10339 = ORIENTED_EDGE('',*,*,#7732,.T.) ;
#10340 = ORIENTED_EDGE('',*,*,#7733,.T.) ;
#10341 = ORIENTED_EDGE('',*,*,#7732,.F.) ;
#10342 = ORIENTED_EDGE('',*,*,#7734,.T.) ;
#10343 = ORIENTED_EDGE('',*,*,#7735,.T.) ;
#10344 = ORIENTED_EDGE('',*,*,#7734,.F.) ;
#10345 = ORIENTED_EDGE('',*,*,#7735,.F.) ;
#10346 = ORIENTED_EDGE('',*,*,#7736,.T.) ;
#10347 = ORIENTED_EDGE('',*,*,#7737,.T.) ;
#10348 = ORIENTED_EDGE('',*,*,#7736,.F.) ;
#10349 = ORIENTED_EDGE('',*,*,#7738,.T.) ;
#10350 = ORIENTED_EDGE('',*,*,#7739,.T.) ;
#10351 = ORIENTED_EDGE('',*,*,#7738,.F.) ;
#10352 = ORIENTED_EDGE('',*,*,#7739,.F.) ;
#10353 = ORIENTED_EDGE('',*,*,#7740,.T.) ;
#10354 = ORIENTED_EDGE('',*,*,#7741,.T.) ;
#10355 = ORIENTED_EDGE('',*,*,#7740,.F.) ;
#10356 = ORIENTED_EDGE('',*,*,#7742,.T.) ;
#10357 = ORIENTED_EDGE('',*,*,#7743,.T.) ;
#10358 = ORIENTED_EDGE('',*,*,#7742,.F.) ;
#10359 = ORIENTED_EDGE('',*,*,#7743,.F.) ;
#10360 = ORIENTED_EDGE('',*,*,#7744,.T.) ;
#10361 = ORIENTED_EDGE('',*,*,#7745,.T.) ;
#10362 = ORIENTED_EDGE('',*,*,#7744,.F.) ;
#10363 = ORIENTED_EDGE('',*,*,#7746,.T.) ;
#10364 = ORIENTED_EDGE('',*,*,#7747,.T.) ;
#10365 = ORIENTED_EDGE('',*,*,#7746,.F.) ;
#10366 = ORIENTED_EDGE('',*,*,#7747,.F.) ;
#10367 = ORIENTED_EDGE('',*,*,#7748,.T.) ;
#10368 = ORIENTED_EDGE('',*,*,#7749,.T.) ;
#10369 = ORIENTED_EDGE('',*,*,#7748,.F.) ;
#10370 = ORIENTED_EDGE('',*,*,#7750,.T.) ;
#10371 = ORIENTED_EDGE('',*,*,#7751,.T.) ;
#10372 = ORIENTED_EDGE('',*,*,#7752,.T.) ;
#10373 = ORIENTED_EDGE('',*,*,#7751,.F.) ;
#10374 = ORIENTED_EDGE('',*,*,#7753,.T.) ;
#10375 = ORIENTED_EDGE('',*,*,#7754,.T.) ;
#10376 = ORIENTED_EDGE('',*,*,#7755,.T.) ;
#10377 = ORIENTED_EDGE('',*,*,#7756,.F.) ;
#10378 = ORIENTED_EDGE('',*,*,#7688,.T.) ;
#10379 = ORIENTED_EDGE('',*,*,#7692,.T.) ;
#10380 = ORIENTED_EDGE('',*,*,#7757,.T.) ;
#10381 = ORIENTED_EDGE('',*,*,#7758,.T.) ;
#10382 = ORIENTED_EDGE('',*,*,#7759,.T.) ;
#10383 = ORIENTED_EDGE('',*,*,#7754,.F.) ;
#10384 = ORIENTED_EDGE('',*,*,#7760,.F.) ;
#10385 = ORIENTED_EDGE('',*,*,#7761,.T.) ;
#10386 = ORIENTED_EDGE('',*,*,#7762,.T.) ;
#10387 = ORIENTED_EDGE('',*,*,#7758,.F.) ;
#10388 = ORIENTED_EDGE('',*,*,#7680,.T.) ;
#10389 = ORIENTED_EDGE('',*,*,#7684,.T.) ;
#10390 = ORIENTED_EDGE('',*,*,#7763,.T.) ;
#10391 = ORIENTED_EDGE('',*,*,#7756,.T.) ;
#10392 = ORIENTED_EDGE('',*,*,#7764,.T.) ;
#10393 = ORIENTED_EDGE('',*,*,#7761,.F.) ;
#10394 = ORIENTED_EDGE('',*,*,#7763,.F.) ;
#10395 = ORIENTED_EDGE('',*,*,#7760,.T.) ;
#10396 = ORIENTED_EDGE('',*,*,#7757,.F.) ;
#10397 = ORIENTED_EDGE('',*,*,#7753,.F.) ;
#10398 = ORIENTED_EDGE('',*,*,#7672,.T.) ;
#10399 = ORIENTED_EDGE('',*,*,#7676,.T.) ;
#10400 = ORIENTED_EDGE('',*,*,#7697,.F.) ;
#10401 = ORIENTED_EDGE('',*,*,#7703,.F.) ;
#10402 = ORIENTED_EDGE('',*,*,#7709,.F.) ;
#10403 = ORIENTED_EDGE('',*,*,#7715,.F.) ;
#10404 = ORIENTED_EDGE('',*,*,#7752,.F.) ;
#10405 = ORIENTED_EDGE('',*,*,#7764,.F.) ;
#10406 = ORIENTED_EDGE('',*,*,#7755,.F.) ;
#10407 = ORIENTED_EDGE('',*,*,#7759,.F.) ;
#10408 = ORIENTED_EDGE('',*,*,#7762,.F.) ;
#10409 = ORIENTED_EDGE('',*,*,#7698,.F.) ;
#10410 = ORIENTED_EDGE('',*,*,#7704,.F.) ;
#10411 = ORIENTED_EDGE('',*,*,#7710,.F.) ;
#10412 = ORIENTED_EDGE('',*,*,#7716,.F.) ;
#10413 = ORIENTED_EDGE('',*,*,#7721,.F.) ;
#10414 = ORIENTED_EDGE('',*,*,#7725,.F.) ;
#10415 = ORIENTED_EDGE('',*,*,#7729,.F.) ;
#10416 = ORIENTED_EDGE('',*,*,#7733,.F.) ;
#10417 = ORIENTED_EDGE('',*,*,#7737,.F.) ;
#10418 = ORIENTED_EDGE('',*,*,#7741,.F.) ;
#10419 = ORIENTED_EDGE('',*,*,#7745,.F.) ;
#10420 = ORIENTED_EDGE('',*,*,#7749,.F.) ;
#10421 = ORIENTED_EDGE('',*,*,#7750,.F.) ;
#10422 = ORIENTED_EDGE('',*,*,#7765,.T.) ;
#10423 = ORIENTED_EDGE('',*,*,#7766,.F.) ;
#10424 = ORIENTED_EDGE('',*,*,#7765,.F.) ;
#10425 = ORIENTED_EDGE('',*,*,#7767,.F.) ;
#10426 = ORIENTED_EDGE('',*,*,#7768,.T.) ;
#10427 = ORIENTED_EDGE('',*,*,#7766,.T.) ;
#10428 = ORIENTED_EDGE('',*,*,#7768,.F.) ;
#10429 = ORIENTED_EDGE('',*,*,#7769,.T.) ;
#10430 = ORIENTED_EDGE('',*,*,#7770,.F.) ;
#10431 = ORIENTED_EDGE('',*,*,#7769,.F.) ;
#10432 = ORIENTED_EDGE('',*,*,#7771,.F.) ;
#10433 = ORIENTED_EDGE('',*,*,#7772,.T.) ;
#10434 = ORIENTED_EDGE('',*,*,#7770,.T.) ;
#10435 = ORIENTED_EDGE('',*,*,#7772,.F.) ;
#10436 = ORIENTED_EDGE('',*,*,#7773,.T.) ;
#10437 = ORIENTED_EDGE('',*,*,#7774,.F.) ;
#10438 = ORIENTED_EDGE('',*,*,#7773,.F.) ;
#10439 = ORIENTED_EDGE('',*,*,#7775,.F.) ;
#10440 = ORIENTED_EDGE('',*,*,#7776,.T.) ;
#10441 = ORIENTED_EDGE('',*,*,#7774,.T.) ;
#10442 = ORIENTED_EDGE('',*,*,#7776,.F.) ;
#10443 = ORIENTED_EDGE('',*,*,#7777,.T.) ;
#10444 = ORIENTED_EDGE('',*,*,#7778,.F.) ;
#10445 = ORIENTED_EDGE('',*,*,#7777,.F.) ;
#10446 = ORIENTED_EDGE('',*,*,#7779,.F.) ;
#10447 = ORIENTED_EDGE('',*,*,#7780,.T.) ;
#10448 = ORIENTED_EDGE('',*,*,#7778,.T.) ;
#10449 = ORIENTED_EDGE('',*,*,#7780,.F.) ;
#10450 = ORIENTED_EDGE('',*,*,#7781,.T.) ;
#10451 = ORIENTED_EDGE('',*,*,#7782,.F.) ;
#10452 = ORIENTED_EDGE('',*,*,#7781,.F.) ;
#10453 = ORIENTED_EDGE('',*,*,#7783,.F.) ;
#10454 = ORIENTED_EDGE('',*,*,#7784,.T.) ;
#10455 = ORIENTED_EDGE('',*,*,#7782,.T.) ;
#10456 = ORIENTED_EDGE('',*,*,#7784,.F.) ;
#10457 = ORIENTED_EDGE('',*,*,#7785,.T.) ;
#10458 = ORIENTED_EDGE('',*,*,#7786,.F.) ;
#10459 = ORIENTED_EDGE('',*,*,#7785,.F.) ;
#10460 = ORIENTED_EDGE('',*,*,#7787,.F.) ;
#10461 = ORIENTED_EDGE('',*,*,#7788,.T.) ;
#10462 = ORIENTED_EDGE('',*,*,#7786,.T.) ;
#10463 = ORIENTED_EDGE('',*,*,#7788,.F.) ;
#10464 = ORIENTED_EDGE('',*,*,#7789,.T.) ;
#10465 = ORIENTED_EDGE('',*,*,#7790,.T.) ;
#10466 = ORIENTED_EDGE('',*,*,#7791,.T.) ;
#10467 = ORIENTED_EDGE('',*,*,#7792,.T.) ;
#10468 = ORIENTED_EDGE('',*,*,#7783,.T.) ;
#10469 = ORIENTED_EDGE('',*,*,#7787,.T.) ;
#10470 = ORIENTED_EDGE('',*,*,#7793,.T.) ;
#10471 = ORIENTED_EDGE('',*,*,#7794,.T.) ;
#10472 = ORIENTED_EDGE('',*,*,#7793,.F.) ;
#10473 = ORIENTED_EDGE('',*,*,#7794,.F.) ;
#10474 = ORIENTED_EDGE('',*,*,#7795,.T.) ;
#10475 = ORIENTED_EDGE('',*,*,#7796,.T.) ;
#10476 = ORIENTED_EDGE('',*,*,#7795,.F.) ;
#10477 = ORIENTED_EDGE('',*,*,#7797,.T.) ;
#10478 = ORIENTED_EDGE('',*,*,#7798,.T.) ;
#10479 = ORIENTED_EDGE('',*,*,#7797,.F.) ;
#10480 = ORIENTED_EDGE('',*,*,#7798,.F.) ;
#10481 = ORIENTED_EDGE('',*,*,#7799,.T.) ;
#10482 = ORIENTED_EDGE('',*,*,#7800,.T.) ;
#10483 = ORIENTED_EDGE('',*,*,#7799,.F.) ;
#10484 = ORIENTED_EDGE('',*,*,#7801,.T.) ;
#10485 = ORIENTED_EDGE('',*,*,#7802,.T.) ;
#10486 = ORIENTED_EDGE('',*,*,#7790,.F.) ;
#10487 = ORIENTED_EDGE('',*,*,#7803,.F.) ;
#10488 = ORIENTED_EDGE('',*,*,#7804,.T.) ;
#10489 = ORIENTED_EDGE('',*,*,#7805,.T.) ;
#10490 = ORIENTED_EDGE('',*,*,#7791,.F.) ;
#10491 = ORIENTED_EDGE('',*,*,#7802,.F.) ;
#10492 = ORIENTED_EDGE('',*,*,#7767,.T.) ;
#10493 = ORIENTED_EDGE('',*,*,#7771,.T.) ;
#10494 = ORIENTED_EDGE('',*,*,#7806,.T.) ;
#10495 = ORIENTED_EDGE('',*,*,#7807,.T.) ;
#10496 = ORIENTED_EDGE('',*,*,#7792,.F.) ;
#10497 = ORIENTED_EDGE('',*,*,#7805,.F.) ;
#10498 = ORIENTED_EDGE('',*,*,#7808,.T.) ;
#10499 = ORIENTED_EDGE('',*,*,#7803,.T.) ;
#10500 = ORIENTED_EDGE('',*,*,#7789,.F.) ;
#10501 = ORIENTED_EDGE('',*,*,#7807,.F.) ;
#10502 = ORIENTED_EDGE('',*,*,#7775,.T.) ;
#10503 = ORIENTED_EDGE('',*,*,#7779,.T.) ;
#10504 = ORIENTED_EDGE('',*,*,#7808,.F.) ;
#10505 = ORIENTED_EDGE('',*,*,#7806,.F.) ;
#10506 = ORIENTED_EDGE('',*,*,#7804,.F.) ;
#10507 = ORIENTED_EDGE('',*,*,#7801,.F.) ;
#10508 = ORIENTED_EDGE('',*,*,#7796,.F.) ;
#10509 = ORIENTED_EDGE('',*,*,#7800,.F.) ;
#10510 = ORIENTED_EDGE('',*,*,#7809,.F.) ;
#10511 = ORIENTED_EDGE('',*,*,#7810,.T.) ;
#10512 = ORIENTED_EDGE('',*,*,#7811,.T.) ;
#10513 = ORIENTED_EDGE('',*,*,#7812,.T.) ;
#10514 = ORIENTED_EDGE('',*,*,#7813,.F.) ;
#10515 = ORIENTED_EDGE('',*,*,#7814,.T.) ;
#10516 = ORIENTED_EDGE('',*,*,#7809,.T.) ;
#10517 = ORIENTED_EDGE('',*,*,#7815,.T.) ;
#10518 = ORIENTED_EDGE('',*,*,#7816,.F.) ;
#10519 = ORIENTED_EDGE('',*,*,#7817,.T.) ;
#10520 = ORIENTED_EDGE('',*,*,#7813,.T.) ;
#10521 = ORIENTED_EDGE('',*,*,#7818,.T.) ;
#10522 = ORIENTED_EDGE('',*,*,#7819,.F.) ;
#10523 = ORIENTED_EDGE('',*,*,#7820,.T.) ;
#10524 = ORIENTED_EDGE('',*,*,#7816,.T.) ;
#10525 = ORIENTED_EDGE('',*,*,#7821,.T.) ;
#10526 = ORIENTED_EDGE('',*,*,#7822,.F.) ;
#10527 = ORIENTED_EDGE('',*,*,#7823,.T.) ;
#10528 = ORIENTED_EDGE('',*,*,#7819,.T.) ;
#10529 = ORIENTED_EDGE('',*,*,#7824,.T.) ;
#10530 = ORIENTED_EDGE('',*,*,#7825,.F.) ;
#10531 = ORIENTED_EDGE('',*,*,#7826,.T.) ;
#10532 = ORIENTED_EDGE('',*,*,#7822,.T.) ;
#10533 = ORIENTED_EDGE('',*,*,#7827,.T.) ;
#10534 = ORIENTED_EDGE('',*,*,#7828,.F.) ;
#10535 = ORIENTED_EDGE('',*,*,#7829,.T.) ;
#10536 = ORIENTED_EDGE('',*,*,#7825,.T.) ;
#10537 = ORIENTED_EDGE('',*,*,#7830,.T.) ;
#10538 = ORIENTED_EDGE('',*,*,#7831,.F.) ;
#10539 = ORIENTED_EDGE('',*,*,#7832,.T.) ;
#10540 = ORIENTED_EDGE('',*,*,#7828,.T.) ;
#10541 = ORIENTED_EDGE('',*,*,#7833,.T.) ;
#10542 = ORIENTED_EDGE('',*,*,#7834,.F.) ;
#10543 = ORIENTED_EDGE('',*,*,#7835,.T.) ;
#10544 = ORIENTED_EDGE('',*,*,#7831,.T.) ;
#10545 = ORIENTED_EDGE('',*,*,#7836,.T.) ;
#10546 = ORIENTED_EDGE('',*,*,#7837,.F.) ;
#10547 = ORIENTED_EDGE('',*,*,#7838,.T.) ;
#10548 = ORIENTED_EDGE('',*,*,#7834,.T.) ;
#10549 = ORIENTED_EDGE('',*,*,#7839,.T.) ;
#10550 = ORIENTED_EDGE('',*,*,#7840,.F.) ;
#10551 = ORIENTED_EDGE('',*,*,#7841,.T.) ;
#10552 = ORIENTED_EDGE('',*,*,#7837,.T.) ;
#10553 = ORIENTED_EDGE('',*,*,#7842,.T.) ;
#10554 = ORIENTED_EDGE('',*,*,#7843,.F.) ;
#10555 = ORIENTED_EDGE('',*,*,#7844,.T.) ;
#10556 = ORIENTED_EDGE('',*,*,#7840,.T.) ;
#10557 = ORIENTED_EDGE('',*,*,#7845,.T.) ;
#10558 = ORIENTED_EDGE('',*,*,#7846,.F.) ;
#10559 = ORIENTED_EDGE('',*,*,#7847,.T.) ;
#10560 = ORIENTED_EDGE('',*,*,#7843,.T.) ;
#10561 = ORIENTED_EDGE('',*,*,#7848,.T.) ;
#10562 = ORIENTED_EDGE('',*,*,#7849,.F.) ;
#10563 = ORIENTED_EDGE('',*,*,#7850,.T.) ;
#10564 = ORIENTED_EDGE('',*,*,#7851,.T.) ;
#10565 = ORIENTED_EDGE('',*,*,#7852,.T.) ;
#10566 = ORIENTED_EDGE('',*,*,#7853,.F.) ;
#10567 = ORIENTED_EDGE('',*,*,#7854,.T.) ;
#10568 = ORIENTED_EDGE('',*,*,#7849,.T.) ;
#10569 = ORIENTED_EDGE('',*,*,#7855,.T.) ;
#10570 = ORIENTED_EDGE('',*,*,#7856,.F.) ;
#10571 = ORIENTED_EDGE('',*,*,#7857,.T.) ;
#10572 = ORIENTED_EDGE('',*,*,#7853,.T.) ;
#10573 = ORIENTED_EDGE('',*,*,#7858,.T.) ;
#10574 = ORIENTED_EDGE('',*,*,#7859,.F.) ;
#10575 = ORIENTED_EDGE('',*,*,#7860,.T.) ;
#10576 = ORIENTED_EDGE('',*,*,#7856,.T.) ;
#10577 = ORIENTED_EDGE('',*,*,#7861,.T.) ;
#10578 = ORIENTED_EDGE('',*,*,#7862,.F.) ;
#10579 = ORIENTED_EDGE('',*,*,#7863,.T.) ;
#10580 = ORIENTED_EDGE('',*,*,#7859,.T.) ;
#10581 = ORIENTED_EDGE('',*,*,#7864,.T.) ;
#10582 = ORIENTED_EDGE('',*,*,#7865,.F.) ;
#10583 = ORIENTED_EDGE('',*,*,#7866,.T.) ;
#10584 = ORIENTED_EDGE('',*,*,#7862,.T.) ;
#10585 = ORIENTED_EDGE('',*,*,#7867,.T.) ;
#10586 = ORIENTED_EDGE('',*,*,#7868,.F.) ;
#10587 = ORIENTED_EDGE('',*,*,#7869,.F.) ;
#10588 = ORIENTED_EDGE('',*,*,#7870,.T.) ;
#10589 = ORIENTED_EDGE('',*,*,#7865,.T.) ;
#10590 = ORIENTED_EDGE('',*,*,#7871,.T.) ;
#10591 = ORIENTED_EDGE('',*,*,#7872,.F.) ;
#10592 = ORIENTED_EDGE('',*,*,#7873,.F.) ;
#10593 = ORIENTED_EDGE('',*,*,#7874,.F.) ;
#10594 = ORIENTED_EDGE('',*,*,#7875,.T.) ;
#10595 = ORIENTED_EDGE('',*,*,#7876,.F.) ;
#10596 = ORIENTED_EDGE('',*,*,#7877,.F.) ;
#10597 = ORIENTED_EDGE('',*,*,#7872,.T.) ;
#10598 = ORIENTED_EDGE('',*,*,#7878,.T.) ;
#10599 = ORIENTED_EDGE('',*,*,#7879,.F.) ;
#10600 = ORIENTED_EDGE('',*,*,#7880,.F.) ;
#10601 = ORIENTED_EDGE('',*,*,#7876,.T.) ;
#10602 = ORIENTED_EDGE('',*,*,#7881,.T.) ;
#10603 = ORIENTED_EDGE('',*,*,#7882,.F.) ;
#10604 = ORIENTED_EDGE('',*,*,#7883,.F.) ;
#10605 = ORIENTED_EDGE('',*,*,#7879,.T.) ;
#10606 = ORIENTED_EDGE('',*,*,#7884,.T.) ;
#10607 = ORIENTED_EDGE('',*,*,#7885,.F.) ;
#10608 = ORIENTED_EDGE('',*,*,#7886,.F.) ;
#10609 = ORIENTED_EDGE('',*,*,#7882,.T.) ;
#10610 = ORIENTED_EDGE('',*,*,#7887,.T.) ;
#10611 = ORIENTED_EDGE('',*,*,#7888,.F.) ;
#10612 = ORIENTED_EDGE('',*,*,#7889,.F.) ;
#10613 = ORIENTED_EDGE('',*,*,#7885,.T.) ;
#10614 = ORIENTED_EDGE('',*,*,#7890,.T.) ;
#10615 = ORIENTED_EDGE('',*,*,#7891,.F.) ;
#10616 = ORIENTED_EDGE('',*,*,#7892,.F.) ;
#10617 = ORIENTED_EDGE('',*,*,#7893,.F.) ;
#10618 = ORIENTED_EDGE('',*,*,#7894,.T.) ;
#10619 = ORIENTED_EDGE('',*,*,#7895,.F.) ;
#10620 = ORIENTED_EDGE('',*,*,#7891,.T.) ;
#10621 = ORIENTED_EDGE('',*,*,#7896,.T.) ;
#10622 = ORIENTED_EDGE('',*,*,#7897,.F.) ;
#10623 = ORIENTED_EDGE('',*,*,#7898,.F.) ;
#10624 = ORIENTED_EDGE('',*,*,#7899,.F.) ;
#10625 = ORIENTED_EDGE('',*,*,#7897,.T.) ;
#10626 = ORIENTED_EDGE('',*,*,#7900,.T.) ;
#10627 = ORIENTED_EDGE('',*,*,#7901,.F.) ;
#10628 = ORIENTED_EDGE('',*,*,#7902,.F.) ;
#10629 = ORIENTED_EDGE('',*,*,#7898,.T.) ;
#10630 = ORIENTED_EDGE('',*,*,#7903,.T.) ;
#10631 = ORIENTED_EDGE('',*,*,#7904,.T.) ;
#10632 = ORIENTED_EDGE('',*,*,#7905,.F.) ;
#10633 = ORIENTED_EDGE('',*,*,#7906,.F.) ;
#10634 = ORIENTED_EDGE('',*,*,#7901,.T.) ;
#10635 = ORIENTED_EDGE('',*,*,#7907,.T.) ;
#10636 = ORIENTED_EDGE('',*,*,#7908,.F.) ;
#10637 = ORIENTED_EDGE('',*,*,#7909,.F.) ;
#10638 = ORIENTED_EDGE('',*,*,#7905,.T.) ;
#10639 = ORIENTED_EDGE('',*,*,#7910,.T.) ;
#10640 = ORIENTED_EDGE('',*,*,#7911,.F.) ;
#10641 = ORIENTED_EDGE('',*,*,#7912,.F.) ;
#10642 = ORIENTED_EDGE('',*,*,#7908,.T.) ;
#10643 = ORIENTED_EDGE('',*,*,#7913,.T.) ;
#10644 = ORIENTED_EDGE('',*,*,#7914,.F.) ;
#10645 = ORIENTED_EDGE('',*,*,#7915,.F.) ;
#10646 = ORIENTED_EDGE('',*,*,#7911,.T.) ;
#10647 = ORIENTED_EDGE('',*,*,#7916,.T.) ;
#10648 = ORIENTED_EDGE('',*,*,#7917,.F.) ;
#10649 = ORIENTED_EDGE('',*,*,#7918,.F.) ;
#10650 = ORIENTED_EDGE('',*,*,#7919,.F.) ;
#10651 = ORIENTED_EDGE('',*,*,#7914,.T.) ;
#10652 = ORIENTED_EDGE('',*,*,#7920,.T.) ;
#10653 = ORIENTED_EDGE('',*,*,#7921,.T.) ;
#10654 = ORIENTED_EDGE('',*,*,#7922,.F.) ;
#10655 = ORIENTED_EDGE('',*,*,#7923,.F.) ;
#10656 = ORIENTED_EDGE('',*,*,#7917,.T.) ;
#10657 = ORIENTED_EDGE('',*,*,#7924,.T.) ;
#10658 = ORIENTED_EDGE('',*,*,#7925,.F.) ;
#10659 = ORIENTED_EDGE('',*,*,#7926,.F.) ;
#10660 = ORIENTED_EDGE('',*,*,#7922,.T.) ;
#10661 = ORIENTED_EDGE('',*,*,#7927,.T.) ;
#10662 = ORIENTED_EDGE('',*,*,#7928,.T.) ;
#10663 = ORIENTED_EDGE('',*,*,#7929,.F.) ;
#10664 = ORIENTED_EDGE('',*,*,#7930,.F.) ;
#10665 = ORIENTED_EDGE('',*,*,#7925,.T.) ;
#10666 = ORIENTED_EDGE('',*,*,#7931,.T.) ;
#10667 = ORIENTED_EDGE('',*,*,#7932,.F.) ;
#10668 = ORIENTED_EDGE('',*,*,#7933,.F.) ;
#10669 = ORIENTED_EDGE('',*,*,#7929,.T.) ;
#10670 = ORIENTED_EDGE('',*,*,#7934,.T.) ;
#10671 = ORIENTED_EDGE('',*,*,#7932,.T.) ;
#10672 = ORIENTED_EDGE('',*,*,#7935,.T.) ;
#10673 = ORIENTED_EDGE('',*,*,#7936,.F.) ;
#10674 = ORIENTED_EDGE('',*,*,#7937,.F.) ;
#10675 = ORIENTED_EDGE('',*,*,#7888,.T.) ;
#10676 = ORIENTED_EDGE('',*,*,#7938,.T.) ;
#10677 = ORIENTED_EDGE('',*,*,#7939,.F.) ;
#10678 = ORIENTED_EDGE('',*,*,#7940,.F.) ;
#10679 = ORIENTED_EDGE('',*,*,#7868,.T.) ;
#10680 = ORIENTED_EDGE('',*,*,#7941,.T.) ;
#10681 = ORIENTED_EDGE('',*,*,#7942,.F.) ;
#10682 = ORIENTED_EDGE('',*,*,#7846,.T.) ;
#10683 = ORIENTED_EDGE('',*,*,#7943,.T.) ;
#10684 = ORIENTED_EDGE('',*,*,#7944,.F.) ;
#10685 = ORIENTED_EDGE('',*,*,#7945,.T.) ;
#10686 = ORIENTED_EDGE('',*,*,#7946,.T.) ;
#10687 = ORIENTED_EDGE('',*,*,#7947,.T.) ;
#10688 = ORIENTED_EDGE('',*,*,#7948,.T.) ;
#10689 = ORIENTED_EDGE('',*,*,#7947,.F.) ;
#10690 = ORIENTED_EDGE('',*,*,#7949,.T.) ;
#10691 = ORIENTED_EDGE('',*,*,#7950,.F.) ;
#10692 = ORIENTED_EDGE('',*,*,#7948,.F.) ;
#10693 = ORIENTED_EDGE('',*,*,#7951,.F.) ;
#10694 = ORIENTED_EDGE('',*,*,#7952,.T.) ;
#10695 = ORIENTED_EDGE('',*,*,#7949,.F.) ;
#10696 = ORIENTED_EDGE('',*,*,#7946,.F.) ;
#10697 = ORIENTED_EDGE('',*,*,#7952,.F.) ;
#10698 = ORIENTED_EDGE('',*,*,#7953,.T.) ;
#10699 = ORIENTED_EDGE('',*,*,#7954,.T.) ;
#10700 = ORIENTED_EDGE('',*,*,#7950,.T.) ;
#10701 = ORIENTED_EDGE('',*,*,#7954,.F.) ;
#10702 = ORIENTED_EDGE('',*,*,#7955,.T.) ;
#10703 = ORIENTED_EDGE('',*,*,#7953,.F.) ;
#10704 = ORIENTED_EDGE('',*,*,#7956,.T.) ;
#10705 = ORIENTED_EDGE('',*,*,#7957,.T.) ;
#10706 = ORIENTED_EDGE('',*,*,#7956,.F.) ;
#10707 = ORIENTED_EDGE('',*,*,#7955,.F.) ;
#10708 = ORIENTED_EDGE('',*,*,#7958,.T.) ;
#10709 = ORIENTED_EDGE('',*,*,#7959,.T.) ;
#10710 = ORIENTED_EDGE('',*,*,#7960,.T.) ;
#10711 = ORIENTED_EDGE('',*,*,#7959,.F.) ;
#10712 = ORIENTED_EDGE('',*,*,#7961,.T.) ;
#10713 = ORIENTED_EDGE('',*,*,#7958,.F.) ;
#10714 = ORIENTED_EDGE('',*,*,#7962,.T.) ;
#10715 = ORIENTED_EDGE('',*,*,#7963,.T.) ;
#10716 = ORIENTED_EDGE('',*,*,#7962,.F.) ;
#10717 = ORIENTED_EDGE('',*,*,#7961,.F.) ;
#10718 = ORIENTED_EDGE('',*,*,#7964,.T.) ;
#10719 = ORIENTED_EDGE('',*,*,#7965,.T.) ;
#10720 = ORIENTED_EDGE('',*,*,#7966,.T.) ;
#10721 = ORIENTED_EDGE('',*,*,#7967,.T.) ;
#10722 = ORIENTED_EDGE('',*,*,#7960,.F.) ;
#10723 = ORIENTED_EDGE('',*,*,#7968,.F.) ;
#10724 = ORIENTED_EDGE('',*,*,#7969,.T.) ;
#10725 = ORIENTED_EDGE('',*,*,#7970,.T.) ;
#10726 = ORIENTED_EDGE('',*,*,#7971,.T.) ;
#10727 = ORIENTED_EDGE('',*,*,#7970,.F.) ;
#10728 = ORIENTED_EDGE('',*,*,#7972,.T.) ;
#10729 = ORIENTED_EDGE('',*,*,#7969,.F.) ;
#10730 = ORIENTED_EDGE('',*,*,#7973,.T.) ;
#10731 = ORIENTED_EDGE('',*,*,#7974,.T.) ;
#10732 = ORIENTED_EDGE('',*,*,#7973,.F.) ;
#10733 = ORIENTED_EDGE('',*,*,#7972,.F.) ;
#10734 = ORIENTED_EDGE('',*,*,#7971,.F.) ;
#10735 = ORIENTED_EDGE('',*,*,#7963,.F.) ;
#10736 = ORIENTED_EDGE('',*,*,#7975,.T.) ;
#10737 = ORIENTED_EDGE('',*,*,#7976,.T.) ;
#10738 = ORIENTED_EDGE('',*,*,#7977,.T.) ;
#10739 = ORIENTED_EDGE('',*,*,#7978,.T.) ;
#10740 = ORIENTED_EDGE('',*,*,#7976,.F.) ;
#10741 = ORIENTED_EDGE('',*,*,#7979,.T.) ;
#10742 = ORIENTED_EDGE('',*,*,#7975,.F.) ;
#10743 = ORIENTED_EDGE('',*,*,#7980,.T.) ;
#10744 = ORIENTED_EDGE('',*,*,#7981,.F.) ;
#10745 = ORIENTED_EDGE('',*,*,#7982,.F.) ;
#10746 = ORIENTED_EDGE('',*,*,#7980,.F.) ;
#10747 = ORIENTED_EDGE('',*,*,#7979,.F.) ;
#10748 = ORIENTED_EDGE('',*,*,#7978,.F.) ;
#10749 = ORIENTED_EDGE('',*,*,#7983,.T.) ;
#10750 = ORIENTED_EDGE('',*,*,#7984,.F.) ;
#10751 = ORIENTED_EDGE('',*,*,#7983,.F.) ;
#10752 = ORIENTED_EDGE('',*,*,#7977,.F.) ;
#10753 = ORIENTED_EDGE('',*,*,#7981,.T.) ;
#10754 = ORIENTED_EDGE('',*,*,#7982,.T.) ;
#10755 = ORIENTED_EDGE('',*,*,#7985,.T.) ;
#10756 = ORIENTED_EDGE('',*,*,#7986,.T.) ;
#10757 = ORIENTED_EDGE('',*,*,#7985,.F.) ;
#10758 = ORIENTED_EDGE('',*,*,#7986,.F.) ;
#10759 = ORIENTED_EDGE('',*,*,#7987,.T.) ;
#10760 = ORIENTED_EDGE('',*,*,#7988,.T.) ;
#10761 = ORIENTED_EDGE('',*,*,#7989,.T.) ;
#10762 = ORIENTED_EDGE('',*,*,#7990,.T.) ;
#10763 = ORIENTED_EDGE('',*,*,#7989,.F.) ;
#10764 = ORIENTED_EDGE('',*,*,#7991,.T.) ;
#10765 = ORIENTED_EDGE('',*,*,#7951,.T.) ;
#10766 = ORIENTED_EDGE('',*,*,#7992,.T.) ;
#10767 = ORIENTED_EDGE('',*,*,#7991,.F.) ;
#10768 = ORIENTED_EDGE('',*,*,#7988,.F.) ;
#10769 = ORIENTED_EDGE('',*,*,#7992,.F.) ;
#10770 = ORIENTED_EDGE('',*,*,#7993,.T.) ;
#10771 = ORIENTED_EDGE('',*,*,#7851,.F.) ;
#10772 = ORIENTED_EDGE('',*,*,#7994,.T.) ;
#10773 = ORIENTED_EDGE('',*,*,#7874,.T.) ;
#10774 = ORIENTED_EDGE('',*,*,#7990,.F.) ;
#10775 = ORIENTED_EDGE('',*,*,#7995,.T.) ;
#10776 = ORIENTED_EDGE('',*,*,#7996,.T.) ;
#10777 = ORIENTED_EDGE('',*,*,#7997,.T.) ;
#10778 = ORIENTED_EDGE('',*,*,#7996,.F.) ;
#10779 = ORIENTED_EDGE('',*,*,#7998,.T.) ;
#10780 = ORIENTED_EDGE('',*,*,#7995,.F.) ;
#10781 = ORIENTED_EDGE('',*,*,#7999,.T.) ;
#10782 = ORIENTED_EDGE('',*,*,#8000,.F.) ;
#10783 = ORIENTED_EDGE('',*,*,#8001,.F.) ;
#10784 = ORIENTED_EDGE('',*,*,#7999,.F.) ;
#10785 = ORIENTED_EDGE('',*,*,#7998,.F.) ;
#10786 = ORIENTED_EDGE('',*,*,#8002,.T.) ;
#10787 = ORIENTED_EDGE('',*,*,#8003,.T.) ;
#10788 = ORIENTED_EDGE('',*,*,#8004,.T.) ;
#10789 = ORIENTED_EDGE('',*,*,#7997,.F.) ;
#10790 = ORIENTED_EDGE('',*,*,#8005,.F.) ;
#10791 = ORIENTED_EDGE('',*,*,#8000,.T.) ;
#10792 = ORIENTED_EDGE('',*,*,#8001,.T.) ;
#10793 = ORIENTED_EDGE('',*,*,#8006,.T.) ;
#10794 = ORIENTED_EDGE('',*,*,#8007,.T.) ;
#10795 = ORIENTED_EDGE('',*,*,#8006,.F.) ;
#10796 = ORIENTED_EDGE('',*,*,#8007,.F.) ;
#10797 = ORIENTED_EDGE('',*,*,#8008,.T.) ;
#10798 = ORIENTED_EDGE('',*,*,#8002,.F.) ;
#10799 = ORIENTED_EDGE('',*,*,#8009,.T.) ;
#10800 = ORIENTED_EDGE('',*,*,#8010,.T.) ;
#10801 = ORIENTED_EDGE('',*,*,#8009,.F.) ;
#10802 = ORIENTED_EDGE('',*,*,#8010,.F.) ;
#10803 = ORIENTED_EDGE('',*,*,#8003,.F.) ;
#10804 = ORIENTED_EDGE('',*,*,#8011,.T.) ;
#10805 = ORIENTED_EDGE('',*,*,#8012,.T.) ;
#10806 = ORIENTED_EDGE('',*,*,#8011,.F.) ;
#10807 = ORIENTED_EDGE('',*,*,#8012,.F.) ;
#10808 = ORIENTED_EDGE('',*,*,#8004,.F.) ;
#10809 = ORIENTED_EDGE('',*,*,#8013,.T.) ;
#10810 = ORIENTED_EDGE('',*,*,#8014,.T.) ;
#10811 = ORIENTED_EDGE('',*,*,#8013,.F.) ;
#10812 = ORIENTED_EDGE('',*,*,#8014,.F.) ;
#10813 = ORIENTED_EDGE('',*,*,#7899,.T.) ;
#10814 = ORIENTED_EDGE('',*,*,#7902,.T.) ;
#10815 = ORIENTED_EDGE('',*,*,#7906,.T.) ;
#10816 = ORIENTED_EDGE('',*,*,#7909,.T.) ;
#10817 = ORIENTED_EDGE('',*,*,#7912,.T.) ;
#10818 = ORIENTED_EDGE('',*,*,#7915,.T.) ;
#10819 = ORIENTED_EDGE('',*,*,#7919,.T.) ;
#10820 = ORIENTED_EDGE('',*,*,#7918,.T.) ;
#10821 = ORIENTED_EDGE('',*,*,#7923,.T.) ;
#10822 = ORIENTED_EDGE('',*,*,#7926,.T.) ;
#10823 = ORIENTED_EDGE('',*,*,#7930,.T.) ;
#10824 = ORIENTED_EDGE('',*,*,#7933,.T.) ;
#10825 = ORIENTED_EDGE('',*,*,#7937,.T.) ;
#10826 = ORIENTED_EDGE('',*,*,#8015,.F.) ;
#10827 = ORIENTED_EDGE('',*,*,#7943,.F.) ;
#10828 = ORIENTED_EDGE('',*,*,#7848,.F.) ;
#10829 = ORIENTED_EDGE('',*,*,#7845,.F.) ;
#10830 = ORIENTED_EDGE('',*,*,#7842,.F.) ;
#10831 = ORIENTED_EDGE('',*,*,#7839,.F.) ;
#10832 = ORIENTED_EDGE('',*,*,#7836,.F.) ;
#10833 = ORIENTED_EDGE('',*,*,#7833,.F.) ;
#10834 = ORIENTED_EDGE('',*,*,#7830,.F.) ;
#10835 = ORIENTED_EDGE('',*,*,#7827,.F.) ;
#10836 = ORIENTED_EDGE('',*,*,#7824,.F.) ;
#10837 = ORIENTED_EDGE('',*,*,#7821,.F.) ;
#10838 = ORIENTED_EDGE('',*,*,#7818,.F.) ;
#10839 = ORIENTED_EDGE('',*,*,#7815,.F.) ;
#10840 = ORIENTED_EDGE('',*,*,#7812,.F.) ;
#10841 = ORIENTED_EDGE('',*,*,#8016,.F.) ;
#10842 = ORIENTED_EDGE('',*,*,#8017,.T.) ;
#10843 = ORIENTED_EDGE('',*,*,#7892,.T.) ;
#10844 = ORIENTED_EDGE('',*,*,#7895,.T.) ;
#10845 = ORIENTED_EDGE('',*,*,#8018,.F.) ;
#10846 = ORIENTED_EDGE('',*,*,#8019,.F.) ;
#10847 = ORIENTED_EDGE('',*,*,#7935,.F.) ;
#10848 = ORIENTED_EDGE('',*,*,#7934,.F.) ;
#10849 = ORIENTED_EDGE('',*,*,#7931,.F.) ;
#10850 = ORIENTED_EDGE('',*,*,#7928,.F.) ;
#10851 = ORIENTED_EDGE('',*,*,#7927,.F.) ;
#10852 = ORIENTED_EDGE('',*,*,#7924,.F.) ;
#10853 = ORIENTED_EDGE('',*,*,#7921,.F.) ;
#10854 = ORIENTED_EDGE('',*,*,#7920,.F.) ;
#10855 = ORIENTED_EDGE('',*,*,#7916,.F.) ;
#10856 = ORIENTED_EDGE('',*,*,#7913,.F.) ;
#10857 = ORIENTED_EDGE('',*,*,#7910,.F.) ;
#10858 = ORIENTED_EDGE('',*,*,#7907,.F.) ;
#10859 = ORIENTED_EDGE('',*,*,#7904,.F.) ;
#10860 = ORIENTED_EDGE('',*,*,#7903,.F.) ;
#10861 = ORIENTED_EDGE('',*,*,#7900,.F.) ;
#10862 = ORIENTED_EDGE('',*,*,#7896,.F.) ;
#10863 = ORIENTED_EDGE('',*,*,#7894,.F.) ;
#10864 = ORIENTED_EDGE('',*,*,#8020,.F.) ;
#10865 = ORIENTED_EDGE('',*,*,#7810,.F.) ;
#10866 = ORIENTED_EDGE('',*,*,#7814,.F.) ;
#10867 = ORIENTED_EDGE('',*,*,#7817,.F.) ;
#10868 = ORIENTED_EDGE('',*,*,#7820,.F.) ;
#10869 = ORIENTED_EDGE('',*,*,#7823,.F.) ;
#10870 = ORIENTED_EDGE('',*,*,#7826,.F.) ;
#10871 = ORIENTED_EDGE('',*,*,#7829,.F.) ;
#10872 = ORIENTED_EDGE('',*,*,#7832,.F.) ;
#10873 = ORIENTED_EDGE('',*,*,#7835,.F.) ;
#10874 = ORIENTED_EDGE('',*,*,#7838,.F.) ;
#10875 = ORIENTED_EDGE('',*,*,#7841,.F.) ;
#10876 = ORIENTED_EDGE('',*,*,#7844,.F.) ;
#10877 = ORIENTED_EDGE('',*,*,#7847,.F.) ;
#10878 = ORIENTED_EDGE('',*,*,#7945,.F.) ;
#10879 = ORIENTED_EDGE('',*,*,#8015,.T.) ;
#10880 = ORIENTED_EDGE('',*,*,#7936,.T.) ;
#10881 = ORIENTED_EDGE('',*,*,#8019,.T.) ;
#10882 = ORIENTED_EDGE('',*,*,#8018,.T.) ;
#10883 = ORIENTED_EDGE('',*,*,#7944,.T.) ;
#10884 = ORIENTED_EDGE('',*,*,#7957,.F.) ;
#10885 = ORIENTED_EDGE('',*,*,#8021,.F.) ;
#10886 = ORIENTED_EDGE('',*,*,#7941,.F.) ;
#10887 = ORIENTED_EDGE('',*,*,#7871,.F.) ;
#10888 = ORIENTED_EDGE('',*,*,#7867,.F.) ;
#10889 = ORIENTED_EDGE('',*,*,#7864,.F.) ;
#10890 = ORIENTED_EDGE('',*,*,#7861,.F.) ;
#10891 = ORIENTED_EDGE('',*,*,#7858,.F.) ;
#10892 = ORIENTED_EDGE('',*,*,#7855,.F.) ;
#10893 = ORIENTED_EDGE('',*,*,#7852,.F.) ;
#10894 = ORIENTED_EDGE('',*,*,#7993,.F.) ;
#10895 = ORIENTED_EDGE('',*,*,#7873,.T.) ;
#10896 = ORIENTED_EDGE('',*,*,#7877,.T.) ;
#10897 = ORIENTED_EDGE('',*,*,#7880,.T.) ;
#10898 = ORIENTED_EDGE('',*,*,#7883,.T.) ;
#10899 = ORIENTED_EDGE('',*,*,#7886,.T.) ;
#10900 = ORIENTED_EDGE('',*,*,#7889,.T.) ;
#10901 = ORIENTED_EDGE('',*,*,#7940,.T.) ;
#10902 = ORIENTED_EDGE('',*,*,#8022,.F.) ;
#10903 = ORIENTED_EDGE('',*,*,#8023,.F.) ;
#10904 = ORIENTED_EDGE('',*,*,#7938,.F.) ;
#10905 = ORIENTED_EDGE('',*,*,#7890,.F.) ;
#10906 = ORIENTED_EDGE('',*,*,#7887,.F.) ;
#10907 = ORIENTED_EDGE('',*,*,#7884,.F.) ;
#10908 = ORIENTED_EDGE('',*,*,#7881,.F.) ;
#10909 = ORIENTED_EDGE('',*,*,#7878,.F.) ;
#10910 = ORIENTED_EDGE('',*,*,#7875,.F.) ;
#10911 = ORIENTED_EDGE('',*,*,#7994,.F.) ;
#10912 = ORIENTED_EDGE('',*,*,#7850,.F.) ;
#10913 = ORIENTED_EDGE('',*,*,#7854,.F.) ;
#10914 = ORIENTED_EDGE('',*,*,#7857,.F.) ;
#10915 = ORIENTED_EDGE('',*,*,#7860,.F.) ;
#10916 = ORIENTED_EDGE('',*,*,#7863,.F.) ;
#10917 = ORIENTED_EDGE('',*,*,#7866,.F.) ;
#10918 = ORIENTED_EDGE('',*,*,#7870,.F.) ;
#10919 = ORIENTED_EDGE('',*,*,#8021,.T.) ;
#10920 = ORIENTED_EDGE('',*,*,#7939,.T.) ;
#10921 = ORIENTED_EDGE('',*,*,#8023,.T.) ;
#10922 = ORIENTED_EDGE('',*,*,#8022,.T.) ;
#10923 = ORIENTED_EDGE('',*,*,#7869,.T.) ;
#10924 = ORIENTED_EDGE('',*,*,#7942,.T.) ;
#10925 = ORIENTED_EDGE('',*,*,#8024,.F.) ;
#10926 = ORIENTED_EDGE('',*,*,#7964,.F.) ;
#10927 = ORIENTED_EDGE('',*,*,#8025,.F.) ;
#10928 = ORIENTED_EDGE('',*,*,#8026,.F.) ;
#10929 = ORIENTED_EDGE('',*,*,#8027,.T.) ;
#10930 = ORIENTED_EDGE('',*,*,#7965,.F.) ;
#10931 = ORIENTED_EDGE('',*,*,#8027,.F.) ;
#10932 = ORIENTED_EDGE('',*,*,#8028,.F.) ;
#10933 = ORIENTED_EDGE('',*,*,#8029,.T.) ;
#10934 = ORIENTED_EDGE('',*,*,#7966,.F.) ;
#10935 = ORIENTED_EDGE('',*,*,#8029,.F.) ;
#10936 = ORIENTED_EDGE('',*,*,#8030,.F.) ;
#10937 = ORIENTED_EDGE('',*,*,#8031,.T.) ;
#10938 = ORIENTED_EDGE('',*,*,#7967,.F.) ;
#10939 = ORIENTED_EDGE('',*,*,#8031,.F.) ;
#10940 = ORIENTED_EDGE('',*,*,#8032,.F.) ;
#10941 = ORIENTED_EDGE('',*,*,#8025,.T.) ;
#10942 = ORIENTED_EDGE('',*,*,#8028,.T.) ;
#10943 = ORIENTED_EDGE('',*,*,#8026,.T.) ;
#10944 = ORIENTED_EDGE('',*,*,#8032,.T.) ;
#10945 = ORIENTED_EDGE('',*,*,#8030,.T.) ;
#10946 = ORIENTED_EDGE('',*,*,#8033,.F.) ;
#10947 = ORIENTED_EDGE('',*,*,#8034,.T.) ;
#10948 = ORIENTED_EDGE('',*,*,#8024,.T.) ;
#10949 = ORIENTED_EDGE('',*,*,#8034,.F.) ;
#10950 = ORIENTED_EDGE('',*,*,#8035,.F.) ;
#10951 = ORIENTED_EDGE('',*,*,#8033,.T.) ;
#10952 = ORIENTED_EDGE('',*,*,#7987,.F.) ;
#10953 = ORIENTED_EDGE('',*,*,#8036,.T.) ;
#10954 = ORIENTED_EDGE('',*,*,#8035,.T.) ;
#10955 = ORIENTED_EDGE('',*,*,#8036,.F.) ;
#10956 = ORIENTED_EDGE('',*,*,#8008,.F.) ;
#10957 = ORIENTED_EDGE('',*,*,#8037,.T.) ;
#10958 = ORIENTED_EDGE('',*,*,#7984,.T.) ;
#10959 = ORIENTED_EDGE('',*,*,#8037,.F.) ;
#10960 = ORIENTED_EDGE('',*,*,#8038,.F.) ;
#10961 = ORIENTED_EDGE('',*,*,#8039,.T.) ;
#10962 = ORIENTED_EDGE('',*,*,#8005,.T.) ;
#10963 = ORIENTED_EDGE('',*,*,#8039,.F.) ;
#10964 = ORIENTED_EDGE('',*,*,#8038,.T.) ;
#10965 = ORIENTED_EDGE('',*,*,#8040,.F.) ;
#10966 = ORIENTED_EDGE('',*,*,#8041,.F.) ;
#10967 = ORIENTED_EDGE('',*,*,#8042,.T.) ;
#10968 = ORIENTED_EDGE('',*,*,#8040,.T.) ;
#10969 = ORIENTED_EDGE('',*,*,#8042,.F.) ;
#10970 = ORIENTED_EDGE('',*,*,#7974,.F.) ;
#10971 = ORIENTED_EDGE('',*,*,#8041,.T.) ;
#10972 = ORIENTED_EDGE('',*,*,#8043,.F.) ;
#10973 = ORIENTED_EDGE('',*,*,#8044,.T.) ;
#10974 = ORIENTED_EDGE('',*,*,#7968,.T.) ;
#10975 = ORIENTED_EDGE('',*,*,#8044,.F.) ;
#10976 = ORIENTED_EDGE('',*,*,#8016,.T.) ;
#10977 = ORIENTED_EDGE('',*,*,#7811,.F.) ;
#10978 = ORIENTED_EDGE('',*,*,#8020,.T.) ;
#10979 = ORIENTED_EDGE('',*,*,#7893,.T.) ;
#10980 = ORIENTED_EDGE('',*,*,#8017,.F.) ;
#10981 = ORIENTED_EDGE('',*,*,#8043,.T.) ;
#10982 = ORIENTED_EDGE('',*,*,#8045,.T.) ;
#10983 = ORIENTED_EDGE('',*,*,#8046,.T.) ;
#10984 = ORIENTED_EDGE('',*,*,#8047,.F.) ;
#10985 = ORIENTED_EDGE('',*,*,#8048,.T.) ;
#10986 = ORIENTED_EDGE('',*,*,#8049,.F.) ;
#10987 = ORIENTED_EDGE('',*,*,#8050,.T.) ;
#10988 = ORIENTED_EDGE('',*,*,#8051,.T.) ;
#10989 = ORIENTED_EDGE('',*,*,#8052,.T.) ;
#10990 = ORIENTED_EDGE('',*,*,#8047,.T.) ;
#10991 = ORIENTED_EDGE('',*,*,#8053,.F.) ;
#10992 = ORIENTED_EDGE('',*,*,#8054,.F.) ;
#10993 = ORIENTED_EDGE('',*,*,#8055,.T.) ;
#10994 = ORIENTED_EDGE('',*,*,#8056,.F.) ;
#10995 = ORIENTED_EDGE('',*,*,#8057,.T.) ;
#10996 = ORIENTED_EDGE('',*,*,#8058,.F.) ;
#10997 = ORIENTED_EDGE('',*,*,#8059,.T.) ;
#10998 = ORIENTED_EDGE('',*,*,#8054,.T.) ;
#10999 = ORIENTED_EDGE('',*,*,#8060,.T.) ;
#11000 = ORIENTED_EDGE('',*,*,#8061,.T.) ;
#11001 = ORIENTED_EDGE('',*,*,#8062,.T.) ;
#11002 = ORIENTED_EDGE('',*,*,#8051,.F.) ;
#11003 = ORIENTED_EDGE('',*,*,#8063,.F.) ;
#11004 = ORIENTED_EDGE('',*,*,#8056,.T.) ;
#11005 = ORIENTED_EDGE('',*,*,#8064,.T.) ;
#11006 = ORIENTED_EDGE('',*,*,#8065,.F.) ;
#11007 = ORIENTED_EDGE('',*,*,#8049,.T.) ;
#11008 = ORIENTED_EDGE('',*,*,#8066,.F.) ;
#11009 = ORIENTED_EDGE('',*,*,#8058,.T.) ;
#11010 = ORIENTED_EDGE('',*,*,#8045,.F.) ;
#11011 = ORIENTED_EDGE('',*,*,#8067,.T.) ;
#11012 = ORIENTED_EDGE('',*,*,#8061,.F.) ;
#11013 = ORIENTED_EDGE('',*,*,#8068,.T.) ;
#11014 = ORIENTED_EDGE('',*,*,#8068,.F.) ;
#11015 = ORIENTED_EDGE('',*,*,#8060,.F.) ;
#11016 = ORIENTED_EDGE('',*,*,#8053,.T.) ;
#11017 = ORIENTED_EDGE('',*,*,#8046,.F.) ;
#11018 = ORIENTED_EDGE('',*,*,#8064,.F.) ;
#11019 = ORIENTED_EDGE('',*,*,#8062,.F.) ;
#11020 = ORIENTED_EDGE('',*,*,#8067,.F.) ;
#11021 = ORIENTED_EDGE('',*,*,#8052,.F.) ;
#11022 = ORIENTED_EDGE('',*,*,#8055,.F.) ;
#11023 = ORIENTED_EDGE('',*,*,#8059,.F.) ;
#11024 = ORIENTED_EDGE('',*,*,#8066,.T.) ;
#11025 = ORIENTED_EDGE('',*,*,#8048,.F.) ;
#11026 = ORIENTED_EDGE('',*,*,#8065,.T.) ;
#11027 = ORIENTED_EDGE('',*,*,#8057,.F.) ;
#11028 = ORIENTED_EDGE('',*,*,#8063,.T.) ;
#11029 = ORIENTED_EDGE('',*,*,#8050,.F.) ;
#11030 = ORIENTED_EDGE('',*,*,#8069,.T.) ;
#11031 = ORIENTED_EDGE('',*,*,#8070,.T.) ;
#11032 = ORIENTED_EDGE('',*,*,#8071,.T.) ;
#11033 = ORIENTED_EDGE('',*,*,#8070,.F.) ;
#11034 = ORIENTED_EDGE('',*,*,#8071,.F.) ;
#11035 = ORIENTED_EDGE('',*,*,#8072,.F.) ;
#11036 = ORIENTED_EDGE('',*,*,#8073,.F.) ;
#11037 = ORIENTED_EDGE('',*,*,#8074,.T.) ;
#11038 = ORIENTED_EDGE('',*,*,#8069,.F.) ;
#11039 = ORIENTED_EDGE('',*,*,#8074,.F.) ;
#11040 = ORIENTED_EDGE('',*,*,#8075,.T.) ;
#11041 = ORIENTED_EDGE('',*,*,#8076,.T.) ;
#11042 = ORIENTED_EDGE('',*,*,#8072,.T.) ;
#11043 = ORIENTED_EDGE('',*,*,#8076,.F.) ;
#11044 = ORIENTED_EDGE('',*,*,#8075,.F.) ;
#11045 = ORIENTED_EDGE('',*,*,#8077,.T.) ;
#11046 = ORIENTED_EDGE('',*,*,#8078,.F.) ;
#11047 = ORIENTED_EDGE('',*,*,#8077,.F.) ;
#11048 = ORIENTED_EDGE('',*,*,#8073,.T.) ;
#11049 = ORIENTED_EDGE('',*,*,#8079,.T.) ;
#11050 = ORIENTED_EDGE('',*,*,#8080,.T.) ;
#11051 = ORIENTED_EDGE('',*,*,#8079,.F.) ;
#11052 = ORIENTED_EDGE('',*,*,#8080,.F.) ;
#11053 = ORIENTED_EDGE('',*,*,#8081,.F.) ;
#11054 = ORIENTED_EDGE('',*,*,#8078,.T.) ;
#11055 = ORIENTED_EDGE('',*,*,#8082,.T.) ;
#11056 = ORIENTED_EDGE('',*,*,#8081,.T.) ;
#11057 = ORIENTED_EDGE('',*,*,#8082,.F.) ;
#11058 = ORIENTED_EDGE('',*,*,#8083,.F.) ;
#11059 = ORIENTED_EDGE('',*,*,#8084,.F.) ;
#11060 = ORIENTED_EDGE('',*,*,#8085,.T.) ;
#11061 = ORIENTED_EDGE('',*,*,#8086,.F.) ;
#11062 = ORIENTED_EDGE('',*,*,#8087,.F.) ;
#11063 = ORIENTED_EDGE('',*,*,#8088,.T.) ;
#11064 = ORIENTED_EDGE('',*,*,#8089,.F.) ;
#11065 = ORIENTED_EDGE('',*,*,#8085,.F.) ;
#11066 = ORIENTED_EDGE('',*,*,#8090,.F.) ;
#11067 = ORIENTED_EDGE('',*,*,#8091,.F.) ;
#11068 = ORIENTED_EDGE('',*,*,#8088,.F.) ;
#11069 = ORIENTED_EDGE('',*,*,#8092,.F.) ;
#11070 = ORIENTED_EDGE('',*,*,#8093,.F.) ;
#11071 = ORIENTED_EDGE('',*,*,#8092,.T.) ;
#11072 = ORIENTED_EDGE('',*,*,#8087,.T.) ;
#11073 = ORIENTED_EDGE('',*,*,#8084,.T.) ;
#11074 = ORIENTED_EDGE('',*,*,#8094,.T.) ;
#11075 = ORIENTED_EDGE('',*,*,#8095,.F.) ;
#11076 = ORIENTED_EDGE('',*,*,#8096,.F.) ;
#11077 = ORIENTED_EDGE('',*,*,#8097,.T.) ;
#11078 = ORIENTED_EDGE('',*,*,#8098,.T.) ;
#11079 = ORIENTED_EDGE('',*,*,#8099,.F.) ;
#11080 = ORIENTED_EDGE('',*,*,#8100,.T.) ;
#11081 = ORIENTED_EDGE('',*,*,#8101,.T.) ;
#11082 = ORIENTED_EDGE('',*,*,#8102,.F.) ;
#11083 = ORIENTED_EDGE('',*,*,#8103,.F.) ;
#11084 = ORIENTED_EDGE('',*,*,#8104,.T.) ;
#11085 = ORIENTED_EDGE('',*,*,#8105,.T.) ;
#11086 = ORIENTED_EDGE('',*,*,#8106,.F.) ;
#11087 = ORIENTED_EDGE('',*,*,#8107,.F.) ;
#11088 = ORIENTED_EDGE('',*,*,#8108,.T.) ;
#11089 = ORIENTED_EDGE('',*,*,#8109,.T.) ;
#11090 = ORIENTED_EDGE('',*,*,#8110,.F.) ;
#11091 = ORIENTED_EDGE('',*,*,#8111,.F.) ;
#11092 = ORIENTED_EDGE('',*,*,#8112,.F.) ;
#11093 = ORIENTED_EDGE('',*,*,#8113,.T.) ;
#11094 = ORIENTED_EDGE('',*,*,#8114,.T.) ;
#11095 = ORIENTED_EDGE('',*,*,#8115,.F.) ;
#11096 = ORIENTED_EDGE('',*,*,#8116,.F.) ;
#11097 = ORIENTED_EDGE('',*,*,#8117,.T.) ;
#11098 = ORIENTED_EDGE('',*,*,#8118,.T.) ;
#11099 = ORIENTED_EDGE('',*,*,#8119,.F.) ;
#11100 = ORIENTED_EDGE('',*,*,#8120,.F.) ;
#11101 = ORIENTED_EDGE('',*,*,#8121,.T.) ;
#11102 = ORIENTED_EDGE('',*,*,#8122,.T.) ;
#11103 = ORIENTED_EDGE('',*,*,#8123,.F.) ;
#11104 = ORIENTED_EDGE('',*,*,#8124,.T.) ;
#11105 = ORIENTED_EDGE('',*,*,#8125,.T.) ;
#11106 = ORIENTED_EDGE('',*,*,#8126,.F.) ;
#11107 = ORIENTED_EDGE('',*,*,#8127,.F.) ;
#11108 = ORIENTED_EDGE('',*,*,#8128,.T.) ;
#11109 = ORIENTED_EDGE('',*,*,#8129,.T.) ;
#11110 = ORIENTED_EDGE('',*,*,#8130,.F.) ;
#11111 = ORIENTED_EDGE('',*,*,#8131,.F.) ;
#11112 = ORIENTED_EDGE('',*,*,#8132,.T.) ;
#11113 = ORIENTED_EDGE('',*,*,#8133,.T.) ;
#11114 = ORIENTED_EDGE('',*,*,#8134,.F.) ;
#11115 = ORIENTED_EDGE('',*,*,#8135,.F.) ;
#11116 = ORIENTED_EDGE('',*,*,#8136,.T.) ;
#11117 = ORIENTED_EDGE('',*,*,#8137,.T.) ;
#11118 = ORIENTED_EDGE('',*,*,#8138,.F.) ;
#11119 = ORIENTED_EDGE('',*,*,#8139,.F.) ;
#11120 = ORIENTED_EDGE('',*,*,#8140,.T.) ;
#11121 = ORIENTED_EDGE('',*,*,#8141,.T.) ;
#11122 = ORIENTED_EDGE('',*,*,#8142,.F.) ;
#11123 = ORIENTED_EDGE('',*,*,#8143,.F.) ;
#11124 = ORIENTED_EDGE('',*,*,#8144,.T.) ;
#11125 = ORIENTED_EDGE('',*,*,#8145,.T.) ;
#11126 = ORIENTED_EDGE('',*,*,#8146,.F.) ;
#11127 = ORIENTED_EDGE('',*,*,#8147,.F.) ;
#11128 = ORIENTED_EDGE('',*,*,#8148,.T.) ;
#11129 = ORIENTED_EDGE('',*,*,#8149,.T.) ;
#11130 = ORIENTED_EDGE('',*,*,#8150,.F.) ;
#11131 = ORIENTED_EDGE('',*,*,#8151,.F.) ;
#11132 = ORIENTED_EDGE('',*,*,#8152,.T.) ;
#11133 = ORIENTED_EDGE('',*,*,#8153,.T.) ;
#11134 = ORIENTED_EDGE('',*,*,#8154,.F.) ;
#11135 = ORIENTED_EDGE('',*,*,#8155,.F.) ;
#11136 = ORIENTED_EDGE('',*,*,#8156,.T.) ;
#11137 = ORIENTED_EDGE('',*,*,#8157,.T.) ;
#11138 = ORIENTED_EDGE('',*,*,#8158,.F.) ;
#11139 = ORIENTED_EDGE('',*,*,#8159,.F.) ;
#11140 = ORIENTED_EDGE('',*,*,#8160,.T.) ;
#11141 = ORIENTED_EDGE('',*,*,#8161,.T.) ;
#11142 = ORIENTED_EDGE('',*,*,#8162,.F.) ;
#11143 = ORIENTED_EDGE('',*,*,#8163,.F.) ;
#11144 = ORIENTED_EDGE('',*,*,#8164,.T.) ;
#11145 = ORIENTED_EDGE('',*,*,#8165,.T.) ;
#11146 = ORIENTED_EDGE('',*,*,#8166,.F.) ;
#11147 = ORIENTED_EDGE('',*,*,#8167,.F.) ;
#11148 = ORIENTED_EDGE('',*,*,#8168,.T.) ;
#11149 = ORIENTED_EDGE('',*,*,#8169,.T.) ;
#11150 = ORIENTED_EDGE('',*,*,#8170,.F.) ;
#11151 = ORIENTED_EDGE('',*,*,#8171,.F.) ;
#11152 = ORIENTED_EDGE('',*,*,#8172,.T.) ;
#11153 = ORIENTED_EDGE('',*,*,#8173,.T.) ;
#11154 = ORIENTED_EDGE('',*,*,#8174,.F.) ;
#11155 = ORIENTED_EDGE('',*,*,#8175,.F.) ;
#11156 = ORIENTED_EDGE('',*,*,#8176,.F.) ;
#11157 = ORIENTED_EDGE('',*,*,#8177,.T.) ;
#11158 = ORIENTED_EDGE('',*,*,#8178,.T.) ;
#11159 = ORIENTED_EDGE('',*,*,#8179,.F.) ;
#11160 = ORIENTED_EDGE('',*,*,#8180,.T.) ;
#11161 = ORIENTED_EDGE('',*,*,#8181,.T.) ;
#11162 = ORIENTED_EDGE('',*,*,#8182,.F.) ;
#11163 = ORIENTED_EDGE('',*,*,#8183,.F.) ;
#11164 = ORIENTED_EDGE('',*,*,#8184,.T.) ;
#11165 = ORIENTED_EDGE('',*,*,#8185,.T.) ;
#11166 = ORIENTED_EDGE('',*,*,#8186,.F.) ;
#11167 = ORIENTED_EDGE('',*,*,#8187,.F.) ;
#11168 = ORIENTED_EDGE('',*,*,#8188,.T.) ;
#11169 = ORIENTED_EDGE('',*,*,#8189,.T.) ;
#11170 = ORIENTED_EDGE('',*,*,#8190,.F.) ;
#11171 = ORIENTED_EDGE('',*,*,#8191,.F.) ;
#11172 = ORIENTED_EDGE('',*,*,#8192,.T.) ;
#11173 = ORIENTED_EDGE('',*,*,#8193,.T.) ;
#11174 = ORIENTED_EDGE('',*,*,#8194,.F.) ;
#11175 = ORIENTED_EDGE('',*,*,#8195,.F.) ;
#11176 = ORIENTED_EDGE('',*,*,#8196,.T.) ;
#11177 = ORIENTED_EDGE('',*,*,#8197,.T.) ;
#11178 = ORIENTED_EDGE('',*,*,#8198,.F.) ;
#11179 = ORIENTED_EDGE('',*,*,#8199,.F.) ;
#11180 = ORIENTED_EDGE('',*,*,#8200,.T.) ;
#11181 = ORIENTED_EDGE('',*,*,#8201,.T.) ;
#11182 = ORIENTED_EDGE('',*,*,#8202,.F.) ;
#11183 = ORIENTED_EDGE('',*,*,#8203,.F.) ;
#11184 = ORIENTED_EDGE('',*,*,#8204,.T.) ;
#11185 = ORIENTED_EDGE('',*,*,#8205,.T.) ;
#11186 = ORIENTED_EDGE('',*,*,#8206,.F.) ;
#11187 = ORIENTED_EDGE('',*,*,#8207,.F.) ;
#11188 = ORIENTED_EDGE('',*,*,#8208,.T.) ;
#11189 = ORIENTED_EDGE('',*,*,#8209,.T.) ;
#11190 = ORIENTED_EDGE('',*,*,#8210,.F.) ;
#11191 = ORIENTED_EDGE('',*,*,#8211,.F.) ;
#11192 = ORIENTED_EDGE('',*,*,#8212,.T.) ;
#11193 = ORIENTED_EDGE('',*,*,#8213,.T.) ;
#11194 = ORIENTED_EDGE('',*,*,#8214,.F.) ;
#11195 = ORIENTED_EDGE('',*,*,#8215,.F.) ;
#11196 = ORIENTED_EDGE('',*,*,#8216,.T.) ;
#11197 = ORIENTED_EDGE('',*,*,#8217,.T.) ;
#11198 = ORIENTED_EDGE('',*,*,#8218,.F.) ;
#11199 = ORIENTED_EDGE('',*,*,#8219,.F.) ;
#11200 = ORIENTED_EDGE('',*,*,#8220,.T.) ;
#11201 = ORIENTED_EDGE('',*,*,#8221,.T.) ;
#11202 = ORIENTED_EDGE('',*,*,#8222,.F.) ;
#11203 = ORIENTED_EDGE('',*,*,#8223,.F.) ;
#11204 = ORIENTED_EDGE('',*,*,#8224,.F.) ;
#11205 = ORIENTED_EDGE('',*,*,#8225,.T.) ;
#11206 = ORIENTED_EDGE('',*,*,#8226,.T.) ;
#11207 = ORIENTED_EDGE('',*,*,#8227,.F.) ;
#11208 = ORIENTED_EDGE('',*,*,#8228,.F.) ;
#11209 = ORIENTED_EDGE('',*,*,#8229,.T.) ;
#11210 = ORIENTED_EDGE('',*,*,#8230,.T.) ;
#11211 = ORIENTED_EDGE('',*,*,#8231,.F.) ;
#11212 = ORIENTED_EDGE('',*,*,#8232,.F.) ;
#11213 = ORIENTED_EDGE('',*,*,#8233,.T.) ;
#11214 = ORIENTED_EDGE('',*,*,#8234,.T.) ;
#11215 = ORIENTED_EDGE('',*,*,#8235,.F.) ;
#11216 = ORIENTED_EDGE('',*,*,#8236,.F.) ;
#11217 = ORIENTED_EDGE('',*,*,#8237,.T.) ;
#11218 = ORIENTED_EDGE('',*,*,#8238,.T.) ;
#11219 = ORIENTED_EDGE('',*,*,#8239,.F.) ;
#11220 = ORIENTED_EDGE('',*,*,#8240,.F.) ;
#11221 = ORIENTED_EDGE('',*,*,#8241,.T.) ;
#11222 = ORIENTED_EDGE('',*,*,#8242,.T.) ;
#11223 = ORIENTED_EDGE('',*,*,#8243,.F.) ;
#11224 = ORIENTED_EDGE('',*,*,#8244,.F.) ;
#11225 = ORIENTED_EDGE('',*,*,#8245,.T.) ;
#11226 = ORIENTED_EDGE('',*,*,#8246,.T.) ;
#11227 = ORIENTED_EDGE('',*,*,#8247,.F.) ;
#11228 = ORIENTED_EDGE('',*,*,#8248,.F.) ;
#11229 = ORIENTED_EDGE('',*,*,#8249,.T.) ;
#11230 = ORIENTED_EDGE('',*,*,#8250,.T.) ;
#11231 = ORIENTED_EDGE('',*,*,#8251,.F.) ;
#11232 = ORIENTED_EDGE('',*,*,#8252,.T.) ;
#11233 = ORIENTED_EDGE('',*,*,#8253,.T.) ;
#11234 = ORIENTED_EDGE('',*,*,#8254,.F.) ;
#11235 = ORIENTED_EDGE('',*,*,#8255,.F.) ;
#11236 = ORIENTED_EDGE('',*,*,#8256,.T.) ;
#11237 = ORIENTED_EDGE('',*,*,#8257,.T.) ;
#11238 = ORIENTED_EDGE('',*,*,#8258,.F.) ;
#11239 = ORIENTED_EDGE('',*,*,#8259,.F.) ;
#11240 = ORIENTED_EDGE('',*,*,#8260,.T.) ;
#11241 = ORIENTED_EDGE('',*,*,#8261,.T.) ;
#11242 = ORIENTED_EDGE('',*,*,#8262,.F.) ;
#11243 = ORIENTED_EDGE('',*,*,#8263,.F.) ;
#11244 = ORIENTED_EDGE('',*,*,#8264,.T.) ;
#11245 = ORIENTED_EDGE('',*,*,#8265,.T.) ;
#11246 = ORIENTED_EDGE('',*,*,#8266,.F.) ;
#11247 = ORIENTED_EDGE('',*,*,#8267,.F.) ;
#11248 = ORIENTED_EDGE('',*,*,#8268,.T.) ;
#11249 = ORIENTED_EDGE('',*,*,#8269,.T.) ;
#11250 = ORIENTED_EDGE('',*,*,#8270,.F.) ;
#11251 = ORIENTED_EDGE('',*,*,#8271,.F.) ;
#11252 = ORIENTED_EDGE('',*,*,#8272,.T.) ;
#11253 = ORIENTED_EDGE('',*,*,#8273,.T.) ;
#11254 = ORIENTED_EDGE('',*,*,#8274,.F.) ;
#11255 = ORIENTED_EDGE('',*,*,#8275,.F.) ;
#11256 = ORIENTED_EDGE('',*,*,#8276,.T.) ;
#11257 = ORIENTED_EDGE('',*,*,#8277,.T.) ;
#11258 = ORIENTED_EDGE('',*,*,#8278,.F.) ;
#11259 = ORIENTED_EDGE('',*,*,#8279,.F.) ;
#11260 = ORIENTED_EDGE('',*,*,#8280,.T.) ;
#11261 = ORIENTED_EDGE('',*,*,#8281,.T.) ;
#11262 = ORIENTED_EDGE('',*,*,#8282,.F.) ;
#11263 = ORIENTED_EDGE('',*,*,#8283,.F.) ;
#11264 = ORIENTED_EDGE('',*,*,#8284,.T.) ;
#11265 = ORIENTED_EDGE('',*,*,#8285,.T.) ;
#11266 = ORIENTED_EDGE('',*,*,#8286,.F.) ;
#11267 = ORIENTED_EDGE('',*,*,#8287,.F.) ;
#11268 = ORIENTED_EDGE('',*,*,#8288,.T.) ;
#11269 = ORIENTED_EDGE('',*,*,#8289,.T.) ;
#11270 = ORIENTED_EDGE('',*,*,#8290,.F.) ;
#11271 = ORIENTED_EDGE('',*,*,#8291,.F.) ;
#11272 = ORIENTED_EDGE('',*,*,#8292,.T.) ;
#11273 = ORIENTED_EDGE('',*,*,#8293,.T.) ;
#11274 = ORIENTED_EDGE('',*,*,#8294,.F.) ;
#11275 = ORIENTED_EDGE('',*,*,#8295,.F.) ;
#11276 = ORIENTED_EDGE('',*,*,#8296,.F.) ;
#11277 = ORIENTED_EDGE('',*,*,#8297,.T.) ;
#11278 = ORIENTED_EDGE('',*,*,#8298,.T.) ;
#11279 = ORIENTED_EDGE('',*,*,#8299,.F.) ;
#11280 = ORIENTED_EDGE('',*,*,#8300,.T.) ;
#11281 = ORIENTED_EDGE('',*,*,#8301,.T.) ;
#11282 = ORIENTED_EDGE('',*,*,#8302,.F.) ;
#11283 = ORIENTED_EDGE('',*,*,#8303,.F.) ;
#11284 = ORIENTED_EDGE('',*,*,#8304,.T.) ;
#11285 = ORIENTED_EDGE('',*,*,#8305,.T.) ;
#11286 = ORIENTED_EDGE('',*,*,#8306,.F.) ;
#11287 = ORIENTED_EDGE('',*,*,#8307,.F.) ;
#11288 = ORIENTED_EDGE('',*,*,#8308,.T.) ;
#11289 = ORIENTED_EDGE('',*,*,#8309,.T.) ;
#11290 = ORIENTED_EDGE('',*,*,#8310,.F.) ;
#11291 = ORIENTED_EDGE('',*,*,#8311,.F.) ;
#11292 = ORIENTED_EDGE('',*,*,#8312,.T.) ;
#11293 = ORIENTED_EDGE('',*,*,#8313,.T.) ;
#11294 = ORIENTED_EDGE('',*,*,#8314,.F.) ;
#11295 = ORIENTED_EDGE('',*,*,#8315,.F.) ;
#11296 = ORIENTED_EDGE('',*,*,#8316,.T.) ;
#11297 = ORIENTED_EDGE('',*,*,#8317,.T.) ;
#11298 = ORIENTED_EDGE('',*,*,#8318,.F.) ;
#11299 = ORIENTED_EDGE('',*,*,#8319,.F.) ;
#11300 = ORIENTED_EDGE('',*,*,#8320,.T.) ;
#11301 = ORIENTED_EDGE('',*,*,#8321,.T.) ;
#11302 = ORIENTED_EDGE('',*,*,#8322,.F.) ;
#11303 = ORIENTED_EDGE('',*,*,#8323,.F.) ;
#11304 = ORIENTED_EDGE('',*,*,#8324,.T.) ;
#11305 = ORIENTED_EDGE('',*,*,#8325,.T.) ;
#11306 = ORIENTED_EDGE('',*,*,#8326,.F.) ;
#11307 = ORIENTED_EDGE('',*,*,#8327,.F.) ;
#11308 = ORIENTED_EDGE('',*,*,#8328,.F.) ;
#11309 = ORIENTED_EDGE('',*,*,#8329,.T.) ;
#11310 = ORIENTED_EDGE('',*,*,#8330,.T.) ;
#11311 = ORIENTED_EDGE('',*,*,#8331,.F.) ;
#11312 = ORIENTED_EDGE('',*,*,#8332,.T.) ;
#11313 = ORIENTED_EDGE('',*,*,#8333,.T.) ;
#11314 = ORIENTED_EDGE('',*,*,#8334,.F.) ;
#11315 = ORIENTED_EDGE('',*,*,#8335,.F.) ;
#11316 = ORIENTED_EDGE('',*,*,#8336,.T.) ;
#11317 = ORIENTED_EDGE('',*,*,#8093,.T.) ;
#11318 = ORIENTED_EDGE('',*,*,#8336,.F.) ;
#11319 = ORIENTED_EDGE('',*,*,#8337,.F.) ;
#11320 = ORIENTED_EDGE('',*,*,#8335,.T.) ;
#11321 = ORIENTED_EDGE('',*,*,#8337,.T.) ;
#11322 = ORIENTED_EDGE('',*,*,#8338,.T.) ;
#11323 = ORIENTED_EDGE('',*,*,#8339,.F.) ;
#11324 = ORIENTED_EDGE('',*,*,#8340,.F.) ;
#11325 = ORIENTED_EDGE('',*,*,#8338,.F.) ;
#11326 = ORIENTED_EDGE('',*,*,#8341,.F.) ;
#11327 = ORIENTED_EDGE('',*,*,#8342,.F.) ;
#11328 = ORIENTED_EDGE('',*,*,#8343,.T.) ;
#11329 = ORIENTED_EDGE('',*,*,#8339,.T.) ;
#11330 = ORIENTED_EDGE('',*,*,#8340,.T.) ;
#11331 = ORIENTED_EDGE('',*,*,#8343,.F.) ;
#11332 = ORIENTED_EDGE('',*,*,#8341,.T.) ;
#11333 = ORIENTED_EDGE('',*,*,#8342,.T.) ;
#11334 = ORIENTED_EDGE('',*,*,#8344,.T.) ;
#11335 = ORIENTED_EDGE('',*,*,#8345,.F.) ;
#11336 = ORIENTED_EDGE('',*,*,#8269,.F.) ;
#11337 = ORIENTED_EDGE('',*,*,#8346,.F.) ;
#11338 = ORIENTED_EDGE('',*,*,#8265,.F.) ;
#11339 = ORIENTED_EDGE('',*,*,#8347,.F.) ;
#11340 = ORIENTED_EDGE('',*,*,#8261,.F.) ;
#11341 = ORIENTED_EDGE('',*,*,#8348,.F.) ;
#11342 = ORIENTED_EDGE('',*,*,#8257,.F.) ;
#11343 = ORIENTED_EDGE('',*,*,#8349,.F.) ;
#11344 = ORIENTED_EDGE('',*,*,#8226,.F.) ;
#11345 = ORIENTED_EDGE('',*,*,#8350,.F.) ;
#11346 = ORIENTED_EDGE('',*,*,#8230,.F.) ;
#11347 = ORIENTED_EDGE('',*,*,#8351,.F.) ;
#11348 = ORIENTED_EDGE('',*,*,#8234,.F.) ;
#11349 = ORIENTED_EDGE('',*,*,#8352,.F.) ;
#11350 = ORIENTED_EDGE('',*,*,#8238,.F.) ;
#11351 = ORIENTED_EDGE('',*,*,#8353,.F.) ;
#11352 = ORIENTED_EDGE('',*,*,#8242,.F.) ;
#11353 = ORIENTED_EDGE('',*,*,#8354,.F.) ;
#11354 = ORIENTED_EDGE('',*,*,#8246,.F.) ;
#11355 = ORIENTED_EDGE('',*,*,#8355,.F.) ;
#11356 = ORIENTED_EDGE('',*,*,#8250,.F.) ;
#11357 = ORIENTED_EDGE('',*,*,#8356,.F.) ;
#11358 = ORIENTED_EDGE('',*,*,#8253,.F.) ;
#11359 = ORIENTED_EDGE('',*,*,#8357,.F.) ;
#11360 = ORIENTED_EDGE('',*,*,#8221,.F.) ;
#11361 = ORIENTED_EDGE('',*,*,#8358,.F.) ;
#11362 = ORIENTED_EDGE('',*,*,#8217,.F.) ;
#11363 = ORIENTED_EDGE('',*,*,#8359,.F.) ;
#11364 = ORIENTED_EDGE('',*,*,#8213,.F.) ;
#11365 = ORIENTED_EDGE('',*,*,#8360,.F.) ;
#11366 = ORIENTED_EDGE('',*,*,#8209,.F.) ;
#11367 = ORIENTED_EDGE('',*,*,#8361,.F.) ;
#11368 = ORIENTED_EDGE('',*,*,#8205,.F.) ;
#11369 = ORIENTED_EDGE('',*,*,#8362,.F.) ;
#11370 = ORIENTED_EDGE('',*,*,#8201,.F.) ;
#11371 = ORIENTED_EDGE('',*,*,#8363,.F.) ;
#11372 = ORIENTED_EDGE('',*,*,#8197,.F.) ;
#11373 = ORIENTED_EDGE('',*,*,#8364,.F.) ;
#11374 = ORIENTED_EDGE('',*,*,#8193,.F.) ;
#11375 = ORIENTED_EDGE('',*,*,#8365,.F.) ;
#11376 = ORIENTED_EDGE('',*,*,#8189,.F.) ;
#11377 = ORIENTED_EDGE('',*,*,#8366,.F.) ;
#11378 = ORIENTED_EDGE('',*,*,#8185,.F.) ;
#11379 = ORIENTED_EDGE('',*,*,#8367,.F.) ;
#11380 = ORIENTED_EDGE('',*,*,#8178,.F.) ;
#11381 = ORIENTED_EDGE('',*,*,#8368,.F.) ;
#11382 = ORIENTED_EDGE('',*,*,#8181,.F.) ;
#11383 = ORIENTED_EDGE('',*,*,#8369,.F.) ;
#11384 = ORIENTED_EDGE('',*,*,#8173,.F.) ;
#11385 = ORIENTED_EDGE('',*,*,#8370,.F.) ;
#11386 = ORIENTED_EDGE('',*,*,#8169,.F.) ;
#11387 = ORIENTED_EDGE('',*,*,#8371,.F.) ;
#11388 = ORIENTED_EDGE('',*,*,#8165,.F.) ;
#11389 = ORIENTED_EDGE('',*,*,#8372,.F.) ;
#11390 = ORIENTED_EDGE('',*,*,#8161,.F.) ;
#11391 = ORIENTED_EDGE('',*,*,#8373,.F.) ;
#11392 = ORIENTED_EDGE('',*,*,#8157,.F.) ;
#11393 = ORIENTED_EDGE('',*,*,#8374,.F.) ;
#11394 = ORIENTED_EDGE('',*,*,#8153,.F.) ;
#11395 = ORIENTED_EDGE('',*,*,#8375,.F.) ;
#11396 = ORIENTED_EDGE('',*,*,#8149,.F.) ;
#11397 = ORIENTED_EDGE('',*,*,#8376,.F.) ;
#11398 = ORIENTED_EDGE('',*,*,#8145,.F.) ;
#11399 = ORIENTED_EDGE('',*,*,#8377,.F.) ;
#11400 = ORIENTED_EDGE('',*,*,#8141,.F.) ;
#11401 = ORIENTED_EDGE('',*,*,#8378,.F.) ;
#11402 = ORIENTED_EDGE('',*,*,#8137,.F.) ;
#11403 = ORIENTED_EDGE('',*,*,#8379,.F.) ;
#11404 = ORIENTED_EDGE('',*,*,#8133,.F.) ;
#11405 = ORIENTED_EDGE('',*,*,#8380,.F.) ;
#11406 = ORIENTED_EDGE('',*,*,#8129,.F.) ;
#11407 = ORIENTED_EDGE('',*,*,#8381,.F.) ;
#11408 = ORIENTED_EDGE('',*,*,#8114,.F.) ;
#11409 = ORIENTED_EDGE('',*,*,#8382,.F.) ;
#11410 = ORIENTED_EDGE('',*,*,#8118,.F.) ;
#11411 = ORIENTED_EDGE('',*,*,#8383,.F.) ;
#11412 = ORIENTED_EDGE('',*,*,#8122,.F.) ;
#11413 = ORIENTED_EDGE('',*,*,#8384,.F.) ;
#11414 = ORIENTED_EDGE('',*,*,#8125,.F.) ;
#11415 = ORIENTED_EDGE('',*,*,#8385,.F.) ;
#11416 = ORIENTED_EDGE('',*,*,#8109,.F.) ;
#11417 = ORIENTED_EDGE('',*,*,#8386,.F.) ;
#11418 = ORIENTED_EDGE('',*,*,#8105,.F.) ;
#11419 = ORIENTED_EDGE('',*,*,#8387,.F.) ;
#11420 = ORIENTED_EDGE('',*,*,#8101,.F.) ;
#11421 = ORIENTED_EDGE('',*,*,#8388,.F.) ;
#11422 = ORIENTED_EDGE('',*,*,#8098,.F.) ;
#11423 = ORIENTED_EDGE('',*,*,#8389,.F.) ;
#11424 = ORIENTED_EDGE('',*,*,#8330,.F.) ;
#11425 = ORIENTED_EDGE('',*,*,#8390,.F.) ;
#11426 = ORIENTED_EDGE('',*,*,#8333,.F.) ;
#11427 = ORIENTED_EDGE('',*,*,#8391,.F.) ;
#11428 = ORIENTED_EDGE('',*,*,#8325,.F.) ;
#11429 = ORIENTED_EDGE('',*,*,#8392,.F.) ;
#11430 = ORIENTED_EDGE('',*,*,#8321,.F.) ;
#11431 = ORIENTED_EDGE('',*,*,#8393,.F.) ;
#11432 = ORIENTED_EDGE('',*,*,#8317,.F.) ;
#11433 = ORIENTED_EDGE('',*,*,#8394,.F.) ;
#11434 = ORIENTED_EDGE('',*,*,#8313,.F.) ;
#11435 = ORIENTED_EDGE('',*,*,#8395,.F.) ;
#11436 = ORIENTED_EDGE('',*,*,#8309,.F.) ;
#11437 = ORIENTED_EDGE('',*,*,#8396,.F.) ;
#11438 = ORIENTED_EDGE('',*,*,#8305,.F.) ;
#11439 = ORIENTED_EDGE('',*,*,#8397,.F.) ;
#11440 = ORIENTED_EDGE('',*,*,#8298,.F.) ;
#11441 = ORIENTED_EDGE('',*,*,#8398,.F.) ;
#11442 = ORIENTED_EDGE('',*,*,#8301,.F.) ;
#11443 = ORIENTED_EDGE('',*,*,#8399,.F.) ;
#11444 = ORIENTED_EDGE('',*,*,#8293,.F.) ;
#11445 = ORIENTED_EDGE('',*,*,#8400,.F.) ;
#11446 = ORIENTED_EDGE('',*,*,#8289,.F.) ;
#11447 = ORIENTED_EDGE('',*,*,#8401,.F.) ;
#11448 = ORIENTED_EDGE('',*,*,#8285,.F.) ;
#11449 = ORIENTED_EDGE('',*,*,#8402,.F.) ;
#11450 = ORIENTED_EDGE('',*,*,#8281,.F.) ;
#11451 = ORIENTED_EDGE('',*,*,#8403,.F.) ;
#11452 = ORIENTED_EDGE('',*,*,#8277,.F.) ;
#11453 = ORIENTED_EDGE('',*,*,#8404,.F.) ;
#11454 = ORIENTED_EDGE('',*,*,#8273,.F.) ;
#11455 = ORIENTED_EDGE('',*,*,#8405,.F.) ;
#11456 = ORIENTED_EDGE('',*,*,#8344,.F.) ;
#11457 = ORIENTED_EDGE('',*,*,#8406,.F.) ;
#11458 = ORIENTED_EDGE('',*,*,#8407,.F.) ;
#11459 = ORIENTED_EDGE('',*,*,#8408,.T.) ;
#11460 = ORIENTED_EDGE('',*,*,#8409,.T.) ;
#11461 = ORIENTED_EDGE('',*,*,#8151,.T.) ;
#11462 = ORIENTED_EDGE('',*,*,#8410,.T.) ;
#11463 = ORIENTED_EDGE('',*,*,#8155,.T.) ;
#11464 = ORIENTED_EDGE('',*,*,#8411,.T.) ;
#11465 = ORIENTED_EDGE('',*,*,#8159,.T.) ;
#11466 = ORIENTED_EDGE('',*,*,#8412,.T.) ;
#11467 = ORIENTED_EDGE('',*,*,#8163,.T.) ;
#11468 = ORIENTED_EDGE('',*,*,#8413,.T.) ;
#11469 = ORIENTED_EDGE('',*,*,#8167,.T.) ;
#11470 = ORIENTED_EDGE('',*,*,#8414,.T.) ;
#11471 = ORIENTED_EDGE('',*,*,#8171,.T.) ;
#11472 = ORIENTED_EDGE('',*,*,#8415,.T.) ;
#11473 = ORIENTED_EDGE('',*,*,#8179,.T.) ;
#11474 = ORIENTED_EDGE('',*,*,#8416,.T.) ;
#11475 = ORIENTED_EDGE('',*,*,#8176,.T.) ;
#11476 = ORIENTED_EDGE('',*,*,#8417,.T.) ;
#11477 = ORIENTED_EDGE('',*,*,#8183,.T.) ;
#11478 = ORIENTED_EDGE('',*,*,#8418,.T.) ;
#11479 = ORIENTED_EDGE('',*,*,#8187,.T.) ;
#11480 = ORIENTED_EDGE('',*,*,#8419,.T.) ;
#11481 = ORIENTED_EDGE('',*,*,#8191,.T.) ;
#11482 = ORIENTED_EDGE('',*,*,#8420,.T.) ;
#11483 = ORIENTED_EDGE('',*,*,#8195,.T.) ;
#11484 = ORIENTED_EDGE('',*,*,#8421,.T.) ;
#11485 = ORIENTED_EDGE('',*,*,#8199,.T.) ;
#11486 = ORIENTED_EDGE('',*,*,#8422,.T.) ;
#11487 = ORIENTED_EDGE('',*,*,#8203,.T.) ;
#11488 = ORIENTED_EDGE('',*,*,#8423,.T.) ;
#11489 = ORIENTED_EDGE('',*,*,#8207,.T.) ;
#11490 = ORIENTED_EDGE('',*,*,#8424,.T.) ;
#11491 = ORIENTED_EDGE('',*,*,#8211,.T.) ;
#11492 = ORIENTED_EDGE('',*,*,#8425,.T.) ;
#11493 = ORIENTED_EDGE('',*,*,#8215,.T.) ;
#11494 = ORIENTED_EDGE('',*,*,#8426,.T.) ;
#11495 = ORIENTED_EDGE('',*,*,#8219,.T.) ;
#11496 = ORIENTED_EDGE('',*,*,#8427,.T.) ;
#11497 = ORIENTED_EDGE('',*,*,#8251,.T.) ;
#11498 = ORIENTED_EDGE('',*,*,#8428,.T.) ;
#11499 = ORIENTED_EDGE('',*,*,#8248,.T.) ;
#11500 = ORIENTED_EDGE('',*,*,#8429,.T.) ;
#11501 = ORIENTED_EDGE('',*,*,#8244,.T.) ;
#11502 = ORIENTED_EDGE('',*,*,#8430,.T.) ;
#11503 = ORIENTED_EDGE('',*,*,#8240,.T.) ;
#11504 = ORIENTED_EDGE('',*,*,#8431,.T.) ;
#11505 = ORIENTED_EDGE('',*,*,#8236,.T.) ;
#11506 = ORIENTED_EDGE('',*,*,#8432,.T.) ;
#11507 = ORIENTED_EDGE('',*,*,#8232,.T.) ;
#11508 = ORIENTED_EDGE('',*,*,#8433,.T.) ;
#11509 = ORIENTED_EDGE('',*,*,#8228,.T.) ;
#11510 = ORIENTED_EDGE('',*,*,#8434,.T.) ;
#11511 = ORIENTED_EDGE('',*,*,#8224,.T.) ;
#11512 = ORIENTED_EDGE('',*,*,#8435,.T.) ;
#11513 = ORIENTED_EDGE('',*,*,#8255,.T.) ;
#11514 = ORIENTED_EDGE('',*,*,#8436,.T.) ;
#11515 = ORIENTED_EDGE('',*,*,#8259,.T.) ;
#11516 = ORIENTED_EDGE('',*,*,#8437,.T.) ;
#11517 = ORIENTED_EDGE('',*,*,#8263,.T.) ;
#11518 = ORIENTED_EDGE('',*,*,#8438,.T.) ;
#11519 = ORIENTED_EDGE('',*,*,#8267,.T.) ;
#11520 = ORIENTED_EDGE('',*,*,#8439,.T.) ;
#11521 = ORIENTED_EDGE('',*,*,#8271,.T.) ;
#11522 = ORIENTED_EDGE('',*,*,#8440,.T.) ;
#11523 = ORIENTED_EDGE('',*,*,#8275,.T.) ;
#11524 = ORIENTED_EDGE('',*,*,#8441,.T.) ;
#11525 = ORIENTED_EDGE('',*,*,#8279,.T.) ;
#11526 = ORIENTED_EDGE('',*,*,#8442,.T.) ;
#11527 = ORIENTED_EDGE('',*,*,#8283,.T.) ;
#11528 = ORIENTED_EDGE('',*,*,#8443,.T.) ;
#11529 = ORIENTED_EDGE('',*,*,#8287,.T.) ;
#11530 = ORIENTED_EDGE('',*,*,#8444,.T.) ;
#11531 = ORIENTED_EDGE('',*,*,#8291,.T.) ;
#11532 = ORIENTED_EDGE('',*,*,#8445,.T.) ;
#11533 = ORIENTED_EDGE('',*,*,#8299,.T.) ;
#11534 = ORIENTED_EDGE('',*,*,#8446,.T.) ;
#11535 = ORIENTED_EDGE('',*,*,#8296,.T.) ;
#11536 = ORIENTED_EDGE('',*,*,#8447,.T.) ;
#11537 = ORIENTED_EDGE('',*,*,#8303,.T.) ;
#11538 = ORIENTED_EDGE('',*,*,#8448,.T.) ;
#11539 = ORIENTED_EDGE('',*,*,#8307,.T.) ;
#11540 = ORIENTED_EDGE('',*,*,#8449,.T.) ;
#11541 = ORIENTED_EDGE('',*,*,#8311,.T.) ;
#11542 = ORIENTED_EDGE('',*,*,#8450,.T.) ;
#11543 = ORIENTED_EDGE('',*,*,#8315,.T.) ;
#11544 = ORIENTED_EDGE('',*,*,#8451,.T.) ;
#11545 = ORIENTED_EDGE('',*,*,#8319,.T.) ;
#11546 = ORIENTED_EDGE('',*,*,#8452,.T.) ;
#11547 = ORIENTED_EDGE('',*,*,#8323,.T.) ;
#11548 = ORIENTED_EDGE('',*,*,#8453,.T.) ;
#11549 = ORIENTED_EDGE('',*,*,#8331,.T.) ;
#11550 = ORIENTED_EDGE('',*,*,#8454,.T.) ;
#11551 = ORIENTED_EDGE('',*,*,#8328,.T.) ;
#11552 = ORIENTED_EDGE('',*,*,#8455,.T.) ;
#11553 = ORIENTED_EDGE('',*,*,#8096,.T.) ;
#11554 = ORIENTED_EDGE('',*,*,#8456,.T.) ;
#11555 = ORIENTED_EDGE('',*,*,#8099,.T.) ;
#11556 = ORIENTED_EDGE('',*,*,#8457,.T.) ;
#11557 = ORIENTED_EDGE('',*,*,#8103,.T.) ;
#11558 = ORIENTED_EDGE('',*,*,#8458,.T.) ;
#11559 = ORIENTED_EDGE('',*,*,#8107,.T.) ;
#11560 = ORIENTED_EDGE('',*,*,#8459,.T.) ;
#11561 = ORIENTED_EDGE('',*,*,#8123,.T.) ;
#11562 = ORIENTED_EDGE('',*,*,#8460,.T.) ;
#11563 = ORIENTED_EDGE('',*,*,#8120,.T.) ;
#11564 = ORIENTED_EDGE('',*,*,#8461,.T.) ;
#11565 = ORIENTED_EDGE('',*,*,#8116,.T.) ;
#11566 = ORIENTED_EDGE('',*,*,#8462,.T.) ;
#11567 = ORIENTED_EDGE('',*,*,#8112,.T.) ;
#11568 = ORIENTED_EDGE('',*,*,#8463,.T.) ;
#11569 = ORIENTED_EDGE('',*,*,#8127,.T.) ;
#11570 = ORIENTED_EDGE('',*,*,#8464,.T.) ;
#11571 = ORIENTED_EDGE('',*,*,#8131,.T.) ;
#11572 = ORIENTED_EDGE('',*,*,#8465,.T.) ;
#11573 = ORIENTED_EDGE('',*,*,#8135,.T.) ;
#11574 = ORIENTED_EDGE('',*,*,#8466,.T.) ;
#11575 = ORIENTED_EDGE('',*,*,#8139,.T.) ;
#11576 = ORIENTED_EDGE('',*,*,#8467,.T.) ;
#11577 = ORIENTED_EDGE('',*,*,#8143,.T.) ;
#11578 = ORIENTED_EDGE('',*,*,#8468,.T.) ;
#11579 = ORIENTED_EDGE('',*,*,#8147,.T.) ;
#11580 = ORIENTED_EDGE('',*,*,#8469,.T.) ;
#11581 = ORIENTED_EDGE('',*,*,#8408,.F.) ;
#11582 = ORIENTED_EDGE('',*,*,#8406,.T.) ;
#11583 = ORIENTED_EDGE('',*,*,#8407,.T.) ;
#11584 = ORIENTED_EDGE('',*,*,#8470,.T.) ;
#11585 = ORIENTED_EDGE('',*,*,#8471,.F.) ;
#11586 = ORIENTED_EDGE('',*,*,#8472,.F.) ;
#11587 = ORIENTED_EDGE('',*,*,#8470,.F.) ;
#11588 = ORIENTED_EDGE('',*,*,#8473,.F.) ;
#11589 = ORIENTED_EDGE('',*,*,#8474,.T.) ;
#11590 = ORIENTED_EDGE('',*,*,#8471,.T.) ;
#11591 = ORIENTED_EDGE('',*,*,#8472,.T.) ;
#11592 = ORIENTED_EDGE('',*,*,#8474,.F.) ;
#11593 = ORIENTED_EDGE('',*,*,#8473,.T.) ;
#11594 = ORIENTED_EDGE('',*,*,#8475,.F.) ;
#11595 = ORIENTED_EDGE('',*,*,#8476,.F.) ;
#11596 = ORIENTED_EDGE('',*,*,#8477,.T.) ;
#11597 = ORIENTED_EDGE('',*,*,#8475,.T.) ;
#11598 = ORIENTED_EDGE('',*,*,#8477,.F.) ;
#11599 = ORIENTED_EDGE('',*,*,#8476,.T.) ;
#11600 = ORIENTED_EDGE('',*,*,#8478,.F.) ;
#11601 = ORIENTED_EDGE('',*,*,#8479,.F.) ;
#11602 = ORIENTED_EDGE('',*,*,#8480,.T.) ;
#11603 = ORIENTED_EDGE('',*,*,#8478,.T.) ;
#11604 = ORIENTED_EDGE('',*,*,#8480,.F.) ;
#11605 = ORIENTED_EDGE('',*,*,#8479,.T.) ;
#11606 = ORIENTED_EDGE('',*,*,#8091,.T.) ;
#11607 = ORIENTED_EDGE('',*,*,#8481,.F.) ;
#11608 = ORIENTED_EDGE('',*,*,#8086,.T.) ;
#11609 = ORIENTED_EDGE('',*,*,#8089,.T.) ;
#11610 = ORIENTED_EDGE('',*,*,#8482,.F.) ;
#11611 = ORIENTED_EDGE('',*,*,#8390,.T.) ;
#11612 = ORIENTED_EDGE('',*,*,#8483,.F.) ;
#11613 = ORIENTED_EDGE('',*,*,#8484,.T.) ;
#11614 = ORIENTED_EDGE('',*,*,#8485,.T.) ;
#11615 = ORIENTED_EDGE('',*,*,#8486,.F.) ;
#11616 = ORIENTED_EDGE('',*,*,#8487,.T.) ;
#11617 = ORIENTED_EDGE('',*,*,#8454,.F.) ;
#11618 = ORIENTED_EDGE('',*,*,#8483,.T.) ;
#11619 = ORIENTED_EDGE('',*,*,#8329,.F.) ;
#11620 = ORIENTED_EDGE('',*,*,#8487,.F.) ;
#11621 = ORIENTED_EDGE('',*,*,#8488,.T.) ;
#11622 = ORIENTED_EDGE('',*,*,#8484,.F.) ;
#11623 = ORIENTED_EDGE('',*,*,#8488,.F.) ;
#11624 = ORIENTED_EDGE('',*,*,#8486,.T.) ;
#11625 = ORIENTED_EDGE('',*,*,#8489,.T.) ;
#11626 = ORIENTED_EDGE('',*,*,#8482,.T.) ;
#11627 = ORIENTED_EDGE('',*,*,#8489,.F.) ;
#11628 = ORIENTED_EDGE('',*,*,#8485,.F.) ;
#11629 = ORIENTED_EDGE('',*,*,#8334,.T.) ;
#11630 = ORIENTED_EDGE('',*,*,#8389,.T.) ;
#11631 = ORIENTED_EDGE('',*,*,#8490,.F.) ;
#11632 = ORIENTED_EDGE('',*,*,#8491,.T.) ;
#11633 = ORIENTED_EDGE('',*,*,#8492,.F.) ;
#11634 = ORIENTED_EDGE('',*,*,#8493,.T.) ;
#11635 = ORIENTED_EDGE('',*,*,#8494,.F.) ;
#11636 = ORIENTED_EDGE('',*,*,#8495,.T.) ;
#11637 = ORIENTED_EDGE('',*,*,#8455,.F.) ;
#11638 = ORIENTED_EDGE('',*,*,#8490,.T.) ;
#11639 = ORIENTED_EDGE('',*,*,#8097,.F.) ;
#11640 = ORIENTED_EDGE('',*,*,#8495,.F.) ;
#11641 = ORIENTED_EDGE('',*,*,#8496,.T.) ;
#11642 = ORIENTED_EDGE('',*,*,#8491,.F.) ;
#11643 = ORIENTED_EDGE('',*,*,#8496,.F.) ;
#11644 = ORIENTED_EDGE('',*,*,#8494,.T.) ;
#11645 = ORIENTED_EDGE('',*,*,#8497,.T.) ;
#11646 = ORIENTED_EDGE('',*,*,#8492,.T.) ;
#11647 = ORIENTED_EDGE('',*,*,#8497,.F.) ;
#11648 = ORIENTED_EDGE('',*,*,#8493,.F.) ;
#11649 = ORIENTED_EDGE('',*,*,#8327,.T.) ;
#11650 = ORIENTED_EDGE('',*,*,#8391,.T.) ;
#11651 = ORIENTED_EDGE('',*,*,#8498,.F.) ;
#11652 = ORIENTED_EDGE('',*,*,#8499,.T.) ;
#11653 = ORIENTED_EDGE('',*,*,#8500,.F.) ;
#11654 = ORIENTED_EDGE('',*,*,#8501,.T.) ;
#11655 = ORIENTED_EDGE('',*,*,#8502,.F.) ;
#11656 = ORIENTED_EDGE('',*,*,#8503,.T.) ;
#11657 = ORIENTED_EDGE('',*,*,#8453,.F.) ;
#11658 = ORIENTED_EDGE('',*,*,#8498,.T.) ;
#11659 = ORIENTED_EDGE('',*,*,#8332,.F.) ;
#11660 = ORIENTED_EDGE('',*,*,#8503,.F.) ;
#11661 = ORIENTED_EDGE('',*,*,#8504,.T.) ;
#11662 = ORIENTED_EDGE('',*,*,#8499,.F.) ;
#11663 = ORIENTED_EDGE('',*,*,#8504,.F.) ;
#11664 = ORIENTED_EDGE('',*,*,#8502,.T.) ;
#11665 = ORIENTED_EDGE('',*,*,#8505,.T.) ;
#11666 = ORIENTED_EDGE('',*,*,#8500,.T.) ;
#11667 = ORIENTED_EDGE('',*,*,#8505,.F.) ;
#11668 = ORIENTED_EDGE('',*,*,#8501,.F.) ;
#11669 = ORIENTED_EDGE('',*,*,#8326,.T.) ;
#11670 = ORIENTED_EDGE('',*,*,#8392,.T.) ;
#11671 = ORIENTED_EDGE('',*,*,#8506,.F.) ;
#11672 = ORIENTED_EDGE('',*,*,#8507,.T.) ;
#11673 = ORIENTED_EDGE('',*,*,#8508,.F.) ;
#11674 = ORIENTED_EDGE('',*,*,#8509,.T.) ;
#11675 = ORIENTED_EDGE('',*,*,#8510,.F.) ;
#11676 = ORIENTED_EDGE('',*,*,#8511,.T.) ;
#11677 = ORIENTED_EDGE('',*,*,#8452,.F.) ;
#11678 = ORIENTED_EDGE('',*,*,#8506,.T.) ;
#11679 = ORIENTED_EDGE('',*,*,#8324,.F.) ;
#11680 = ORIENTED_EDGE('',*,*,#8511,.F.) ;
#11681 = ORIENTED_EDGE('',*,*,#8512,.T.) ;
#11682 = ORIENTED_EDGE('',*,*,#8507,.F.) ;
#11683 = ORIENTED_EDGE('',*,*,#8512,.F.) ;
#11684 = ORIENTED_EDGE('',*,*,#8510,.T.) ;
#11685 = ORIENTED_EDGE('',*,*,#8513,.T.) ;
#11686 = ORIENTED_EDGE('',*,*,#8508,.T.) ;
#11687 = ORIENTED_EDGE('',*,*,#8513,.F.) ;
#11688 = ORIENTED_EDGE('',*,*,#8509,.F.) ;
#11689 = ORIENTED_EDGE('',*,*,#8322,.T.) ;
#11690 = ORIENTED_EDGE('',*,*,#8393,.T.) ;
#11691 = ORIENTED_EDGE('',*,*,#8514,.F.) ;
#11692 = ORIENTED_EDGE('',*,*,#8515,.T.) ;
#11693 = ORIENTED_EDGE('',*,*,#8516,.F.) ;
#11694 = ORIENTED_EDGE('',*,*,#8517,.T.) ;
#11695 = ORIENTED_EDGE('',*,*,#8518,.F.) ;
#11696 = ORIENTED_EDGE('',*,*,#8519,.T.) ;
#11697 = ORIENTED_EDGE('',*,*,#8451,.F.) ;
#11698 = ORIENTED_EDGE('',*,*,#8514,.T.) ;
#11699 = ORIENTED_EDGE('',*,*,#8320,.F.) ;
#11700 = ORIENTED_EDGE('',*,*,#8519,.F.) ;
#11701 = ORIENTED_EDGE('',*,*,#8520,.T.) ;
#11702 = ORIENTED_EDGE('',*,*,#8515,.F.) ;
#11703 = ORIENTED_EDGE('',*,*,#8520,.F.) ;
#11704 = ORIENTED_EDGE('',*,*,#8518,.T.) ;
#11705 = ORIENTED_EDGE('',*,*,#8521,.T.) ;
#11706 = ORIENTED_EDGE('',*,*,#8516,.T.) ;
#11707 = ORIENTED_EDGE('',*,*,#8521,.F.) ;
#11708 = ORIENTED_EDGE('',*,*,#8517,.F.) ;
#11709 = ORIENTED_EDGE('',*,*,#8318,.T.) ;
#11710 = ORIENTED_EDGE('',*,*,#8394,.T.) ;
#11711 = ORIENTED_EDGE('',*,*,#8522,.F.) ;
#11712 = ORIENTED_EDGE('',*,*,#8523,.T.) ;
#11713 = ORIENTED_EDGE('',*,*,#8524,.F.) ;
#11714 = ORIENTED_EDGE('',*,*,#8525,.T.) ;
#11715 = ORIENTED_EDGE('',*,*,#8526,.F.) ;
#11716 = ORIENTED_EDGE('',*,*,#8527,.T.) ;
#11717 = ORIENTED_EDGE('',*,*,#8450,.F.) ;
#11718 = ORIENTED_EDGE('',*,*,#8522,.T.) ;
#11719 = ORIENTED_EDGE('',*,*,#8316,.F.) ;
#11720 = ORIENTED_EDGE('',*,*,#8527,.F.) ;
#11721 = ORIENTED_EDGE('',*,*,#8528,.T.) ;
#11722 = ORIENTED_EDGE('',*,*,#8523,.F.) ;
#11723 = ORIENTED_EDGE('',*,*,#8528,.F.) ;
#11724 = ORIENTED_EDGE('',*,*,#8526,.T.) ;
#11725 = ORIENTED_EDGE('',*,*,#8529,.T.) ;
#11726 = ORIENTED_EDGE('',*,*,#8524,.T.) ;
#11727 = ORIENTED_EDGE('',*,*,#8529,.F.) ;
#11728 = ORIENTED_EDGE('',*,*,#8525,.F.) ;
#11729 = ORIENTED_EDGE('',*,*,#8314,.T.) ;
#11730 = ORIENTED_EDGE('',*,*,#8395,.T.) ;
#11731 = ORIENTED_EDGE('',*,*,#8530,.F.) ;
#11732 = ORIENTED_EDGE('',*,*,#8531,.T.) ;
#11733 = ORIENTED_EDGE('',*,*,#8532,.F.) ;
#11734 = ORIENTED_EDGE('',*,*,#8533,.T.) ;
#11735 = ORIENTED_EDGE('',*,*,#8534,.F.) ;
#11736 = ORIENTED_EDGE('',*,*,#8535,.T.) ;
#11737 = ORIENTED_EDGE('',*,*,#8449,.F.) ;
#11738 = ORIENTED_EDGE('',*,*,#8530,.T.) ;
#11739 = ORIENTED_EDGE('',*,*,#8312,.F.) ;
#11740 = ORIENTED_EDGE('',*,*,#8535,.F.) ;
#11741 = ORIENTED_EDGE('',*,*,#8536,.T.) ;
#11742 = ORIENTED_EDGE('',*,*,#8531,.F.) ;
#11743 = ORIENTED_EDGE('',*,*,#8536,.F.) ;
#11744 = ORIENTED_EDGE('',*,*,#8534,.T.) ;
#11745 = ORIENTED_EDGE('',*,*,#8537,.T.) ;
#11746 = ORIENTED_EDGE('',*,*,#8532,.T.) ;
#11747 = ORIENTED_EDGE('',*,*,#8537,.F.) ;
#11748 = ORIENTED_EDGE('',*,*,#8533,.F.) ;
#11749 = ORIENTED_EDGE('',*,*,#8310,.T.) ;
#11750 = ORIENTED_EDGE('',*,*,#8396,.T.) ;
#11751 = ORIENTED_EDGE('',*,*,#8538,.F.) ;
#11752 = ORIENTED_EDGE('',*,*,#8539,.T.) ;
#11753 = ORIENTED_EDGE('',*,*,#8540,.F.) ;
#11754 = ORIENTED_EDGE('',*,*,#8541,.T.) ;
#11755 = ORIENTED_EDGE('',*,*,#8542,.F.) ;
#11756 = ORIENTED_EDGE('',*,*,#8543,.T.) ;
#11757 = ORIENTED_EDGE('',*,*,#8448,.F.) ;
#11758 = ORIENTED_EDGE('',*,*,#8538,.T.) ;
#11759 = ORIENTED_EDGE('',*,*,#8308,.F.) ;
#11760 = ORIENTED_EDGE('',*,*,#8543,.F.) ;
#11761 = ORIENTED_EDGE('',*,*,#8544,.T.) ;
#11762 = ORIENTED_EDGE('',*,*,#8539,.F.) ;
#11763 = ORIENTED_EDGE('',*,*,#8544,.F.) ;
#11764 = ORIENTED_EDGE('',*,*,#8542,.T.) ;
#11765 = ORIENTED_EDGE('',*,*,#8545,.T.) ;
#11766 = ORIENTED_EDGE('',*,*,#8540,.T.) ;
#11767 = ORIENTED_EDGE('',*,*,#8545,.F.) ;
#11768 = ORIENTED_EDGE('',*,*,#8541,.F.) ;
#11769 = ORIENTED_EDGE('',*,*,#8306,.T.) ;
#11770 = ORIENTED_EDGE('',*,*,#8398,.T.) ;
#11771 = ORIENTED_EDGE('',*,*,#8546,.F.) ;
#11772 = ORIENTED_EDGE('',*,*,#8547,.T.) ;
#11773 = ORIENTED_EDGE('',*,*,#8548,.F.) ;
#11774 = ORIENTED_EDGE('',*,*,#8549,.T.) ;
#11775 = ORIENTED_EDGE('',*,*,#8550,.F.) ;
#11776 = ORIENTED_EDGE('',*,*,#8551,.T.) ;
#11777 = ORIENTED_EDGE('',*,*,#8446,.F.) ;
#11778 = ORIENTED_EDGE('',*,*,#8546,.T.) ;
#11779 = ORIENTED_EDGE('',*,*,#8297,.F.) ;
#11780 = ORIENTED_EDGE('',*,*,#8551,.F.) ;
#11781 = ORIENTED_EDGE('',*,*,#8552,.T.) ;
#11782 = ORIENTED_EDGE('',*,*,#8547,.F.) ;
#11783 = ORIENTED_EDGE('',*,*,#8552,.F.) ;
#11784 = ORIENTED_EDGE('',*,*,#8550,.T.) ;
#11785 = ORIENTED_EDGE('',*,*,#8553,.T.) ;
#11786 = ORIENTED_EDGE('',*,*,#8548,.T.) ;
#11787 = ORIENTED_EDGE('',*,*,#8553,.F.) ;
#11788 = ORIENTED_EDGE('',*,*,#8549,.F.) ;
#11789 = ORIENTED_EDGE('',*,*,#8302,.T.) ;
#11790 = ORIENTED_EDGE('',*,*,#8397,.T.) ;
#11791 = ORIENTED_EDGE('',*,*,#8554,.F.) ;
#11792 = ORIENTED_EDGE('',*,*,#8555,.T.) ;
#11793 = ORIENTED_EDGE('',*,*,#8556,.F.) ;
#11794 = ORIENTED_EDGE('',*,*,#8557,.T.) ;
#11795 = ORIENTED_EDGE('',*,*,#8558,.F.) ;
#11796 = ORIENTED_EDGE('',*,*,#8559,.T.) ;
#11797 = ORIENTED_EDGE('',*,*,#8447,.F.) ;
#11798 = ORIENTED_EDGE('',*,*,#8554,.T.) ;
#11799 = ORIENTED_EDGE('',*,*,#8304,.F.) ;
#11800 = ORIENTED_EDGE('',*,*,#8559,.F.) ;
#11801 = ORIENTED_EDGE('',*,*,#8560,.T.) ;
#11802 = ORIENTED_EDGE('',*,*,#8555,.F.) ;
#11803 = ORIENTED_EDGE('',*,*,#8560,.F.) ;
#11804 = ORIENTED_EDGE('',*,*,#8558,.T.) ;
#11805 = ORIENTED_EDGE('',*,*,#8561,.T.) ;
#11806 = ORIENTED_EDGE('',*,*,#8556,.T.) ;
#11807 = ORIENTED_EDGE('',*,*,#8561,.F.) ;
#11808 = ORIENTED_EDGE('',*,*,#8557,.F.) ;
#11809 = ORIENTED_EDGE('',*,*,#8295,.T.) ;
#11810 = ORIENTED_EDGE('',*,*,#8399,.T.) ;
#11811 = ORIENTED_EDGE('',*,*,#8562,.F.) ;
#11812 = ORIENTED_EDGE('',*,*,#8563,.T.) ;
#11813 = ORIENTED_EDGE('',*,*,#8564,.F.) ;
#11814 = ORIENTED_EDGE('',*,*,#8565,.T.) ;
#11815 = ORIENTED_EDGE('',*,*,#8566,.F.) ;
#11816 = ORIENTED_EDGE('',*,*,#8567,.T.) ;
#11817 = ORIENTED_EDGE('',*,*,#8445,.F.) ;
#11818 = ORIENTED_EDGE('',*,*,#8562,.T.) ;
#11819 = ORIENTED_EDGE('',*,*,#8300,.F.) ;
#11820 = ORIENTED_EDGE('',*,*,#8567,.F.) ;
#11821 = ORIENTED_EDGE('',*,*,#8568,.T.) ;
#11822 = ORIENTED_EDGE('',*,*,#8563,.F.) ;
#11823 = ORIENTED_EDGE('',*,*,#8568,.F.) ;
#11824 = ORIENTED_EDGE('',*,*,#8566,.T.) ;
#11825 = ORIENTED_EDGE('',*,*,#8569,.T.) ;
#11826 = ORIENTED_EDGE('',*,*,#8564,.T.) ;
#11827 = ORIENTED_EDGE('',*,*,#8569,.F.) ;
#11828 = ORIENTED_EDGE('',*,*,#8565,.F.) ;
#11829 = ORIENTED_EDGE('',*,*,#8294,.T.) ;
#11830 = ORIENTED_EDGE('',*,*,#8400,.T.) ;
#11831 = ORIENTED_EDGE('',*,*,#8570,.F.) ;
#11832 = ORIENTED_EDGE('',*,*,#8571,.T.) ;
#11833 = ORIENTED_EDGE('',*,*,#8572,.F.) ;
#11834 = ORIENTED_EDGE('',*,*,#8573,.T.) ;
#11835 = ORIENTED_EDGE('',*,*,#8574,.F.) ;
#11836 = ORIENTED_EDGE('',*,*,#8575,.T.) ;
#11837 = ORIENTED_EDGE('',*,*,#8444,.F.) ;
#11838 = ORIENTED_EDGE('',*,*,#8570,.T.) ;
#11839 = ORIENTED_EDGE('',*,*,#8292,.F.) ;
#11840 = ORIENTED_EDGE('',*,*,#8575,.F.) ;
#11841 = ORIENTED_EDGE('',*,*,#8576,.T.) ;
#11842 = ORIENTED_EDGE('',*,*,#8571,.F.) ;
#11843 = ORIENTED_EDGE('',*,*,#8576,.F.) ;
#11844 = ORIENTED_EDGE('',*,*,#8574,.T.) ;
#11845 = ORIENTED_EDGE('',*,*,#8577,.T.) ;
#11846 = ORIENTED_EDGE('',*,*,#8572,.T.) ;
#11847 = ORIENTED_EDGE('',*,*,#8577,.F.) ;
#11848 = ORIENTED_EDGE('',*,*,#8573,.F.) ;
#11849 = ORIENTED_EDGE('',*,*,#8290,.T.) ;
#11850 = ORIENTED_EDGE('',*,*,#8401,.T.) ;
#11851 = ORIENTED_EDGE('',*,*,#8578,.F.) ;
#11852 = ORIENTED_EDGE('',*,*,#8579,.T.) ;
#11853 = ORIENTED_EDGE('',*,*,#8580,.F.) ;
#11854 = ORIENTED_EDGE('',*,*,#8581,.T.) ;
#11855 = ORIENTED_EDGE('',*,*,#8582,.F.) ;
#11856 = ORIENTED_EDGE('',*,*,#8583,.T.) ;
#11857 = ORIENTED_EDGE('',*,*,#8443,.F.) ;
#11858 = ORIENTED_EDGE('',*,*,#8578,.T.) ;
#11859 = ORIENTED_EDGE('',*,*,#8288,.F.) ;
#11860 = ORIENTED_EDGE('',*,*,#8583,.F.) ;
#11861 = ORIENTED_EDGE('',*,*,#8584,.T.) ;
#11862 = ORIENTED_EDGE('',*,*,#8579,.F.) ;
#11863 = ORIENTED_EDGE('',*,*,#8584,.F.) ;
#11864 = ORIENTED_EDGE('',*,*,#8582,.T.) ;
#11865 = ORIENTED_EDGE('',*,*,#8585,.T.) ;
#11866 = ORIENTED_EDGE('',*,*,#8580,.T.) ;
#11867 = ORIENTED_EDGE('',*,*,#8585,.F.) ;
#11868 = ORIENTED_EDGE('',*,*,#8581,.F.) ;
#11869 = ORIENTED_EDGE('',*,*,#8286,.T.) ;
#11870 = ORIENTED_EDGE('',*,*,#8402,.T.) ;
#11871 = ORIENTED_EDGE('',*,*,#8586,.F.) ;
#11872 = ORIENTED_EDGE('',*,*,#8587,.T.) ;
#11873 = ORIENTED_EDGE('',*,*,#8588,.F.) ;
#11874 = ORIENTED_EDGE('',*,*,#8589,.T.) ;
#11875 = ORIENTED_EDGE('',*,*,#8590,.F.) ;
#11876 = ORIENTED_EDGE('',*,*,#8591,.T.) ;
#11877 = ORIENTED_EDGE('',*,*,#8442,.F.) ;
#11878 = ORIENTED_EDGE('',*,*,#8586,.T.) ;
#11879 = ORIENTED_EDGE('',*,*,#8284,.F.) ;
#11880 = ORIENTED_EDGE('',*,*,#8591,.F.) ;
#11881 = ORIENTED_EDGE('',*,*,#8592,.T.) ;
#11882 = ORIENTED_EDGE('',*,*,#8587,.F.) ;
#11883 = ORIENTED_EDGE('',*,*,#8592,.F.) ;
#11884 = ORIENTED_EDGE('',*,*,#8590,.T.) ;
#11885 = ORIENTED_EDGE('',*,*,#8593,.T.) ;
#11886 = ORIENTED_EDGE('',*,*,#8588,.T.) ;
#11887 = ORIENTED_EDGE('',*,*,#8593,.F.) ;
#11888 = ORIENTED_EDGE('',*,*,#8589,.F.) ;
#11889 = ORIENTED_EDGE('',*,*,#8282,.T.) ;
#11890 = ORIENTED_EDGE('',*,*,#8403,.T.) ;
#11891 = ORIENTED_EDGE('',*,*,#8594,.F.) ;
#11892 = ORIENTED_EDGE('',*,*,#8595,.T.) ;
#11893 = ORIENTED_EDGE('',*,*,#8596,.F.) ;
#11894 = ORIENTED_EDGE('',*,*,#8597,.T.) ;
#11895 = ORIENTED_EDGE('',*,*,#8598,.F.) ;
#11896 = ORIENTED_EDGE('',*,*,#8599,.T.) ;
#11897 = ORIENTED_EDGE('',*,*,#8441,.F.) ;
#11898 = ORIENTED_EDGE('',*,*,#8594,.T.) ;
#11899 = ORIENTED_EDGE('',*,*,#8280,.F.) ;
#11900 = ORIENTED_EDGE('',*,*,#8599,.F.) ;
#11901 = ORIENTED_EDGE('',*,*,#8600,.T.) ;
#11902 = ORIENTED_EDGE('',*,*,#8595,.F.) ;
#11903 = ORIENTED_EDGE('',*,*,#8600,.F.) ;
#11904 = ORIENTED_EDGE('',*,*,#8598,.T.) ;
#11905 = ORIENTED_EDGE('',*,*,#8601,.T.) ;
#11906 = ORIENTED_EDGE('',*,*,#8596,.T.) ;
#11907 = ORIENTED_EDGE('',*,*,#8601,.F.) ;
#11908 = ORIENTED_EDGE('',*,*,#8597,.F.) ;
#11909 = ORIENTED_EDGE('',*,*,#8278,.T.) ;
#11910 = ORIENTED_EDGE('',*,*,#8404,.T.) ;
#11911 = ORIENTED_EDGE('',*,*,#8602,.F.) ;
#11912 = ORIENTED_EDGE('',*,*,#8603,.T.) ;
#11913 = ORIENTED_EDGE('',*,*,#8604,.F.) ;
#11914 = ORIENTED_EDGE('',*,*,#8605,.T.) ;
#11915 = ORIENTED_EDGE('',*,*,#8606,.F.) ;
#11916 = ORIENTED_EDGE('',*,*,#8607,.T.) ;
#11917 = ORIENTED_EDGE('',*,*,#8440,.F.) ;
#11918 = ORIENTED_EDGE('',*,*,#8602,.T.) ;
#11919 = ORIENTED_EDGE('',*,*,#8276,.F.) ;
#11920 = ORIENTED_EDGE('',*,*,#8607,.F.) ;
#11921 = ORIENTED_EDGE('',*,*,#8608,.T.) ;
#11922 = ORIENTED_EDGE('',*,*,#8603,.F.) ;
#11923 = ORIENTED_EDGE('',*,*,#8608,.F.) ;
#11924 = ORIENTED_EDGE('',*,*,#8606,.T.) ;
#11925 = ORIENTED_EDGE('',*,*,#8609,.T.) ;
#11926 = ORIENTED_EDGE('',*,*,#8604,.T.) ;
#11927 = ORIENTED_EDGE('',*,*,#8609,.F.) ;
#11928 = ORIENTED_EDGE('',*,*,#8605,.F.) ;
#11929 = ORIENTED_EDGE('',*,*,#8274,.T.) ;
#11930 = ORIENTED_EDGE('',*,*,#8345,.T.) ;
#11931 = ORIENTED_EDGE('',*,*,#8405,.T.) ;
#11932 = ORIENTED_EDGE('',*,*,#8610,.F.) ;
#11933 = ORIENTED_EDGE('',*,*,#8611,.T.) ;
#11934 = ORIENTED_EDGE('',*,*,#8612,.F.) ;
#11935 = ORIENTED_EDGE('',*,*,#8613,.T.) ;
#11936 = ORIENTED_EDGE('',*,*,#8614,.F.) ;
#11937 = ORIENTED_EDGE('',*,*,#8615,.T.) ;
#11938 = ORIENTED_EDGE('',*,*,#8439,.F.) ;
#11939 = ORIENTED_EDGE('',*,*,#8610,.T.) ;
#11940 = ORIENTED_EDGE('',*,*,#8272,.F.) ;
#11941 = ORIENTED_EDGE('',*,*,#8615,.F.) ;
#11942 = ORIENTED_EDGE('',*,*,#8616,.T.) ;
#11943 = ORIENTED_EDGE('',*,*,#8611,.F.) ;
#11944 = ORIENTED_EDGE('',*,*,#8616,.F.) ;
#11945 = ORIENTED_EDGE('',*,*,#8614,.T.) ;
#11946 = ORIENTED_EDGE('',*,*,#8617,.T.) ;
#11947 = ORIENTED_EDGE('',*,*,#8612,.T.) ;
#11948 = ORIENTED_EDGE('',*,*,#8617,.F.) ;
#11949 = ORIENTED_EDGE('',*,*,#8613,.F.) ;
#11950 = ORIENTED_EDGE('',*,*,#8270,.T.) ;
#11951 = ORIENTED_EDGE('',*,*,#8346,.T.) ;
#11952 = ORIENTED_EDGE('',*,*,#8618,.F.) ;
#11953 = ORIENTED_EDGE('',*,*,#8619,.T.) ;
#11954 = ORIENTED_EDGE('',*,*,#8620,.F.) ;
#11955 = ORIENTED_EDGE('',*,*,#8621,.T.) ;
#11956 = ORIENTED_EDGE('',*,*,#8622,.F.) ;
#11957 = ORIENTED_EDGE('',*,*,#8623,.T.) ;
#11958 = ORIENTED_EDGE('',*,*,#8438,.F.) ;
#11959 = ORIENTED_EDGE('',*,*,#8618,.T.) ;
#11960 = ORIENTED_EDGE('',*,*,#8268,.F.) ;
#11961 = ORIENTED_EDGE('',*,*,#8623,.F.) ;
#11962 = ORIENTED_EDGE('',*,*,#8624,.T.) ;
#11963 = ORIENTED_EDGE('',*,*,#8619,.F.) ;
#11964 = ORIENTED_EDGE('',*,*,#8624,.F.) ;
#11965 = ORIENTED_EDGE('',*,*,#8622,.T.) ;
#11966 = ORIENTED_EDGE('',*,*,#8625,.T.) ;
#11967 = ORIENTED_EDGE('',*,*,#8620,.T.) ;
#11968 = ORIENTED_EDGE('',*,*,#8625,.F.) ;
#11969 = ORIENTED_EDGE('',*,*,#8621,.F.) ;
#11970 = ORIENTED_EDGE('',*,*,#8266,.T.) ;
#11971 = ORIENTED_EDGE('',*,*,#8347,.T.) ;
#11972 = ORIENTED_EDGE('',*,*,#8626,.F.) ;
#11973 = ORIENTED_EDGE('',*,*,#8627,.T.) ;
#11974 = ORIENTED_EDGE('',*,*,#8628,.F.) ;
#11975 = ORIENTED_EDGE('',*,*,#8629,.T.) ;
#11976 = ORIENTED_EDGE('',*,*,#8630,.F.) ;
#11977 = ORIENTED_EDGE('',*,*,#8631,.T.) ;
#11978 = ORIENTED_EDGE('',*,*,#8437,.F.) ;
#11979 = ORIENTED_EDGE('',*,*,#8626,.T.) ;
#11980 = ORIENTED_EDGE('',*,*,#8264,.F.) ;
#11981 = ORIENTED_EDGE('',*,*,#8631,.F.) ;
#11982 = ORIENTED_EDGE('',*,*,#8632,.T.) ;
#11983 = ORIENTED_EDGE('',*,*,#8627,.F.) ;
#11984 = ORIENTED_EDGE('',*,*,#8632,.F.) ;
#11985 = ORIENTED_EDGE('',*,*,#8630,.T.) ;
#11986 = ORIENTED_EDGE('',*,*,#8633,.T.) ;
#11987 = ORIENTED_EDGE('',*,*,#8628,.T.) ;
#11988 = ORIENTED_EDGE('',*,*,#8633,.F.) ;
#11989 = ORIENTED_EDGE('',*,*,#8629,.F.) ;
#11990 = ORIENTED_EDGE('',*,*,#8262,.T.) ;
#11991 = ORIENTED_EDGE('',*,*,#8348,.T.) ;
#11992 = ORIENTED_EDGE('',*,*,#8634,.F.) ;
#11993 = ORIENTED_EDGE('',*,*,#8635,.T.) ;
#11994 = ORIENTED_EDGE('',*,*,#8636,.F.) ;
#11995 = ORIENTED_EDGE('',*,*,#8637,.T.) ;
#11996 = ORIENTED_EDGE('',*,*,#8638,.F.) ;
#11997 = ORIENTED_EDGE('',*,*,#8639,.T.) ;
#11998 = ORIENTED_EDGE('',*,*,#8436,.F.) ;
#11999 = ORIENTED_EDGE('',*,*,#8634,.T.) ;
#12000 = ORIENTED_EDGE('',*,*,#8260,.F.) ;
#12001 = ORIENTED_EDGE('',*,*,#8639,.F.) ;
#12002 = ORIENTED_EDGE('',*,*,#8640,.T.) ;
#12003 = ORIENTED_EDGE('',*,*,#8635,.F.) ;
#12004 = ORIENTED_EDGE('',*,*,#8640,.F.) ;
#12005 = ORIENTED_EDGE('',*,*,#8638,.T.) ;
#12006 = ORIENTED_EDGE('',*,*,#8641,.T.) ;
#12007 = ORIENTED_EDGE('',*,*,#8636,.T.) ;
#12008 = ORIENTED_EDGE('',*,*,#8641,.F.) ;
#12009 = ORIENTED_EDGE('',*,*,#8637,.F.) ;
#12010 = ORIENTED_EDGE('',*,*,#8258,.T.) ;
#12011 = ORIENTED_EDGE('',*,*,#8356,.T.) ;
#12012 = ORIENTED_EDGE('',*,*,#8642,.F.) ;
#12013 = ORIENTED_EDGE('',*,*,#8643,.T.) ;
#12014 = ORIENTED_EDGE('',*,*,#8644,.F.) ;
#12015 = ORIENTED_EDGE('',*,*,#8645,.T.) ;
#12016 = ORIENTED_EDGE('',*,*,#8646,.F.) ;
#12017 = ORIENTED_EDGE('',*,*,#8647,.T.) ;
#12018 = ORIENTED_EDGE('',*,*,#8428,.F.) ;
#12019 = ORIENTED_EDGE('',*,*,#8642,.T.) ;
#12020 = ORIENTED_EDGE('',*,*,#8249,.F.) ;
#12021 = ORIENTED_EDGE('',*,*,#8647,.F.) ;
#12022 = ORIENTED_EDGE('',*,*,#8648,.T.) ;
#12023 = ORIENTED_EDGE('',*,*,#8643,.F.) ;
#12024 = ORIENTED_EDGE('',*,*,#8648,.F.) ;
#12025 = ORIENTED_EDGE('',*,*,#8646,.T.) ;
#12026 = ORIENTED_EDGE('',*,*,#8649,.T.) ;
#12027 = ORIENTED_EDGE('',*,*,#8644,.T.) ;
#12028 = ORIENTED_EDGE('',*,*,#8649,.F.) ;
#12029 = ORIENTED_EDGE('',*,*,#8645,.F.) ;
#12030 = ORIENTED_EDGE('',*,*,#8254,.T.) ;
#12031 = ORIENTED_EDGE('',*,*,#8355,.T.) ;
#12032 = ORIENTED_EDGE('',*,*,#8650,.F.) ;
#12033 = ORIENTED_EDGE('',*,*,#8651,.T.) ;
#12034 = ORIENTED_EDGE('',*,*,#8652,.F.) ;
#12035 = ORIENTED_EDGE('',*,*,#8653,.T.) ;
#12036 = ORIENTED_EDGE('',*,*,#8654,.F.) ;
#12037 = ORIENTED_EDGE('',*,*,#8655,.T.) ;
#12038 = ORIENTED_EDGE('',*,*,#8429,.F.) ;
#12039 = ORIENTED_EDGE('',*,*,#8650,.T.) ;
#12040 = ORIENTED_EDGE('',*,*,#8245,.F.) ;
#12041 = ORIENTED_EDGE('',*,*,#8655,.F.) ;
#12042 = ORIENTED_EDGE('',*,*,#8656,.T.) ;
#12043 = ORIENTED_EDGE('',*,*,#8651,.F.) ;
#12044 = ORIENTED_EDGE('',*,*,#8656,.F.) ;
#12045 = ORIENTED_EDGE('',*,*,#8654,.T.) ;
#12046 = ORIENTED_EDGE('',*,*,#8657,.T.) ;
#12047 = ORIENTED_EDGE('',*,*,#8652,.T.) ;
#12048 = ORIENTED_EDGE('',*,*,#8657,.F.) ;
#12049 = ORIENTED_EDGE('',*,*,#8653,.F.) ;
#12050 = ORIENTED_EDGE('',*,*,#8247,.T.) ;
#12051 = ORIENTED_EDGE('',*,*,#8354,.T.) ;
#12052 = ORIENTED_EDGE('',*,*,#8658,.F.) ;
#12053 = ORIENTED_EDGE('',*,*,#8659,.T.) ;
#12054 = ORIENTED_EDGE('',*,*,#8660,.F.) ;
#12055 = ORIENTED_EDGE('',*,*,#8661,.T.) ;
#12056 = ORIENTED_EDGE('',*,*,#8662,.F.) ;
#12057 = ORIENTED_EDGE('',*,*,#8663,.T.) ;
#12058 = ORIENTED_EDGE('',*,*,#8430,.F.) ;
#12059 = ORIENTED_EDGE('',*,*,#8658,.T.) ;
#12060 = ORIENTED_EDGE('',*,*,#8241,.F.) ;
#12061 = ORIENTED_EDGE('',*,*,#8663,.F.) ;
#12062 = ORIENTED_EDGE('',*,*,#8664,.T.) ;
#12063 = ORIENTED_EDGE('',*,*,#8659,.F.) ;
#12064 = ORIENTED_EDGE('',*,*,#8664,.F.) ;
#12065 = ORIENTED_EDGE('',*,*,#8662,.T.) ;
#12066 = ORIENTED_EDGE('',*,*,#8665,.T.) ;
#12067 = ORIENTED_EDGE('',*,*,#8660,.T.) ;
#12068 = ORIENTED_EDGE('',*,*,#8665,.F.) ;
#12069 = ORIENTED_EDGE('',*,*,#8661,.F.) ;
#12070 = ORIENTED_EDGE('',*,*,#8243,.T.) ;
#12071 = ORIENTED_EDGE('',*,*,#8353,.T.) ;
#12072 = ORIENTED_EDGE('',*,*,#8666,.F.) ;
#12073 = ORIENTED_EDGE('',*,*,#8667,.T.) ;
#12074 = ORIENTED_EDGE('',*,*,#8668,.F.) ;
#12075 = ORIENTED_EDGE('',*,*,#8669,.T.) ;
#12076 = ORIENTED_EDGE('',*,*,#8670,.F.) ;
#12077 = ORIENTED_EDGE('',*,*,#8671,.T.) ;
#12078 = ORIENTED_EDGE('',*,*,#8431,.F.) ;
#12079 = ORIENTED_EDGE('',*,*,#8666,.T.) ;
#12080 = ORIENTED_EDGE('',*,*,#8237,.F.) ;
#12081 = ORIENTED_EDGE('',*,*,#8671,.F.) ;
#12082 = ORIENTED_EDGE('',*,*,#8672,.T.) ;
#12083 = ORIENTED_EDGE('',*,*,#8667,.F.) ;
#12084 = ORIENTED_EDGE('',*,*,#8672,.F.) ;
#12085 = ORIENTED_EDGE('',*,*,#8670,.T.) ;
#12086 = ORIENTED_EDGE('',*,*,#8673,.T.) ;
#12087 = ORIENTED_EDGE('',*,*,#8668,.T.) ;
#12088 = ORIENTED_EDGE('',*,*,#8673,.F.) ;
#12089 = ORIENTED_EDGE('',*,*,#8669,.F.) ;
#12090 = ORIENTED_EDGE('',*,*,#8239,.T.) ;
#12091 = ORIENTED_EDGE('',*,*,#8352,.T.) ;
#12092 = ORIENTED_EDGE('',*,*,#8674,.F.) ;
#12093 = ORIENTED_EDGE('',*,*,#8675,.T.) ;
#12094 = ORIENTED_EDGE('',*,*,#8676,.F.) ;
#12095 = ORIENTED_EDGE('',*,*,#8677,.T.) ;
#12096 = ORIENTED_EDGE('',*,*,#8678,.F.) ;
#12097 = ORIENTED_EDGE('',*,*,#8679,.T.) ;
#12098 = ORIENTED_EDGE('',*,*,#8432,.F.) ;
#12099 = ORIENTED_EDGE('',*,*,#8674,.T.) ;
#12100 = ORIENTED_EDGE('',*,*,#8233,.F.) ;
#12101 = ORIENTED_EDGE('',*,*,#8679,.F.) ;
#12102 = ORIENTED_EDGE('',*,*,#8680,.T.) ;
#12103 = ORIENTED_EDGE('',*,*,#8675,.F.) ;
#12104 = ORIENTED_EDGE('',*,*,#8680,.F.) ;
#12105 = ORIENTED_EDGE('',*,*,#8678,.T.) ;
#12106 = ORIENTED_EDGE('',*,*,#8681,.T.) ;
#12107 = ORIENTED_EDGE('',*,*,#8676,.T.) ;
#12108 = ORIENTED_EDGE('',*,*,#8681,.F.) ;
#12109 = ORIENTED_EDGE('',*,*,#8677,.F.) ;
#12110 = ORIENTED_EDGE('',*,*,#8235,.T.) ;
#12111 = ORIENTED_EDGE('',*,*,#8351,.T.) ;
#12112 = ORIENTED_EDGE('',*,*,#8682,.F.) ;
#12113 = ORIENTED_EDGE('',*,*,#8683,.T.) ;
#12114 = ORIENTED_EDGE('',*,*,#8684,.F.) ;
#12115 = ORIENTED_EDGE('',*,*,#8685,.T.) ;
#12116 = ORIENTED_EDGE('',*,*,#8686,.F.) ;
#12117 = ORIENTED_EDGE('',*,*,#8687,.T.) ;
#12118 = ORIENTED_EDGE('',*,*,#8433,.F.) ;
#12119 = ORIENTED_EDGE('',*,*,#8682,.T.) ;
#12120 = ORIENTED_EDGE('',*,*,#8229,.F.) ;
#12121 = ORIENTED_EDGE('',*,*,#8687,.F.) ;
#12122 = ORIENTED_EDGE('',*,*,#8688,.T.) ;
#12123 = ORIENTED_EDGE('',*,*,#8683,.F.) ;
#12124 = ORIENTED_EDGE('',*,*,#8688,.F.) ;
#12125 = ORIENTED_EDGE('',*,*,#8686,.T.) ;
#12126 = ORIENTED_EDGE('',*,*,#8689,.T.) ;
#12127 = ORIENTED_EDGE('',*,*,#8684,.T.) ;
#12128 = ORIENTED_EDGE('',*,*,#8689,.F.) ;
#12129 = ORIENTED_EDGE('',*,*,#8685,.F.) ;
#12130 = ORIENTED_EDGE('',*,*,#8231,.T.) ;
#12131 = ORIENTED_EDGE('',*,*,#8350,.T.) ;
#12132 = ORIENTED_EDGE('',*,*,#8690,.F.) ;
#12133 = ORIENTED_EDGE('',*,*,#8691,.T.) ;
#12134 = ORIENTED_EDGE('',*,*,#8692,.F.) ;
#12135 = ORIENTED_EDGE('',*,*,#8693,.T.) ;
#12136 = ORIENTED_EDGE('',*,*,#8694,.F.) ;
#12137 = ORIENTED_EDGE('',*,*,#8695,.T.) ;
#12138 = ORIENTED_EDGE('',*,*,#8434,.F.) ;
#12139 = ORIENTED_EDGE('',*,*,#8690,.T.) ;
#12140 = ORIENTED_EDGE('',*,*,#8225,.F.) ;
#12141 = ORIENTED_EDGE('',*,*,#8695,.F.) ;
#12142 = ORIENTED_EDGE('',*,*,#8696,.T.) ;
#12143 = ORIENTED_EDGE('',*,*,#8691,.F.) ;
#12144 = ORIENTED_EDGE('',*,*,#8696,.F.) ;
#12145 = ORIENTED_EDGE('',*,*,#8694,.T.) ;
#12146 = ORIENTED_EDGE('',*,*,#8697,.T.) ;
#12147 = ORIENTED_EDGE('',*,*,#8692,.T.) ;
#12148 = ORIENTED_EDGE('',*,*,#8697,.F.) ;
#12149 = ORIENTED_EDGE('',*,*,#8693,.F.) ;
#12150 = ORIENTED_EDGE('',*,*,#8227,.T.) ;
#12151 = ORIENTED_EDGE('',*,*,#8349,.T.) ;
#12152 = ORIENTED_EDGE('',*,*,#8698,.F.) ;
#12153 = ORIENTED_EDGE('',*,*,#8699,.T.) ;
#12154 = ORIENTED_EDGE('',*,*,#8700,.F.) ;
#12155 = ORIENTED_EDGE('',*,*,#8701,.T.) ;
#12156 = ORIENTED_EDGE('',*,*,#8702,.F.) ;
#12157 = ORIENTED_EDGE('',*,*,#8703,.T.) ;
#12158 = ORIENTED_EDGE('',*,*,#8435,.F.) ;
#12159 = ORIENTED_EDGE('',*,*,#8698,.T.) ;
#12160 = ORIENTED_EDGE('',*,*,#8256,.F.) ;
#12161 = ORIENTED_EDGE('',*,*,#8703,.F.) ;
#12162 = ORIENTED_EDGE('',*,*,#8704,.T.) ;
#12163 = ORIENTED_EDGE('',*,*,#8699,.F.) ;
#12164 = ORIENTED_EDGE('',*,*,#8704,.F.) ;
#12165 = ORIENTED_EDGE('',*,*,#8702,.T.) ;
#12166 = ORIENTED_EDGE('',*,*,#8705,.T.) ;
#12167 = ORIENTED_EDGE('',*,*,#8700,.T.) ;
#12168 = ORIENTED_EDGE('',*,*,#8705,.F.) ;
#12169 = ORIENTED_EDGE('',*,*,#8701,.F.) ;
#12170 = ORIENTED_EDGE('',*,*,#8223,.T.) ;
#12171 = ORIENTED_EDGE('',*,*,#8357,.T.) ;
#12172 = ORIENTED_EDGE('',*,*,#8706,.F.) ;
#12173 = ORIENTED_EDGE('',*,*,#8707,.T.) ;
#12174 = ORIENTED_EDGE('',*,*,#8708,.F.) ;
#12175 = ORIENTED_EDGE('',*,*,#8709,.T.) ;
#12176 = ORIENTED_EDGE('',*,*,#8710,.F.) ;
#12177 = ORIENTED_EDGE('',*,*,#8711,.T.) ;
#12178 = ORIENTED_EDGE('',*,*,#8427,.F.) ;
#12179 = ORIENTED_EDGE('',*,*,#8706,.T.) ;
#12180 = ORIENTED_EDGE('',*,*,#8252,.F.) ;
#12181 = ORIENTED_EDGE('',*,*,#8711,.F.) ;
#12182 = ORIENTED_EDGE('',*,*,#8712,.T.) ;
#12183 = ORIENTED_EDGE('',*,*,#8707,.F.) ;
#12184 = ORIENTED_EDGE('',*,*,#8712,.F.) ;
#12185 = ORIENTED_EDGE('',*,*,#8710,.T.) ;
#12186 = ORIENTED_EDGE('',*,*,#8713,.T.) ;
#12187 = ORIENTED_EDGE('',*,*,#8708,.T.) ;
#12188 = ORIENTED_EDGE('',*,*,#8713,.F.) ;
#12189 = ORIENTED_EDGE('',*,*,#8709,.F.) ;
#12190 = ORIENTED_EDGE('',*,*,#8222,.T.) ;
#12191 = ORIENTED_EDGE('',*,*,#8358,.T.) ;
#12192 = ORIENTED_EDGE('',*,*,#8714,.F.) ;
#12193 = ORIENTED_EDGE('',*,*,#8715,.T.) ;
#12194 = ORIENTED_EDGE('',*,*,#8716,.F.) ;
#12195 = ORIENTED_EDGE('',*,*,#8717,.T.) ;
#12196 = ORIENTED_EDGE('',*,*,#8718,.F.) ;
#12197 = ORIENTED_EDGE('',*,*,#8719,.T.) ;
#12198 = ORIENTED_EDGE('',*,*,#8426,.F.) ;
#12199 = ORIENTED_EDGE('',*,*,#8714,.T.) ;
#12200 = ORIENTED_EDGE('',*,*,#8220,.F.) ;
#12201 = ORIENTED_EDGE('',*,*,#8719,.F.) ;
#12202 = ORIENTED_EDGE('',*,*,#8720,.T.) ;
#12203 = ORIENTED_EDGE('',*,*,#8715,.F.) ;
#12204 = ORIENTED_EDGE('',*,*,#8720,.F.) ;
#12205 = ORIENTED_EDGE('',*,*,#8718,.T.) ;
#12206 = ORIENTED_EDGE('',*,*,#8721,.T.) ;
#12207 = ORIENTED_EDGE('',*,*,#8716,.T.) ;
#12208 = ORIENTED_EDGE('',*,*,#8721,.F.) ;
#12209 = ORIENTED_EDGE('',*,*,#8717,.F.) ;
#12210 = ORIENTED_EDGE('',*,*,#8218,.T.) ;
#12211 = ORIENTED_EDGE('',*,*,#8359,.T.) ;
#12212 = ORIENTED_EDGE('',*,*,#8722,.F.) ;
#12213 = ORIENTED_EDGE('',*,*,#8723,.T.) ;
#12214 = ORIENTED_EDGE('',*,*,#8724,.F.) ;
#12215 = ORIENTED_EDGE('',*,*,#8725,.T.) ;
#12216 = ORIENTED_EDGE('',*,*,#8726,.F.) ;
#12217 = ORIENTED_EDGE('',*,*,#8727,.T.) ;
#12218 = ORIENTED_EDGE('',*,*,#8425,.F.) ;
#12219 = ORIENTED_EDGE('',*,*,#8722,.T.) ;
#12220 = ORIENTED_EDGE('',*,*,#8216,.F.) ;
#12221 = ORIENTED_EDGE('',*,*,#8727,.F.) ;
#12222 = ORIENTED_EDGE('',*,*,#8728,.T.) ;
#12223 = ORIENTED_EDGE('',*,*,#8723,.F.) ;
#12224 = ORIENTED_EDGE('',*,*,#8728,.F.) ;
#12225 = ORIENTED_EDGE('',*,*,#8726,.T.) ;
#12226 = ORIENTED_EDGE('',*,*,#8729,.T.) ;
#12227 = ORIENTED_EDGE('',*,*,#8724,.T.) ;
#12228 = ORIENTED_EDGE('',*,*,#8729,.F.) ;
#12229 = ORIENTED_EDGE('',*,*,#8725,.F.) ;
#12230 = ORIENTED_EDGE('',*,*,#8214,.T.) ;
#12231 = ORIENTED_EDGE('',*,*,#8360,.T.) ;
#12232 = ORIENTED_EDGE('',*,*,#8730,.F.) ;
#12233 = ORIENTED_EDGE('',*,*,#8731,.T.) ;
#12234 = ORIENTED_EDGE('',*,*,#8732,.F.) ;
#12235 = ORIENTED_EDGE('',*,*,#8733,.T.) ;
#12236 = ORIENTED_EDGE('',*,*,#8734,.F.) ;
#12237 = ORIENTED_EDGE('',*,*,#8735,.T.) ;
#12238 = ORIENTED_EDGE('',*,*,#8424,.F.) ;
#12239 = ORIENTED_EDGE('',*,*,#8730,.T.) ;
#12240 = ORIENTED_EDGE('',*,*,#8212,.F.) ;
#12241 = ORIENTED_EDGE('',*,*,#8735,.F.) ;
#12242 = ORIENTED_EDGE('',*,*,#8736,.T.) ;
#12243 = ORIENTED_EDGE('',*,*,#8731,.F.) ;
#12244 = ORIENTED_EDGE('',*,*,#8736,.F.) ;
#12245 = ORIENTED_EDGE('',*,*,#8734,.T.) ;
#12246 = ORIENTED_EDGE('',*,*,#8737,.T.) ;
#12247 = ORIENTED_EDGE('',*,*,#8732,.T.) ;
#12248 = ORIENTED_EDGE('',*,*,#8737,.F.) ;
#12249 = ORIENTED_EDGE('',*,*,#8733,.F.) ;
#12250 = ORIENTED_EDGE('',*,*,#8210,.T.) ;
#12251 = ORIENTED_EDGE('',*,*,#8361,.T.) ;
#12252 = ORIENTED_EDGE('',*,*,#8738,.F.) ;
#12253 = ORIENTED_EDGE('',*,*,#8739,.T.) ;
#12254 = ORIENTED_EDGE('',*,*,#8740,.F.) ;
#12255 = ORIENTED_EDGE('',*,*,#8741,.T.) ;
#12256 = ORIENTED_EDGE('',*,*,#8742,.F.) ;
#12257 = ORIENTED_EDGE('',*,*,#8743,.T.) ;
#12258 = ORIENTED_EDGE('',*,*,#8423,.F.) ;
#12259 = ORIENTED_EDGE('',*,*,#8738,.T.) ;
#12260 = ORIENTED_EDGE('',*,*,#8208,.F.) ;
#12261 = ORIENTED_EDGE('',*,*,#8743,.F.) ;
#12262 = ORIENTED_EDGE('',*,*,#8744,.T.) ;
#12263 = ORIENTED_EDGE('',*,*,#8739,.F.) ;
#12264 = ORIENTED_EDGE('',*,*,#8744,.F.) ;
#12265 = ORIENTED_EDGE('',*,*,#8742,.T.) ;
#12266 = ORIENTED_EDGE('',*,*,#8745,.T.) ;
#12267 = ORIENTED_EDGE('',*,*,#8740,.T.) ;
#12268 = ORIENTED_EDGE('',*,*,#8745,.F.) ;
#12269 = ORIENTED_EDGE('',*,*,#8741,.F.) ;
#12270 = ORIENTED_EDGE('',*,*,#8206,.T.) ;
#12271 = ORIENTED_EDGE('',*,*,#8362,.T.) ;
#12272 = ORIENTED_EDGE('',*,*,#8746,.F.) ;
#12273 = ORIENTED_EDGE('',*,*,#8747,.T.) ;
#12274 = ORIENTED_EDGE('',*,*,#8748,.F.) ;
#12275 = ORIENTED_EDGE('',*,*,#8749,.T.) ;
#12276 = ORIENTED_EDGE('',*,*,#8750,.F.) ;
#12277 = ORIENTED_EDGE('',*,*,#8751,.T.) ;
#12278 = ORIENTED_EDGE('',*,*,#8422,.F.) ;
#12279 = ORIENTED_EDGE('',*,*,#8746,.T.) ;
#12280 = ORIENTED_EDGE('',*,*,#8204,.F.) ;
#12281 = ORIENTED_EDGE('',*,*,#8751,.F.) ;
#12282 = ORIENTED_EDGE('',*,*,#8752,.T.) ;
#12283 = ORIENTED_EDGE('',*,*,#8747,.F.) ;
#12284 = ORIENTED_EDGE('',*,*,#8752,.F.) ;
#12285 = ORIENTED_EDGE('',*,*,#8750,.T.) ;
#12286 = ORIENTED_EDGE('',*,*,#8753,.T.) ;
#12287 = ORIENTED_EDGE('',*,*,#8748,.T.) ;
#12288 = ORIENTED_EDGE('',*,*,#8753,.F.) ;
#12289 = ORIENTED_EDGE('',*,*,#8749,.F.) ;
#12290 = ORIENTED_EDGE('',*,*,#8202,.T.) ;
#12291 = ORIENTED_EDGE('',*,*,#8363,.T.) ;
#12292 = ORIENTED_EDGE('',*,*,#8754,.F.) ;
#12293 = ORIENTED_EDGE('',*,*,#8755,.T.) ;
#12294 = ORIENTED_EDGE('',*,*,#8756,.F.) ;
#12295 = ORIENTED_EDGE('',*,*,#8757,.T.) ;
#12296 = ORIENTED_EDGE('',*,*,#8758,.F.) ;
#12297 = ORIENTED_EDGE('',*,*,#8759,.T.) ;
#12298 = ORIENTED_EDGE('',*,*,#8421,.F.) ;
#12299 = ORIENTED_EDGE('',*,*,#8754,.T.) ;
#12300 = ORIENTED_EDGE('',*,*,#8200,.F.) ;
#12301 = ORIENTED_EDGE('',*,*,#8759,.F.) ;
#12302 = ORIENTED_EDGE('',*,*,#8760,.T.) ;
#12303 = ORIENTED_EDGE('',*,*,#8755,.F.) ;
#12304 = ORIENTED_EDGE('',*,*,#8760,.F.) ;
#12305 = ORIENTED_EDGE('',*,*,#8758,.T.) ;
#12306 = ORIENTED_EDGE('',*,*,#8761,.T.) ;
#12307 = ORIENTED_EDGE('',*,*,#8756,.T.) ;
#12308 = ORIENTED_EDGE('',*,*,#8761,.F.) ;
#12309 = ORIENTED_EDGE('',*,*,#8757,.F.) ;
#12310 = ORIENTED_EDGE('',*,*,#8198,.T.) ;
#12311 = ORIENTED_EDGE('',*,*,#8364,.T.) ;
#12312 = ORIENTED_EDGE('',*,*,#8762,.F.) ;
#12313 = ORIENTED_EDGE('',*,*,#8763,.T.) ;
#12314 = ORIENTED_EDGE('',*,*,#8764,.F.) ;
#12315 = ORIENTED_EDGE('',*,*,#8765,.T.) ;
#12316 = ORIENTED_EDGE('',*,*,#8766,.F.) ;
#12317 = ORIENTED_EDGE('',*,*,#8767,.T.) ;
#12318 = ORIENTED_EDGE('',*,*,#8420,.F.) ;
#12319 = ORIENTED_EDGE('',*,*,#8762,.T.) ;
#12320 = ORIENTED_EDGE('',*,*,#8196,.F.) ;
#12321 = ORIENTED_EDGE('',*,*,#8767,.F.) ;
#12322 = ORIENTED_EDGE('',*,*,#8768,.T.) ;
#12323 = ORIENTED_EDGE('',*,*,#8763,.F.) ;
#12324 = ORIENTED_EDGE('',*,*,#8768,.F.) ;
#12325 = ORIENTED_EDGE('',*,*,#8766,.T.) ;
#12326 = ORIENTED_EDGE('',*,*,#8769,.T.) ;
#12327 = ORIENTED_EDGE('',*,*,#8764,.T.) ;
#12328 = ORIENTED_EDGE('',*,*,#8769,.F.) ;
#12329 = ORIENTED_EDGE('',*,*,#8765,.F.) ;
#12330 = ORIENTED_EDGE('',*,*,#8194,.T.) ;
#12331 = ORIENTED_EDGE('',*,*,#8365,.T.) ;
#12332 = ORIENTED_EDGE('',*,*,#8770,.F.) ;
#12333 = ORIENTED_EDGE('',*,*,#8771,.T.) ;
#12334 = ORIENTED_EDGE('',*,*,#8772,.F.) ;
#12335 = ORIENTED_EDGE('',*,*,#8773,.T.) ;
#12336 = ORIENTED_EDGE('',*,*,#8774,.F.) ;
#12337 = ORIENTED_EDGE('',*,*,#8775,.T.) ;
#12338 = ORIENTED_EDGE('',*,*,#8419,.F.) ;
#12339 = ORIENTED_EDGE('',*,*,#8770,.T.) ;
#12340 = ORIENTED_EDGE('',*,*,#8192,.F.) ;
#12341 = ORIENTED_EDGE('',*,*,#8775,.F.) ;
#12342 = ORIENTED_EDGE('',*,*,#8776,.T.) ;
#12343 = ORIENTED_EDGE('',*,*,#8771,.F.) ;
#12344 = ORIENTED_EDGE('',*,*,#8776,.F.) ;
#12345 = ORIENTED_EDGE('',*,*,#8774,.T.) ;
#12346 = ORIENTED_EDGE('',*,*,#8777,.T.) ;
#12347 = ORIENTED_EDGE('',*,*,#8772,.T.) ;
#12348 = ORIENTED_EDGE('',*,*,#8777,.F.) ;
#12349 = ORIENTED_EDGE('',*,*,#8773,.F.) ;
#12350 = ORIENTED_EDGE('',*,*,#8190,.T.) ;
#12351 = ORIENTED_EDGE('',*,*,#8366,.T.) ;
#12352 = ORIENTED_EDGE('',*,*,#8778,.F.) ;
#12353 = ORIENTED_EDGE('',*,*,#8779,.T.) ;
#12354 = ORIENTED_EDGE('',*,*,#8780,.F.) ;
#12355 = ORIENTED_EDGE('',*,*,#8781,.T.) ;
#12356 = ORIENTED_EDGE('',*,*,#8782,.F.) ;
#12357 = ORIENTED_EDGE('',*,*,#8783,.T.) ;
#12358 = ORIENTED_EDGE('',*,*,#8418,.F.) ;
#12359 = ORIENTED_EDGE('',*,*,#8778,.T.) ;
#12360 = ORIENTED_EDGE('',*,*,#8188,.F.) ;
#12361 = ORIENTED_EDGE('',*,*,#8783,.F.) ;
#12362 = ORIENTED_EDGE('',*,*,#8784,.T.) ;
#12363 = ORIENTED_EDGE('',*,*,#8779,.F.) ;
#12364 = ORIENTED_EDGE('',*,*,#8784,.F.) ;
#12365 = ORIENTED_EDGE('',*,*,#8782,.T.) ;
#12366 = ORIENTED_EDGE('',*,*,#8785,.T.) ;
#12367 = ORIENTED_EDGE('',*,*,#8780,.T.) ;
#12368 = ORIENTED_EDGE('',*,*,#8785,.F.) ;
#12369 = ORIENTED_EDGE('',*,*,#8781,.F.) ;
#12370 = ORIENTED_EDGE('',*,*,#8186,.T.) ;
#12371 = ORIENTED_EDGE('',*,*,#8368,.T.) ;
#12372 = ORIENTED_EDGE('',*,*,#8786,.F.) ;
#12373 = ORIENTED_EDGE('',*,*,#8787,.T.) ;
#12374 = ORIENTED_EDGE('',*,*,#8788,.F.) ;
#12375 = ORIENTED_EDGE('',*,*,#8789,.T.) ;
#12376 = ORIENTED_EDGE('',*,*,#8790,.F.) ;
#12377 = ORIENTED_EDGE('',*,*,#8791,.T.) ;
#12378 = ORIENTED_EDGE('',*,*,#8416,.F.) ;
#12379 = ORIENTED_EDGE('',*,*,#8786,.T.) ;
#12380 = ORIENTED_EDGE('',*,*,#8177,.F.) ;
#12381 = ORIENTED_EDGE('',*,*,#8791,.F.) ;
#12382 = ORIENTED_EDGE('',*,*,#8792,.T.) ;
#12383 = ORIENTED_EDGE('',*,*,#8787,.F.) ;
#12384 = ORIENTED_EDGE('',*,*,#8792,.F.) ;
#12385 = ORIENTED_EDGE('',*,*,#8790,.T.) ;
#12386 = ORIENTED_EDGE('',*,*,#8793,.T.) ;
#12387 = ORIENTED_EDGE('',*,*,#8788,.T.) ;
#12388 = ORIENTED_EDGE('',*,*,#8793,.F.) ;
#12389 = ORIENTED_EDGE('',*,*,#8789,.F.) ;
#12390 = ORIENTED_EDGE('',*,*,#8182,.T.) ;
#12391 = ORIENTED_EDGE('',*,*,#8367,.T.) ;
#12392 = ORIENTED_EDGE('',*,*,#8794,.F.) ;
#12393 = ORIENTED_EDGE('',*,*,#8795,.T.) ;
#12394 = ORIENTED_EDGE('',*,*,#8796,.F.) ;
#12395 = ORIENTED_EDGE('',*,*,#8797,.T.) ;
#12396 = ORIENTED_EDGE('',*,*,#8798,.F.) ;
#12397 = ORIENTED_EDGE('',*,*,#8799,.T.) ;
#12398 = ORIENTED_EDGE('',*,*,#8417,.F.) ;
#12399 = ORIENTED_EDGE('',*,*,#8794,.T.) ;
#12400 = ORIENTED_EDGE('',*,*,#8184,.F.) ;
#12401 = ORIENTED_EDGE('',*,*,#8799,.F.) ;
#12402 = ORIENTED_EDGE('',*,*,#8800,.T.) ;
#12403 = ORIENTED_EDGE('',*,*,#8795,.F.) ;
#12404 = ORIENTED_EDGE('',*,*,#8800,.F.) ;
#12405 = ORIENTED_EDGE('',*,*,#8798,.T.) ;
#12406 = ORIENTED_EDGE('',*,*,#8801,.T.) ;
#12407 = ORIENTED_EDGE('',*,*,#8796,.T.) ;
#12408 = ORIENTED_EDGE('',*,*,#8801,.F.) ;
#12409 = ORIENTED_EDGE('',*,*,#8797,.F.) ;
#12410 = ORIENTED_EDGE('',*,*,#8175,.T.) ;
#12411 = ORIENTED_EDGE('',*,*,#8369,.T.) ;
#12412 = ORIENTED_EDGE('',*,*,#8802,.F.) ;
#12413 = ORIENTED_EDGE('',*,*,#8803,.T.) ;
#12414 = ORIENTED_EDGE('',*,*,#8804,.F.) ;
#12415 = ORIENTED_EDGE('',*,*,#8805,.T.) ;
#12416 = ORIENTED_EDGE('',*,*,#8806,.F.) ;
#12417 = ORIENTED_EDGE('',*,*,#8807,.T.) ;
#12418 = ORIENTED_EDGE('',*,*,#8415,.F.) ;
#12419 = ORIENTED_EDGE('',*,*,#8802,.T.) ;
#12420 = ORIENTED_EDGE('',*,*,#8180,.F.) ;
#12421 = ORIENTED_EDGE('',*,*,#8807,.F.) ;
#12422 = ORIENTED_EDGE('',*,*,#8808,.T.) ;
#12423 = ORIENTED_EDGE('',*,*,#8803,.F.) ;
#12424 = ORIENTED_EDGE('',*,*,#8808,.F.) ;
#12425 = ORIENTED_EDGE('',*,*,#8806,.T.) ;
#12426 = ORIENTED_EDGE('',*,*,#8809,.T.) ;
#12427 = ORIENTED_EDGE('',*,*,#8804,.T.) ;
#12428 = ORIENTED_EDGE('',*,*,#8809,.F.) ;
#12429 = ORIENTED_EDGE('',*,*,#8805,.F.) ;
#12430 = ORIENTED_EDGE('',*,*,#8174,.T.) ;
#12431 = ORIENTED_EDGE('',*,*,#8370,.T.) ;
#12432 = ORIENTED_EDGE('',*,*,#8810,.F.) ;
#12433 = ORIENTED_EDGE('',*,*,#8811,.T.) ;
#12434 = ORIENTED_EDGE('',*,*,#8812,.F.) ;
#12435 = ORIENTED_EDGE('',*,*,#8813,.T.) ;
#12436 = ORIENTED_EDGE('',*,*,#8814,.F.) ;
#12437 = ORIENTED_EDGE('',*,*,#8815,.T.) ;
#12438 = ORIENTED_EDGE('',*,*,#8414,.F.) ;
#12439 = ORIENTED_EDGE('',*,*,#8810,.T.) ;
#12440 = ORIENTED_EDGE('',*,*,#8172,.F.) ;
#12441 = ORIENTED_EDGE('',*,*,#8815,.F.) ;
#12442 = ORIENTED_EDGE('',*,*,#8816,.T.) ;
#12443 = ORIENTED_EDGE('',*,*,#8811,.F.) ;
#12444 = ORIENTED_EDGE('',*,*,#8816,.F.) ;
#12445 = ORIENTED_EDGE('',*,*,#8814,.T.) ;
#12446 = ORIENTED_EDGE('',*,*,#8817,.T.) ;
#12447 = ORIENTED_EDGE('',*,*,#8812,.T.) ;
#12448 = ORIENTED_EDGE('',*,*,#8817,.F.) ;
#12449 = ORIENTED_EDGE('',*,*,#8813,.F.) ;
#12450 = ORIENTED_EDGE('',*,*,#8170,.T.) ;
#12451 = ORIENTED_EDGE('',*,*,#8371,.T.) ;
#12452 = ORIENTED_EDGE('',*,*,#8818,.F.) ;
#12453 = ORIENTED_EDGE('',*,*,#8819,.T.) ;
#12454 = ORIENTED_EDGE('',*,*,#8820,.F.) ;
#12455 = ORIENTED_EDGE('',*,*,#8821,.T.) ;
#12456 = ORIENTED_EDGE('',*,*,#8822,.F.) ;
#12457 = ORIENTED_EDGE('',*,*,#8823,.T.) ;
#12458 = ORIENTED_EDGE('',*,*,#8413,.F.) ;
#12459 = ORIENTED_EDGE('',*,*,#8818,.T.) ;
#12460 = ORIENTED_EDGE('',*,*,#8168,.F.) ;
#12461 = ORIENTED_EDGE('',*,*,#8823,.F.) ;
#12462 = ORIENTED_EDGE('',*,*,#8824,.T.) ;
#12463 = ORIENTED_EDGE('',*,*,#8819,.F.) ;
#12464 = ORIENTED_EDGE('',*,*,#8824,.F.) ;
#12465 = ORIENTED_EDGE('',*,*,#8822,.T.) ;
#12466 = ORIENTED_EDGE('',*,*,#8825,.T.) ;
#12467 = ORIENTED_EDGE('',*,*,#8820,.T.) ;
#12468 = ORIENTED_EDGE('',*,*,#8825,.F.) ;
#12469 = ORIENTED_EDGE('',*,*,#8821,.F.) ;
#12470 = ORIENTED_EDGE('',*,*,#8166,.T.) ;
#12471 = ORIENTED_EDGE('',*,*,#8372,.T.) ;
#12472 = ORIENTED_EDGE('',*,*,#8826,.F.) ;
#12473 = ORIENTED_EDGE('',*,*,#8827,.T.) ;
#12474 = ORIENTED_EDGE('',*,*,#8828,.F.) ;
#12475 = ORIENTED_EDGE('',*,*,#8829,.T.) ;
#12476 = ORIENTED_EDGE('',*,*,#8830,.F.) ;
#12477 = ORIENTED_EDGE('',*,*,#8831,.T.) ;
#12478 = ORIENTED_EDGE('',*,*,#8412,.F.) ;
#12479 = ORIENTED_EDGE('',*,*,#8826,.T.) ;
#12480 = ORIENTED_EDGE('',*,*,#8164,.F.) ;
#12481 = ORIENTED_EDGE('',*,*,#8831,.F.) ;
#12482 = ORIENTED_EDGE('',*,*,#8832,.T.) ;
#12483 = ORIENTED_EDGE('',*,*,#8827,.F.) ;
#12484 = ORIENTED_EDGE('',*,*,#8832,.F.) ;
#12485 = ORIENTED_EDGE('',*,*,#8830,.T.) ;
#12486 = ORIENTED_EDGE('',*,*,#8833,.T.) ;
#12487 = ORIENTED_EDGE('',*,*,#8828,.T.) ;
#12488 = ORIENTED_EDGE('',*,*,#8833,.F.) ;
#12489 = ORIENTED_EDGE('',*,*,#8829,.F.) ;
#12490 = ORIENTED_EDGE('',*,*,#8162,.T.) ;
#12491 = ORIENTED_EDGE('',*,*,#8373,.T.) ;
#12492 = ORIENTED_EDGE('',*,*,#8834,.F.) ;
#12493 = ORIENTED_EDGE('',*,*,#8835,.T.) ;
#12494 = ORIENTED_EDGE('',*,*,#8836,.F.) ;
#12495 = ORIENTED_EDGE('',*,*,#8837,.T.) ;
#12496 = ORIENTED_EDGE('',*,*,#8838,.F.) ;
#12497 = ORIENTED_EDGE('',*,*,#8839,.T.) ;
#12498 = ORIENTED_EDGE('',*,*,#8411,.F.) ;
#12499 = ORIENTED_EDGE('',*,*,#8834,.T.) ;
#12500 = ORIENTED_EDGE('',*,*,#8160,.F.) ;
#12501 = ORIENTED_EDGE('',*,*,#8839,.F.) ;
#12502 = ORIENTED_EDGE('',*,*,#8840,.T.) ;
#12503 = ORIENTED_EDGE('',*,*,#8835,.F.) ;
#12504 = ORIENTED_EDGE('',*,*,#8840,.F.) ;
#12505 = ORIENTED_EDGE('',*,*,#8838,.T.) ;
#12506 = ORIENTED_EDGE('',*,*,#8841,.T.) ;
#12507 = ORIENTED_EDGE('',*,*,#8836,.T.) ;
#12508 = ORIENTED_EDGE('',*,*,#8841,.F.) ;
#12509 = ORIENTED_EDGE('',*,*,#8837,.F.) ;
#12510 = ORIENTED_EDGE('',*,*,#8158,.T.) ;
#12511 = ORIENTED_EDGE('',*,*,#8374,.T.) ;
#12512 = ORIENTED_EDGE('',*,*,#8842,.F.) ;
#12513 = ORIENTED_EDGE('',*,*,#8843,.T.) ;
#12514 = ORIENTED_EDGE('',*,*,#8844,.F.) ;
#12515 = ORIENTED_EDGE('',*,*,#8845,.T.) ;
#12516 = ORIENTED_EDGE('',*,*,#8846,.F.) ;
#12517 = ORIENTED_EDGE('',*,*,#8847,.T.) ;
#12518 = ORIENTED_EDGE('',*,*,#8410,.F.) ;
#12519 = ORIENTED_EDGE('',*,*,#8842,.T.) ;
#12520 = ORIENTED_EDGE('',*,*,#8156,.F.) ;
#12521 = ORIENTED_EDGE('',*,*,#8847,.F.) ;
#12522 = ORIENTED_EDGE('',*,*,#8848,.T.) ;
#12523 = ORIENTED_EDGE('',*,*,#8843,.F.) ;
#12524 = ORIENTED_EDGE('',*,*,#8848,.F.) ;
#12525 = ORIENTED_EDGE('',*,*,#8846,.T.) ;
#12526 = ORIENTED_EDGE('',*,*,#8849,.T.) ;
#12527 = ORIENTED_EDGE('',*,*,#8844,.T.) ;
#12528 = ORIENTED_EDGE('',*,*,#8849,.F.) ;
#12529 = ORIENTED_EDGE('',*,*,#8845,.F.) ;
#12530 = ORIENTED_EDGE('',*,*,#8154,.T.) ;
#12531 = ORIENTED_EDGE('',*,*,#8375,.T.) ;
#12532 = ORIENTED_EDGE('',*,*,#8850,.F.) ;
#12533 = ORIENTED_EDGE('',*,*,#8851,.T.) ;
#12534 = ORIENTED_EDGE('',*,*,#8852,.F.) ;
#12535 = ORIENTED_EDGE('',*,*,#8853,.T.) ;
#12536 = ORIENTED_EDGE('',*,*,#8854,.F.) ;
#12537 = ORIENTED_EDGE('',*,*,#8855,.T.) ;
#12538 = ORIENTED_EDGE('',*,*,#8409,.F.) ;
#12539 = ORIENTED_EDGE('',*,*,#8469,.F.) ;
#12540 = ORIENTED_EDGE('',*,*,#8850,.T.) ;
#12541 = ORIENTED_EDGE('',*,*,#8152,.F.) ;
#12542 = ORIENTED_EDGE('',*,*,#8855,.F.) ;
#12543 = ORIENTED_EDGE('',*,*,#8856,.T.) ;
#12544 = ORIENTED_EDGE('',*,*,#8851,.F.) ;
#12545 = ORIENTED_EDGE('',*,*,#8856,.F.) ;
#12546 = ORIENTED_EDGE('',*,*,#8854,.T.) ;
#12547 = ORIENTED_EDGE('',*,*,#8857,.T.) ;
#12548 = ORIENTED_EDGE('',*,*,#8852,.T.) ;
#12549 = ORIENTED_EDGE('',*,*,#8857,.F.) ;
#12550 = ORIENTED_EDGE('',*,*,#8853,.F.) ;
#12551 = ORIENTED_EDGE('',*,*,#8150,.T.) ;
#12552 = ORIENTED_EDGE('',*,*,#8376,.T.) ;
#12553 = ORIENTED_EDGE('',*,*,#8858,.F.) ;
#12554 = ORIENTED_EDGE('',*,*,#8859,.T.) ;
#12555 = ORIENTED_EDGE('',*,*,#8860,.F.) ;
#12556 = ORIENTED_EDGE('',*,*,#8861,.T.) ;
#12557 = ORIENTED_EDGE('',*,*,#8862,.F.) ;
#12558 = ORIENTED_EDGE('',*,*,#8863,.T.) ;
#12559 = ORIENTED_EDGE('',*,*,#8468,.F.) ;
#12560 = ORIENTED_EDGE('',*,*,#8858,.T.) ;
#12561 = ORIENTED_EDGE('',*,*,#8148,.F.) ;
#12562 = ORIENTED_EDGE('',*,*,#8863,.F.) ;
#12563 = ORIENTED_EDGE('',*,*,#8864,.T.) ;
#12564 = ORIENTED_EDGE('',*,*,#8859,.F.) ;
#12565 = ORIENTED_EDGE('',*,*,#8864,.F.) ;
#12566 = ORIENTED_EDGE('',*,*,#8862,.T.) ;
#12567 = ORIENTED_EDGE('',*,*,#8865,.T.) ;
#12568 = ORIENTED_EDGE('',*,*,#8860,.T.) ;
#12569 = ORIENTED_EDGE('',*,*,#8865,.F.) ;
#12570 = ORIENTED_EDGE('',*,*,#8861,.F.) ;
#12571 = ORIENTED_EDGE('',*,*,#8146,.T.) ;
#12572 = ORIENTED_EDGE('',*,*,#8377,.T.) ;
#12573 = ORIENTED_EDGE('',*,*,#8866,.F.) ;
#12574 = ORIENTED_EDGE('',*,*,#8867,.T.) ;
#12575 = ORIENTED_EDGE('',*,*,#8868,.F.) ;
#12576 = ORIENTED_EDGE('',*,*,#8869,.T.) ;
#12577 = ORIENTED_EDGE('',*,*,#8870,.F.) ;
#12578 = ORIENTED_EDGE('',*,*,#8871,.T.) ;
#12579 = ORIENTED_EDGE('',*,*,#8467,.F.) ;
#12580 = ORIENTED_EDGE('',*,*,#8866,.T.) ;
#12581 = ORIENTED_EDGE('',*,*,#8144,.F.) ;
#12582 = ORIENTED_EDGE('',*,*,#8871,.F.) ;
#12583 = ORIENTED_EDGE('',*,*,#8872,.T.) ;
#12584 = ORIENTED_EDGE('',*,*,#8867,.F.) ;
#12585 = ORIENTED_EDGE('',*,*,#8872,.F.) ;
#12586 = ORIENTED_EDGE('',*,*,#8870,.T.) ;
#12587 = ORIENTED_EDGE('',*,*,#8873,.T.) ;
#12588 = ORIENTED_EDGE('',*,*,#8868,.T.) ;
#12589 = ORIENTED_EDGE('',*,*,#8873,.F.) ;
#12590 = ORIENTED_EDGE('',*,*,#8869,.F.) ;
#12591 = ORIENTED_EDGE('',*,*,#8142,.T.) ;
#12592 = ORIENTED_EDGE('',*,*,#8378,.T.) ;
#12593 = ORIENTED_EDGE('',*,*,#8874,.F.) ;
#12594 = ORIENTED_EDGE('',*,*,#8875,.T.) ;
#12595 = ORIENTED_EDGE('',*,*,#8876,.F.) ;
#12596 = ORIENTED_EDGE('',*,*,#8877,.T.) ;
#12597 = ORIENTED_EDGE('',*,*,#8878,.F.) ;
#12598 = ORIENTED_EDGE('',*,*,#8879,.T.) ;
#12599 = ORIENTED_EDGE('',*,*,#8466,.F.) ;
#12600 = ORIENTED_EDGE('',*,*,#8874,.T.) ;
#12601 = ORIENTED_EDGE('',*,*,#8140,.F.) ;
#12602 = ORIENTED_EDGE('',*,*,#8879,.F.) ;
#12603 = ORIENTED_EDGE('',*,*,#8880,.T.) ;
#12604 = ORIENTED_EDGE('',*,*,#8875,.F.) ;
#12605 = ORIENTED_EDGE('',*,*,#8880,.F.) ;
#12606 = ORIENTED_EDGE('',*,*,#8878,.T.) ;
#12607 = ORIENTED_EDGE('',*,*,#8881,.T.) ;
#12608 = ORIENTED_EDGE('',*,*,#8876,.T.) ;
#12609 = ORIENTED_EDGE('',*,*,#8881,.F.) ;
#12610 = ORIENTED_EDGE('',*,*,#8877,.F.) ;
#12611 = ORIENTED_EDGE('',*,*,#8138,.T.) ;
#12612 = ORIENTED_EDGE('',*,*,#8379,.T.) ;
#12613 = ORIENTED_EDGE('',*,*,#8882,.F.) ;
#12614 = ORIENTED_EDGE('',*,*,#8883,.T.) ;
#12615 = ORIENTED_EDGE('',*,*,#8884,.F.) ;
#12616 = ORIENTED_EDGE('',*,*,#8885,.T.) ;
#12617 = ORIENTED_EDGE('',*,*,#8886,.F.) ;
#12618 = ORIENTED_EDGE('',*,*,#8887,.T.) ;
#12619 = ORIENTED_EDGE('',*,*,#8465,.F.) ;
#12620 = ORIENTED_EDGE('',*,*,#8882,.T.) ;
#12621 = ORIENTED_EDGE('',*,*,#8136,.F.) ;
#12622 = ORIENTED_EDGE('',*,*,#8887,.F.) ;
#12623 = ORIENTED_EDGE('',*,*,#8888,.T.) ;
#12624 = ORIENTED_EDGE('',*,*,#8883,.F.) ;
#12625 = ORIENTED_EDGE('',*,*,#8888,.F.) ;
#12626 = ORIENTED_EDGE('',*,*,#8886,.T.) ;
#12627 = ORIENTED_EDGE('',*,*,#8889,.T.) ;
#12628 = ORIENTED_EDGE('',*,*,#8884,.T.) ;
#12629 = ORIENTED_EDGE('',*,*,#8889,.F.) ;
#12630 = ORIENTED_EDGE('',*,*,#8885,.F.) ;
#12631 = ORIENTED_EDGE('',*,*,#8134,.T.) ;
#12632 = ORIENTED_EDGE('',*,*,#8380,.T.) ;
#12633 = ORIENTED_EDGE('',*,*,#8890,.F.) ;
#12634 = ORIENTED_EDGE('',*,*,#8891,.T.) ;
#12635 = ORIENTED_EDGE('',*,*,#8892,.F.) ;
#12636 = ORIENTED_EDGE('',*,*,#8893,.T.) ;
#12637 = ORIENTED_EDGE('',*,*,#8894,.F.) ;
#12638 = ORIENTED_EDGE('',*,*,#8895,.T.) ;
#12639 = ORIENTED_EDGE('',*,*,#8464,.F.) ;
#12640 = ORIENTED_EDGE('',*,*,#8890,.T.) ;
#12641 = ORIENTED_EDGE('',*,*,#8132,.F.) ;
#12642 = ORIENTED_EDGE('',*,*,#8895,.F.) ;
#12643 = ORIENTED_EDGE('',*,*,#8896,.T.) ;
#12644 = ORIENTED_EDGE('',*,*,#8891,.F.) ;
#12645 = ORIENTED_EDGE('',*,*,#8896,.F.) ;
#12646 = ORIENTED_EDGE('',*,*,#8894,.T.) ;
#12647 = ORIENTED_EDGE('',*,*,#8897,.T.) ;
#12648 = ORIENTED_EDGE('',*,*,#8892,.T.) ;
#12649 = ORIENTED_EDGE('',*,*,#8897,.F.) ;
#12650 = ORIENTED_EDGE('',*,*,#8893,.F.) ;
#12651 = ORIENTED_EDGE('',*,*,#8130,.T.) ;
#12652 = ORIENTED_EDGE('',*,*,#8384,.T.) ;
#12653 = ORIENTED_EDGE('',*,*,#8898,.F.) ;
#12654 = ORIENTED_EDGE('',*,*,#8899,.T.) ;
#12655 = ORIENTED_EDGE('',*,*,#8900,.F.) ;
#12656 = ORIENTED_EDGE('',*,*,#8901,.T.) ;
#12657 = ORIENTED_EDGE('',*,*,#8902,.F.) ;
#12658 = ORIENTED_EDGE('',*,*,#8903,.T.) ;
#12659 = ORIENTED_EDGE('',*,*,#8460,.F.) ;
#12660 = ORIENTED_EDGE('',*,*,#8898,.T.) ;
#12661 = ORIENTED_EDGE('',*,*,#8121,.F.) ;
#12662 = ORIENTED_EDGE('',*,*,#8903,.F.) ;
#12663 = ORIENTED_EDGE('',*,*,#8904,.T.) ;
#12664 = ORIENTED_EDGE('',*,*,#8899,.F.) ;
#12665 = ORIENTED_EDGE('',*,*,#8904,.F.) ;
#12666 = ORIENTED_EDGE('',*,*,#8902,.T.) ;
#12667 = ORIENTED_EDGE('',*,*,#8905,.T.) ;
#12668 = ORIENTED_EDGE('',*,*,#8900,.T.) ;
#12669 = ORIENTED_EDGE('',*,*,#8905,.F.) ;
#12670 = ORIENTED_EDGE('',*,*,#8901,.F.) ;
#12671 = ORIENTED_EDGE('',*,*,#8126,.T.) ;
#12672 = ORIENTED_EDGE('',*,*,#8383,.T.) ;
#12673 = ORIENTED_EDGE('',*,*,#8906,.F.) ;
#12674 = ORIENTED_EDGE('',*,*,#8907,.T.) ;
#12675 = ORIENTED_EDGE('',*,*,#8908,.F.) ;
#12676 = ORIENTED_EDGE('',*,*,#8909,.T.) ;
#12677 = ORIENTED_EDGE('',*,*,#8910,.F.) ;
#12678 = ORIENTED_EDGE('',*,*,#8911,.T.) ;
#12679 = ORIENTED_EDGE('',*,*,#8461,.F.) ;
#12680 = ORIENTED_EDGE('',*,*,#8906,.T.) ;
#12681 = ORIENTED_EDGE('',*,*,#8117,.F.) ;
#12682 = ORIENTED_EDGE('',*,*,#8911,.F.) ;
#12683 = ORIENTED_EDGE('',*,*,#8912,.T.) ;
#12684 = ORIENTED_EDGE('',*,*,#8907,.F.) ;
#12685 = ORIENTED_EDGE('',*,*,#8912,.F.) ;
#12686 = ORIENTED_EDGE('',*,*,#8910,.T.) ;
#12687 = ORIENTED_EDGE('',*,*,#8913,.T.) ;
#12688 = ORIENTED_EDGE('',*,*,#8908,.T.) ;
#12689 = ORIENTED_EDGE('',*,*,#8913,.F.) ;
#12690 = ORIENTED_EDGE('',*,*,#8909,.F.) ;
#12691 = ORIENTED_EDGE('',*,*,#8119,.T.) ;
#12692 = ORIENTED_EDGE('',*,*,#8382,.T.) ;
#12693 = ORIENTED_EDGE('',*,*,#8914,.F.) ;
#12694 = ORIENTED_EDGE('',*,*,#8915,.T.) ;
#12695 = ORIENTED_EDGE('',*,*,#8916,.F.) ;
#12696 = ORIENTED_EDGE('',*,*,#8917,.T.) ;
#12697 = ORIENTED_EDGE('',*,*,#8918,.F.) ;
#12698 = ORIENTED_EDGE('',*,*,#8919,.T.) ;
#12699 = ORIENTED_EDGE('',*,*,#8462,.F.) ;
#12700 = ORIENTED_EDGE('',*,*,#8914,.T.) ;
#12701 = ORIENTED_EDGE('',*,*,#8113,.F.) ;
#12702 = ORIENTED_EDGE('',*,*,#8919,.F.) ;
#12703 = ORIENTED_EDGE('',*,*,#8920,.T.) ;
#12704 = ORIENTED_EDGE('',*,*,#8915,.F.) ;
#12705 = ORIENTED_EDGE('',*,*,#8920,.F.) ;
#12706 = ORIENTED_EDGE('',*,*,#8918,.T.) ;
#12707 = ORIENTED_EDGE('',*,*,#8921,.T.) ;
#12708 = ORIENTED_EDGE('',*,*,#8916,.T.) ;
#12709 = ORIENTED_EDGE('',*,*,#8921,.F.) ;
#12710 = ORIENTED_EDGE('',*,*,#8917,.F.) ;
#12711 = ORIENTED_EDGE('',*,*,#8115,.T.) ;
#12712 = ORIENTED_EDGE('',*,*,#8381,.T.) ;
#12713 = ORIENTED_EDGE('',*,*,#8922,.F.) ;
#12714 = ORIENTED_EDGE('',*,*,#8923,.T.) ;
#12715 = ORIENTED_EDGE('',*,*,#8924,.F.) ;
#12716 = ORIENTED_EDGE('',*,*,#8925,.T.) ;
#12717 = ORIENTED_EDGE('',*,*,#8926,.F.) ;
#12718 = ORIENTED_EDGE('',*,*,#8927,.T.) ;
#12719 = ORIENTED_EDGE('',*,*,#8463,.F.) ;
#12720 = ORIENTED_EDGE('',*,*,#8922,.T.) ;
#12721 = ORIENTED_EDGE('',*,*,#8128,.F.) ;
#12722 = ORIENTED_EDGE('',*,*,#8927,.F.) ;
#12723 = ORIENTED_EDGE('',*,*,#8928,.T.) ;
#12724 = ORIENTED_EDGE('',*,*,#8923,.F.) ;
#12725 = ORIENTED_EDGE('',*,*,#8928,.F.) ;
#12726 = ORIENTED_EDGE('',*,*,#8926,.T.) ;
#12727 = ORIENTED_EDGE('',*,*,#8929,.T.) ;
#12728 = ORIENTED_EDGE('',*,*,#8924,.T.) ;
#12729 = ORIENTED_EDGE('',*,*,#8929,.F.) ;
#12730 = ORIENTED_EDGE('',*,*,#8925,.F.) ;
#12731 = ORIENTED_EDGE('',*,*,#8111,.T.) ;
#12732 = ORIENTED_EDGE('',*,*,#8385,.T.) ;
#12733 = ORIENTED_EDGE('',*,*,#8930,.F.) ;
#12734 = ORIENTED_EDGE('',*,*,#8931,.T.) ;
#12735 = ORIENTED_EDGE('',*,*,#8932,.F.) ;
#12736 = ORIENTED_EDGE('',*,*,#8933,.T.) ;
#12737 = ORIENTED_EDGE('',*,*,#8934,.F.) ;
#12738 = ORIENTED_EDGE('',*,*,#8935,.T.) ;
#12739 = ORIENTED_EDGE('',*,*,#8459,.F.) ;
#12740 = ORIENTED_EDGE('',*,*,#8930,.T.) ;
#12741 = ORIENTED_EDGE('',*,*,#8124,.F.) ;
#12742 = ORIENTED_EDGE('',*,*,#8935,.F.) ;
#12743 = ORIENTED_EDGE('',*,*,#8936,.T.) ;
#12744 = ORIENTED_EDGE('',*,*,#8931,.F.) ;
#12745 = ORIENTED_EDGE('',*,*,#8936,.F.) ;
#12746 = ORIENTED_EDGE('',*,*,#8934,.T.) ;
#12747 = ORIENTED_EDGE('',*,*,#8937,.T.) ;
#12748 = ORIENTED_EDGE('',*,*,#8932,.T.) ;
#12749 = ORIENTED_EDGE('',*,*,#8937,.F.) ;
#12750 = ORIENTED_EDGE('',*,*,#8933,.F.) ;
#12751 = ORIENTED_EDGE('',*,*,#8110,.T.) ;
#12752 = ORIENTED_EDGE('',*,*,#8386,.T.) ;
#12753 = ORIENTED_EDGE('',*,*,#8938,.F.) ;
#12754 = ORIENTED_EDGE('',*,*,#8939,.T.) ;
#12755 = ORIENTED_EDGE('',*,*,#8940,.F.) ;
#12756 = ORIENTED_EDGE('',*,*,#8941,.T.) ;
#12757 = ORIENTED_EDGE('',*,*,#8942,.F.) ;
#12758 = ORIENTED_EDGE('',*,*,#8943,.T.) ;
#12759 = ORIENTED_EDGE('',*,*,#8458,.F.) ;
#12760 = ORIENTED_EDGE('',*,*,#8938,.T.) ;
#12761 = ORIENTED_EDGE('',*,*,#8108,.F.) ;
#12762 = ORIENTED_EDGE('',*,*,#8943,.F.) ;
#12763 = ORIENTED_EDGE('',*,*,#8944,.T.) ;
#12764 = ORIENTED_EDGE('',*,*,#8939,.F.) ;
#12765 = ORIENTED_EDGE('',*,*,#8944,.F.) ;
#12766 = ORIENTED_EDGE('',*,*,#8942,.T.) ;
#12767 = ORIENTED_EDGE('',*,*,#8945,.T.) ;
#12768 = ORIENTED_EDGE('',*,*,#8940,.T.) ;
#12769 = ORIENTED_EDGE('',*,*,#8945,.F.) ;
#12770 = ORIENTED_EDGE('',*,*,#8941,.F.) ;
#12771 = ORIENTED_EDGE('',*,*,#8106,.T.) ;
#12772 = ORIENTED_EDGE('',*,*,#8387,.T.) ;
#12773 = ORIENTED_EDGE('',*,*,#8946,.F.) ;
#12774 = ORIENTED_EDGE('',*,*,#8947,.T.) ;
#12775 = ORIENTED_EDGE('',*,*,#8948,.F.) ;
#12776 = ORIENTED_EDGE('',*,*,#8949,.T.) ;
#12777 = ORIENTED_EDGE('',*,*,#8950,.F.) ;
#12778 = ORIENTED_EDGE('',*,*,#8951,.T.) ;
#12779 = ORIENTED_EDGE('',*,*,#8457,.F.) ;
#12780 = ORIENTED_EDGE('',*,*,#8946,.T.) ;
#12781 = ORIENTED_EDGE('',*,*,#8104,.F.) ;
#12782 = ORIENTED_EDGE('',*,*,#8951,.F.) ;
#12783 = ORIENTED_EDGE('',*,*,#8952,.T.) ;
#12784 = ORIENTED_EDGE('',*,*,#8947,.F.) ;
#12785 = ORIENTED_EDGE('',*,*,#8952,.F.) ;
#12786 = ORIENTED_EDGE('',*,*,#8950,.T.) ;
#12787 = ORIENTED_EDGE('',*,*,#8953,.T.) ;
#12788 = ORIENTED_EDGE('',*,*,#8948,.T.) ;
#12789 = ORIENTED_EDGE('',*,*,#8953,.F.) ;
#12790 = ORIENTED_EDGE('',*,*,#8949,.F.) ;
#12791 = ORIENTED_EDGE('',*,*,#8102,.T.) ;
#12792 = ORIENTED_EDGE('',*,*,#8388,.T.) ;
#12793 = ORIENTED_EDGE('',*,*,#8954,.F.) ;
#12794 = ORIENTED_EDGE('',*,*,#8955,.T.) ;
#12795 = ORIENTED_EDGE('',*,*,#8956,.F.) ;
#12796 = ORIENTED_EDGE('',*,*,#8957,.T.) ;
#12797 = ORIENTED_EDGE('',*,*,#8958,.F.) ;
#12798 = ORIENTED_EDGE('',*,*,#8959,.T.) ;
#12799 = ORIENTED_EDGE('',*,*,#8456,.F.) ;
#12800 = ORIENTED_EDGE('',*,*,#8954,.T.) ;
#12801 = ORIENTED_EDGE('',*,*,#8100,.F.) ;
#12802 = ORIENTED_EDGE('',*,*,#8959,.F.) ;
#12803 = ORIENTED_EDGE('',*,*,#8960,.T.) ;
#12804 = ORIENTED_EDGE('',*,*,#8955,.F.) ;
#12805 = ORIENTED_EDGE('',*,*,#8960,.F.) ;
#12806 = ORIENTED_EDGE('',*,*,#8958,.T.) ;
#12807 = ORIENTED_EDGE('',*,*,#8961,.T.) ;
#12808 = ORIENTED_EDGE('',*,*,#8956,.T.) ;
#12809 = ORIENTED_EDGE('',*,*,#8961,.F.) ;
#12810 = ORIENTED_EDGE('',*,*,#8957,.F.) ;
#12811 = ORIENTED_EDGE('',*,*,#8095,.T.) ;
#12812 = ORIENTED_EDGE('',*,*,#8090,.T.) ;
#12813 = ORIENTED_EDGE('',*,*,#8094,.F.) ;
#12814 = ORIENTED_EDGE('',*,*,#8083,.T.) ;
#12815 = ORIENTED_EDGE('',*,*,#8481,.T.) ;
#12816 = ORIENTED_EDGE('',*,*,#8962,.F.) ;
#12817 = ORIENTED_EDGE('',*,*,#8963,.F.) ;
#12818 = ORIENTED_EDGE('',*,*,#8964,.T.) ;
#12819 = ORIENTED_EDGE('',*,*,#8965,.T.) ;
#12820 = ORIENTED_EDGE('',*,*,#8964,.F.) ;
#12821 = ORIENTED_EDGE('',*,*,#8965,.F.) ;
#12822 = ORIENTED_EDGE('',*,*,#8966,.T.) ;
#12823 = ORIENTED_EDGE('',*,*,#8967,.T.) ;
#12824 = ORIENTED_EDGE('',*,*,#8966,.F.) ;
#12825 = ORIENTED_EDGE('',*,*,#8968,.T.) ;
#12826 = ORIENTED_EDGE('',*,*,#8967,.F.) ;
#12827 = ORIENTED_EDGE('',*,*,#8969,.T.) ;
#12828 = ORIENTED_EDGE('',*,*,#8970,.T.) ;
#12829 = ORIENTED_EDGE('',*,*,#8968,.F.) ;
#12830 = ORIENTED_EDGE('',*,*,#8970,.F.) ;
#12831 = ORIENTED_EDGE('',*,*,#8971,.T.) ;
#12832 = ORIENTED_EDGE('',*,*,#8969,.F.) ;
#12833 = ORIENTED_EDGE('',*,*,#8972,.T.) ;
#12834 = ORIENTED_EDGE('',*,*,#8973,.T.) ;
#12835 = ORIENTED_EDGE('',*,*,#8972,.F.) ;
#12836 = ORIENTED_EDGE('',*,*,#8971,.F.) ;
#12837 = ORIENTED_EDGE('',*,*,#8973,.F.) ;
#12838 = ORIENTED_EDGE('',*,*,#8974,.T.) ;
#12839 = ORIENTED_EDGE('',*,*,#8975,.T.) ;
#12840 = ORIENTED_EDGE('',*,*,#8974,.F.) ;
#12841 = ORIENTED_EDGE('',*,*,#8975,.F.) ;
#12842 = ORIENTED_EDGE('',*,*,#8976,.T.) ;
#12843 = ORIENTED_EDGE('',*,*,#8962,.T.) ;
#12844 = ORIENTED_EDGE('',*,*,#8963,.T.) ;
#12845 = ORIENTED_EDGE('',*,*,#8977,.T.) ;
#12846 = ORIENTED_EDGE('',*,*,#8976,.F.) ;
#12847 = ORIENTED_EDGE('',*,*,#8977,.F.) ;
#12848 = ORIENTED_EDGE('',*,*,#8978,.F.) ;
#12849 = ORIENTED_EDGE('',*,*,#8979,.F.) ;
#12850 = ORIENTED_EDGE('',*,*,#8980,.F.) ;
#12851 = ORIENTED_EDGE('',*,*,#8981,.F.) ;
#12852 = ORIENTED_EDGE('',*,*,#8982,.F.) ;
#12853 = ORIENTED_EDGE('',*,*,#8983,.T.) ;
#12854 = ORIENTED_EDGE('',*,*,#8984,.F.) ;
#12855 = ORIENTED_EDGE('',*,*,#8985,.F.) ;
#12856 = ORIENTED_EDGE('',*,*,#8986,.T.) ;
#12857 = ORIENTED_EDGE('',*,*,#8981,.T.) ;
#12858 = ORIENTED_EDGE('',*,*,#8987,.F.) ;
#12859 = ORIENTED_EDGE('',*,*,#8983,.F.) ;
#12860 = ORIENTED_EDGE('',*,*,#8984,.T.) ;
#12861 = ORIENTED_EDGE('',*,*,#8987,.T.) ;
#12862 = ORIENTED_EDGE('',*,*,#8980,.T.) ;
#12863 = ORIENTED_EDGE('',*,*,#8988,.F.) ;
#12864 = ORIENTED_EDGE('',*,*,#8989,.T.) ;
#12865 = ORIENTED_EDGE('',*,*,#8990,.T.) ;
#12866 = ORIENTED_EDGE('',*,*,#8991,.T.) ;
#12867 = ORIENTED_EDGE('',*,*,#8992,.F.) ;
#12868 = ORIENTED_EDGE('',*,*,#8993,.T.) ;
#12869 = ORIENTED_EDGE('',*,*,#8994,.T.) ;
#12870 = ORIENTED_EDGE('',*,*,#8995,.T.) ;
#12871 = ORIENTED_EDGE('',*,*,#8996,.F.) ;
#12872 = ORIENTED_EDGE('',*,*,#8997,.T.) ;
#12873 = ORIENTED_EDGE('',*,*,#8998,.T.) ;
#12874 = ORIENTED_EDGE('',*,*,#8999,.T.) ;
#12875 = ORIENTED_EDGE('',*,*,#9000,.F.) ;
#12876 = ORIENTED_EDGE('',*,*,#9001,.F.) ;
#12877 = ORIENTED_EDGE('',*,*,#8979,.T.) ;
#12878 = ORIENTED_EDGE('',*,*,#9002,.F.) ;
#12879 = ORIENTED_EDGE('',*,*,#9003,.T.) ;
#12880 = ORIENTED_EDGE('',*,*,#8988,.T.) ;
#12881 = ORIENTED_EDGE('',*,*,#8978,.T.) ;
#12882 = ORIENTED_EDGE('',*,*,#9004,.T.) ;
#12883 = ORIENTED_EDGE('',*,*,#9005,.T.) ;
#12884 = ORIENTED_EDGE('',*,*,#9002,.T.) ;
#12885 = ORIENTED_EDGE('',*,*,#9006,.F.) ;
#12886 = ORIENTED_EDGE('',*,*,#9007,.F.) ;
#12887 = ORIENTED_EDGE('',*,*,#8991,.F.) ;
#12888 = ORIENTED_EDGE('',*,*,#9008,.F.) ;
#12889 = ORIENTED_EDGE('',*,*,#9005,.F.) ;
#12890 = ORIENTED_EDGE('',*,*,#9009,.T.) ;
#12891 = ORIENTED_EDGE('',*,*,#8989,.F.) ;
#12892 = ORIENTED_EDGE('',*,*,#9003,.F.) ;
#12893 = ORIENTED_EDGE('',*,*,#9010,.T.) ;
#12894 = ORIENTED_EDGE('',*,*,#9008,.T.) ;
#12895 = ORIENTED_EDGE('',*,*,#8990,.F.) ;
#12896 = ORIENTED_EDGE('',*,*,#9009,.F.) ;
#12897 = ORIENTED_EDGE('',*,*,#9007,.T.) ;
#12898 = ORIENTED_EDGE('',*,*,#9011,.F.) ;
#12899 = ORIENTED_EDGE('',*,*,#9012,.T.) ;
#12900 = ORIENTED_EDGE('',*,*,#8992,.T.) ;
#12901 = ORIENTED_EDGE('',*,*,#9006,.T.) ;
#12902 = ORIENTED_EDGE('',*,*,#9013,.T.) ;
#12903 = ORIENTED_EDGE('',*,*,#9014,.T.) ;
#12904 = ORIENTED_EDGE('',*,*,#9011,.T.) ;
#12905 = ORIENTED_EDGE('',*,*,#9015,.F.) ;
#12906 = ORIENTED_EDGE('',*,*,#9016,.F.) ;
#12907 = ORIENTED_EDGE('',*,*,#8995,.F.) ;
#12908 = ORIENTED_EDGE('',*,*,#9017,.F.) ;
#12909 = ORIENTED_EDGE('',*,*,#9014,.F.) ;
#12910 = ORIENTED_EDGE('',*,*,#9018,.T.) ;
#12911 = ORIENTED_EDGE('',*,*,#8993,.F.) ;
#12912 = ORIENTED_EDGE('',*,*,#9012,.F.) ;
#12913 = ORIENTED_EDGE('',*,*,#9019,.T.) ;
#12914 = ORIENTED_EDGE('',*,*,#9017,.T.) ;
#12915 = ORIENTED_EDGE('',*,*,#8994,.F.) ;
#12916 = ORIENTED_EDGE('',*,*,#9018,.F.) ;
#12917 = ORIENTED_EDGE('',*,*,#9016,.T.) ;
#12918 = ORIENTED_EDGE('',*,*,#9020,.F.) ;
#12919 = ORIENTED_EDGE('',*,*,#9021,.T.) ;
#12920 = ORIENTED_EDGE('',*,*,#8996,.T.) ;
#12921 = ORIENTED_EDGE('',*,*,#9015,.T.) ;
#12922 = ORIENTED_EDGE('',*,*,#9022,.T.) ;
#12923 = ORIENTED_EDGE('',*,*,#9023,.T.) ;
#12924 = ORIENTED_EDGE('',*,*,#9020,.T.) ;
#12925 = ORIENTED_EDGE('',*,*,#9024,.F.) ;
#12926 = ORIENTED_EDGE('',*,*,#9025,.F.) ;
#12927 = ORIENTED_EDGE('',*,*,#8999,.F.) ;
#12928 = ORIENTED_EDGE('',*,*,#9026,.F.) ;
#12929 = ORIENTED_EDGE('',*,*,#9023,.F.) ;
#12930 = ORIENTED_EDGE('',*,*,#9027,.T.) ;
#12931 = ORIENTED_EDGE('',*,*,#8997,.F.) ;
#12932 = ORIENTED_EDGE('',*,*,#9021,.F.) ;
#12933 = ORIENTED_EDGE('',*,*,#9028,.T.) ;
#12934 = ORIENTED_EDGE('',*,*,#9026,.T.) ;
#12935 = ORIENTED_EDGE('',*,*,#8998,.F.) ;
#12936 = ORIENTED_EDGE('',*,*,#9027,.F.) ;
#12937 = ORIENTED_EDGE('',*,*,#8982,.T.) ;
#12938 = ORIENTED_EDGE('',*,*,#9029,.T.) ;
#12939 = ORIENTED_EDGE('',*,*,#9024,.T.) ;
#12940 = ORIENTED_EDGE('',*,*,#9030,.T.) ;
#12941 = ORIENTED_EDGE('',*,*,#8985,.T.) ;
#12942 = ORIENTED_EDGE('',*,*,#9000,.T.) ;
#12943 = ORIENTED_EDGE('',*,*,#9025,.T.) ;
#12944 = ORIENTED_EDGE('',*,*,#9029,.F.) ;
#12945 = ORIENTED_EDGE('',*,*,#9030,.F.) ;
#12946 = ORIENTED_EDGE('',*,*,#9028,.F.) ;
#12947 = ORIENTED_EDGE('',*,*,#9022,.F.) ;
#12948 = ORIENTED_EDGE('',*,*,#9019,.F.) ;
#12949 = ORIENTED_EDGE('',*,*,#9013,.F.) ;
#12950 = ORIENTED_EDGE('',*,*,#9010,.F.) ;
#12951 = ORIENTED_EDGE('',*,*,#9004,.F.) ;
#12952 = ORIENTED_EDGE('',*,*,#8986,.F.) ;
#12953 = ORIENTED_EDGE('',*,*,#9031,.T.) ;
#12954 = ORIENTED_EDGE('',*,*,#9001,.T.) ;
#12955 = ORIENTED_EDGE('',*,*,#9032,.T.) ;
#12956 = ORIENTED_EDGE('',*,*,#9031,.F.) ;
#12957 = ORIENTED_EDGE('',*,*,#9032,.F.) ;
#12958 = ORIENTED_EDGE('',*,*,#9033,.F.) ;
#12959 = ORIENTED_EDGE('',*,*,#9034,.T.) ;
#12960 = ORIENTED_EDGE('',*,*,#9035,.T.) ;
#12961 = ORIENTED_EDGE('',*,*,#9036,.T.) ;
#12962 = ORIENTED_EDGE('',*,*,#9037,.F.) ;
#12963 = ORIENTED_EDGE('',*,*,#9038,.T.) ;
#12964 = ORIENTED_EDGE('',*,*,#9039,.F.) ;
#12965 = ORIENTED_EDGE('',*,*,#9040,.T.) ;
#12966 = ORIENTED_EDGE('',*,*,#9041,.T.) ;
#12967 = ORIENTED_EDGE('',*,*,#9042,.T.) ;
#12968 = ORIENTED_EDGE('',*,*,#9043,.F.) ;
#12969 = ORIENTED_EDGE('',*,*,#9044,.T.) ;
#12970 = ORIENTED_EDGE('',*,*,#9045,.F.) ;
#12971 = ORIENTED_EDGE('',*,*,#9046,.T.) ;
#12972 = ORIENTED_EDGE('',*,*,#9047,.T.) ;
#12973 = ORIENTED_EDGE('',*,*,#9048,.T.) ;
#12974 = ORIENTED_EDGE('',*,*,#9049,.F.) ;
#12975 = ORIENTED_EDGE('',*,*,#9050,.T.) ;
#12976 = ORIENTED_EDGE('',*,*,#9051,.F.) ;
#12977 = ORIENTED_EDGE('',*,*,#9052,.T.) ;
#12978 = ORIENTED_EDGE('',*,*,#9053,.T.) ;
#12979 = ORIENTED_EDGE('',*,*,#9054,.T.) ;
#12980 = ORIENTED_EDGE('',*,*,#9055,.F.) ;
#12981 = ORIENTED_EDGE('',*,*,#9056,.T.) ;
#12982 = ORIENTED_EDGE('',*,*,#9057,.F.) ;
#12983 = ORIENTED_EDGE('',*,*,#9058,.T.) ;
#12984 = ORIENTED_EDGE('',*,*,#9059,.T.) ;
#12985 = ORIENTED_EDGE('',*,*,#9060,.T.) ;
#12986 = ORIENTED_EDGE('',*,*,#9061,.F.) ;
#12987 = ORIENTED_EDGE('',*,*,#9062,.T.) ;
#12988 = ORIENTED_EDGE('',*,*,#9063,.F.) ;
#12989 = ORIENTED_EDGE('',*,*,#9064,.T.) ;
#12990 = ORIENTED_EDGE('',*,*,#9065,.T.) ;
#12991 = ORIENTED_EDGE('',*,*,#9066,.T.) ;
#12992 = ORIENTED_EDGE('',*,*,#9067,.F.) ;
#12993 = ORIENTED_EDGE('',*,*,#9068,.T.) ;
#12994 = ORIENTED_EDGE('',*,*,#9069,.F.) ;
#12995 = ORIENTED_EDGE('',*,*,#9070,.T.) ;
#12996 = ORIENTED_EDGE('',*,*,#9071,.T.) ;
#12997 = ORIENTED_EDGE('',*,*,#9072,.T.) ;
#12998 = ORIENTED_EDGE('',*,*,#9073,.F.) ;
#12999 = ORIENTED_EDGE('',*,*,#9074,.T.) ;
#13000 = ORIENTED_EDGE('',*,*,#9075,.F.) ;
#13001 = ORIENTED_EDGE('',*,*,#9076,.T.) ;
#13002 = ORIENTED_EDGE('',*,*,#9077,.T.) ;
#13003 = ORIENTED_EDGE('',*,*,#9078,.T.) ;
#13004 = ORIENTED_EDGE('',*,*,#9079,.F.) ;
#13005 = ORIENTED_EDGE('',*,*,#9080,.T.) ;
#13006 = ORIENTED_EDGE('',*,*,#9081,.F.) ;
#13007 = ORIENTED_EDGE('',*,*,#9082,.T.) ;
#13008 = ORIENTED_EDGE('',*,*,#9083,.T.) ;
#13009 = ORIENTED_EDGE('',*,*,#9084,.T.) ;
#13010 = ORIENTED_EDGE('',*,*,#9085,.F.) ;
#13011 = ORIENTED_EDGE('',*,*,#9086,.T.) ;
#13012 = ORIENTED_EDGE('',*,*,#9087,.F.) ;
#13013 = ORIENTED_EDGE('',*,*,#9088,.T.) ;
#13014 = ORIENTED_EDGE('',*,*,#9089,.T.) ;
#13015 = ORIENTED_EDGE('',*,*,#9090,.T.) ;
#13016 = ORIENTED_EDGE('',*,*,#9091,.F.) ;
#13017 = ORIENTED_EDGE('',*,*,#9092,.T.) ;
#13018 = ORIENTED_EDGE('',*,*,#9093,.F.) ;
#13019 = ORIENTED_EDGE('',*,*,#9094,.T.) ;
#13020 = ORIENTED_EDGE('',*,*,#9095,.T.) ;
#13021 = ORIENTED_EDGE('',*,*,#9096,.T.) ;
#13022 = ORIENTED_EDGE('',*,*,#9097,.F.) ;
#13023 = ORIENTED_EDGE('',*,*,#9098,.T.) ;
#13024 = ORIENTED_EDGE('',*,*,#9099,.F.) ;
#13025 = ORIENTED_EDGE('',*,*,#9100,.T.) ;
#13026 = ORIENTED_EDGE('',*,*,#9101,.T.) ;
#13027 = ORIENTED_EDGE('',*,*,#9102,.T.) ;
#13028 = ORIENTED_EDGE('',*,*,#9103,.F.) ;
#13029 = ORIENTED_EDGE('',*,*,#9104,.T.) ;
#13030 = ORIENTED_EDGE('',*,*,#9105,.F.) ;
#13031 = ORIENTED_EDGE('',*,*,#9106,.T.) ;
#13032 = ORIENTED_EDGE('',*,*,#9107,.T.) ;
#13033 = ORIENTED_EDGE('',*,*,#9108,.T.) ;
#13034 = ORIENTED_EDGE('',*,*,#9109,.F.) ;
#13035 = ORIENTED_EDGE('',*,*,#9110,.T.) ;
#13036 = ORIENTED_EDGE('',*,*,#9111,.F.) ;
#13037 = ORIENTED_EDGE('',*,*,#9112,.T.) ;
#13038 = ORIENTED_EDGE('',*,*,#9113,.T.) ;
#13039 = ORIENTED_EDGE('',*,*,#9114,.T.) ;
#13040 = ORIENTED_EDGE('',*,*,#9115,.F.) ;
#13041 = ORIENTED_EDGE('',*,*,#9116,.T.) ;
#13042 = ORIENTED_EDGE('',*,*,#9117,.F.) ;
#13043 = ORIENTED_EDGE('',*,*,#9118,.T.) ;
#13044 = ORIENTED_EDGE('',*,*,#9119,.T.) ;
#13045 = ORIENTED_EDGE('',*,*,#9120,.T.) ;
#13046 = ORIENTED_EDGE('',*,*,#9121,.F.) ;
#13047 = ORIENTED_EDGE('',*,*,#9122,.T.) ;
#13048 = ORIENTED_EDGE('',*,*,#9123,.F.) ;
#13049 = ORIENTED_EDGE('',*,*,#9124,.T.) ;
#13050 = ORIENTED_EDGE('',*,*,#9125,.T.) ;
#13051 = ORIENTED_EDGE('',*,*,#9126,.T.) ;
#13052 = ORIENTED_EDGE('',*,*,#9127,.F.) ;
#13053 = ORIENTED_EDGE('',*,*,#9128,.T.) ;
#13054 = ORIENTED_EDGE('',*,*,#9129,.F.) ;
#13055 = ORIENTED_EDGE('',*,*,#9130,.T.) ;
#13056 = ORIENTED_EDGE('',*,*,#9131,.T.) ;
#13057 = ORIENTED_EDGE('',*,*,#9132,.T.) ;
#13058 = ORIENTED_EDGE('',*,*,#9133,.F.) ;
#13059 = ORIENTED_EDGE('',*,*,#9134,.T.) ;
#13060 = ORIENTED_EDGE('',*,*,#9135,.F.) ;
#13061 = ORIENTED_EDGE('',*,*,#9136,.T.) ;
#13062 = ORIENTED_EDGE('',*,*,#9137,.T.) ;
#13063 = ORIENTED_EDGE('',*,*,#9138,.T.) ;
#13064 = ORIENTED_EDGE('',*,*,#9139,.F.) ;
#13065 = ORIENTED_EDGE('',*,*,#9140,.T.) ;
#13066 = ORIENTED_EDGE('',*,*,#9141,.F.) ;
#13067 = ORIENTED_EDGE('',*,*,#9142,.T.) ;
#13068 = ORIENTED_EDGE('',*,*,#9143,.T.) ;
#13069 = ORIENTED_EDGE('',*,*,#9144,.T.) ;
#13070 = ORIENTED_EDGE('',*,*,#9145,.F.) ;
#13071 = ORIENTED_EDGE('',*,*,#9146,.T.) ;
#13072 = ORIENTED_EDGE('',*,*,#9147,.F.) ;
#13073 = ORIENTED_EDGE('',*,*,#9148,.T.) ;
#13074 = ORIENTED_EDGE('',*,*,#9149,.T.) ;
#13075 = ORIENTED_EDGE('',*,*,#9150,.T.) ;
#13076 = ORIENTED_EDGE('',*,*,#9151,.F.) ;
#13077 = ORIENTED_EDGE('',*,*,#9152,.T.) ;
#13078 = ORIENTED_EDGE('',*,*,#9153,.F.) ;
#13079 = ORIENTED_EDGE('',*,*,#9154,.T.) ;
#13080 = ORIENTED_EDGE('',*,*,#9155,.T.) ;
#13081 = ORIENTED_EDGE('',*,*,#9156,.T.) ;
#13082 = ORIENTED_EDGE('',*,*,#9157,.F.) ;
#13083 = ORIENTED_EDGE('',*,*,#9158,.T.) ;
#13084 = ORIENTED_EDGE('',*,*,#9159,.F.) ;
#13085 = ORIENTED_EDGE('',*,*,#9160,.T.) ;
#13086 = ORIENTED_EDGE('',*,*,#9161,.T.) ;
#13087 = ORIENTED_EDGE('',*,*,#9162,.T.) ;
#13088 = ORIENTED_EDGE('',*,*,#9163,.F.) ;
#13089 = ORIENTED_EDGE('',*,*,#9164,.T.) ;
#13090 = ORIENTED_EDGE('',*,*,#9165,.F.) ;
#13091 = ORIENTED_EDGE('',*,*,#9166,.T.) ;
#13092 = ORIENTED_EDGE('',*,*,#9167,.T.) ;
#13093 = ORIENTED_EDGE('',*,*,#9168,.T.) ;
#13094 = ORIENTED_EDGE('',*,*,#9169,.F.) ;
#13095 = ORIENTED_EDGE('',*,*,#9170,.T.) ;
#13096 = ORIENTED_EDGE('',*,*,#9171,.F.) ;
#13097 = ORIENTED_EDGE('',*,*,#9172,.T.) ;
#13098 = ORIENTED_EDGE('',*,*,#9173,.T.) ;
#13099 = ORIENTED_EDGE('',*,*,#9174,.T.) ;
#13100 = ORIENTED_EDGE('',*,*,#9175,.F.) ;
#13101 = ORIENTED_EDGE('',*,*,#9176,.T.) ;
#13102 = ORIENTED_EDGE('',*,*,#9177,.F.) ;
#13103 = ORIENTED_EDGE('',*,*,#9178,.T.) ;
#13104 = ORIENTED_EDGE('',*,*,#9179,.T.) ;
#13105 = ORIENTED_EDGE('',*,*,#9180,.T.) ;
#13106 = ORIENTED_EDGE('',*,*,#9181,.F.) ;
#13107 = ORIENTED_EDGE('',*,*,#9182,.T.) ;
#13108 = ORIENTED_EDGE('',*,*,#9183,.F.) ;
#13109 = ORIENTED_EDGE('',*,*,#9184,.T.) ;
#13110 = ORIENTED_EDGE('',*,*,#9185,.T.) ;
#13111 = ORIENTED_EDGE('',*,*,#9186,.T.) ;
#13112 = ORIENTED_EDGE('',*,*,#9187,.F.) ;
#13113 = ORIENTED_EDGE('',*,*,#9188,.T.) ;
#13114 = ORIENTED_EDGE('',*,*,#9189,.F.) ;
#13115 = ORIENTED_EDGE('',*,*,#9190,.T.) ;
#13116 = ORIENTED_EDGE('',*,*,#9191,.T.) ;
#13117 = ORIENTED_EDGE('',*,*,#9192,.T.) ;
#13118 = ORIENTED_EDGE('',*,*,#9193,.F.) ;
#13119 = ORIENTED_EDGE('',*,*,#9194,.T.) ;
#13120 = ORIENTED_EDGE('',*,*,#9195,.F.) ;
#13121 = ORIENTED_EDGE('',*,*,#9196,.T.) ;
#13122 = ORIENTED_EDGE('',*,*,#9197,.T.) ;
#13123 = ORIENTED_EDGE('',*,*,#9198,.T.) ;
#13124 = ORIENTED_EDGE('',*,*,#9199,.F.) ;
#13125 = ORIENTED_EDGE('',*,*,#9200,.T.) ;
#13126 = ORIENTED_EDGE('',*,*,#9201,.F.) ;
#13127 = ORIENTED_EDGE('',*,*,#9202,.T.) ;
#13128 = ORIENTED_EDGE('',*,*,#9203,.T.) ;
#13129 = ORIENTED_EDGE('',*,*,#9204,.T.) ;
#13130 = ORIENTED_EDGE('',*,*,#9205,.F.) ;
#13131 = ORIENTED_EDGE('',*,*,#9206,.T.) ;
#13132 = ORIENTED_EDGE('',*,*,#9207,.F.) ;
#13133 = ORIENTED_EDGE('',*,*,#9208,.T.) ;
#13134 = ORIENTED_EDGE('',*,*,#9209,.T.) ;
#13135 = ORIENTED_EDGE('',*,*,#9034,.F.) ;
#13136 = ORIENTED_EDGE('',*,*,#9033,.T.) ;
#13137 = ORIENTED_EDGE('',*,*,#9210,.T.) ;
#13138 = ORIENTED_EDGE('',*,*,#9211,.F.) ;
#13139 = ORIENTED_EDGE('',*,*,#9212,.F.) ;
#13140 = ORIENTED_EDGE('',*,*,#9213,.F.) ;
#13141 = ORIENTED_EDGE('',*,*,#9214,.F.) ;
#13142 = ORIENTED_EDGE('',*,*,#9215,.F.) ;
#13143 = ORIENTED_EDGE('',*,*,#9216,.F.) ;
#13144 = ORIENTED_EDGE('',*,*,#9217,.F.) ;
#13145 = ORIENTED_EDGE('',*,*,#9218,.F.) ;
#13146 = ORIENTED_EDGE('',*,*,#9219,.F.) ;
#13147 = ORIENTED_EDGE('',*,*,#9220,.F.) ;
#13148 = ORIENTED_EDGE('',*,*,#9221,.F.) ;
#13149 = ORIENTED_EDGE('',*,*,#9222,.F.) ;
#13150 = ORIENTED_EDGE('',*,*,#9223,.F.) ;
#13151 = ORIENTED_EDGE('',*,*,#9224,.F.) ;
#13152 = ORIENTED_EDGE('',*,*,#9225,.F.) ;
#13153 = ORIENTED_EDGE('',*,*,#9226,.F.) ;
#13154 = ORIENTED_EDGE('',*,*,#9227,.F.) ;
#13155 = ORIENTED_EDGE('',*,*,#9228,.F.) ;
#13156 = ORIENTED_EDGE('',*,*,#9229,.F.) ;
#13157 = ORIENTED_EDGE('',*,*,#9230,.F.) ;
#13158 = ORIENTED_EDGE('',*,*,#9231,.F.) ;
#13159 = ORIENTED_EDGE('',*,*,#9232,.F.) ;
#13160 = ORIENTED_EDGE('',*,*,#9233,.F.) ;
#13161 = ORIENTED_EDGE('',*,*,#9234,.F.) ;
#13162 = ORIENTED_EDGE('',*,*,#9235,.F.) ;
#13163 = ORIENTED_EDGE('',*,*,#9236,.F.) ;
#13164 = ORIENTED_EDGE('',*,*,#9237,.F.) ;
#13165 = ORIENTED_EDGE('',*,*,#9238,.F.) ;
#13166 = ORIENTED_EDGE('',*,*,#9239,.F.) ;
#13167 = ORIENTED_EDGE('',*,*,#9240,.F.) ;
#13168 = ORIENTED_EDGE('',*,*,#9241,.F.) ;
#13169 = ORIENTED_EDGE('',*,*,#9242,.F.) ;
#13170 = ORIENTED_EDGE('',*,*,#9243,.F.) ;
#13171 = ORIENTED_EDGE('',*,*,#9244,.F.) ;
#13172 = ORIENTED_EDGE('',*,*,#9245,.F.) ;
#13173 = ORIENTED_EDGE('',*,*,#9246,.F.) ;
#13174 = ORIENTED_EDGE('',*,*,#9247,.F.) ;
#13175 = ORIENTED_EDGE('',*,*,#9248,.F.) ;
#13176 = ORIENTED_EDGE('',*,*,#9249,.F.) ;
#13177 = ORIENTED_EDGE('',*,*,#9250,.F.) ;
#13178 = ORIENTED_EDGE('',*,*,#9251,.F.) ;
#13179 = ORIENTED_EDGE('',*,*,#9252,.F.) ;
#13180 = ORIENTED_EDGE('',*,*,#9253,.F.) ;
#13181 = ORIENTED_EDGE('',*,*,#9254,.F.) ;
#13182 = ORIENTED_EDGE('',*,*,#9255,.F.) ;
#13183 = ORIENTED_EDGE('',*,*,#9256,.F.) ;
#13184 = ORIENTED_EDGE('',*,*,#9257,.F.) ;
#13185 = ORIENTED_EDGE('',*,*,#9258,.F.) ;
#13186 = ORIENTED_EDGE('',*,*,#9259,.F.) ;
#13187 = ORIENTED_EDGE('',*,*,#9260,.F.) ;
#13188 = ORIENTED_EDGE('',*,*,#9261,.F.) ;
#13189 = ORIENTED_EDGE('',*,*,#9262,.F.) ;
#13190 = ORIENTED_EDGE('',*,*,#9263,.F.) ;
#13191 = ORIENTED_EDGE('',*,*,#9264,.F.) ;
#13192 = ORIENTED_EDGE('',*,*,#9265,.F.) ;
#13193 = ORIENTED_EDGE('',*,*,#9266,.F.) ;
#13194 = ORIENTED_EDGE('',*,*,#9267,.F.) ;
#13195 = ORIENTED_EDGE('',*,*,#9268,.F.) ;
#13196 = ORIENTED_EDGE('',*,*,#9269,.F.) ;
#13197 = ORIENTED_EDGE('',*,*,#9270,.F.) ;
#13198 = ORIENTED_EDGE('',*,*,#9271,.F.) ;
#13199 = ORIENTED_EDGE('',*,*,#9272,.F.) ;
#13200 = ORIENTED_EDGE('',*,*,#9273,.F.) ;
#13201 = ORIENTED_EDGE('',*,*,#9274,.F.) ;
#13202 = ORIENTED_EDGE('',*,*,#9275,.F.) ;
#13203 = ORIENTED_EDGE('',*,*,#9276,.F.) ;
#13204 = ORIENTED_EDGE('',*,*,#9277,.F.) ;
#13205 = ORIENTED_EDGE('',*,*,#9278,.F.) ;
#13206 = ORIENTED_EDGE('',*,*,#9279,.F.) ;
#13207 = ORIENTED_EDGE('',*,*,#9280,.F.) ;
#13208 = ORIENTED_EDGE('',*,*,#9281,.F.) ;
#13209 = ORIENTED_EDGE('',*,*,#9282,.F.) ;
#13210 = ORIENTED_EDGE('',*,*,#9283,.F.) ;
#13211 = ORIENTED_EDGE('',*,*,#9284,.F.) ;
#13212 = ORIENTED_EDGE('',*,*,#9285,.F.) ;
#13213 = ORIENTED_EDGE('',*,*,#9286,.F.) ;
#13214 = ORIENTED_EDGE('',*,*,#9287,.F.) ;
#13215 = ORIENTED_EDGE('',*,*,#9288,.F.) ;
#13216 = ORIENTED_EDGE('',*,*,#9289,.F.) ;
#13217 = ORIENTED_EDGE('',*,*,#9290,.F.) ;
#13218 = ORIENTED_EDGE('',*,*,#9291,.F.) ;
#13219 = ORIENTED_EDGE('',*,*,#9292,.F.) ;
#13220 = ORIENTED_EDGE('',*,*,#9293,.F.) ;
#13221 = ORIENTED_EDGE('',*,*,#9294,.F.) ;
#13222 = ORIENTED_EDGE('',*,*,#9295,.F.) ;
#13223 = ORIENTED_EDGE('',*,*,#9296,.F.) ;
#13224 = ORIENTED_EDGE('',*,*,#9297,.F.) ;
#13225 = ORIENTED_EDGE('',*,*,#9298,.F.) ;
#13226 = ORIENTED_EDGE('',*,*,#9299,.F.) ;
#13227 = ORIENTED_EDGE('',*,*,#9300,.F.) ;
#13228 = ORIENTED_EDGE('',*,*,#9301,.F.) ;
#13229 = ORIENTED_EDGE('',*,*,#9302,.F.) ;
#13230 = ORIENTED_EDGE('',*,*,#9303,.F.) ;
#13231 = ORIENTED_EDGE('',*,*,#9304,.F.) ;
#13232 = ORIENTED_EDGE('',*,*,#9305,.F.) ;
#13233 = ORIENTED_EDGE('',*,*,#9306,.F.) ;
#13234 = ORIENTED_EDGE('',*,*,#9307,.F.) ;
#13235 = ORIENTED_EDGE('',*,*,#9308,.F.) ;
#13236 = ORIENTED_EDGE('',*,*,#9309,.F.) ;
#13237 = ORIENTED_EDGE('',*,*,#9310,.F.) ;
#13238 = ORIENTED_EDGE('',*,*,#9311,.F.) ;
#13239 = ORIENTED_EDGE('',*,*,#9312,.F.) ;
#13240 = ORIENTED_EDGE('',*,*,#9313,.F.) ;
#13241 = ORIENTED_EDGE('',*,*,#9314,.F.) ;
#13242 = ORIENTED_EDGE('',*,*,#9315,.F.) ;
#13243 = ORIENTED_EDGE('',*,*,#9316,.F.) ;
#13244 = ORIENTED_EDGE('',*,*,#9317,.F.) ;
#13245 = ORIENTED_EDGE('',*,*,#9318,.F.) ;
#13246 = ORIENTED_EDGE('',*,*,#9319,.F.) ;
#13247 = ORIENTED_EDGE('',*,*,#9320,.F.) ;
#13248 = ORIENTED_EDGE('',*,*,#9321,.F.) ;
#13249 = ORIENTED_EDGE('',*,*,#9210,.F.) ;
#13250 = ORIENTED_EDGE('',*,*,#9322,.F.) ;
#13251 = ORIENTED_EDGE('',*,*,#9323,.F.) ;
#13252 = ORIENTED_EDGE('',*,*,#9324,.F.) ;
#13253 = ORIENTED_EDGE('',*,*,#9325,.F.) ;
#13254 = ORIENTED_EDGE('',*,*,#9326,.F.) ;
#13255 = ORIENTED_EDGE('',*,*,#9327,.F.) ;
#13256 = ORIENTED_EDGE('',*,*,#9209,.F.) ;
#13257 = ORIENTED_EDGE('',*,*,#9328,.T.) ;
#13258 = ORIENTED_EDGE('',*,*,#9329,.F.) ;
#13259 = ORIENTED_EDGE('',*,*,#9206,.F.) ;
#13260 = ORIENTED_EDGE('',*,*,#9330,.F.) ;
#13261 = ORIENTED_EDGE('',*,*,#9331,.T.) ;
#13262 = ORIENTED_EDGE('',*,*,#9203,.F.) ;
#13263 = ORIENTED_EDGE('',*,*,#9332,.T.) ;
#13264 = ORIENTED_EDGE('',*,*,#9333,.F.) ;
#13265 = ORIENTED_EDGE('',*,*,#9200,.F.) ;
#13266 = ORIENTED_EDGE('',*,*,#9334,.F.) ;
#13267 = ORIENTED_EDGE('',*,*,#9335,.T.) ;
#13268 = ORIENTED_EDGE('',*,*,#9197,.F.) ;
#13269 = ORIENTED_EDGE('',*,*,#9336,.T.) ;
#13270 = ORIENTED_EDGE('',*,*,#9337,.F.) ;
#13271 = ORIENTED_EDGE('',*,*,#9194,.F.) ;
#13272 = ORIENTED_EDGE('',*,*,#9338,.F.) ;
#13273 = ORIENTED_EDGE('',*,*,#9339,.T.) ;
#13274 = ORIENTED_EDGE('',*,*,#9191,.F.) ;
#13275 = ORIENTED_EDGE('',*,*,#9340,.T.) ;
#13276 = ORIENTED_EDGE('',*,*,#9341,.F.) ;
#13277 = ORIENTED_EDGE('',*,*,#9188,.F.) ;
#13278 = ORIENTED_EDGE('',*,*,#9342,.F.) ;
#13279 = ORIENTED_EDGE('',*,*,#9343,.T.) ;
#13280 = ORIENTED_EDGE('',*,*,#9185,.F.) ;
#13281 = ORIENTED_EDGE('',*,*,#9344,.T.) ;
#13282 = ORIENTED_EDGE('',*,*,#9345,.F.) ;
#13283 = ORIENTED_EDGE('',*,*,#9182,.F.) ;
#13284 = ORIENTED_EDGE('',*,*,#9346,.F.) ;
#13285 = ORIENTED_EDGE('',*,*,#9347,.T.) ;
#13286 = ORIENTED_EDGE('',*,*,#9179,.F.) ;
#13287 = ORIENTED_EDGE('',*,*,#9348,.T.) ;
#13288 = ORIENTED_EDGE('',*,*,#9349,.F.) ;
#13289 = ORIENTED_EDGE('',*,*,#9176,.F.) ;
#13290 = ORIENTED_EDGE('',*,*,#9350,.F.) ;
#13291 = ORIENTED_EDGE('',*,*,#9351,.T.) ;
#13292 = ORIENTED_EDGE('',*,*,#9173,.F.) ;
#13293 = ORIENTED_EDGE('',*,*,#9352,.T.) ;
#13294 = ORIENTED_EDGE('',*,*,#9353,.F.) ;
#13295 = ORIENTED_EDGE('',*,*,#9170,.F.) ;
#13296 = ORIENTED_EDGE('',*,*,#9354,.F.) ;
#13297 = ORIENTED_EDGE('',*,*,#9355,.T.) ;
#13298 = ORIENTED_EDGE('',*,*,#9167,.F.) ;
#13299 = ORIENTED_EDGE('',*,*,#9356,.T.) ;
#13300 = ORIENTED_EDGE('',*,*,#9357,.F.) ;
#13301 = ORIENTED_EDGE('',*,*,#9164,.F.) ;
#13302 = ORIENTED_EDGE('',*,*,#9358,.F.) ;
#13303 = ORIENTED_EDGE('',*,*,#9359,.T.) ;
#13304 = ORIENTED_EDGE('',*,*,#9161,.F.) ;
#13305 = ORIENTED_EDGE('',*,*,#9360,.T.) ;
#13306 = ORIENTED_EDGE('',*,*,#9361,.F.) ;
#13307 = ORIENTED_EDGE('',*,*,#9158,.F.) ;
#13308 = ORIENTED_EDGE('',*,*,#9362,.F.) ;
#13309 = ORIENTED_EDGE('',*,*,#9363,.T.) ;
#13310 = ORIENTED_EDGE('',*,*,#9155,.F.) ;
#13311 = ORIENTED_EDGE('',*,*,#9364,.T.) ;
#13312 = ORIENTED_EDGE('',*,*,#9365,.F.) ;
#13313 = ORIENTED_EDGE('',*,*,#9152,.F.) ;
#13314 = ORIENTED_EDGE('',*,*,#9366,.F.) ;
#13315 = ORIENTED_EDGE('',*,*,#9367,.T.) ;
#13316 = ORIENTED_EDGE('',*,*,#9149,.F.) ;
#13317 = ORIENTED_EDGE('',*,*,#9368,.T.) ;
#13318 = ORIENTED_EDGE('',*,*,#9369,.F.) ;
#13319 = ORIENTED_EDGE('',*,*,#9146,.F.) ;
#13320 = ORIENTED_EDGE('',*,*,#9370,.F.) ;
#13321 = ORIENTED_EDGE('',*,*,#9371,.T.) ;
#13322 = ORIENTED_EDGE('',*,*,#9143,.F.) ;
#13323 = ORIENTED_EDGE('',*,*,#9372,.T.) ;
#13324 = ORIENTED_EDGE('',*,*,#9373,.F.) ;
#13325 = ORIENTED_EDGE('',*,*,#9140,.F.) ;
#13326 = ORIENTED_EDGE('',*,*,#9374,.F.) ;
#13327 = ORIENTED_EDGE('',*,*,#9375,.T.) ;
#13328 = ORIENTED_EDGE('',*,*,#9137,.F.) ;
#13329 = ORIENTED_EDGE('',*,*,#9376,.T.) ;
#13330 = ORIENTED_EDGE('',*,*,#9377,.F.) ;
#13331 = ORIENTED_EDGE('',*,*,#9134,.F.) ;
#13332 = ORIENTED_EDGE('',*,*,#9378,.F.) ;
#13333 = ORIENTED_EDGE('',*,*,#9379,.T.) ;
#13334 = ORIENTED_EDGE('',*,*,#9131,.F.) ;
#13335 = ORIENTED_EDGE('',*,*,#9380,.T.) ;
#13336 = ORIENTED_EDGE('',*,*,#9381,.F.) ;
#13337 = ORIENTED_EDGE('',*,*,#9128,.F.) ;
#13338 = ORIENTED_EDGE('',*,*,#9382,.F.) ;
#13339 = ORIENTED_EDGE('',*,*,#9383,.T.) ;
#13340 = ORIENTED_EDGE('',*,*,#9125,.F.) ;
#13341 = ORIENTED_EDGE('',*,*,#9384,.T.) ;
#13342 = ORIENTED_EDGE('',*,*,#9385,.F.) ;
#13343 = ORIENTED_EDGE('',*,*,#9122,.F.) ;
#13344 = ORIENTED_EDGE('',*,*,#9386,.F.) ;
#13345 = ORIENTED_EDGE('',*,*,#9387,.T.) ;
#13346 = ORIENTED_EDGE('',*,*,#9119,.F.) ;
#13347 = ORIENTED_EDGE('',*,*,#9388,.T.) ;
#13348 = ORIENTED_EDGE('',*,*,#9389,.F.) ;
#13349 = ORIENTED_EDGE('',*,*,#9116,.F.) ;
#13350 = ORIENTED_EDGE('',*,*,#9390,.F.) ;
#13351 = ORIENTED_EDGE('',*,*,#9391,.T.) ;
#13352 = ORIENTED_EDGE('',*,*,#9113,.F.) ;
#13353 = ORIENTED_EDGE('',*,*,#9392,.T.) ;
#13354 = ORIENTED_EDGE('',*,*,#9393,.F.) ;
#13355 = ORIENTED_EDGE('',*,*,#9110,.F.) ;
#13356 = ORIENTED_EDGE('',*,*,#9394,.F.) ;
#13357 = ORIENTED_EDGE('',*,*,#9395,.T.) ;
#13358 = ORIENTED_EDGE('',*,*,#9107,.F.) ;
#13359 = ORIENTED_EDGE('',*,*,#9396,.T.) ;
#13360 = ORIENTED_EDGE('',*,*,#9397,.F.) ;
#13361 = ORIENTED_EDGE('',*,*,#9104,.F.) ;
#13362 = ORIENTED_EDGE('',*,*,#9398,.F.) ;
#13363 = ORIENTED_EDGE('',*,*,#9399,.T.) ;
#13364 = ORIENTED_EDGE('',*,*,#9101,.F.) ;
#13365 = ORIENTED_EDGE('',*,*,#9400,.T.) ;
#13366 = ORIENTED_EDGE('',*,*,#9401,.F.) ;
#13367 = ORIENTED_EDGE('',*,*,#9098,.F.) ;
#13368 = ORIENTED_EDGE('',*,*,#9402,.F.) ;
#13369 = ORIENTED_EDGE('',*,*,#9403,.T.) ;
#13370 = ORIENTED_EDGE('',*,*,#9095,.F.) ;
#13371 = ORIENTED_EDGE('',*,*,#9404,.T.) ;
#13372 = ORIENTED_EDGE('',*,*,#9405,.F.) ;
#13373 = ORIENTED_EDGE('',*,*,#9092,.F.) ;
#13374 = ORIENTED_EDGE('',*,*,#9406,.F.) ;
#13375 = ORIENTED_EDGE('',*,*,#9407,.T.) ;
#13376 = ORIENTED_EDGE('',*,*,#9089,.F.) ;
#13377 = ORIENTED_EDGE('',*,*,#9408,.T.) ;
#13378 = ORIENTED_EDGE('',*,*,#9409,.F.) ;
#13379 = ORIENTED_EDGE('',*,*,#9086,.F.) ;
#13380 = ORIENTED_EDGE('',*,*,#9410,.F.) ;
#13381 = ORIENTED_EDGE('',*,*,#9411,.T.) ;
#13382 = ORIENTED_EDGE('',*,*,#9083,.F.) ;
#13383 = ORIENTED_EDGE('',*,*,#9412,.T.) ;
#13384 = ORIENTED_EDGE('',*,*,#9413,.F.) ;
#13385 = ORIENTED_EDGE('',*,*,#9080,.F.) ;
#13386 = ORIENTED_EDGE('',*,*,#9414,.F.) ;
#13387 = ORIENTED_EDGE('',*,*,#9415,.T.) ;
#13388 = ORIENTED_EDGE('',*,*,#9077,.F.) ;
#13389 = ORIENTED_EDGE('',*,*,#9416,.T.) ;
#13390 = ORIENTED_EDGE('',*,*,#9417,.F.) ;
#13391 = ORIENTED_EDGE('',*,*,#9074,.F.) ;
#13392 = ORIENTED_EDGE('',*,*,#9418,.F.) ;
#13393 = ORIENTED_EDGE('',*,*,#9419,.T.) ;
#13394 = ORIENTED_EDGE('',*,*,#9071,.F.) ;
#13395 = ORIENTED_EDGE('',*,*,#9420,.T.) ;
#13396 = ORIENTED_EDGE('',*,*,#9421,.F.) ;
#13397 = ORIENTED_EDGE('',*,*,#9068,.F.) ;
#13398 = ORIENTED_EDGE('',*,*,#9422,.F.) ;
#13399 = ORIENTED_EDGE('',*,*,#9423,.T.) ;
#13400 = ORIENTED_EDGE('',*,*,#9065,.F.) ;
#13401 = ORIENTED_EDGE('',*,*,#9424,.T.) ;
#13402 = ORIENTED_EDGE('',*,*,#9425,.F.) ;
#13403 = ORIENTED_EDGE('',*,*,#9062,.F.) ;
#13404 = ORIENTED_EDGE('',*,*,#9426,.F.) ;
#13405 = ORIENTED_EDGE('',*,*,#9427,.T.) ;
#13406 = ORIENTED_EDGE('',*,*,#9059,.F.) ;
#13407 = ORIENTED_EDGE('',*,*,#9428,.T.) ;
#13408 = ORIENTED_EDGE('',*,*,#9429,.F.) ;
#13409 = ORIENTED_EDGE('',*,*,#9056,.F.) ;
#13410 = ORIENTED_EDGE('',*,*,#9430,.F.) ;
#13411 = ORIENTED_EDGE('',*,*,#9431,.T.) ;
#13412 = ORIENTED_EDGE('',*,*,#9053,.F.) ;
#13413 = ORIENTED_EDGE('',*,*,#9432,.T.) ;
#13414 = ORIENTED_EDGE('',*,*,#9433,.F.) ;
#13415 = ORIENTED_EDGE('',*,*,#9050,.F.) ;
#13416 = ORIENTED_EDGE('',*,*,#9434,.F.) ;
#13417 = ORIENTED_EDGE('',*,*,#9435,.T.) ;
#13418 = ORIENTED_EDGE('',*,*,#9047,.F.) ;
#13419 = ORIENTED_EDGE('',*,*,#9436,.T.) ;
#13420 = ORIENTED_EDGE('',*,*,#9437,.F.) ;
#13421 = ORIENTED_EDGE('',*,*,#9044,.F.) ;
#13422 = ORIENTED_EDGE('',*,*,#9438,.F.) ;
#13423 = ORIENTED_EDGE('',*,*,#9439,.T.) ;
#13424 = ORIENTED_EDGE('',*,*,#9041,.F.) ;
#13425 = ORIENTED_EDGE('',*,*,#9440,.T.) ;
#13426 = ORIENTED_EDGE('',*,*,#9441,.F.) ;
#13427 = ORIENTED_EDGE('',*,*,#9038,.F.) ;
#13428 = ORIENTED_EDGE('',*,*,#9442,.F.) ;
#13429 = ORIENTED_EDGE('',*,*,#9443,.T.) ;
#13430 = ORIENTED_EDGE('',*,*,#9035,.F.) ;
#13431 = ORIENTED_EDGE('',*,*,#9444,.T.) ;
#13432 = ORIENTED_EDGE('',*,*,#9445,.T.) ;
#13433 = ORIENTED_EDGE('',*,*,#9444,.F.) ;
#13434 = ORIENTED_EDGE('',*,*,#9446,.T.) ;
#13435 = ORIENTED_EDGE('',*,*,#9447,.T.) ;
#13436 = ORIENTED_EDGE('',*,*,#9448,.F.) ;
#13437 = ORIENTED_EDGE('',*,*,#9447,.F.) ;
#13438 = ORIENTED_EDGE('',*,*,#9449,.F.) ;
#13439 = ORIENTED_EDGE('',*,*,#9450,.F.) ;
#13440 = ORIENTED_EDGE('',*,*,#9451,.F.) ;
#13441 = ORIENTED_EDGE('',*,*,#9452,.F.) ;
#13442 = ORIENTED_EDGE('',*,*,#9453,.F.) ;
#13443 = ORIENTED_EDGE('',*,*,#9454,.F.) ;
#13444 = ORIENTED_EDGE('',*,*,#9455,.F.) ;
#13445 = ORIENTED_EDGE('',*,*,#9456,.F.) ;
#13446 = ORIENTED_EDGE('',*,*,#9457,.F.) ;
#13447 = ORIENTED_EDGE('',*,*,#9458,.F.) ;
#13448 = ORIENTED_EDGE('',*,*,#9459,.F.) ;
#13449 = ORIENTED_EDGE('',*,*,#9460,.F.) ;
#13450 = ORIENTED_EDGE('',*,*,#9461,.F.) ;
#13451 = ORIENTED_EDGE('',*,*,#9462,.F.) ;
#13452 = ORIENTED_EDGE('',*,*,#9463,.F.) ;
#13453 = ORIENTED_EDGE('',*,*,#9464,.F.) ;
#13454 = ORIENTED_EDGE('',*,*,#9465,.F.) ;
#13455 = ORIENTED_EDGE('',*,*,#9466,.F.) ;
#13456 = ORIENTED_EDGE('',*,*,#9467,.F.) ;
#13457 = ORIENTED_EDGE('',*,*,#9468,.F.) ;
#13458 = ORIENTED_EDGE('',*,*,#9469,.F.) ;
#13459 = ORIENTED_EDGE('',*,*,#9470,.F.) ;
#13460 = ORIENTED_EDGE('',*,*,#9471,.F.) ;
#13461 = ORIENTED_EDGE('',*,*,#9472,.F.) ;
#13462 = ORIENTED_EDGE('',*,*,#9473,.F.) ;
#13463 = ORIENTED_EDGE('',*,*,#9474,.F.) ;
#13464 = ORIENTED_EDGE('',*,*,#9475,.F.) ;
#13465 = ORIENTED_EDGE('',*,*,#9476,.F.) ;
#13466 = ORIENTED_EDGE('',*,*,#9477,.F.) ;
#13467 = ORIENTED_EDGE('',*,*,#9478,.F.) ;
#13468 = ORIENTED_EDGE('',*,*,#9479,.F.) ;
#13469 = ORIENTED_EDGE('',*,*,#9480,.F.) ;
#13470 = ORIENTED_EDGE('',*,*,#9481,.F.) ;
#13471 = ORIENTED_EDGE('',*,*,#9482,.F.) ;
#13472 = ORIENTED_EDGE('',*,*,#9483,.F.) ;
#13473 = ORIENTED_EDGE('',*,*,#9484,.F.) ;
#13474 = ORIENTED_EDGE('',*,*,#9485,.F.) ;
#13475 = ORIENTED_EDGE('',*,*,#9486,.F.) ;
#13476 = ORIENTED_EDGE('',*,*,#9487,.F.) ;
#13477 = ORIENTED_EDGE('',*,*,#9488,.F.) ;
#13478 = ORIENTED_EDGE('',*,*,#9489,.F.) ;
#13479 = ORIENTED_EDGE('',*,*,#9490,.F.) ;
#13480 = ORIENTED_EDGE('',*,*,#9491,.F.) ;
#13481 = ORIENTED_EDGE('',*,*,#9492,.F.) ;
#13482 = ORIENTED_EDGE('',*,*,#9493,.F.) ;
#13483 = ORIENTED_EDGE('',*,*,#9494,.F.) ;
#13484 = ORIENTED_EDGE('',*,*,#9495,.F.) ;
#13485 = ORIENTED_EDGE('',*,*,#9496,.F.) ;
#13486 = ORIENTED_EDGE('',*,*,#9497,.F.) ;
#13487 = ORIENTED_EDGE('',*,*,#9498,.F.) ;
#13488 = ORIENTED_EDGE('',*,*,#9499,.F.) ;
#13489 = ORIENTED_EDGE('',*,*,#9500,.F.) ;
#13490 = ORIENTED_EDGE('',*,*,#9501,.F.) ;
#13491 = ORIENTED_EDGE('',*,*,#9502,.F.) ;
#13492 = ORIENTED_EDGE('',*,*,#9503,.F.) ;
#13493 = ORIENTED_EDGE('',*,*,#9504,.F.) ;
#13494 = ORIENTED_EDGE('',*,*,#9505,.F.) ;
#13495 = ORIENTED_EDGE('',*,*,#9506,.F.) ;
#13496 = ORIENTED_EDGE('',*,*,#9507,.F.) ;
#13497 = ORIENTED_EDGE('',*,*,#9508,.F.) ;
#13498 = ORIENTED_EDGE('',*,*,#9509,.F.) ;
#13499 = ORIENTED_EDGE('',*,*,#9510,.F.) ;
#13500 = ORIENTED_EDGE('',*,*,#9511,.F.) ;
#13501 = ORIENTED_EDGE('',*,*,#9512,.F.) ;
#13502 = ORIENTED_EDGE('',*,*,#9513,.F.) ;
#13503 = ORIENTED_EDGE('',*,*,#9514,.F.) ;
#13504 = ORIENTED_EDGE('',*,*,#9515,.F.) ;
#13505 = ORIENTED_EDGE('',*,*,#9516,.F.) ;
#13506 = ORIENTED_EDGE('',*,*,#9517,.F.) ;
#13507 = ORIENTED_EDGE('',*,*,#9518,.F.) ;
#13508 = ORIENTED_EDGE('',*,*,#9519,.F.) ;
#13509 = ORIENTED_EDGE('',*,*,#9520,.F.) ;
#13510 = ORIENTED_EDGE('',*,*,#9521,.F.) ;
#13511 = ORIENTED_EDGE('',*,*,#9522,.F.) ;
#13512 = ORIENTED_EDGE('',*,*,#9523,.F.) ;
#13513 = ORIENTED_EDGE('',*,*,#9524,.F.) ;
#13514 = ORIENTED_EDGE('',*,*,#9525,.F.) ;
#13515 = ORIENTED_EDGE('',*,*,#9526,.F.) ;
#13516 = ORIENTED_EDGE('',*,*,#9527,.F.) ;
#13517 = ORIENTED_EDGE('',*,*,#9528,.F.) ;
#13518 = ORIENTED_EDGE('',*,*,#9529,.F.) ;
#13519 = ORIENTED_EDGE('',*,*,#9530,.F.) ;
#13520 = ORIENTED_EDGE('',*,*,#9531,.F.) ;
#13521 = ORIENTED_EDGE('',*,*,#9532,.F.) ;
#13522 = ORIENTED_EDGE('',*,*,#9533,.F.) ;
#13523 = ORIENTED_EDGE('',*,*,#9534,.F.) ;
#13524 = ORIENTED_EDGE('',*,*,#9535,.F.) ;
#13525 = ORIENTED_EDGE('',*,*,#9536,.F.) ;
#13526 = ORIENTED_EDGE('',*,*,#9537,.T.) ;
#13527 = ORIENTED_EDGE('',*,*,#9538,.T.) ;
#13528 = ORIENTED_EDGE('',*,*,#9537,.F.) ;
#13529 = ORIENTED_EDGE('',*,*,#9539,.F.) ;
#13530 = ORIENTED_EDGE('',*,*,#9540,.T.) ;
#13531 = ORIENTED_EDGE('',*,*,#9541,.T.) ;
#13532 = ORIENTED_EDGE('',*,*,#9540,.F.) ;
#13533 = ORIENTED_EDGE('',*,*,#9542,.F.) ;
#13534 = ORIENTED_EDGE('',*,*,#9543,.T.) ;
#13535 = ORIENTED_EDGE('',*,*,#9544,.T.) ;
#13536 = ORIENTED_EDGE('',*,*,#9543,.F.) ;
#13537 = ORIENTED_EDGE('',*,*,#9545,.F.) ;
#13538 = ORIENTED_EDGE('',*,*,#9546,.T.) ;
#13539 = ORIENTED_EDGE('',*,*,#9547,.T.) ;
#13540 = ORIENTED_EDGE('',*,*,#9546,.F.) ;
#13541 = ORIENTED_EDGE('',*,*,#9541,.F.) ;
#13542 = ORIENTED_EDGE('',*,*,#9548,.T.) ;
#13543 = ORIENTED_EDGE('',*,*,#9549,.T.) ;
#13544 = ORIENTED_EDGE('',*,*,#9548,.F.) ;
#13545 = ORIENTED_EDGE('',*,*,#9549,.F.) ;
#13546 = ORIENTED_EDGE('',*,*,#9550,.T.) ;
#13547 = ORIENTED_EDGE('',*,*,#9551,.T.) ;
#13548 = ORIENTED_EDGE('',*,*,#9550,.F.) ;
#13549 = ORIENTED_EDGE('',*,*,#9544,.F.) ;
#13550 = ORIENTED_EDGE('',*,*,#9552,.T.) ;
#13551 = ORIENTED_EDGE('',*,*,#9545,.T.) ;
#13552 = ORIENTED_EDGE('',*,*,#9552,.F.) ;
#13553 = ORIENTED_EDGE('',*,*,#9536,.T.) ;
#13554 = ORIENTED_EDGE('',*,*,#9551,.F.) ;
#13555 = ORIENTED_EDGE('',*,*,#9547,.F.) ;
#13556 = ORIENTED_EDGE('',*,*,#9448,.T.) ;
#13557 = ORIENTED_EDGE('',*,*,#9542,.T.) ;
#13558 = ORIENTED_EDGE('',*,*,#9446,.F.) ;
#13559 = ORIENTED_EDGE('',*,*,#9553,.T.) ;
#13560 = ORIENTED_EDGE('',*,*,#9554,.T.) ;
#13561 = ORIENTED_EDGE('',*,*,#9555,.T.) ;
#13562 = ORIENTED_EDGE('',*,*,#9556,.T.) ;
#13563 = ORIENTED_EDGE('',*,*,#9557,.T.) ;
#13564 = ORIENTED_EDGE('',*,*,#9558,.T.) ;
#13565 = ORIENTED_EDGE('',*,*,#9559,.T.) ;
#13566 = ORIENTED_EDGE('',*,*,#9560,.T.) ;
#13567 = ORIENTED_EDGE('',*,*,#9561,.T.) ;
#13568 = ORIENTED_EDGE('',*,*,#9562,.T.) ;
#13569 = ORIENTED_EDGE('',*,*,#9563,.T.) ;
#13570 = ORIENTED_EDGE('',*,*,#9564,.T.) ;
#13571 = ORIENTED_EDGE('',*,*,#9565,.T.) ;
#13572 = ORIENTED_EDGE('',*,*,#9566,.T.) ;
#13573 = ORIENTED_EDGE('',*,*,#9567,.T.) ;
#13574 = ORIENTED_EDGE('',*,*,#9568,.T.) ;
#13575 = ORIENTED_EDGE('',*,*,#9569,.T.) ;
#13576 = ORIENTED_EDGE('',*,*,#9570,.T.) ;
#13577 = ORIENTED_EDGE('',*,*,#9571,.T.) ;
#13578 = ORIENTED_EDGE('',*,*,#9572,.T.) ;
#13579 = ORIENTED_EDGE('',*,*,#9573,.T.) ;
#13580 = ORIENTED_EDGE('',*,*,#9574,.T.) ;
#13581 = ORIENTED_EDGE('',*,*,#9575,.T.) ;
#13582 = ORIENTED_EDGE('',*,*,#9576,.T.) ;
#13583 = ORIENTED_EDGE('',*,*,#9577,.T.) ;
#13584 = ORIENTED_EDGE('',*,*,#9578,.T.) ;
#13585 = ORIENTED_EDGE('',*,*,#9579,.T.) ;
#13586 = ORIENTED_EDGE('',*,*,#9580,.T.) ;
#13587 = ORIENTED_EDGE('',*,*,#9581,.T.) ;
#13588 = ORIENTED_EDGE('',*,*,#9582,.T.) ;
#13589 = ORIENTED_EDGE('',*,*,#9583,.T.) ;
#13590 = ORIENTED_EDGE('',*,*,#9584,.T.) ;
#13591 = ORIENTED_EDGE('',*,*,#9585,.T.) ;
#13592 = ORIENTED_EDGE('',*,*,#9586,.T.) ;
#13593 = ORIENTED_EDGE('',*,*,#9587,.T.) ;
#13594 = ORIENTED_EDGE('',*,*,#9588,.T.) ;
#13595 = ORIENTED_EDGE('',*,*,#9589,.T.) ;
#13596 = ORIENTED_EDGE('',*,*,#9590,.T.) ;
#13597 = ORIENTED_EDGE('',*,*,#9591,.T.) ;
#13598 = ORIENTED_EDGE('',*,*,#9592,.T.) ;
#13599 = ORIENTED_EDGE('',*,*,#9593,.T.) ;
#13600 = ORIENTED_EDGE('',*,*,#9594,.T.) ;
#13601 = ORIENTED_EDGE('',*,*,#9595,.T.) ;
#13602 = ORIENTED_EDGE('',*,*,#9596,.T.) ;
#13603 = ORIENTED_EDGE('',*,*,#9597,.T.) ;
#13604 = ORIENTED_EDGE('',*,*,#9598,.T.) ;
#13605 = ORIENTED_EDGE('',*,*,#9599,.T.) ;
#13606 = ORIENTED_EDGE('',*,*,#9600,.T.) ;
#13607 = ORIENTED_EDGE('',*,*,#9601,.T.) ;
#13608 = ORIENTED_EDGE('',*,*,#9602,.T.) ;
#13609 = ORIENTED_EDGE('',*,*,#9603,.T.) ;
#13610 = ORIENTED_EDGE('',*,*,#9604,.T.) ;
#13611 = ORIENTED_EDGE('',*,*,#9605,.T.) ;
#13612 = ORIENTED_EDGE('',*,*,#9606,.T.) ;
#13613 = ORIENTED_EDGE('',*,*,#9607,.T.) ;
#13614 = ORIENTED_EDGE('',*,*,#9608,.T.) ;
#13615 = ORIENTED_EDGE('',*,*,#9445,.F.) ;
#13616 = ORIENTED_EDGE('',*,*,#9539,.T.) ;
#13617 = ORIENTED_EDGE('',*,*,#9609,.T.) ;
#13618 = ORIENTED_EDGE('',*,*,#9610,.T.) ;
#13619 = ORIENTED_EDGE('',*,*,#9538,.F.) ;
#13620 = ORIENTED_EDGE('',*,*,#9611,.T.) ;
#13621 = ORIENTED_EDGE('',*,*,#9321,.T.) ;
#13622 = ORIENTED_EDGE('',*,*,#9317,.T.) ;
#13623 = ORIENTED_EDGE('',*,*,#9313,.T.) ;
#13624 = ORIENTED_EDGE('',*,*,#9309,.T.) ;
#13625 = ORIENTED_EDGE('',*,*,#9305,.T.) ;
#13626 = ORIENTED_EDGE('',*,*,#9301,.T.) ;
#13627 = ORIENTED_EDGE('',*,*,#9297,.T.) ;
#13628 = ORIENTED_EDGE('',*,*,#9293,.T.) ;
#13629 = ORIENTED_EDGE('',*,*,#9289,.T.) ;
#13630 = ORIENTED_EDGE('',*,*,#9285,.T.) ;
#13631 = ORIENTED_EDGE('',*,*,#9281,.T.) ;
#13632 = ORIENTED_EDGE('',*,*,#9277,.T.) ;
#13633 = ORIENTED_EDGE('',*,*,#9273,.T.) ;
#13634 = ORIENTED_EDGE('',*,*,#9269,.T.) ;
#13635 = ORIENTED_EDGE('',*,*,#9265,.T.) ;
#13636 = ORIENTED_EDGE('',*,*,#9261,.T.) ;
#13637 = ORIENTED_EDGE('',*,*,#9260,.T.) ;
#13638 = ORIENTED_EDGE('',*,*,#9256,.T.) ;
#13639 = ORIENTED_EDGE('',*,*,#9252,.T.) ;
#13640 = ORIENTED_EDGE('',*,*,#9248,.T.) ;
#13641 = ORIENTED_EDGE('',*,*,#9244,.T.) ;
#13642 = ORIENTED_EDGE('',*,*,#9243,.T.) ;
#13643 = ORIENTED_EDGE('',*,*,#9239,.T.) ;
#13644 = ORIENTED_EDGE('',*,*,#9235,.T.) ;
#13645 = ORIENTED_EDGE('',*,*,#9231,.T.) ;
#13646 = ORIENTED_EDGE('',*,*,#9227,.T.) ;
#13647 = ORIENTED_EDGE('',*,*,#9223,.T.) ;
#13648 = ORIENTED_EDGE('',*,*,#9219,.T.) ;
#13649 = ORIENTED_EDGE('',*,*,#9215,.T.) ;
#13650 = ORIENTED_EDGE('',*,*,#9211,.T.) ;
#13651 = ORIENTED_EDGE('',*,*,#9611,.F.) ;
#13652 = ORIENTED_EDGE('',*,*,#9124,.F.) ;
#13653 = ORIENTED_EDGE('',*,*,#9612,.T.) ;
#13654 = ORIENTED_EDGE('',*,*,#9262,.T.) ;
#13655 = ORIENTED_EDGE('',*,*,#9553,.F.) ;
#13656 = ORIENTED_EDGE('',*,*,#9451,.T.) ;
#13657 = ORIENTED_EDGE('',*,*,#9613,.T.) ;
#13658 = ORIENTED_EDGE('',*,*,#9384,.F.) ;
#13659 = ORIENTED_EDGE('',*,*,#9121,.T.) ;
#13660 = ORIENTED_EDGE('',*,*,#9614,.F.) ;
#13661 = ORIENTED_EDGE('',*,*,#9263,.T.) ;
#13662 = ORIENTED_EDGE('',*,*,#9612,.F.) ;
#13663 = ORIENTED_EDGE('',*,*,#9123,.T.) ;
#13664 = ORIENTED_EDGE('',*,*,#9385,.T.) ;
#13665 = ORIENTED_EDGE('',*,*,#9613,.F.) ;
#13666 = ORIENTED_EDGE('',*,*,#9450,.T.) ;
#13667 = ORIENTED_EDGE('',*,*,#9615,.F.) ;
#13668 = ORIENTED_EDGE('',*,*,#9386,.T.) ;
#13669 = ORIENTED_EDGE('',*,*,#9120,.F.) ;
#13670 = ORIENTED_EDGE('',*,*,#9387,.F.) ;
#13671 = ORIENTED_EDGE('',*,*,#9615,.T.) ;
#13672 = ORIENTED_EDGE('',*,*,#9449,.T.) ;
#13673 = ORIENTED_EDGE('',*,*,#9554,.F.) ;
#13674 = ORIENTED_EDGE('',*,*,#9264,.T.) ;
#13675 = ORIENTED_EDGE('',*,*,#9614,.T.) ;
#13676 = ORIENTED_EDGE('',*,*,#9118,.F.) ;
#13677 = ORIENTED_EDGE('',*,*,#9616,.T.) ;
#13678 = ORIENTED_EDGE('',*,*,#9266,.T.) ;
#13679 = ORIENTED_EDGE('',*,*,#9555,.F.) ;
#13680 = ORIENTED_EDGE('',*,*,#9534,.T.) ;
#13681 = ORIENTED_EDGE('',*,*,#9617,.T.) ;
#13682 = ORIENTED_EDGE('',*,*,#9388,.F.) ;
#13683 = ORIENTED_EDGE('',*,*,#9115,.T.) ;
#13684 = ORIENTED_EDGE('',*,*,#9618,.F.) ;
#13685 = ORIENTED_EDGE('',*,*,#9267,.T.) ;
#13686 = ORIENTED_EDGE('',*,*,#9616,.F.) ;
#13687 = ORIENTED_EDGE('',*,*,#9117,.T.) ;
#13688 = ORIENTED_EDGE('',*,*,#9389,.T.) ;
#13689 = ORIENTED_EDGE('',*,*,#9617,.F.) ;
#13690 = ORIENTED_EDGE('',*,*,#9533,.T.) ;
#13691 = ORIENTED_EDGE('',*,*,#9619,.F.) ;
#13692 = ORIENTED_EDGE('',*,*,#9390,.T.) ;
#13693 = ORIENTED_EDGE('',*,*,#9114,.F.) ;
#13694 = ORIENTED_EDGE('',*,*,#9391,.F.) ;
#13695 = ORIENTED_EDGE('',*,*,#9619,.T.) ;
#13696 = ORIENTED_EDGE('',*,*,#9535,.T.) ;
#13697 = ORIENTED_EDGE('',*,*,#9556,.F.) ;
#13698 = ORIENTED_EDGE('',*,*,#9268,.T.) ;
#13699 = ORIENTED_EDGE('',*,*,#9618,.T.) ;
#13700 = ORIENTED_EDGE('',*,*,#9112,.F.) ;
#13701 = ORIENTED_EDGE('',*,*,#9620,.T.) ;
#13702 = ORIENTED_EDGE('',*,*,#9270,.T.) ;
#13703 = ORIENTED_EDGE('',*,*,#9557,.F.) ;
#13704 = ORIENTED_EDGE('',*,*,#9495,.T.) ;
#13705 = ORIENTED_EDGE('',*,*,#9621,.T.) ;
#13706 = ORIENTED_EDGE('',*,*,#9392,.F.) ;
#13707 = ORIENTED_EDGE('',*,*,#9109,.T.) ;
#13708 = ORIENTED_EDGE('',*,*,#9622,.F.) ;
#13709 = ORIENTED_EDGE('',*,*,#9271,.T.) ;
#13710 = ORIENTED_EDGE('',*,*,#9620,.F.) ;
#13711 = ORIENTED_EDGE('',*,*,#9111,.T.) ;
#13712 = ORIENTED_EDGE('',*,*,#9393,.T.) ;
#13713 = ORIENTED_EDGE('',*,*,#9621,.F.) ;
#13714 = ORIENTED_EDGE('',*,*,#9494,.T.) ;
#13715 = ORIENTED_EDGE('',*,*,#9623,.F.) ;
#13716 = ORIENTED_EDGE('',*,*,#9394,.T.) ;
#13717 = ORIENTED_EDGE('',*,*,#9108,.F.) ;
#13718 = ORIENTED_EDGE('',*,*,#9395,.F.) ;
#13719 = ORIENTED_EDGE('',*,*,#9623,.T.) ;
#13720 = ORIENTED_EDGE('',*,*,#9496,.T.) ;
#13721 = ORIENTED_EDGE('',*,*,#9558,.F.) ;
#13722 = ORIENTED_EDGE('',*,*,#9272,.T.) ;
#13723 = ORIENTED_EDGE('',*,*,#9622,.T.) ;
#13724 = ORIENTED_EDGE('',*,*,#9106,.F.) ;
#13725 = ORIENTED_EDGE('',*,*,#9624,.T.) ;
#13726 = ORIENTED_EDGE('',*,*,#9274,.T.) ;
#13727 = ORIENTED_EDGE('',*,*,#9559,.F.) ;
#13728 = ORIENTED_EDGE('',*,*,#9531,.T.) ;
#13729 = ORIENTED_EDGE('',*,*,#9625,.T.) ;
#13730 = ORIENTED_EDGE('',*,*,#9396,.F.) ;
#13731 = ORIENTED_EDGE('',*,*,#9103,.T.) ;
#13732 = ORIENTED_EDGE('',*,*,#9626,.F.) ;
#13733 = ORIENTED_EDGE('',*,*,#9275,.T.) ;
#13734 = ORIENTED_EDGE('',*,*,#9624,.F.) ;
#13735 = ORIENTED_EDGE('',*,*,#9105,.T.) ;
#13736 = ORIENTED_EDGE('',*,*,#9397,.T.) ;
#13737 = ORIENTED_EDGE('',*,*,#9625,.F.) ;
#13738 = ORIENTED_EDGE('',*,*,#9530,.T.) ;
#13739 = ORIENTED_EDGE('',*,*,#9627,.F.) ;
#13740 = ORIENTED_EDGE('',*,*,#9398,.T.) ;
#13741 = ORIENTED_EDGE('',*,*,#9102,.F.) ;
#13742 = ORIENTED_EDGE('',*,*,#9399,.F.) ;
#13743 = ORIENTED_EDGE('',*,*,#9627,.T.) ;
#13744 = ORIENTED_EDGE('',*,*,#9532,.T.) ;
#13745 = ORIENTED_EDGE('',*,*,#9560,.F.) ;
#13746 = ORIENTED_EDGE('',*,*,#9276,.T.) ;
#13747 = ORIENTED_EDGE('',*,*,#9626,.T.) ;
#13748 = ORIENTED_EDGE('',*,*,#9100,.F.) ;
#13749 = ORIENTED_EDGE('',*,*,#9628,.T.) ;
#13750 = ORIENTED_EDGE('',*,*,#9278,.T.) ;
#13751 = ORIENTED_EDGE('',*,*,#9561,.F.) ;
#13752 = ORIENTED_EDGE('',*,*,#9498,.T.) ;
#13753 = ORIENTED_EDGE('',*,*,#9629,.T.) ;
#13754 = ORIENTED_EDGE('',*,*,#9400,.F.) ;
#13755 = ORIENTED_EDGE('',*,*,#9097,.T.) ;
#13756 = ORIENTED_EDGE('',*,*,#9630,.F.) ;
#13757 = ORIENTED_EDGE('',*,*,#9279,.T.) ;
#13758 = ORIENTED_EDGE('',*,*,#9628,.F.) ;
#13759 = ORIENTED_EDGE('',*,*,#9099,.T.) ;
#13760 = ORIENTED_EDGE('',*,*,#9401,.T.) ;
#13761 = ORIENTED_EDGE('',*,*,#9629,.F.) ;
#13762 = ORIENTED_EDGE('',*,*,#9497,.T.) ;
#13763 = ORIENTED_EDGE('',*,*,#9631,.F.) ;
#13764 = ORIENTED_EDGE('',*,*,#9402,.T.) ;
#13765 = ORIENTED_EDGE('',*,*,#9096,.F.) ;
#13766 = ORIENTED_EDGE('',*,*,#9403,.F.) ;
#13767 = ORIENTED_EDGE('',*,*,#9631,.T.) ;
#13768 = ORIENTED_EDGE('',*,*,#9499,.T.) ;
#13769 = ORIENTED_EDGE('',*,*,#9562,.F.) ;
#13770 = ORIENTED_EDGE('',*,*,#9280,.T.) ;
#13771 = ORIENTED_EDGE('',*,*,#9630,.T.) ;
#13772 = ORIENTED_EDGE('',*,*,#9094,.F.) ;
#13773 = ORIENTED_EDGE('',*,*,#9632,.T.) ;
#13774 = ORIENTED_EDGE('',*,*,#9282,.T.) ;
#13775 = ORIENTED_EDGE('',*,*,#9563,.F.) ;
#13776 = ORIENTED_EDGE('',*,*,#9528,.T.) ;
#13777 = ORIENTED_EDGE('',*,*,#9633,.T.) ;
#13778 = ORIENTED_EDGE('',*,*,#9404,.F.) ;
#13779 = ORIENTED_EDGE('',*,*,#9091,.T.) ;
#13780 = ORIENTED_EDGE('',*,*,#9634,.F.) ;
#13781 = ORIENTED_EDGE('',*,*,#9283,.T.) ;
#13782 = ORIENTED_EDGE('',*,*,#9632,.F.) ;
#13783 = ORIENTED_EDGE('',*,*,#9093,.T.) ;
#13784 = ORIENTED_EDGE('',*,*,#9405,.T.) ;
#13785 = ORIENTED_EDGE('',*,*,#9633,.F.) ;
#13786 = ORIENTED_EDGE('',*,*,#9527,.T.) ;
#13787 = ORIENTED_EDGE('',*,*,#9635,.F.) ;
#13788 = ORIENTED_EDGE('',*,*,#9406,.T.) ;
#13789 = ORIENTED_EDGE('',*,*,#9090,.F.) ;
#13790 = ORIENTED_EDGE('',*,*,#9407,.F.) ;
#13791 = ORIENTED_EDGE('',*,*,#9635,.T.) ;
#13792 = ORIENTED_EDGE('',*,*,#9529,.T.) ;
#13793 = ORIENTED_EDGE('',*,*,#9564,.F.) ;
#13794 = ORIENTED_EDGE('',*,*,#9284,.T.) ;
#13795 = ORIENTED_EDGE('',*,*,#9634,.T.) ;
#13796 = ORIENTED_EDGE('',*,*,#9088,.F.) ;
#13797 = ORIENTED_EDGE('',*,*,#9636,.T.) ;
#13798 = ORIENTED_EDGE('',*,*,#9286,.T.) ;
#13799 = ORIENTED_EDGE('',*,*,#9565,.F.) ;
#13800 = ORIENTED_EDGE('',*,*,#9501,.T.) ;
#13801 = ORIENTED_EDGE('',*,*,#9637,.T.) ;
#13802 = ORIENTED_EDGE('',*,*,#9408,.F.) ;
#13803 = ORIENTED_EDGE('',*,*,#9085,.T.) ;
#13804 = ORIENTED_EDGE('',*,*,#9638,.F.) ;
#13805 = ORIENTED_EDGE('',*,*,#9287,.T.) ;
#13806 = ORIENTED_EDGE('',*,*,#9636,.F.) ;
#13807 = ORIENTED_EDGE('',*,*,#9087,.T.) ;
#13808 = ORIENTED_EDGE('',*,*,#9409,.T.) ;
#13809 = ORIENTED_EDGE('',*,*,#9637,.F.) ;
#13810 = ORIENTED_EDGE('',*,*,#9500,.T.) ;
#13811 = ORIENTED_EDGE('',*,*,#9639,.F.) ;
#13812 = ORIENTED_EDGE('',*,*,#9410,.T.) ;
#13813 = ORIENTED_EDGE('',*,*,#9084,.F.) ;
#13814 = ORIENTED_EDGE('',*,*,#9411,.F.) ;
#13815 = ORIENTED_EDGE('',*,*,#9639,.T.) ;
#13816 = ORIENTED_EDGE('',*,*,#9502,.T.) ;
#13817 = ORIENTED_EDGE('',*,*,#9566,.F.) ;
#13818 = ORIENTED_EDGE('',*,*,#9288,.T.) ;
#13819 = ORIENTED_EDGE('',*,*,#9638,.T.) ;
#13820 = ORIENTED_EDGE('',*,*,#9082,.F.) ;
#13821 = ORIENTED_EDGE('',*,*,#9640,.T.) ;
#13822 = ORIENTED_EDGE('',*,*,#9290,.T.) ;
#13823 = ORIENTED_EDGE('',*,*,#9567,.F.) ;
#13824 = ORIENTED_EDGE('',*,*,#9525,.T.) ;
#13825 = ORIENTED_EDGE('',*,*,#9641,.T.) ;
#13826 = ORIENTED_EDGE('',*,*,#9412,.F.) ;
#13827 = ORIENTED_EDGE('',*,*,#9079,.T.) ;
#13828 = ORIENTED_EDGE('',*,*,#9642,.F.) ;
#13829 = ORIENTED_EDGE('',*,*,#9291,.T.) ;
#13830 = ORIENTED_EDGE('',*,*,#9640,.F.) ;
#13831 = ORIENTED_EDGE('',*,*,#9081,.T.) ;
#13832 = ORIENTED_EDGE('',*,*,#9413,.T.) ;
#13833 = ORIENTED_EDGE('',*,*,#9641,.F.) ;
#13834 = ORIENTED_EDGE('',*,*,#9524,.T.) ;
#13835 = ORIENTED_EDGE('',*,*,#9643,.F.) ;
#13836 = ORIENTED_EDGE('',*,*,#9414,.T.) ;
#13837 = ORIENTED_EDGE('',*,*,#9078,.F.) ;
#13838 = ORIENTED_EDGE('',*,*,#9415,.F.) ;
#13839 = ORIENTED_EDGE('',*,*,#9643,.T.) ;
#13840 = ORIENTED_EDGE('',*,*,#9526,.T.) ;
#13841 = ORIENTED_EDGE('',*,*,#9568,.F.) ;
#13842 = ORIENTED_EDGE('',*,*,#9292,.T.) ;
#13843 = ORIENTED_EDGE('',*,*,#9642,.T.) ;
#13844 = ORIENTED_EDGE('',*,*,#9076,.F.) ;
#13845 = ORIENTED_EDGE('',*,*,#9644,.T.) ;
#13846 = ORIENTED_EDGE('',*,*,#9294,.T.) ;
#13847 = ORIENTED_EDGE('',*,*,#9569,.F.) ;
#13848 = ORIENTED_EDGE('',*,*,#9504,.T.) ;
#13849 = ORIENTED_EDGE('',*,*,#9645,.T.) ;
#13850 = ORIENTED_EDGE('',*,*,#9416,.F.) ;
#13851 = ORIENTED_EDGE('',*,*,#9075,.T.) ;
#13852 = ORIENTED_EDGE('',*,*,#9417,.T.) ;
#13853 = ORIENTED_EDGE('',*,*,#9645,.F.) ;
#13854 = ORIENTED_EDGE('',*,*,#9503,.T.) ;
#13855 = ORIENTED_EDGE('',*,*,#9646,.F.) ;
#13856 = ORIENTED_EDGE('',*,*,#9418,.T.) ;
#13857 = ORIENTED_EDGE('',*,*,#9073,.T.) ;
#13858 = ORIENTED_EDGE('',*,*,#9647,.F.) ;
#13859 = ORIENTED_EDGE('',*,*,#9295,.T.) ;
#13860 = ORIENTED_EDGE('',*,*,#9644,.F.) ;
#13861 = ORIENTED_EDGE('',*,*,#9072,.F.) ;
#13862 = ORIENTED_EDGE('',*,*,#9419,.F.) ;
#13863 = ORIENTED_EDGE('',*,*,#9646,.T.) ;
#13864 = ORIENTED_EDGE('',*,*,#9505,.T.) ;
#13865 = ORIENTED_EDGE('',*,*,#9570,.F.) ;
#13866 = ORIENTED_EDGE('',*,*,#9296,.T.) ;
#13867 = ORIENTED_EDGE('',*,*,#9647,.T.) ;
#13868 = ORIENTED_EDGE('',*,*,#9070,.F.) ;
#13869 = ORIENTED_EDGE('',*,*,#9648,.T.) ;
#13870 = ORIENTED_EDGE('',*,*,#9298,.T.) ;
#13871 = ORIENTED_EDGE('',*,*,#9571,.F.) ;
#13872 = ORIENTED_EDGE('',*,*,#9522,.T.) ;
#13873 = ORIENTED_EDGE('',*,*,#9649,.T.) ;
#13874 = ORIENTED_EDGE('',*,*,#9420,.F.) ;
#13875 = ORIENTED_EDGE('',*,*,#9069,.T.) ;
#13876 = ORIENTED_EDGE('',*,*,#9421,.T.) ;
#13877 = ORIENTED_EDGE('',*,*,#9649,.F.) ;
#13878 = ORIENTED_EDGE('',*,*,#9521,.T.) ;
#13879 = ORIENTED_EDGE('',*,*,#9650,.F.) ;
#13880 = ORIENTED_EDGE('',*,*,#9422,.T.) ;
#13881 = ORIENTED_EDGE('',*,*,#9067,.T.) ;
#13882 = ORIENTED_EDGE('',*,*,#9651,.F.) ;
#13883 = ORIENTED_EDGE('',*,*,#9299,.T.) ;
#13884 = ORIENTED_EDGE('',*,*,#9648,.F.) ;
#13885 = ORIENTED_EDGE('',*,*,#9066,.F.) ;
#13886 = ORIENTED_EDGE('',*,*,#9423,.F.) ;
#13887 = ORIENTED_EDGE('',*,*,#9650,.T.) ;
#13888 = ORIENTED_EDGE('',*,*,#9523,.T.) ;
#13889 = ORIENTED_EDGE('',*,*,#9572,.F.) ;
#13890 = ORIENTED_EDGE('',*,*,#9300,.T.) ;
#13891 = ORIENTED_EDGE('',*,*,#9651,.T.) ;
#13892 = ORIENTED_EDGE('',*,*,#9064,.F.) ;
#13893 = ORIENTED_EDGE('',*,*,#9652,.T.) ;
#13894 = ORIENTED_EDGE('',*,*,#9302,.T.) ;
#13895 = ORIENTED_EDGE('',*,*,#9573,.F.) ;
#13896 = ORIENTED_EDGE('',*,*,#9507,.T.) ;
#13897 = ORIENTED_EDGE('',*,*,#9653,.T.) ;
#13898 = ORIENTED_EDGE('',*,*,#9424,.F.) ;
#13899 = ORIENTED_EDGE('',*,*,#9063,.T.) ;
#13900 = ORIENTED_EDGE('',*,*,#9425,.T.) ;
#13901 = ORIENTED_EDGE('',*,*,#9653,.F.) ;
#13902 = ORIENTED_EDGE('',*,*,#9506,.T.) ;
#13903 = ORIENTED_EDGE('',*,*,#9654,.F.) ;
#13904 = ORIENTED_EDGE('',*,*,#9426,.T.) ;
#13905 = ORIENTED_EDGE('',*,*,#9061,.T.) ;
#13906 = ORIENTED_EDGE('',*,*,#9655,.F.) ;
#13907 = ORIENTED_EDGE('',*,*,#9303,.T.) ;
#13908 = ORIENTED_EDGE('',*,*,#9652,.F.) ;
#13909 = ORIENTED_EDGE('',*,*,#9060,.F.) ;
#13910 = ORIENTED_EDGE('',*,*,#9427,.F.) ;
#13911 = ORIENTED_EDGE('',*,*,#9654,.T.) ;
#13912 = ORIENTED_EDGE('',*,*,#9508,.T.) ;
#13913 = ORIENTED_EDGE('',*,*,#9574,.F.) ;
#13914 = ORIENTED_EDGE('',*,*,#9304,.T.) ;
#13915 = ORIENTED_EDGE('',*,*,#9655,.T.) ;
#13916 = ORIENTED_EDGE('',*,*,#9058,.F.) ;
#13917 = ORIENTED_EDGE('',*,*,#9656,.T.) ;
#13918 = ORIENTED_EDGE('',*,*,#9306,.T.) ;
#13919 = ORIENTED_EDGE('',*,*,#9575,.F.) ;
#13920 = ORIENTED_EDGE('',*,*,#9519,.T.) ;
#13921 = ORIENTED_EDGE('',*,*,#9657,.T.) ;
#13922 = ORIENTED_EDGE('',*,*,#9428,.F.) ;
#13923 = ORIENTED_EDGE('',*,*,#9057,.T.) ;
#13924 = ORIENTED_EDGE('',*,*,#9429,.T.) ;
#13925 = ORIENTED_EDGE('',*,*,#9657,.F.) ;
#13926 = ORIENTED_EDGE('',*,*,#9518,.T.) ;
#13927 = ORIENTED_EDGE('',*,*,#9658,.F.) ;
#13928 = ORIENTED_EDGE('',*,*,#9430,.T.) ;
#13929 = ORIENTED_EDGE('',*,*,#9055,.T.) ;
#13930 = ORIENTED_EDGE('',*,*,#9659,.F.) ;
#13931 = ORIENTED_EDGE('',*,*,#9307,.T.) ;
#13932 = ORIENTED_EDGE('',*,*,#9656,.F.) ;
#13933 = ORIENTED_EDGE('',*,*,#9054,.F.) ;
#13934 = ORIENTED_EDGE('',*,*,#9431,.F.) ;
#13935 = ORIENTED_EDGE('',*,*,#9658,.T.) ;
#13936 = ORIENTED_EDGE('',*,*,#9520,.T.) ;
#13937 = ORIENTED_EDGE('',*,*,#9576,.F.) ;
#13938 = ORIENTED_EDGE('',*,*,#9308,.T.) ;
#13939 = ORIENTED_EDGE('',*,*,#9659,.T.) ;
#13940 = ORIENTED_EDGE('',*,*,#9052,.F.) ;
#13941 = ORIENTED_EDGE('',*,*,#9660,.T.) ;
#13942 = ORIENTED_EDGE('',*,*,#9310,.T.) ;
#13943 = ORIENTED_EDGE('',*,*,#9577,.F.) ;
#13944 = ORIENTED_EDGE('',*,*,#9510,.T.) ;
#13945 = ORIENTED_EDGE('',*,*,#9661,.T.) ;
#13946 = ORIENTED_EDGE('',*,*,#9432,.F.) ;
#13947 = ORIENTED_EDGE('',*,*,#9051,.T.) ;
#13948 = ORIENTED_EDGE('',*,*,#9433,.T.) ;
#13949 = ORIENTED_EDGE('',*,*,#9661,.F.) ;
#13950 = ORIENTED_EDGE('',*,*,#9509,.T.) ;
#13951 = ORIENTED_EDGE('',*,*,#9662,.F.) ;
#13952 = ORIENTED_EDGE('',*,*,#9434,.T.) ;
#13953 = ORIENTED_EDGE('',*,*,#9049,.T.) ;
#13954 = ORIENTED_EDGE('',*,*,#9663,.F.) ;
#13955 = ORIENTED_EDGE('',*,*,#9311,.T.) ;
#13956 = ORIENTED_EDGE('',*,*,#9660,.F.) ;
#13957 = ORIENTED_EDGE('',*,*,#9048,.F.) ;
#13958 = ORIENTED_EDGE('',*,*,#9435,.F.) ;
#13959 = ORIENTED_EDGE('',*,*,#9662,.T.) ;
#13960 = ORIENTED_EDGE('',*,*,#9511,.T.) ;
#13961 = ORIENTED_EDGE('',*,*,#9578,.F.) ;
#13962 = ORIENTED_EDGE('',*,*,#9312,.T.) ;
#13963 = ORIENTED_EDGE('',*,*,#9663,.T.) ;
#13964 = ORIENTED_EDGE('',*,*,#9046,.F.) ;
#13965 = ORIENTED_EDGE('',*,*,#9664,.T.) ;
#13966 = ORIENTED_EDGE('',*,*,#9314,.T.) ;
#13967 = ORIENTED_EDGE('',*,*,#9579,.F.) ;
#13968 = ORIENTED_EDGE('',*,*,#9516,.T.) ;
#13969 = ORIENTED_EDGE('',*,*,#9665,.T.) ;
#13970 = ORIENTED_EDGE('',*,*,#9436,.F.) ;
#13971 = ORIENTED_EDGE('',*,*,#9045,.T.) ;
#13972 = ORIENTED_EDGE('',*,*,#9437,.T.) ;
#13973 = ORIENTED_EDGE('',*,*,#9665,.F.) ;
#13974 = ORIENTED_EDGE('',*,*,#9515,.T.) ;
#13975 = ORIENTED_EDGE('',*,*,#9666,.F.) ;
#13976 = ORIENTED_EDGE('',*,*,#9438,.T.) ;
#13977 = ORIENTED_EDGE('',*,*,#9043,.T.) ;
#13978 = ORIENTED_EDGE('',*,*,#9667,.F.) ;
#13979 = ORIENTED_EDGE('',*,*,#9315,.T.) ;
#13980 = ORIENTED_EDGE('',*,*,#9664,.F.) ;
#13981 = ORIENTED_EDGE('',*,*,#9042,.F.) ;
#13982 = ORIENTED_EDGE('',*,*,#9439,.F.) ;
#13983 = ORIENTED_EDGE('',*,*,#9666,.T.) ;
#13984 = ORIENTED_EDGE('',*,*,#9517,.T.) ;
#13985 = ORIENTED_EDGE('',*,*,#9580,.F.) ;
#13986 = ORIENTED_EDGE('',*,*,#9316,.T.) ;
#13987 = ORIENTED_EDGE('',*,*,#9667,.T.) ;
#13988 = ORIENTED_EDGE('',*,*,#9040,.F.) ;
#13989 = ORIENTED_EDGE('',*,*,#9668,.T.) ;
#13990 = ORIENTED_EDGE('',*,*,#9318,.T.) ;
#13991 = ORIENTED_EDGE('',*,*,#9581,.F.) ;
#13992 = ORIENTED_EDGE('',*,*,#9513,.T.) ;
#13993 = ORIENTED_EDGE('',*,*,#9669,.T.) ;
#13994 = ORIENTED_EDGE('',*,*,#9440,.F.) ;
#13995 = ORIENTED_EDGE('',*,*,#9039,.T.) ;
#13996 = ORIENTED_EDGE('',*,*,#9441,.T.) ;
#13997 = ORIENTED_EDGE('',*,*,#9669,.F.) ;
#13998 = ORIENTED_EDGE('',*,*,#9512,.T.) ;
#13999 = ORIENTED_EDGE('',*,*,#9670,.F.) ;
#14000 = ORIENTED_EDGE('',*,*,#9442,.T.) ;
#14001 = ORIENTED_EDGE('',*,*,#9037,.T.) ;
#14002 = ORIENTED_EDGE('',*,*,#9671,.F.) ;
#14003 = ORIENTED_EDGE('',*,*,#9319,.T.) ;
#14004 = ORIENTED_EDGE('',*,*,#9668,.F.) ;
#14005 = ORIENTED_EDGE('',*,*,#9036,.F.) ;
#14006 = ORIENTED_EDGE('',*,*,#9443,.F.) ;
#14007 = ORIENTED_EDGE('',*,*,#9670,.T.) ;
#14008 = ORIENTED_EDGE('',*,*,#9514,.T.) ;
#14009 = ORIENTED_EDGE('',*,*,#9582,.F.) ;
#14010 = ORIENTED_EDGE('',*,*,#9320,.T.) ;
#14011 = ORIENTED_EDGE('',*,*,#9671,.T.) ;
#14012 = ORIENTED_EDGE('',*,*,#9208,.F.) ;
#14013 = ORIENTED_EDGE('',*,*,#9672,.T.) ;
#14014 = ORIENTED_EDGE('',*,*,#9212,.T.) ;
#14015 = ORIENTED_EDGE('',*,*,#9583,.F.) ;
#14016 = ORIENTED_EDGE('',*,*,#9471,.T.) ;
#14017 = ORIENTED_EDGE('',*,*,#9673,.T.) ;
#14018 = ORIENTED_EDGE('',*,*,#9328,.F.) ;
#14019 = ORIENTED_EDGE('',*,*,#9207,.T.) ;
#14020 = ORIENTED_EDGE('',*,*,#9329,.T.) ;
#14021 = ORIENTED_EDGE('',*,*,#9673,.F.) ;
#14022 = ORIENTED_EDGE('',*,*,#9470,.T.) ;
#14023 = ORIENTED_EDGE('',*,*,#9674,.F.) ;
#14024 = ORIENTED_EDGE('',*,*,#9330,.T.) ;
#14025 = ORIENTED_EDGE('',*,*,#9205,.T.) ;
#14026 = ORIENTED_EDGE('',*,*,#9675,.F.) ;
#14027 = ORIENTED_EDGE('',*,*,#9213,.T.) ;
#14028 = ORIENTED_EDGE('',*,*,#9672,.F.) ;
#14029 = ORIENTED_EDGE('',*,*,#9204,.F.) ;
#14030 = ORIENTED_EDGE('',*,*,#9331,.F.) ;
#14031 = ORIENTED_EDGE('',*,*,#9674,.T.) ;
#14032 = ORIENTED_EDGE('',*,*,#9472,.T.) ;
#14033 = ORIENTED_EDGE('',*,*,#9584,.F.) ;
#14034 = ORIENTED_EDGE('',*,*,#9214,.T.) ;
#14035 = ORIENTED_EDGE('',*,*,#9675,.T.) ;
#14036 = ORIENTED_EDGE('',*,*,#9202,.F.) ;
#14037 = ORIENTED_EDGE('',*,*,#9676,.T.) ;
#14038 = ORIENTED_EDGE('',*,*,#9216,.T.) ;
#14039 = ORIENTED_EDGE('',*,*,#9585,.F.) ;
#14040 = ORIENTED_EDGE('',*,*,#9474,.T.) ;
#14041 = ORIENTED_EDGE('',*,*,#9677,.T.) ;
#14042 = ORIENTED_EDGE('',*,*,#9332,.F.) ;
#14043 = ORIENTED_EDGE('',*,*,#9201,.T.) ;
#14044 = ORIENTED_EDGE('',*,*,#9333,.T.) ;
#14045 = ORIENTED_EDGE('',*,*,#9677,.F.) ;
#14046 = ORIENTED_EDGE('',*,*,#9473,.T.) ;
#14047 = ORIENTED_EDGE('',*,*,#9678,.F.) ;
#14048 = ORIENTED_EDGE('',*,*,#9334,.T.) ;
#14049 = ORIENTED_EDGE('',*,*,#9199,.T.) ;
#14050 = ORIENTED_EDGE('',*,*,#9679,.F.) ;
#14051 = ORIENTED_EDGE('',*,*,#9217,.T.) ;
#14052 = ORIENTED_EDGE('',*,*,#9676,.F.) ;
#14053 = ORIENTED_EDGE('',*,*,#9198,.F.) ;
#14054 = ORIENTED_EDGE('',*,*,#9335,.F.) ;
#14055 = ORIENTED_EDGE('',*,*,#9678,.T.) ;
#14056 = ORIENTED_EDGE('',*,*,#9475,.T.) ;
#14057 = ORIENTED_EDGE('',*,*,#9586,.F.) ;
#14058 = ORIENTED_EDGE('',*,*,#9218,.T.) ;
#14059 = ORIENTED_EDGE('',*,*,#9679,.T.) ;
#14060 = ORIENTED_EDGE('',*,*,#9196,.F.) ;
#14061 = ORIENTED_EDGE('',*,*,#9680,.T.) ;
#14062 = ORIENTED_EDGE('',*,*,#9220,.T.) ;
#14063 = ORIENTED_EDGE('',*,*,#9587,.F.) ;
#14064 = ORIENTED_EDGE('',*,*,#9468,.T.) ;
#14065 = ORIENTED_EDGE('',*,*,#9681,.T.) ;
#14066 = ORIENTED_EDGE('',*,*,#9336,.F.) ;
#14067 = ORIENTED_EDGE('',*,*,#9195,.T.) ;
#14068 = ORIENTED_EDGE('',*,*,#9337,.T.) ;
#14069 = ORIENTED_EDGE('',*,*,#9681,.F.) ;
#14070 = ORIENTED_EDGE('',*,*,#9467,.T.) ;
#14071 = ORIENTED_EDGE('',*,*,#9682,.F.) ;
#14072 = ORIENTED_EDGE('',*,*,#9338,.T.) ;
#14073 = ORIENTED_EDGE('',*,*,#9193,.T.) ;
#14074 = ORIENTED_EDGE('',*,*,#9683,.F.) ;
#14075 = ORIENTED_EDGE('',*,*,#9221,.T.) ;
#14076 = ORIENTED_EDGE('',*,*,#9680,.F.) ;
#14077 = ORIENTED_EDGE('',*,*,#9192,.F.) ;
#14078 = ORIENTED_EDGE('',*,*,#9339,.F.) ;
#14079 = ORIENTED_EDGE('',*,*,#9682,.T.) ;
#14080 = ORIENTED_EDGE('',*,*,#9469,.T.) ;
#14081 = ORIENTED_EDGE('',*,*,#9588,.F.) ;
#14082 = ORIENTED_EDGE('',*,*,#9222,.T.) ;
#14083 = ORIENTED_EDGE('',*,*,#9683,.T.) ;
#14084 = ORIENTED_EDGE('',*,*,#9190,.F.) ;
#14085 = ORIENTED_EDGE('',*,*,#9684,.T.) ;
#14086 = ORIENTED_EDGE('',*,*,#9224,.T.) ;
#14087 = ORIENTED_EDGE('',*,*,#9589,.F.) ;
#14088 = ORIENTED_EDGE('',*,*,#9477,.T.) ;
#14089 = ORIENTED_EDGE('',*,*,#9685,.T.) ;
#14090 = ORIENTED_EDGE('',*,*,#9340,.F.) ;
#14091 = ORIENTED_EDGE('',*,*,#9189,.T.) ;
#14092 = ORIENTED_EDGE('',*,*,#9341,.T.) ;
#14093 = ORIENTED_EDGE('',*,*,#9685,.F.) ;
#14094 = ORIENTED_EDGE('',*,*,#9476,.T.) ;
#14095 = ORIENTED_EDGE('',*,*,#9686,.F.) ;
#14096 = ORIENTED_EDGE('',*,*,#9342,.T.) ;
#14097 = ORIENTED_EDGE('',*,*,#9187,.T.) ;
#14098 = ORIENTED_EDGE('',*,*,#9687,.F.) ;
#14099 = ORIENTED_EDGE('',*,*,#9225,.T.) ;
#14100 = ORIENTED_EDGE('',*,*,#9684,.F.) ;
#14101 = ORIENTED_EDGE('',*,*,#9186,.F.) ;
#14102 = ORIENTED_EDGE('',*,*,#9343,.F.) ;
#14103 = ORIENTED_EDGE('',*,*,#9686,.T.) ;
#14104 = ORIENTED_EDGE('',*,*,#9478,.T.) ;
#14105 = ORIENTED_EDGE('',*,*,#9590,.F.) ;
#14106 = ORIENTED_EDGE('',*,*,#9226,.T.) ;
#14107 = ORIENTED_EDGE('',*,*,#9687,.T.) ;
#14108 = ORIENTED_EDGE('',*,*,#9184,.F.) ;
#14109 = ORIENTED_EDGE('',*,*,#9688,.T.) ;
#14110 = ORIENTED_EDGE('',*,*,#9228,.T.) ;
#14111 = ORIENTED_EDGE('',*,*,#9591,.F.) ;
#14112 = ORIENTED_EDGE('',*,*,#9465,.T.) ;
#14113 = ORIENTED_EDGE('',*,*,#9689,.T.) ;
#14114 = ORIENTED_EDGE('',*,*,#9344,.F.) ;
#14115 = ORIENTED_EDGE('',*,*,#9183,.T.) ;
#14116 = ORIENTED_EDGE('',*,*,#9345,.T.) ;
#14117 = ORIENTED_EDGE('',*,*,#9689,.F.) ;
#14118 = ORIENTED_EDGE('',*,*,#9464,.T.) ;
#14119 = ORIENTED_EDGE('',*,*,#9690,.F.) ;
#14120 = ORIENTED_EDGE('',*,*,#9346,.T.) ;
#14121 = ORIENTED_EDGE('',*,*,#9181,.T.) ;
#14122 = ORIENTED_EDGE('',*,*,#9691,.F.) ;
#14123 = ORIENTED_EDGE('',*,*,#9229,.T.) ;
#14124 = ORIENTED_EDGE('',*,*,#9688,.F.) ;
#14125 = ORIENTED_EDGE('',*,*,#9180,.F.) ;
#14126 = ORIENTED_EDGE('',*,*,#9347,.F.) ;
#14127 = ORIENTED_EDGE('',*,*,#9690,.T.) ;
#14128 = ORIENTED_EDGE('',*,*,#9466,.T.) ;
#14129 = ORIENTED_EDGE('',*,*,#9592,.F.) ;
#14130 = ORIENTED_EDGE('',*,*,#9230,.T.) ;
#14131 = ORIENTED_EDGE('',*,*,#9691,.T.) ;
#14132 = ORIENTED_EDGE('',*,*,#9178,.F.) ;
#14133 = ORIENTED_EDGE('',*,*,#9692,.T.) ;
#14134 = ORIENTED_EDGE('',*,*,#9232,.T.) ;
#14135 = ORIENTED_EDGE('',*,*,#9593,.F.) ;
#14136 = ORIENTED_EDGE('',*,*,#9480,.T.) ;
#14137 = ORIENTED_EDGE('',*,*,#9693,.T.) ;
#14138 = ORIENTED_EDGE('',*,*,#9348,.F.) ;
#14139 = ORIENTED_EDGE('',*,*,#9177,.T.) ;
#14140 = ORIENTED_EDGE('',*,*,#9349,.T.) ;
#14141 = ORIENTED_EDGE('',*,*,#9693,.F.) ;
#14142 = ORIENTED_EDGE('',*,*,#9479,.T.) ;
#14143 = ORIENTED_EDGE('',*,*,#9694,.F.) ;
#14144 = ORIENTED_EDGE('',*,*,#9350,.T.) ;
#14145 = ORIENTED_EDGE('',*,*,#9175,.T.) ;
#14146 = ORIENTED_EDGE('',*,*,#9695,.F.) ;
#14147 = ORIENTED_EDGE('',*,*,#9233,.T.) ;
#14148 = ORIENTED_EDGE('',*,*,#9692,.F.) ;
#14149 = ORIENTED_EDGE('',*,*,#9174,.F.) ;
#14150 = ORIENTED_EDGE('',*,*,#9351,.F.) ;
#14151 = ORIENTED_EDGE('',*,*,#9694,.T.) ;
#14152 = ORIENTED_EDGE('',*,*,#9481,.T.) ;
#14153 = ORIENTED_EDGE('',*,*,#9594,.F.) ;
#14154 = ORIENTED_EDGE('',*,*,#9234,.T.) ;
#14155 = ORIENTED_EDGE('',*,*,#9695,.T.) ;
#14156 = ORIENTED_EDGE('',*,*,#9172,.F.) ;
#14157 = ORIENTED_EDGE('',*,*,#9696,.T.) ;
#14158 = ORIENTED_EDGE('',*,*,#9236,.T.) ;
#14159 = ORIENTED_EDGE('',*,*,#9595,.F.) ;
#14160 = ORIENTED_EDGE('',*,*,#9462,.T.) ;
#14161 = ORIENTED_EDGE('',*,*,#9697,.T.) ;
#14162 = ORIENTED_EDGE('',*,*,#9352,.F.) ;
#14163 = ORIENTED_EDGE('',*,*,#9171,.T.) ;
#14164 = ORIENTED_EDGE('',*,*,#9353,.T.) ;
#14165 = ORIENTED_EDGE('',*,*,#9697,.F.) ;
#14166 = ORIENTED_EDGE('',*,*,#9461,.T.) ;
#14167 = ORIENTED_EDGE('',*,*,#9698,.F.) ;
#14168 = ORIENTED_EDGE('',*,*,#9354,.T.) ;
#14169 = ORIENTED_EDGE('',*,*,#9169,.T.) ;
#14170 = ORIENTED_EDGE('',*,*,#9699,.F.) ;
#14171 = ORIENTED_EDGE('',*,*,#9237,.T.) ;
#14172 = ORIENTED_EDGE('',*,*,#9696,.F.) ;
#14173 = ORIENTED_EDGE('',*,*,#9168,.F.) ;
#14174 = ORIENTED_EDGE('',*,*,#9355,.F.) ;
#14175 = ORIENTED_EDGE('',*,*,#9698,.T.) ;
#14176 = ORIENTED_EDGE('',*,*,#9463,.T.) ;
#14177 = ORIENTED_EDGE('',*,*,#9596,.F.) ;
#14178 = ORIENTED_EDGE('',*,*,#9238,.T.) ;
#14179 = ORIENTED_EDGE('',*,*,#9699,.T.) ;
#14180 = ORIENTED_EDGE('',*,*,#9166,.F.) ;
#14181 = ORIENTED_EDGE('',*,*,#9700,.T.) ;
#14182 = ORIENTED_EDGE('',*,*,#9240,.T.) ;
#14183 = ORIENTED_EDGE('',*,*,#9597,.F.) ;
#14184 = ORIENTED_EDGE('',*,*,#9483,.T.) ;
#14185 = ORIENTED_EDGE('',*,*,#9701,.T.) ;
#14186 = ORIENTED_EDGE('',*,*,#9356,.F.) ;
#14187 = ORIENTED_EDGE('',*,*,#9163,.T.) ;
#14188 = ORIENTED_EDGE('',*,*,#9702,.F.) ;
#14189 = ORIENTED_EDGE('',*,*,#9241,.T.) ;
#14190 = ORIENTED_EDGE('',*,*,#9700,.F.) ;
#14191 = ORIENTED_EDGE('',*,*,#9165,.T.) ;
#14192 = ORIENTED_EDGE('',*,*,#9357,.T.) ;
#14193 = ORIENTED_EDGE('',*,*,#9701,.F.) ;
#14194 = ORIENTED_EDGE('',*,*,#9482,.T.) ;
#14195 = ORIENTED_EDGE('',*,*,#9703,.F.) ;
#14196 = ORIENTED_EDGE('',*,*,#9358,.T.) ;
#14197 = ORIENTED_EDGE('',*,*,#9162,.F.) ;
#14198 = ORIENTED_EDGE('',*,*,#9359,.F.) ;
#14199 = ORIENTED_EDGE('',*,*,#9703,.T.) ;
#14200 = ORIENTED_EDGE('',*,*,#9484,.T.) ;
#14201 = ORIENTED_EDGE('',*,*,#9598,.F.) ;
#14202 = ORIENTED_EDGE('',*,*,#9242,.T.) ;
#14203 = ORIENTED_EDGE('',*,*,#9702,.T.) ;
#14204 = ORIENTED_EDGE('',*,*,#9160,.F.) ;
#14205 = ORIENTED_EDGE('',*,*,#9704,.T.) ;
#14206 = ORIENTED_EDGE('',*,*,#9322,.T.) ;
#14207 = ORIENTED_EDGE('',*,*,#9599,.F.) ;
#14208 = ORIENTED_EDGE('',*,*,#9459,.T.) ;
#14209 = ORIENTED_EDGE('',*,*,#9705,.T.) ;
#14210 = ORIENTED_EDGE('',*,*,#9360,.F.) ;
#14211 = ORIENTED_EDGE('',*,*,#9157,.T.) ;
#14212 = ORIENTED_EDGE('',*,*,#9706,.F.) ;
#14213 = ORIENTED_EDGE('',*,*,#9323,.T.) ;
#14214 = ORIENTED_EDGE('',*,*,#9704,.F.) ;
#14215 = ORIENTED_EDGE('',*,*,#9159,.T.) ;
#14216 = ORIENTED_EDGE('',*,*,#9361,.T.) ;
#14217 = ORIENTED_EDGE('',*,*,#9705,.F.) ;
#14218 = ORIENTED_EDGE('',*,*,#9458,.T.) ;
#14219 = ORIENTED_EDGE('',*,*,#9707,.F.) ;
#14220 = ORIENTED_EDGE('',*,*,#9362,.T.) ;
#14221 = ORIENTED_EDGE('',*,*,#9156,.F.) ;
#14222 = ORIENTED_EDGE('',*,*,#9363,.F.) ;
#14223 = ORIENTED_EDGE('',*,*,#9707,.T.) ;
#14224 = ORIENTED_EDGE('',*,*,#9460,.T.) ;
#14225 = ORIENTED_EDGE('',*,*,#9600,.F.) ;
#14226 = ORIENTED_EDGE('',*,*,#9324,.T.) ;
#14227 = ORIENTED_EDGE('',*,*,#9706,.T.) ;
#14228 = ORIENTED_EDGE('',*,*,#9154,.F.) ;
#14229 = ORIENTED_EDGE('',*,*,#9708,.T.) ;
#14230 = ORIENTED_EDGE('',*,*,#9245,.T.) ;
#14231 = ORIENTED_EDGE('',*,*,#9601,.F.) ;
#14232 = ORIENTED_EDGE('',*,*,#9486,.T.) ;
#14233 = ORIENTED_EDGE('',*,*,#9709,.T.) ;
#14234 = ORIENTED_EDGE('',*,*,#9364,.F.) ;
#14235 = ORIENTED_EDGE('',*,*,#9151,.T.) ;
#14236 = ORIENTED_EDGE('',*,*,#9710,.F.) ;
#14237 = ORIENTED_EDGE('',*,*,#9246,.T.) ;
#14238 = ORIENTED_EDGE('',*,*,#9708,.F.) ;
#14239 = ORIENTED_EDGE('',*,*,#9153,.T.) ;
#14240 = ORIENTED_EDGE('',*,*,#9365,.T.) ;
#14241 = ORIENTED_EDGE('',*,*,#9709,.F.) ;
#14242 = ORIENTED_EDGE('',*,*,#9485,.T.) ;
#14243 = ORIENTED_EDGE('',*,*,#9711,.F.) ;
#14244 = ORIENTED_EDGE('',*,*,#9366,.T.) ;
#14245 = ORIENTED_EDGE('',*,*,#9150,.F.) ;
#14246 = ORIENTED_EDGE('',*,*,#9367,.F.) ;
#14247 = ORIENTED_EDGE('',*,*,#9711,.T.) ;
#14248 = ORIENTED_EDGE('',*,*,#9487,.T.) ;
#14249 = ORIENTED_EDGE('',*,*,#9602,.F.) ;
#14250 = ORIENTED_EDGE('',*,*,#9247,.T.) ;
#14251 = ORIENTED_EDGE('',*,*,#9710,.T.) ;
#14252 = ORIENTED_EDGE('',*,*,#9148,.F.) ;
#14253 = ORIENTED_EDGE('',*,*,#9712,.T.) ;
#14254 = ORIENTED_EDGE('',*,*,#9249,.T.) ;
#14255 = ORIENTED_EDGE('',*,*,#9603,.F.) ;
#14256 = ORIENTED_EDGE('',*,*,#9456,.T.) ;
#14257 = ORIENTED_EDGE('',*,*,#9713,.T.) ;
#14258 = ORIENTED_EDGE('',*,*,#9368,.F.) ;
#14259 = ORIENTED_EDGE('',*,*,#9145,.T.) ;
#14260 = ORIENTED_EDGE('',*,*,#9714,.F.) ;
#14261 = ORIENTED_EDGE('',*,*,#9250,.T.) ;
#14262 = ORIENTED_EDGE('',*,*,#9712,.F.) ;
#14263 = ORIENTED_EDGE('',*,*,#9147,.T.) ;
#14264 = ORIENTED_EDGE('',*,*,#9369,.T.) ;
#14265 = ORIENTED_EDGE('',*,*,#9713,.F.) ;
#14266 = ORIENTED_EDGE('',*,*,#9455,.T.) ;
#14267 = ORIENTED_EDGE('',*,*,#9715,.F.) ;
#14268 = ORIENTED_EDGE('',*,*,#9370,.T.) ;
#14269 = ORIENTED_EDGE('',*,*,#9144,.F.) ;
#14270 = ORIENTED_EDGE('',*,*,#9371,.F.) ;
#14271 = ORIENTED_EDGE('',*,*,#9715,.T.) ;
#14272 = ORIENTED_EDGE('',*,*,#9457,.T.) ;
#14273 = ORIENTED_EDGE('',*,*,#9604,.F.) ;
#14274 = ORIENTED_EDGE('',*,*,#9251,.T.) ;
#14275 = ORIENTED_EDGE('',*,*,#9714,.T.) ;
#14276 = ORIENTED_EDGE('',*,*,#9142,.F.) ;
#14277 = ORIENTED_EDGE('',*,*,#9716,.T.) ;
#14278 = ORIENTED_EDGE('',*,*,#9253,.T.) ;
#14279 = ORIENTED_EDGE('',*,*,#9605,.F.) ;
#14280 = ORIENTED_EDGE('',*,*,#9489,.T.) ;
#14281 = ORIENTED_EDGE('',*,*,#9717,.T.) ;
#14282 = ORIENTED_EDGE('',*,*,#9372,.F.) ;
#14283 = ORIENTED_EDGE('',*,*,#9139,.T.) ;
#14284 = ORIENTED_EDGE('',*,*,#9718,.F.) ;
#14285 = ORIENTED_EDGE('',*,*,#9254,.T.) ;
#14286 = ORIENTED_EDGE('',*,*,#9716,.F.) ;
#14287 = ORIENTED_EDGE('',*,*,#9141,.T.) ;
#14288 = ORIENTED_EDGE('',*,*,#9373,.T.) ;
#14289 = ORIENTED_EDGE('',*,*,#9717,.F.) ;
#14290 = ORIENTED_EDGE('',*,*,#9488,.T.) ;
#14291 = ORIENTED_EDGE('',*,*,#9719,.F.) ;
#14292 = ORIENTED_EDGE('',*,*,#9374,.T.) ;
#14293 = ORIENTED_EDGE('',*,*,#9138,.F.) ;
#14294 = ORIENTED_EDGE('',*,*,#9375,.F.) ;
#14295 = ORIENTED_EDGE('',*,*,#9719,.T.) ;
#14296 = ORIENTED_EDGE('',*,*,#9490,.T.) ;
#14297 = ORIENTED_EDGE('',*,*,#9606,.F.) ;
#14298 = ORIENTED_EDGE('',*,*,#9255,.T.) ;
#14299 = ORIENTED_EDGE('',*,*,#9718,.T.) ;
#14300 = ORIENTED_EDGE('',*,*,#9136,.F.) ;
#14301 = ORIENTED_EDGE('',*,*,#9720,.T.) ;
#14302 = ORIENTED_EDGE('',*,*,#9257,.T.) ;
#14303 = ORIENTED_EDGE('',*,*,#9607,.F.) ;
#14304 = ORIENTED_EDGE('',*,*,#9453,.T.) ;
#14305 = ORIENTED_EDGE('',*,*,#9721,.T.) ;
#14306 = ORIENTED_EDGE('',*,*,#9376,.F.) ;
#14307 = ORIENTED_EDGE('',*,*,#9133,.T.) ;
#14308 = ORIENTED_EDGE('',*,*,#9722,.F.) ;
#14309 = ORIENTED_EDGE('',*,*,#9258,.T.) ;
#14310 = ORIENTED_EDGE('',*,*,#9720,.F.) ;
#14311 = ORIENTED_EDGE('',*,*,#9135,.T.) ;
#14312 = ORIENTED_EDGE('',*,*,#9377,.T.) ;
#14313 = ORIENTED_EDGE('',*,*,#9721,.F.) ;
#14314 = ORIENTED_EDGE('',*,*,#9452,.T.) ;
#14315 = ORIENTED_EDGE('',*,*,#9723,.F.) ;
#14316 = ORIENTED_EDGE('',*,*,#9378,.T.) ;
#14317 = ORIENTED_EDGE('',*,*,#9132,.F.) ;
#14318 = ORIENTED_EDGE('',*,*,#9379,.F.) ;
#14319 = ORIENTED_EDGE('',*,*,#9723,.T.) ;
#14320 = ORIENTED_EDGE('',*,*,#9454,.T.) ;
#14321 = ORIENTED_EDGE('',*,*,#9608,.F.) ;
#14322 = ORIENTED_EDGE('',*,*,#9259,.T.) ;
#14323 = ORIENTED_EDGE('',*,*,#9722,.T.) ;
#14324 = ORIENTED_EDGE('',*,*,#9130,.F.) ;
#14325 = ORIENTED_EDGE('',*,*,#9724,.T.) ;
#14326 = ORIENTED_EDGE('',*,*,#9325,.T.) ;
#14327 = ORIENTED_EDGE('',*,*,#9609,.F.) ;
#14328 = ORIENTED_EDGE('',*,*,#9492,.T.) ;
#14329 = ORIENTED_EDGE('',*,*,#9725,.T.) ;
#14330 = ORIENTED_EDGE('',*,*,#9380,.F.) ;
#14331 = ORIENTED_EDGE('',*,*,#9127,.T.) ;
#14332 = ORIENTED_EDGE('',*,*,#9726,.F.) ;
#14333 = ORIENTED_EDGE('',*,*,#9326,.T.) ;
#14334 = ORIENTED_EDGE('',*,*,#9724,.F.) ;
#14335 = ORIENTED_EDGE('',*,*,#9129,.T.) ;
#14336 = ORIENTED_EDGE('',*,*,#9381,.T.) ;
#14337 = ORIENTED_EDGE('',*,*,#9725,.F.) ;
#14338 = ORIENTED_EDGE('',*,*,#9491,.T.) ;
#14339 = ORIENTED_EDGE('',*,*,#9727,.F.) ;
#14340 = ORIENTED_EDGE('',*,*,#9382,.T.) ;
#14341 = ORIENTED_EDGE('',*,*,#9126,.F.) ;
#14342 = ORIENTED_EDGE('',*,*,#9383,.F.) ;
#14343 = ORIENTED_EDGE('',*,*,#9727,.T.) ;
#14344 = ORIENTED_EDGE('',*,*,#9493,.T.) ;
#14345 = ORIENTED_EDGE('',*,*,#9610,.F.) ;
#14346 = ORIENTED_EDGE('',*,*,#9327,.T.) ;
#14347 = ORIENTED_EDGE('',*,*,#9726,.T.) ;
#14348 = ORIENTED_EDGE('',*,*,#9728,.T.) ;
#14349 = ORIENTED_EDGE('',*,*,#9729,.T.) ;
#14350 = ORIENTED_EDGE('',*,*,#9730,.T.) ;
#14351 = ORIENTED_EDGE('',*,*,#9729,.F.) ;
#14352 = ORIENTED_EDGE('',*,*,#9730,.F.) ;
#14353 = ORIENTED_EDGE('',*,*,#9731,.F.) ;
#14354 = ORIENTED_EDGE('',*,*,#9732,.F.) ;
#14355 = ORIENTED_EDGE('',*,*,#9733,.T.) ;
#14356 = ORIENTED_EDGE('',*,*,#9728,.F.) ;
#14357 = ORIENTED_EDGE('',*,*,#9733,.F.) ;
#14358 = ORIENTED_EDGE('',*,*,#9734,.T.) ;
#14359 = ORIENTED_EDGE('',*,*,#9735,.T.) ;
#14360 = ORIENTED_EDGE('',*,*,#9731,.T.) ;
#14361 = ORIENTED_EDGE('',*,*,#9735,.F.) ;
#14362 = ORIENTED_EDGE('',*,*,#9734,.F.) ;
#14363 = ORIENTED_EDGE('',*,*,#9736,.T.) ;
#14364 = ORIENTED_EDGE('',*,*,#9737,.F.) ;
#14365 = ORIENTED_EDGE('',*,*,#9736,.F.) ;
#14366 = ORIENTED_EDGE('',*,*,#9732,.T.) ;
#14367 = ORIENTED_EDGE('',*,*,#9738,.T.) ;
#14368 = ORIENTED_EDGE('',*,*,#9739,.T.) ;
#14369 = ORIENTED_EDGE('',*,*,#9738,.F.) ;
#14370 = ORIENTED_EDGE('',*,*,#9739,.F.) ;
#14371 = ORIENTED_EDGE('',*,*,#9740,.F.) ;
#14372 = ORIENTED_EDGE('',*,*,#9737,.T.) ;
#14373 = ORIENTED_EDGE('',*,*,#9741,.T.) ;
#14374 = ORIENTED_EDGE('',*,*,#9740,.T.) ;
#14375 = ORIENTED_EDGE('',*,*,#9741,.F.) ;
#14376 = ORIENTED_EDGE('',*,*,#9742,.F.) ;
#14377 = ORIENTED_EDGE('',*,*,#9743,.T.) ;
#14378 = ORIENTED_EDGE('',*,*,#9744,.F.) ;
#14379 = ORIENTED_EDGE('',*,*,#9743,.F.) ;
#14380 = ORIENTED_EDGE('',*,*,#9745,.F.) ;
#14381 = ORIENTED_EDGE('',*,*,#9746,.T.) ;
#14382 = ORIENTED_EDGE('',*,*,#9747,.F.) ;
#14383 = ORIENTED_EDGE('',*,*,#9746,.F.) ;
#14384 = ORIENTED_EDGE('',*,*,#9748,.F.) ;
#14385 = ORIENTED_EDGE('',*,*,#9749,.T.) ;
#14386 = ORIENTED_EDGE('',*,*,#9750,.F.) ;
#14387 = ORIENTED_EDGE('',*,*,#9749,.F.) ;
#14388 = ORIENTED_EDGE('',*,*,#9751,.F.) ;
#14389 = ORIENTED_EDGE('',*,*,#9752,.T.) ;
#14390 = ORIENTED_EDGE('',*,*,#9753,.F.) ;
#14391 = ORIENTED_EDGE('',*,*,#9752,.F.) ;
#14392 = ORIENTED_EDGE('',*,*,#9754,.F.) ;
#14393 = ORIENTED_EDGE('',*,*,#9755,.T.) ;
#14394 = ORIENTED_EDGE('',*,*,#9756,.F.) ;
#14395 = ORIENTED_EDGE('',*,*,#9755,.F.) ;
#14396 = ORIENTED_EDGE('',*,*,#9757,.F.) ;
#14397 = ORIENTED_EDGE('',*,*,#9758,.T.) ;
#14398 = ORIENTED_EDGE('',*,*,#9759,.F.) ;
#14399 = ORIENTED_EDGE('',*,*,#9758,.F.) ;
#14400 = ORIENTED_EDGE('',*,*,#9760,.F.) ;
#14401 = ORIENTED_EDGE('',*,*,#9761,.T.) ;
#14402 = ORIENTED_EDGE('',*,*,#9762,.F.) ;
#14403 = ORIENTED_EDGE('',*,*,#9761,.F.) ;
#14404 = ORIENTED_EDGE('',*,*,#9763,.F.) ;
#14405 = ORIENTED_EDGE('',*,*,#9764,.T.) ;
#14406 = ORIENTED_EDGE('',*,*,#9765,.F.) ;
#14407 = ORIENTED_EDGE('',*,*,#9764,.F.) ;
#14408 = ORIENTED_EDGE('',*,*,#9766,.F.) ;
#14409 = ORIENTED_EDGE('',*,*,#9767,.T.) ;
#14410 = ORIENTED_EDGE('',*,*,#9768,.F.) ;
#14411 = ORIENTED_EDGE('',*,*,#9767,.F.) ;
#14412 = ORIENTED_EDGE('',*,*,#9769,.F.) ;
#14413 = ORIENTED_EDGE('',*,*,#9770,.T.) ;
#14414 = ORIENTED_EDGE('',*,*,#9771,.F.) ;
#14415 = ORIENTED_EDGE('',*,*,#9770,.F.) ;
#14416 = ORIENTED_EDGE('',*,*,#9771,.T.) ;
#14417 = ORIENTED_EDGE('',*,*,#9744,.T.) ;
#14418 = ORIENTED_EDGE('',*,*,#9747,.T.) ;
#14419 = ORIENTED_EDGE('',*,*,#9750,.T.) ;
#14420 = ORIENTED_EDGE('',*,*,#9753,.T.) ;
#14421 = ORIENTED_EDGE('',*,*,#9756,.T.) ;
#14422 = ORIENTED_EDGE('',*,*,#9759,.T.) ;
#14423 = ORIENTED_EDGE('',*,*,#9762,.T.) ;
#14424 = ORIENTED_EDGE('',*,*,#9765,.T.) ;
#14425 = ORIENTED_EDGE('',*,*,#9766,.T.) ;
#14426 = ORIENTED_EDGE('',*,*,#9769,.T.) ;
#14427 = ORIENTED_EDGE('',*,*,#9742,.T.) ;
#14428 = ORIENTED_EDGE('',*,*,#9745,.T.) ;
#14429 = ORIENTED_EDGE('',*,*,#9748,.T.) ;
#14430 = ORIENTED_EDGE('',*,*,#9751,.T.) ;
#14431 = ORIENTED_EDGE('',*,*,#9754,.T.) ;
#14432 = ORIENTED_EDGE('',*,*,#9757,.T.) ;
#14433 = ORIENTED_EDGE('',*,*,#9760,.T.) ;
#14434 = ORIENTED_EDGE('',*,*,#9763,.T.) ;
#14435 = ORIENTED_EDGE('',*,*,#9768,.T.) ;
#14436 = ORIENTED_EDGE('',*,*,#9772,.T.) ;
#14437 = ORIENTED_EDGE('',*,*,#9773,.T.) ;
#14438 = ORIENTED_EDGE('',*,*,#9774,.T.) ;
#14439 = ORIENTED_EDGE('',*,*,#9773,.F.) ;
#14440 = ORIENTED_EDGE('',*,*,#9775,.T.) ;
#14441 = ORIENTED_EDGE('',*,*,#9776,.T.) ;
#14442 = ORIENTED_EDGE('',*,*,#9777,.T.) ;
#14443 = ORIENTED_EDGE('',*,*,#9776,.F.) ;
#14444 = ORIENTED_EDGE('',*,*,#9778,.T.) ;
#14445 = ORIENTED_EDGE('',*,*,#9779,.T.) ;
#14446 = ORIENTED_EDGE('',*,*,#9780,.T.) ;
#14447 = ORIENTED_EDGE('',*,*,#9779,.F.) ;
#14448 = ORIENTED_EDGE('',*,*,#9781,.T.) ;
#14449 = ORIENTED_EDGE('',*,*,#9782,.T.) ;
#14450 = ORIENTED_EDGE('',*,*,#9783,.T.) ;
#14451 = ORIENTED_EDGE('',*,*,#9782,.F.) ;
#14452 = ORIENTED_EDGE('',*,*,#9784,.T.) ;
#14453 = ORIENTED_EDGE('',*,*,#9785,.T.) ;
#14454 = ORIENTED_EDGE('',*,*,#9786,.T.) ;
#14455 = ORIENTED_EDGE('',*,*,#9785,.F.) ;
#14456 = ORIENTED_EDGE('',*,*,#9787,.T.) ;
#14457 = ORIENTED_EDGE('',*,*,#9788,.T.) ;
#14458 = ORIENTED_EDGE('',*,*,#9789,.T.) ;
#14459 = ORIENTED_EDGE('',*,*,#9788,.F.) ;
#14460 = ORIENTED_EDGE('',*,*,#9790,.T.) ;
#14461 = ORIENTED_EDGE('',*,*,#9791,.T.) ;
#14462 = ORIENTED_EDGE('',*,*,#9792,.T.) ;
#14463 = ORIENTED_EDGE('',*,*,#9791,.F.) ;
#14464 = ORIENTED_EDGE('',*,*,#9793,.T.) ;
#14465 = ORIENTED_EDGE('',*,*,#9794,.T.) ;
#14466 = ORIENTED_EDGE('',*,*,#9795,.T.) ;
#14467 = ORIENTED_EDGE('',*,*,#9794,.F.) ;
#14468 = ORIENTED_EDGE('',*,*,#9796,.T.) ;
#14469 = ORIENTED_EDGE('',*,*,#9797,.T.) ;
#14470 = ORIENTED_EDGE('',*,*,#9798,.T.) ;
#14471 = ORIENTED_EDGE('',*,*,#9797,.F.) ;
#14472 = ORIENTED_EDGE('',*,*,#9799,.T.) ;
#14473 = ORIENTED_EDGE('',*,*,#9800,.T.) ;
#14474 = ORIENTED_EDGE('',*,*,#9801,.T.) ;
#14475 = ORIENTED_EDGE('',*,*,#9800,.F.) ;
#14476 = ORIENTED_EDGE('',*,*,#9799,.F.) ;
#14477 = ORIENTED_EDGE('',*,*,#9772,.F.) ;
#14478 = ORIENTED_EDGE('',*,*,#9775,.F.) ;
#14479 = ORIENTED_EDGE('',*,*,#9778,.F.) ;
#14480 = ORIENTED_EDGE('',*,*,#9781,.F.) ;
#14481 = ORIENTED_EDGE('',*,*,#9784,.F.) ;
#14482 = ORIENTED_EDGE('',*,*,#9787,.F.) ;
#14483 = ORIENTED_EDGE('',*,*,#9790,.F.) ;
#14484 = ORIENTED_EDGE('',*,*,#9793,.F.) ;
#14485 = ORIENTED_EDGE('',*,*,#9798,.F.) ;
#14486 = ORIENTED_EDGE('',*,*,#9801,.F.) ;
#14487 = ORIENTED_EDGE('',*,*,#9774,.F.) ;
#14488 = ORIENTED_EDGE('',*,*,#9777,.F.) ;
#14489 = ORIENTED_EDGE('',*,*,#9780,.F.) ;
#14490 = ORIENTED_EDGE('',*,*,#9783,.F.) ;
#14491 = ORIENTED_EDGE('',*,*,#9786,.F.) ;
#14492 = ORIENTED_EDGE('',*,*,#9789,.F.) ;
#14493 = ORIENTED_EDGE('',*,*,#9792,.F.) ;
#14494 = ORIENTED_EDGE('',*,*,#9795,.F.) ;
#14495 = ORIENTED_EDGE('',*,*,#9796,.F.) ;
#14496 = CONICAL_SURFACE('',#15677,2.42186816158307,1.02974425867665) ;
#14497 = CONICAL_SURFACE('',#15681,2.42186816158307,1.02974425867665) ;
#14498 = CONICAL_SURFACE('',#15685,2.42186816158307,1.02974425867665) ;
#14499 = CONICAL_SURFACE('',#15689,2.42186816158307,1.02974425867665) ;
#14500 = CONICAL_SURFACE('',#15721,1.65,1.02974425867665) ;
#14501 = CONICAL_SURFACE('',#15725,1.44243074893998,1.02974425867665) ;
#14502 = CONICAL_SURFACE('',#15729,1.44243074893998,1.02974425867665) ;
#14503 = CONICAL_SURFACE('',#15733,1.44243074893998,1.02974425867665) ;
#14504 = CONICAL_SURFACE('',#15737,1.44243074893998,1.02974425867665) ;
#14505 = CONICAL_SURFACE('',#15741,1.44243074893998,1.02974425867665) ;
#14506 = CONICAL_SURFACE('',#15745,1.44243074893998,1.02974425867665) ;
#14507 = CONICAL_SURFACE('',#15749,1.65,1.02974425867665) ;
#14508 = CONICAL_SURFACE('',#15854,2.42186816158307,1.02974425867665) ;
#14509 = CONICAL_SURFACE('',#15858,2.42186816158307,1.02974425867665) ;
#14510 = CONICAL_SURFACE('',#15862,2.42186816158307,1.02974425867665) ;
#14511 = CONICAL_SURFACE('',#15866,2.42186816158307,1.02974425867665) ;
#14512 = CONICAL_SURFACE('',#15870,2.42186816158307,1.02974425867665) ;
#14513 = CONICAL_SURFACE('',#15874,2.42186816158307,1.02974425867665) ;
#14514 = CONICAL_SURFACE('',#15879,2.42186816158307,1.02974425867665) ;
#14515 = CONICAL_SURFACE('',#15883,2.42186816158307,1.02974425867665) ;
#14516 = CONICAL_SURFACE('',#15893,1.20708774962173,1.02974425867665) ;
#14517 = CONICAL_SURFACE('',#15897,1.20708774962173,1.02974425867665) ;
#14518 = CONICAL_SURFACE('',#15901,2.42186816158307,1.02974425867665) ;
#14519 = CONICAL_SURFACE('',#15905,2.42186816158307,1.02974425867665) ;
#14520 = CONICAL_SURFACE('',#15909,2.42186816158307,1.02974425867665) ;
#14521 = CONICAL_SURFACE('',#15913,2.42186816158307,1.02974425867665) ;
#14522 = CONICAL_SURFACE('',#15945,1.65,1.02974425867665) ;
#14523 = CONICAL_SURFACE('',#15949,1.44243074893998,1.02974425867665) ;
#14524 = CONICAL_SURFACE('',#15953,1.44243074893998,1.02974425867665) ;
#14525 = CONICAL_SURFACE('',#15957,1.44243074893998,1.02974425867665) ;
#14526 = CONICAL_SURFACE('',#15961,1.44243074893998,1.02974425867665) ;
#14527 = CONICAL_SURFACE('',#15965,1.44243074893998,1.02974425867665) ;
#14528 = CONICAL_SURFACE('',#15969,1.44243074893998,1.02974425867665) ;
#14529 = CONICAL_SURFACE('',#15973,1.65,1.02974425867665) ;
#14530 = CONICAL_SURFACE('',#15987,2.42186816158307,1.02974425867665) ;
#14531 = CONICAL_SURFACE('',#15991,2.42186816158307,1.02974425867665) ;
#14532 = CONICAL_SURFACE('',#15995,2.42186816158307,1.02974425867665) ;
#14533 = CONICAL_SURFACE('',#15999,2.42186816158307,1.02974425867665) ;
#14534 = CONICAL_SURFACE('',#16003,2.42186816158307,1.02974425867665) ;
#14535 = CONICAL_SURFACE('',#16007,2.42186816158307,1.02974425867665) ;
#14536 = CONICAL_SURFACE('',#16012,2.42186816158307,1.02974425867665) ;
#14537 = CONICAL_SURFACE('',#16016,2.42186816158307,1.02974425867665) ;
#14538 = CONICAL_SURFACE('',#16078,13.3250000000001,0.785398163397564) ;
#14539 = CONICAL_SURFACE('',#16086,17.375,0.785398163397199) ;
#14540 = CONICAL_SURFACE('',#16091,19.8749999999998,0.785398163397706) ;
#14541 = CONICAL_SURFACE('',#16099,22.375,0.785398163397484) ;
#14542 = CONICAL_SURFACE('',#16106,33.3824824663842,0.611520837079942) ;
#14543 = CONICAL_SURFACE('',#16114,26.7825,1.22304167415987) ;
#14544 = CONICAL_SURFACE('',#16116,33.375,0.785398163397448) ;
#14545 = CONICAL_SURFACE('',#16120,15.7556101392397,0.797758865436123) ;
#14546 = CONICAL_SURFACE('',#16124,14.41685,0.0247214040773807) ;
#14547 = CONICAL_SURFACE('',#16126,33.375,0.785398163397439) ;
#14548 = CONICAL_SURFACE('',#16135,33.375,0.785398163397439) ;
#14549 = CONICAL_SURFACE('',#16192,26.9,0.785398163397449) ;
#14550 = CONICAL_SURFACE('',#16199,22.6,0.785398163397449) ;
#14551 = CONICAL_SURFACE('',#16203,26.9,0.785398163397448) ;
#14552 = CONICAL_SURFACE('',#16207,22.6,0.785398163397448) ;
#14553 = CONICAL_SURFACE('',#16399,47.0433475024125,1.30899693899575) ;
#14554 = CONICAL_SURFACE('',#16402,49.2411809548974,0.261799387799187) ;
#14555 = CONICAL_SURFACE('',#16405,49.5,1.30899693899575) ;
#14556 = CONICAL_SURFACE('',#16467,47.175,1.30899693899575) ;
#14557 = CONICAL_SURFACE('',#16531,49.5,0.261799387799147) ;
#14558 = CONICAL_SURFACE('',#16534,49.2411809548975,1.30899693899575) ;
#14559 = CONICAL_SURFACE('',#17212,20.,0.785398163397449) ;
#14560 = CONICAL_SURFACE('',#17216,24.5,0.785398163397449) ;
#14561 = CONICAL_SURFACE('',#17221,25.,0.785398163397448) ;
#14562 = CONICAL_SURFACE('',#17225,20.5,0.785398163397448) ;
#14563 = CONICAL_SURFACE('',#17243,27.,0.785398163397448) ;
#14564 = CONICAL_SURFACE('',#17251,27.,0.785398163397448) ;
#14565 = CONICAL_SURFACE('',#17259,27.,0.785398163397448) ;
#14566 = CONICAL_SURFACE('',#17265,27.,0.785398163397448) ;
#14567 = CONICAL_SURFACE('',#17273,28.523658167371,1.38589614583862) ;
#14568 = CONICAL_SURFACE('',#17334,26.6311750163962,0.166009849666151) ;
#14569 = CONICAL_SURFACE('',#17454,32.4669335366504,0.203790512246407) ;
#14570 = CONICAL_SURFACE('',#17598,26.3029085923563,1.38589614583862) ;
#14571 = CONICAL_SURFACE('',#17599,3.04415568548155,0.0188926771603406) ;
#14572 = CONICAL_SURFACE('',#17605,3.04415568548155,0.0188926771603406) ;
#14573 = CONICAL_SURFACE('',#17606,3.04415568548155,0.0188926771603406) ;
#14574 = CONICAL_SURFACE('',#17612,3.04415568548155,0.0188926771603406) ;
#14575 = CONICAL_SURFACE('',#17613,3.04415568548155,0.0188926771603406) ;
#14576 = CONICAL_SURFACE('',#17619,3.04415568548155,0.0188926771603406) ;
#14577 = CONICAL_SURFACE('',#17620,3.04415568548155,0.0188926771603406) ;
#14578 = CONICAL_SURFACE('',#17626,3.04415568548155,0.0188926771603406) ;
#14579 = CONICAL_SURFACE('',#17627,3.04415568548155,0.0188926771603406) ;
#14580 = CONICAL_SURFACE('',#17633,3.04415568548155,0.0188926771603406) ;
#14581 = CONICAL_SURFACE('',#17634,3.04415568548155,0.0188926771603406) ;
#14582 = CONICAL_SURFACE('',#17640,3.04415568548155,0.0188926771603406) ;
#14583 = CONICAL_SURFACE('',#17641,3.04415568548155,0.0188926771603406) ;
#14584 = CONICAL_SURFACE('',#17647,3.04415568548155,0.0188926771603406) ;
#14585 = CONICAL_SURFACE('',#17648,3.04415568548155,0.0188926771603406) ;
#14586 = CONICAL_SURFACE('',#17654,3.04415568548155,0.0188926771603406) ;
#14587 = CONICAL_SURFACE('',#17655,3.04415568548155,0.0188926771603406) ;
#14588 = CONICAL_SURFACE('',#17661,3.04415568548155,0.0188926771603406) ;
#14589 = CONICAL_SURFACE('',#17662,3.04415568548155,0.0188926771603406) ;
#14590 = CONICAL_SURFACE('',#17668,3.04415568548155,0.0188926771603406) ;
#14591 = CONICAL_SURFACE('',#17669,3.04415568548155,0.0188926771603406) ;
#14592 = CONICAL_SURFACE('',#17675,3.04415568548155,0.0188926771603406) ;
#14593 = CONICAL_SURFACE('',#17676,3.04415568548155,0.0188926771603406) ;
#14594 = CONICAL_SURFACE('',#17682,3.04415568548155,0.0188926771603406) ;
#14595 = CONICAL_SURFACE('',#17683,3.04415568548155,0.0188926771603406) ;
#14596 = CONICAL_SURFACE('',#17689,3.04415568548155,0.0188926771603406) ;
#14597 = CONICAL_SURFACE('',#17690,3.04415568548155,0.0188926771603406) ;
#14598 = CONICAL_SURFACE('',#17696,3.04415568548155,0.0188926771603406) ;
#14599 = CONICAL_SURFACE('',#17697,3.04415568548155,0.0188926771603406) ;
#14600 = CONICAL_SURFACE('',#17703,3.04415568548155,0.0188926771603406) ;
#14601 = CONICAL_SURFACE('',#17704,3.04415568548155,0.0188926771603406) ;
#14602 = CONICAL_SURFACE('',#17710,3.04415568548155,0.0188926771603406) ;
#14603 = CONICAL_SURFACE('',#17711,3.04415568548155,0.0188926771603406) ;
#14604 = CONICAL_SURFACE('',#17717,3.04415568548155,0.0188926771603406) ;
#14605 = CONICAL_SURFACE('',#17718,3.04415568548155,0.0188926771603406) ;
#14606 = CONICAL_SURFACE('',#17724,3.04415568548155,0.0188926771603406) ;
#14607 = CONICAL_SURFACE('',#17725,3.04415568548155,0.0188926771603406) ;
#14608 = CONICAL_SURFACE('',#17731,3.04415568548155,0.0188926771603406) ;
#14609 = CONICAL_SURFACE('',#17732,3.04415568548155,0.0188926771603406) ;
#14610 = CONICAL_SURFACE('',#17738,3.04415568548155,0.0188926771603406) ;
#14611 = CONICAL_SURFACE('',#17739,3.04415568548155,0.0188926771603406) ;
#14612 = CONICAL_SURFACE('',#17745,3.04415568548155,0.0188926771603406) ;
#14613 = CONICAL_SURFACE('',#17746,3.04415568548155,0.0188926771603406) ;
#14614 = CONICAL_SURFACE('',#17752,3.04415568548155,0.0188926771603406) ;
#14615 = CONICAL_SURFACE('',#17753,3.04415568548155,0.0188926771603406) ;
#14616 = CONICAL_SURFACE('',#17759,3.04415568548155,0.0188926771603406) ;
#14617 = CONICAL_SURFACE('',#17760,3.04415568548155,0.0188926771603406) ;
#14618 = CONICAL_SURFACE('',#17766,3.04415568548155,0.0188926771603406) ;
#14619 = CONICAL_SURFACE('',#17767,3.04415568548155,0.0188926771603406) ;
#14620 = CONICAL_SURFACE('',#17773,3.04415568548155,0.0188926771603406) ;
#14621 = CONICAL_SURFACE('',#17774,3.04415568548155,0.0188926771603406) ;
#14622 = CONICAL_SURFACE('',#17780,3.04415568548155,0.0188926771603406) ;
#14623 = CONICAL_SURFACE('',#17781,3.04415568548155,0.0188926771603406) ;
#14624 = CONICAL_SURFACE('',#17787,3.04415568548155,0.0188926771603406) ;
#14625 = CONICAL_SURFACE('',#17788,3.04415568548155,0.0188926771603406) ;
#14626 = CONICAL_SURFACE('',#17794,3.04415568548155,0.0188926771603406) ;
#14627 = CONICAL_SURFACE('',#17795,3.04415568548155,0.0188926771603406) ;
#14628 = CONICAL_SURFACE('',#17801,3.04415568548155,0.0188926771603406) ;
#14629 = CONICAL_SURFACE('',#17803,36.4,0.785398163397449) ;
#14630 = CONICAL_SURFACE('',#17810,22.6,0.785398163397449) ;
#14631 = CONICAL_SURFACE('',#17814,36.4,0.785398163397448) ;
#14632 = CONICAL_SURFACE('',#17818,22.6,0.785398163397448) ;
#14633 = ADVANCED_FACE('',(#1545),#14496,.F.) ;
#14634 = ADVANCED_FACE('',(#1546),#1116,.F.) ;
#14635 = ADVANCED_FACE('',(#1547),#14497,.F.) ;
#14636 = ADVANCED_FACE('',(#1548),#1117,.F.) ;
#14637 = ADVANCED_FACE('',(#1549),#14498,.F.) ;
#14638 = ADVANCED_FACE('',(#1550),#1118,.F.) ;
#14639 = ADVANCED_FACE('',(#1551),#14499,.F.) ;
#14640 = ADVANCED_FACE('',(#1552),#1119,.F.) ;
#14641 = ADVANCED_FACE('',(#1553,#625),#832,.F.) ;
#14642 = ADVANCED_FACE('',(#1554),#1120,.F.) ;
#14643 = ADVANCED_FACE('',(#1555),#1121,.F.) ;
#14644 = ADVANCED_FACE('',(#1556,#626),#833,.F.) ;
#14645 = ADVANCED_FACE('',(#1557),#1122,.F.) ;
#14646 = ADVANCED_FACE('',(#1558),#1123,.F.) ;
#14647 = ADVANCED_FACE('',(#1559,#627),#834,.F.) ;
#14648 = ADVANCED_FACE('',(#1560),#1124,.F.) ;
#14649 = ADVANCED_FACE('',(#1561),#1125,.F.) ;
#14650 = ADVANCED_FACE('',(#1562,#628),#835,.F.) ;
#14651 = ADVANCED_FACE('',(#1563),#1126,.F.) ;
#14652 = ADVANCED_FACE('',(#1564),#1127,.F.) ;
#14653 = ADVANCED_FACE('',(#1565),#14500,.F.) ;
#14654 = ADVANCED_FACE('',(#1566),#1128,.F.) ;
#14655 = ADVANCED_FACE('',(#1567),#14501,.F.) ;
#14656 = ADVANCED_FACE('',(#1568),#1129,.F.) ;
#14657 = ADVANCED_FACE('',(#1569),#14502,.F.) ;
#14658 = ADVANCED_FACE('',(#1570),#1130,.F.) ;
#14659 = ADVANCED_FACE('',(#1571),#14503,.F.) ;
#14660 = ADVANCED_FACE('',(#1572),#1131,.F.) ;
#14661 = ADVANCED_FACE('',(#1573),#14504,.F.) ;
#14662 = ADVANCED_FACE('',(#1574),#1132,.F.) ;
#14663 = ADVANCED_FACE('',(#1575),#14505,.F.) ;
#14664 = ADVANCED_FACE('',(#1576),#1133,.F.) ;
#14665 = ADVANCED_FACE('',(#1577),#14506,.F.) ;
#14666 = ADVANCED_FACE('',(#1578),#1134,.F.) ;
#14667 = ADVANCED_FACE('',(#1579),#14507,.F.) ;
#14668 = ADVANCED_FACE('',(#1580),#1135,.F.) ;
#14669 = ADVANCED_FACE('',(#1581),#1136,.F.) ;
#14670 = ADVANCED_FACE('',(#1582,#629,#630),#836,.T.) ;
#14671 = ADVANCED_FACE('',(#1583),#837,.T.) ;
#14672 = ADVANCED_FACE('',(#1584,#631,#632),#838,.T.) ;
#14673 = ADVANCED_FACE('',(#1585),#839,.T.) ;
#14674 = ADVANCED_FACE('',(#1586,#633,#634,#635,#636,#637),#840,.T.) ;
#14675 = ADVANCED_FACE('',(#1587,#638,#639,#640,#641,#642,#643,#644,#645,
#646,#647,#648,#649,#650),#841,.F.) ;
#14676 = ADVANCED_FACE('',(#1588,#651),#842,.F.) ;
#14677 = ADVANCED_FACE('',(#1589),#1137,.F.) ;
#14678 = ADVANCED_FACE('',(#1590),#1138,.F.) ;
#14679 = ADVANCED_FACE('',(#1591,#652),#843,.F.) ;
#14680 = ADVANCED_FACE('',(#1592),#1139,.F.) ;
#14681 = ADVANCED_FACE('',(#1593),#1140,.F.) ;
#14682 = ADVANCED_FACE('',(#1594,#653),#844,.F.) ;
#14683 = ADVANCED_FACE('',(#1595),#1141,.F.) ;
#14684 = ADVANCED_FACE('',(#1596),#1142,.F.) ;
#14685 = ADVANCED_FACE('',(#1597,#654),#845,.F.) ;
#14686 = ADVANCED_FACE('',(#1598),#1143,.F.) ;
#14687 = ADVANCED_FACE('',(#1599),#1144,.F.) ;
#14688 = ADVANCED_FACE('',(#1600,#655),#846,.F.) ;
#14689 = ADVANCED_FACE('',(#1601),#1145,.F.) ;
#14690 = ADVANCED_FACE('',(#1602),#1146,.F.) ;
#14691 = ADVANCED_FACE('',(#1603,#656),#847,.F.) ;
#14692 = ADVANCED_FACE('',(#1604),#1147,.F.) ;
#14693 = ADVANCED_FACE('',(#1605),#1148,.F.) ;
#14694 = ADVANCED_FACE('',(#1606,#657),#848,.F.) ;
#14695 = ADVANCED_FACE('',(#1607),#1149,.F.) ;
#14696 = ADVANCED_FACE('',(#1608),#1150,.F.) ;
#14697 = ADVANCED_FACE('',(#1609,#658),#849,.F.) ;
#14698 = ADVANCED_FACE('',(#1610),#1151,.F.) ;
#14699 = ADVANCED_FACE('',(#1611),#1152,.F.) ;
#14700 = ADVANCED_FACE('',(#1612,#659),#850,.F.) ;
#14701 = ADVANCED_FACE('',(#1613),#1153,.F.) ;
#14702 = ADVANCED_FACE('',(#1614),#1154,.F.) ;
#14703 = ADVANCED_FACE('',(#1615,#660),#851,.F.) ;
#14704 = ADVANCED_FACE('',(#1616),#1155,.F.) ;
#14705 = ADVANCED_FACE('',(#1617),#1156,.F.) ;
#14706 = ADVANCED_FACE('',(#1618,#661),#852,.F.) ;
#14707 = ADVANCED_FACE('',(#1619),#1157,.F.) ;
#14708 = ADVANCED_FACE('',(#1620),#1158,.F.) ;
#14709 = ADVANCED_FACE('',(#1621,#662),#853,.F.) ;
#14710 = ADVANCED_FACE('',(#1622),#1159,.F.) ;
#14711 = ADVANCED_FACE('',(#1623),#1160,.F.) ;
#14712 = ADVANCED_FACE('',(#1624,#663,#664,#665,#666,#667,#668,#669,#670,
#671,#672,#673,#674),#854,.T.) ;
#14713 = ADVANCED_FACE('',(#1625),#855,.T.) ;
#14714 = ADVANCED_FACE('',(#1626,#675,#676,#677,#678,#679,#680,#681,#682,
#683,#684,#685,#686),#856,.T.) ;
#14715 = ADVANCED_FACE('',(#1627),#857,.T.) ;
#14716 = ADVANCED_FACE('',(#1628),#858,.T.) ;
#14717 = ADVANCED_FACE('',(#1629),#859,.T.) ;
#14718 = ADVANCED_FACE('',(#1630),#14508,.F.) ;
#14719 = ADVANCED_FACE('',(#1631),#1161,.F.) ;
#14720 = ADVANCED_FACE('',(#1632),#14509,.F.) ;
#14721 = ADVANCED_FACE('',(#1633),#1162,.F.) ;
#14722 = ADVANCED_FACE('',(#1634),#14510,.F.) ;
#14723 = ADVANCED_FACE('',(#1635),#1163,.F.) ;
#14724 = ADVANCED_FACE('',(#1636),#14511,.F.) ;
#14725 = ADVANCED_FACE('',(#1637),#1164,.F.) ;
#14726 = ADVANCED_FACE('',(#1638),#14512,.F.) ;
#14727 = ADVANCED_FACE('',(#1639),#1165,.F.) ;
#14728 = ADVANCED_FACE('',(#1640),#14513,.F.) ;
#14729 = ADVANCED_FACE('',(#1641),#1166,.F.) ;
#14730 = ADVANCED_FACE('',(#1642,#687,#688),#860,.T.) ;
#14731 = ADVANCED_FACE('',(#1643),#14514,.F.) ;
#14732 = ADVANCED_FACE('',(#1644),#1167,.F.) ;
#14733 = ADVANCED_FACE('',(#1645),#14515,.F.) ;
#14734 = ADVANCED_FACE('',(#1646),#1168,.F.) ;
#14735 = ADVANCED_FACE('',(#1647),#861,.T.) ;
#14736 = ADVANCED_FACE('',(#1648,#689,#690),#862,.T.) ;
#14737 = ADVANCED_FACE('',(#1649),#863,.T.) ;
#14738 = ADVANCED_FACE('',(#1650,#691,#692),#864,.T.) ;
#14739 = ADVANCED_FACE('',(#1651,#693,#694),#865,.F.) ;
#14740 = ADVANCED_FACE('',(#1652),#14516,.F.) ;
#14741 = ADVANCED_FACE('',(#1653),#1169,.F.) ;
#14742 = ADVANCED_FACE('',(#1654),#14517,.F.) ;
#14743 = ADVANCED_FACE('',(#1655),#1170,.F.) ;
#14744 = ADVANCED_FACE('',(#1656),#14518,.F.) ;
#14745 = ADVANCED_FACE('',(#1657),#1171,.F.) ;
#14746 = ADVANCED_FACE('',(#1658),#14519,.F.) ;
#14747 = ADVANCED_FACE('',(#1659),#1172,.F.) ;
#14748 = ADVANCED_FACE('',(#1660),#14520,.F.) ;
#14749 = ADVANCED_FACE('',(#1661),#1173,.F.) ;
#14750 = ADVANCED_FACE('',(#1662),#14521,.F.) ;
#14751 = ADVANCED_FACE('',(#1663),#1174,.F.) ;
#14752 = ADVANCED_FACE('',(#1664,#695),#866,.T.) ;
#14753 = ADVANCED_FACE('',(#1665),#1175,.F.) ;
#14754 = ADVANCED_FACE('',(#1666),#1176,.F.) ;
#14755 = ADVANCED_FACE('',(#1667,#696),#867,.T.) ;
#14756 = ADVANCED_FACE('',(#1668),#1177,.F.) ;
#14757 = ADVANCED_FACE('',(#1669),#1178,.F.) ;
#14758 = ADVANCED_FACE('',(#1670,#697),#868,.T.) ;
#14759 = ADVANCED_FACE('',(#1671),#1179,.F.) ;
#14760 = ADVANCED_FACE('',(#1672),#1180,.F.) ;
#14761 = ADVANCED_FACE('',(#1673,#698),#869,.T.) ;
#14762 = ADVANCED_FACE('',(#1674),#1181,.F.) ;
#14763 = ADVANCED_FACE('',(#1675),#1182,.F.) ;
#14764 = ADVANCED_FACE('',(#1676),#14522,.F.) ;
#14765 = ADVANCED_FACE('',(#1677),#1183,.F.) ;
#14766 = ADVANCED_FACE('',(#1678),#14523,.F.) ;
#14767 = ADVANCED_FACE('',(#1679),#1184,.F.) ;
#14768 = ADVANCED_FACE('',(#1680),#14524,.F.) ;
#14769 = ADVANCED_FACE('',(#1681),#1185,.F.) ;
#14770 = ADVANCED_FACE('',(#1682),#14525,.F.) ;
#14771 = ADVANCED_FACE('',(#1683),#1186,.F.) ;
#14772 = ADVANCED_FACE('',(#1684),#14526,.F.) ;
#14773 = ADVANCED_FACE('',(#1685),#1187,.F.) ;
#14774 = ADVANCED_FACE('',(#1686),#14527,.F.) ;
#14775 = ADVANCED_FACE('',(#1687),#1188,.F.) ;
#14776 = ADVANCED_FACE('',(#1688),#14528,.F.) ;
#14777 = ADVANCED_FACE('',(#1689),#1189,.F.) ;
#14778 = ADVANCED_FACE('',(#1690),#14529,.F.) ;
#14779 = ADVANCED_FACE('',(#1691),#1190,.F.) ;
#14780 = ADVANCED_FACE('',(#1692),#1191,.F.) ;
#14781 = ADVANCED_FACE('',(#1693,#699,#700),#870,.F.) ;
#14782 = ADVANCED_FACE('',(#1694),#871,.F.) ;
#14783 = ADVANCED_FACE('',(#1695,#701,#702),#872,.F.) ;
#14784 = ADVANCED_FACE('',(#1696),#873,.F.) ;
#14785 = ADVANCED_FACE('',(#1697,#703,#704,#705,#706,#707,#708,#709),#874,
 .F.) ;
#14786 = ADVANCED_FACE('',(#1698,#710,#711,#712,#713,#714,#715,#716,#717,
#718,#719,#720,#721,#722),#875,.T.) ;
#14787 = ADVANCED_FACE('',(#1699),#14530,.F.) ;
#14788 = ADVANCED_FACE('',(#1700),#1192,.F.) ;
#14789 = ADVANCED_FACE('',(#1701),#14531,.F.) ;
#14790 = ADVANCED_FACE('',(#1702),#1193,.F.) ;
#14791 = ADVANCED_FACE('',(#1703),#14532,.F.) ;
#14792 = ADVANCED_FACE('',(#1704),#1194,.F.) ;
#14793 = ADVANCED_FACE('',(#1705),#14533,.F.) ;
#14794 = ADVANCED_FACE('',(#1706),#1195,.F.) ;
#14795 = ADVANCED_FACE('',(#1707),#14534,.F.) ;
#14796 = ADVANCED_FACE('',(#1708),#1196,.F.) ;
#14797 = ADVANCED_FACE('',(#1709),#14535,.F.) ;
#14798 = ADVANCED_FACE('',(#1710),#1197,.F.) ;
#14799 = ADVANCED_FACE('',(#1711,#723,#724),#876,.F.) ;
#14800 = ADVANCED_FACE('',(#1712),#14536,.F.) ;
#14801 = ADVANCED_FACE('',(#1713),#1198,.F.) ;
#14802 = ADVANCED_FACE('',(#1714),#14537,.F.) ;
#14803 = ADVANCED_FACE('',(#1715),#1199,.F.) ;
#14804 = ADVANCED_FACE('',(#1716),#877,.F.) ;
#14805 = ADVANCED_FACE('',(#1717,#725,#726),#878,.F.) ;
#14806 = ADVANCED_FACE('',(#1718),#879,.F.) ;
#14807 = ADVANCED_FACE('',(#1719,#727,#728),#880,.F.) ;
#14808 = ADVANCED_FACE('',(#1720,#729,#730),#881,.T.) ;
#14809 = ADVANCED_FACE('',(#1721),#1200,.T.) ;
#14810 = ADVANCED_FACE('',(#1722),#1201,.T.) ;
#14811 = ADVANCED_FACE('',(#1723),#1202,.T.) ;
#14812 = ADVANCED_FACE('',(#1724),#1203,.T.) ;
#14813 = ADVANCED_FACE('',(#1725),#1204,.T.) ;
#14814 = ADVANCED_FACE('',(#1726),#1205,.T.) ;
#14815 = ADVANCED_FACE('',(#1727),#1206,.T.) ;
#14816 = ADVANCED_FACE('',(#1728),#1207,.T.) ;
#14817 = ADVANCED_FACE('',(#1729),#1208,.T.) ;
#14818 = ADVANCED_FACE('',(#1730),#1209,.T.) ;
#14819 = ADVANCED_FACE('',(#1731),#1210,.T.) ;
#14820 = ADVANCED_FACE('',(#1732),#1211,.T.) ;
#14821 = ADVANCED_FACE('',(#1733),#1212,.T.) ;
#14822 = ADVANCED_FACE('',(#1734),#1213,.T.) ;
#14823 = ADVANCED_FACE('',(#1735),#1214,.T.) ;
#14824 = ADVANCED_FACE('',(#1736),#1215,.T.) ;
#14825 = ADVANCED_FACE('',(#1737),#1216,.T.) ;
#14826 = ADVANCED_FACE('',(#1738),#1217,.T.) ;
#14827 = ADVANCED_FACE('',(#1739),#1218,.T.) ;
#14828 = ADVANCED_FACE('',(#1740),#1219,.T.) ;
#14829 = ADVANCED_FACE('',(#1741),#1220,.T.) ;
#14830 = ADVANCED_FACE('',(#1742),#1221,.T.) ;
#14831 = ADVANCED_FACE('',(#1743),#1222,.T.) ;
#14832 = ADVANCED_FACE('',(#1744),#1223,.T.) ;
#14833 = ADVANCED_FACE('',(#1745),#1224,.T.) ;
#14834 = ADVANCED_FACE('',(#1746),#1225,.T.) ;
#14835 = ADVANCED_FACE('',(#1747),#1226,.T.) ;
#14836 = ADVANCED_FACE('',(#1748),#1227,.T.) ;
#14837 = ADVANCED_FACE('',(#1749),#1228,.T.) ;
#14838 = ADVANCED_FACE('',(#1750),#1229,.T.) ;
#14839 = ADVANCED_FACE('',(#1751),#1230,.T.) ;
#14840 = ADVANCED_FACE('',(#1752),#1231,.T.) ;
#14841 = ADVANCED_FACE('',(#1753),#1232,.T.) ;
#14842 = ADVANCED_FACE('',(#1754),#1233,.T.) ;
#14843 = ADVANCED_FACE('',(#1755),#1234,.T.) ;
#14844 = ADVANCED_FACE('',(#1756),#1235,.T.) ;
#14845 = ADVANCED_FACE('',(#1757),#1236,.T.) ;
#14846 = ADVANCED_FACE('',(#1758),#1237,.T.) ;
#14847 = ADVANCED_FACE('',(#1759),#1238,.T.) ;
#14848 = ADVANCED_FACE('',(#1760),#1239,.T.) ;
#14849 = ADVANCED_FACE('',(#1761),#1240,.T.) ;
#14850 = ADVANCED_FACE('',(#1762),#1241,.T.) ;
#14851 = ADVANCED_FACE('',(#1763),#1242,.T.) ;
#14852 = ADVANCED_FACE('',(#1764),#14538,.F.) ;
#14853 = ADVANCED_FACE('',(#1765,#731),#882,.T.) ;
#14854 = ADVANCED_FACE('',(#1766),#1243,.F.) ;
#14855 = ADVANCED_FACE('',(#1767),#14539,.T.) ;
#14856 = ADVANCED_FACE('',(#1768),#1244,.T.) ;
#14857 = ADVANCED_FACE('',(#1769),#14540,.T.) ;
#14858 = ADVANCED_FACE('',(#1770,#732),#1245,.T.) ;
#14859 = ADVANCED_FACE('',(#1771,#733),#883,.T.) ;
#14860 = ADVANCED_FACE('',(#1772),#14541,.T.) ;
#14861 = ADVANCED_FACE('',(#1773),#1246,.T.) ;
#14862 = ADVANCED_FACE('',(#1774,#734),#884,.T.) ;
#14863 = ADVANCED_FACE('',(#1775),#14542,.T.) ;
#14864 = ADVANCED_FACE('',(#1776),#1247,.T.) ;
#14865 = ADVANCED_FACE('',(#1777),#14543,.T.) ;
#14866 = ADVANCED_FACE('',(#1778),#14544,.T.) ;
#14867 = ADVANCED_FACE('',(#1779,#735),#885,.T.) ;
#14868 = ADVANCED_FACE('',(#1780),#14545,.F.) ;
#14869 = ADVANCED_FACE('',(#1781),#14546,.F.) ;
#14870 = ADVANCED_FACE('',(#1782,#736),#886,.T.) ;
#14871 = ADVANCED_FACE('',(#1783),#14547,.T.) ;
#14872 = ADVANCED_FACE('',(#1784,#737,#738,#739),#1248,.T.) ;
#14873 = ADVANCED_FACE('',(#1785,#740),#887,.T.) ;
#14874 = ADVANCED_FACE('',(#1786),#14548,.T.) ;
#14875 = ADVANCED_FACE('',(#1787,#741),#888,.T.) ;
#14876 = ADVANCED_FACE('',(#1788),#215,.F.) ;
#14877 = ADVANCED_FACE('',(#1789),#1249,.T.) ;
#14878 = ADVANCED_FACE('',(#1790),#216,.F.) ;
#14879 = ADVANCED_FACE('',(#1791),#1250,.T.) ;
#14880 = ADVANCED_FACE('',(#1792),#217,.F.) ;
#14881 = ADVANCED_FACE('',(#1793),#1251,.T.) ;
#14882 = ADVANCED_FACE('',(#1794),#218,.F.) ;
#14883 = ADVANCED_FACE('',(#1795),#219,.F.) ;
#14884 = ADVANCED_FACE('',(#1796,#742),#889,.T.) ;
#14885 = ADVANCED_FACE('',(#1797),#220,.F.) ;
#14886 = ADVANCED_FACE('',(#1798),#221,.F.) ;
#14887 = ADVANCED_FACE('',(#1799,#743),#890,.T.) ;
#14888 = ADVANCED_FACE('',(#1800),#891,.F.) ;
#14889 = ADVANCED_FACE('',(#1801),#1252,.F.) ;
#14890 = ADVANCED_FACE('',(#1802),#892,.F.) ;
#14891 = ADVANCED_FACE('',(#1803),#1253,.F.) ;
#14892 = ADVANCED_FACE('',(#1804),#893,.T.) ;
#14893 = ADVANCED_FACE('',(#1805),#1254,.T.) ;
#14894 = ADVANCED_FACE('',(#1806,#744),#894,.T.) ;
#14895 = ADVANCED_FACE('',(#1807),#1255,.T.) ;
#14896 = ADVANCED_FACE('',(#1808),#1256,.T.) ;
#14897 = ADVANCED_FACE('',(#1809),#1257,.T.) ;
#14898 = ADVANCED_FACE('',(#1810,#745),#895,.T.) ;
#14899 = ADVANCED_FACE('',(#1811),#1258,.T.) ;
#14900 = ADVANCED_FACE('',(#1812,#746),#896,.T.) ;
#14901 = ADVANCED_FACE('',(#1813),#1259,.T.) ;
#14902 = ADVANCED_FACE('',(#1814,#747),#897,.T.) ;
#14903 = ADVANCED_FACE('',(#1815),#1260,.T.) ;
#14904 = ADVANCED_FACE('',(#1816),#898,.F.) ;
#14905 = ADVANCED_FACE('',(#1817),#1261,.T.) ;
#14906 = ADVANCED_FACE('',(#1818),#899,.F.) ;
#14907 = ADVANCED_FACE('',(#1819),#900,.T.) ;
#14908 = ADVANCED_FACE('',(#1820),#901,.F.) ;
#14909 = ADVANCED_FACE('',(#1821),#902,.F.) ;
#14910 = ADVANCED_FACE('',(#1822),#903,.F.) ;
#14911 = ADVANCED_FACE('',(#1823),#904,.F.) ;
#14912 = ADVANCED_FACE('',(#1824),#905,.F.) ;
#14913 = ADVANCED_FACE('',(#1825),#14549,.T.) ;
#14914 = ADVANCED_FACE('',(#1826,#748),#906,.F.) ;
#14915 = ADVANCED_FACE('',(#1827),#1262,.T.) ;
#14916 = ADVANCED_FACE('',(#1828),#14550,.F.) ;
#14917 = ADVANCED_FACE('',(#1829),#1263,.F.) ;
#14918 = ADVANCED_FACE('',(#1830),#14551,.T.) ;
#14919 = ADVANCED_FACE('',(#1831,#749),#907,.T.) ;
#14920 = ADVANCED_FACE('',(#1832),#14552,.F.) ;
#14921 = ADVANCED_FACE('',(#1833),#908,.F.) ;
#14922 = ADVANCED_FACE('',(#1834),#909,.F.) ;
#14923 = ADVANCED_FACE('',(#1835),#910,.F.) ;
#14924 = ADVANCED_FACE('',(#1836,#750),#911,.F.) ;
#14925 = ADVANCED_FACE('',(#1837),#1264,.T.) ;
#14926 = ADVANCED_FACE('',(#1838),#1265,.T.) ;
#14927 = ADVANCED_FACE('',(#1839),#1266,.T.) ;
#14928 = ADVANCED_FACE('',(#1840),#1267,.T.) ;
#14929 = ADVANCED_FACE('',(#1841),#1268,.T.) ;
#14930 = ADVANCED_FACE('',(#1842),#1269,.T.) ;
#14931 = ADVANCED_FACE('',(#1843),#1270,.T.) ;
#14932 = ADVANCED_FACE('',(#1844),#1271,.T.) ;
#14933 = ADVANCED_FACE('',(#1845),#1272,.T.) ;
#14934 = ADVANCED_FACE('',(#1846),#1273,.T.) ;
#14935 = ADVANCED_FACE('',(#1847),#1274,.T.) ;
#14936 = ADVANCED_FACE('',(#1848),#1275,.T.) ;
#14937 = ADVANCED_FACE('',(#1849),#1276,.T.) ;
#14938 = ADVANCED_FACE('',(#1850),#1277,.T.) ;
#14939 = ADVANCED_FACE('',(#1851),#1278,.T.) ;
#14940 = ADVANCED_FACE('',(#1852),#1279,.T.) ;
#14941 = ADVANCED_FACE('',(#1853),#1280,.T.) ;
#14942 = ADVANCED_FACE('',(#1854),#1281,.T.) ;
#14943 = ADVANCED_FACE('',(#1855),#1282,.T.) ;
#14944 = ADVANCED_FACE('',(#1856),#1283,.T.) ;
#14945 = ADVANCED_FACE('',(#1857),#1284,.T.) ;
#14946 = ADVANCED_FACE('',(#1858),#1285,.T.) ;
#14947 = ADVANCED_FACE('',(#1859),#1286,.T.) ;
#14948 = ADVANCED_FACE('',(#1860),#1287,.T.) ;
#14949 = ADVANCED_FACE('',(#1861),#1288,.T.) ;
#14950 = ADVANCED_FACE('',(#1862),#1289,.T.) ;
#14951 = ADVANCED_FACE('',(#1863),#1290,.T.) ;
#14952 = ADVANCED_FACE('',(#1864),#1291,.T.) ;
#14953 = ADVANCED_FACE('',(#1865),#1292,.T.) ;
#14954 = ADVANCED_FACE('',(#1866),#1293,.T.) ;
#14955 = ADVANCED_FACE('',(#1867),#1294,.T.) ;
#14956 = ADVANCED_FACE('',(#1868),#1295,.T.) ;
#14957 = ADVANCED_FACE('',(#1869),#1296,.T.) ;
#14958 = ADVANCED_FACE('',(#1870),#1297,.T.) ;
#14959 = ADVANCED_FACE('',(#1871),#1298,.T.) ;
#14960 = ADVANCED_FACE('',(#1872),#1299,.T.) ;
#14961 = ADVANCED_FACE('',(#1873),#1300,.T.) ;
#14962 = ADVANCED_FACE('',(#1874),#1301,.T.) ;
#14963 = ADVANCED_FACE('',(#1875),#1302,.T.) ;
#14964 = ADVANCED_FACE('',(#1876),#1303,.T.) ;
#14965 = ADVANCED_FACE('',(#1877),#1304,.T.) ;
#14966 = ADVANCED_FACE('',(#1878),#1305,.T.) ;
#14967 = ADVANCED_FACE('',(#1879),#1306,.T.) ;
#14968 = ADVANCED_FACE('',(#1880),#1307,.T.) ;
#14969 = ADVANCED_FACE('',(#1881),#1308,.T.) ;
#14970 = ADVANCED_FACE('',(#1882),#1309,.T.) ;
#14971 = ADVANCED_FACE('',(#1883),#1310,.T.) ;
#14972 = ADVANCED_FACE('',(#1884),#1311,.T.) ;
#14973 = ADVANCED_FACE('',(#1885),#1312,.T.) ;
#14974 = ADVANCED_FACE('',(#1886),#1313,.T.) ;
#14975 = ADVANCED_FACE('',(#1887),#1314,.T.) ;
#14976 = ADVANCED_FACE('',(#1888),#1315,.T.) ;
#14977 = ADVANCED_FACE('',(#1889),#1316,.T.) ;
#14978 = ADVANCED_FACE('',(#1890),#1317,.T.) ;
#14979 = ADVANCED_FACE('',(#1891),#1318,.T.) ;
#14980 = ADVANCED_FACE('',(#1892),#1319,.T.) ;
#14981 = ADVANCED_FACE('',(#1893),#1320,.T.) ;
#14982 = ADVANCED_FACE('',(#1894),#1321,.T.) ;
#14983 = ADVANCED_FACE('',(#1895),#1322,.T.) ;
#14984 = ADVANCED_FACE('',(#1896),#1323,.T.) ;
#14985 = ADVANCED_FACE('',(#1897),#1324,.T.) ;
#14986 = ADVANCED_FACE('',(#1898,#751),#912,.F.) ;
#14987 = ADVANCED_FACE('',(#1899),#14553,.F.) ;
#14988 = ADVANCED_FACE('',(#1900),#14554,.T.) ;
#14989 = ADVANCED_FACE('',(#1901),#14555,.T.) ;
#14990 = ADVANCED_FACE('',(#1902),#14556,.T.) ;
#14991 = ADVANCED_FACE('',(#1903),#14557,.T.) ;
#14992 = ADVANCED_FACE('',(#1904),#14558,.F.) ;
#14993 = ADVANCED_FACE('',(#1905,#752),#913,.F.) ;
#14994 = ADVANCED_FACE('',(#1906),#1325,.T.) ;
#14995 = ADVANCED_FACE('',(#1907,#753),#914,.F.) ;
#14996 = ADVANCED_FACE('',(#1908),#1326,.T.) ;
#14997 = ADVANCED_FACE('',(#1909,#754),#915,.F.) ;
#14998 = ADVANCED_FACE('',(#1910),#916,.T.) ;
#14999 = ADVANCED_FACE('',(#1911),#917,.F.) ;
#15000 = ADVANCED_FACE('',(#1912),#1327,.T.) ;
#15001 = ADVANCED_FACE('',(#1913),#1328,.F.) ;
#15002 = ADVANCED_FACE('',(#1914),#1329,.T.) ;
#15003 = ADVANCED_FACE('',(#1915),#918,.T.) ;
#15004 = ADVANCED_FACE('',(#1916),#919,.F.) ;
#15005 = ADVANCED_FACE('',(#1917),#1330,.T.) ;
#15006 = ADVANCED_FACE('',(#1918),#1331,.F.) ;
#15007 = ADVANCED_FACE('',(#1919),#1332,.T.) ;
#15008 = ADVANCED_FACE('',(#1920),#920,.T.) ;
#15009 = ADVANCED_FACE('',(#1921),#921,.F.) ;
#15010 = ADVANCED_FACE('',(#1922),#1333,.T.) ;
#15011 = ADVANCED_FACE('',(#1923),#1334,.F.) ;
#15012 = ADVANCED_FACE('',(#1924),#1335,.T.) ;
#15013 = ADVANCED_FACE('',(#1925),#922,.T.) ;
#15014 = ADVANCED_FACE('',(#1926),#923,.F.) ;
#15015 = ADVANCED_FACE('',(#1927),#1336,.T.) ;
#15016 = ADVANCED_FACE('',(#1928),#1337,.F.) ;
#15017 = ADVANCED_FACE('',(#1929),#1338,.T.) ;
#15018 = ADVANCED_FACE('',(#1930),#924,.T.) ;
#15019 = ADVANCED_FACE('',(#1931),#925,.F.) ;
#15020 = ADVANCED_FACE('',(#1932),#1339,.T.) ;
#15021 = ADVANCED_FACE('',(#1933),#1340,.F.) ;
#15022 = ADVANCED_FACE('',(#1934),#1341,.T.) ;
#15023 = ADVANCED_FACE('',(#1935),#926,.T.) ;
#15024 = ADVANCED_FACE('',(#1936),#927,.F.) ;
#15025 = ADVANCED_FACE('',(#1937),#1342,.T.) ;
#15026 = ADVANCED_FACE('',(#1938),#1343,.F.) ;
#15027 = ADVANCED_FACE('',(#1939),#1344,.T.) ;
#15028 = ADVANCED_FACE('',(#1940),#928,.T.) ;
#15029 = ADVANCED_FACE('',(#1941),#929,.F.) ;
#15030 = ADVANCED_FACE('',(#1942),#1345,.T.) ;
#15031 = ADVANCED_FACE('',(#1943),#1346,.F.) ;
#15032 = ADVANCED_FACE('',(#1944),#1347,.T.) ;
#15033 = ADVANCED_FACE('',(#1945),#930,.T.) ;
#15034 = ADVANCED_FACE('',(#1946),#931,.F.) ;
#15035 = ADVANCED_FACE('',(#1947),#1348,.T.) ;
#15036 = ADVANCED_FACE('',(#1948),#1349,.F.) ;
#15037 = ADVANCED_FACE('',(#1949),#1350,.T.) ;
#15038 = ADVANCED_FACE('',(#1950),#932,.T.) ;
#15039 = ADVANCED_FACE('',(#1951),#933,.F.) ;
#15040 = ADVANCED_FACE('',(#1952),#1351,.T.) ;
#15041 = ADVANCED_FACE('',(#1953),#1352,.F.) ;
#15042 = ADVANCED_FACE('',(#1954),#1353,.T.) ;
#15043 = ADVANCED_FACE('',(#1955),#934,.T.) ;
#15044 = ADVANCED_FACE('',(#1956),#935,.F.) ;
#15045 = ADVANCED_FACE('',(#1957),#1354,.T.) ;
#15046 = ADVANCED_FACE('',(#1958),#1355,.F.) ;
#15047 = ADVANCED_FACE('',(#1959),#1356,.T.) ;
#15048 = ADVANCED_FACE('',(#1960),#936,.T.) ;
#15049 = ADVANCED_FACE('',(#1961),#937,.F.) ;
#15050 = ADVANCED_FACE('',(#1962),#1357,.T.) ;
#15051 = ADVANCED_FACE('',(#1963),#1358,.F.) ;
#15052 = ADVANCED_FACE('',(#1964),#1359,.T.) ;
#15053 = ADVANCED_FACE('',(#1965),#938,.T.) ;
#15054 = ADVANCED_FACE('',(#1966),#939,.F.) ;
#15055 = ADVANCED_FACE('',(#1967),#1360,.T.) ;
#15056 = ADVANCED_FACE('',(#1968),#1361,.F.) ;
#15057 = ADVANCED_FACE('',(#1969),#1362,.T.) ;
#15058 = ADVANCED_FACE('',(#1970),#940,.T.) ;
#15059 = ADVANCED_FACE('',(#1971),#941,.F.) ;
#15060 = ADVANCED_FACE('',(#1972),#1363,.T.) ;
#15061 = ADVANCED_FACE('',(#1973),#1364,.F.) ;
#15062 = ADVANCED_FACE('',(#1974),#1365,.T.) ;
#15063 = ADVANCED_FACE('',(#1975),#942,.T.) ;
#15064 = ADVANCED_FACE('',(#1976),#943,.F.) ;
#15065 = ADVANCED_FACE('',(#1977),#1366,.T.) ;
#15066 = ADVANCED_FACE('',(#1978),#1367,.F.) ;
#15067 = ADVANCED_FACE('',(#1979),#1368,.T.) ;
#15068 = ADVANCED_FACE('',(#1980),#944,.T.) ;
#15069 = ADVANCED_FACE('',(#1981),#945,.F.) ;
#15070 = ADVANCED_FACE('',(#1982),#1369,.T.) ;
#15071 = ADVANCED_FACE('',(#1983),#1370,.F.) ;
#15072 = ADVANCED_FACE('',(#1984),#1371,.T.) ;
#15073 = ADVANCED_FACE('',(#1985),#946,.T.) ;
#15074 = ADVANCED_FACE('',(#1986),#947,.F.) ;
#15075 = ADVANCED_FACE('',(#1987),#1372,.T.) ;
#15076 = ADVANCED_FACE('',(#1988),#1373,.F.) ;
#15077 = ADVANCED_FACE('',(#1989),#1374,.T.) ;
#15078 = ADVANCED_FACE('',(#1990),#948,.T.) ;
#15079 = ADVANCED_FACE('',(#1991),#949,.F.) ;
#15080 = ADVANCED_FACE('',(#1992),#1375,.T.) ;
#15081 = ADVANCED_FACE('',(#1993),#1376,.F.) ;
#15082 = ADVANCED_FACE('',(#1994),#1377,.T.) ;
#15083 = ADVANCED_FACE('',(#1995),#950,.T.) ;
#15084 = ADVANCED_FACE('',(#1996),#951,.F.) ;
#15085 = ADVANCED_FACE('',(#1997),#1378,.T.) ;
#15086 = ADVANCED_FACE('',(#1998),#1379,.F.) ;
#15087 = ADVANCED_FACE('',(#1999),#1380,.T.) ;
#15088 = ADVANCED_FACE('',(#2000),#952,.T.) ;
#15089 = ADVANCED_FACE('',(#2001),#953,.F.) ;
#15090 = ADVANCED_FACE('',(#2002),#1381,.T.) ;
#15091 = ADVANCED_FACE('',(#2003),#1382,.F.) ;
#15092 = ADVANCED_FACE('',(#2004),#1383,.T.) ;
#15093 = ADVANCED_FACE('',(#2005),#954,.T.) ;
#15094 = ADVANCED_FACE('',(#2006),#955,.F.) ;
#15095 = ADVANCED_FACE('',(#2007),#1384,.T.) ;
#15096 = ADVANCED_FACE('',(#2008),#1385,.F.) ;
#15097 = ADVANCED_FACE('',(#2009),#1386,.T.) ;
#15098 = ADVANCED_FACE('',(#2010),#956,.T.) ;
#15099 = ADVANCED_FACE('',(#2011),#957,.F.) ;
#15100 = ADVANCED_FACE('',(#2012),#1387,.T.) ;
#15101 = ADVANCED_FACE('',(#2013),#1388,.F.) ;
#15102 = ADVANCED_FACE('',(#2014),#1389,.T.) ;
#15103 = ADVANCED_FACE('',(#2015),#958,.T.) ;
#15104 = ADVANCED_FACE('',(#2016),#959,.F.) ;
#15105 = ADVANCED_FACE('',(#2017),#1390,.T.) ;
#15106 = ADVANCED_FACE('',(#2018),#1391,.F.) ;
#15107 = ADVANCED_FACE('',(#2019),#1392,.T.) ;
#15108 = ADVANCED_FACE('',(#2020),#960,.T.) ;
#15109 = ADVANCED_FACE('',(#2021),#961,.F.) ;
#15110 = ADVANCED_FACE('',(#2022),#1393,.T.) ;
#15111 = ADVANCED_FACE('',(#2023),#1394,.F.) ;
#15112 = ADVANCED_FACE('',(#2024),#1395,.T.) ;
#15113 = ADVANCED_FACE('',(#2025),#962,.T.) ;
#15114 = ADVANCED_FACE('',(#2026),#963,.F.) ;
#15115 = ADVANCED_FACE('',(#2027),#1396,.T.) ;
#15116 = ADVANCED_FACE('',(#2028),#1397,.F.) ;
#15117 = ADVANCED_FACE('',(#2029),#1398,.T.) ;
#15118 = ADVANCED_FACE('',(#2030),#964,.T.) ;
#15119 = ADVANCED_FACE('',(#2031),#965,.F.) ;
#15120 = ADVANCED_FACE('',(#2032),#1399,.T.) ;
#15121 = ADVANCED_FACE('',(#2033),#1400,.F.) ;
#15122 = ADVANCED_FACE('',(#2034),#1401,.T.) ;
#15123 = ADVANCED_FACE('',(#2035),#966,.T.) ;
#15124 = ADVANCED_FACE('',(#2036),#967,.F.) ;
#15125 = ADVANCED_FACE('',(#2037),#1402,.T.) ;
#15126 = ADVANCED_FACE('',(#2038),#1403,.F.) ;
#15127 = ADVANCED_FACE('',(#2039),#1404,.T.) ;
#15128 = ADVANCED_FACE('',(#2040),#968,.T.) ;
#15129 = ADVANCED_FACE('',(#2041),#969,.F.) ;
#15130 = ADVANCED_FACE('',(#2042),#1405,.T.) ;
#15131 = ADVANCED_FACE('',(#2043),#1406,.F.) ;
#15132 = ADVANCED_FACE('',(#2044),#1407,.T.) ;
#15133 = ADVANCED_FACE('',(#2045),#970,.T.) ;
#15134 = ADVANCED_FACE('',(#2046),#971,.F.) ;
#15135 = ADVANCED_FACE('',(#2047),#1408,.T.) ;
#15136 = ADVANCED_FACE('',(#2048),#1409,.F.) ;
#15137 = ADVANCED_FACE('',(#2049),#1410,.T.) ;
#15138 = ADVANCED_FACE('',(#2050),#972,.T.) ;
#15139 = ADVANCED_FACE('',(#2051),#973,.F.) ;
#15140 = ADVANCED_FACE('',(#2052),#1411,.T.) ;
#15141 = ADVANCED_FACE('',(#2053),#1412,.F.) ;
#15142 = ADVANCED_FACE('',(#2054),#1413,.T.) ;
#15143 = ADVANCED_FACE('',(#2055),#974,.T.) ;
#15144 = ADVANCED_FACE('',(#2056),#975,.F.) ;
#15145 = ADVANCED_FACE('',(#2057),#1414,.T.) ;
#15146 = ADVANCED_FACE('',(#2058),#1415,.F.) ;
#15147 = ADVANCED_FACE('',(#2059),#1416,.T.) ;
#15148 = ADVANCED_FACE('',(#2060),#976,.T.) ;
#15149 = ADVANCED_FACE('',(#2061),#977,.F.) ;
#15150 = ADVANCED_FACE('',(#2062),#1417,.T.) ;
#15151 = ADVANCED_FACE('',(#2063),#1418,.F.) ;
#15152 = ADVANCED_FACE('',(#2064),#1419,.T.) ;
#15153 = ADVANCED_FACE('',(#2065),#978,.T.) ;
#15154 = ADVANCED_FACE('',(#2066),#979,.F.) ;
#15155 = ADVANCED_FACE('',(#2067),#1420,.T.) ;
#15156 = ADVANCED_FACE('',(#2068),#1421,.F.) ;
#15157 = ADVANCED_FACE('',(#2069),#1422,.T.) ;
#15158 = ADVANCED_FACE('',(#2070),#980,.T.) ;
#15159 = ADVANCED_FACE('',(#2071),#981,.F.) ;
#15160 = ADVANCED_FACE('',(#2072),#1423,.T.) ;
#15161 = ADVANCED_FACE('',(#2073),#1424,.F.) ;
#15162 = ADVANCED_FACE('',(#2074),#1425,.T.) ;
#15163 = ADVANCED_FACE('',(#2075),#982,.T.) ;
#15164 = ADVANCED_FACE('',(#2076),#983,.F.) ;
#15165 = ADVANCED_FACE('',(#2077),#1426,.T.) ;
#15166 = ADVANCED_FACE('',(#2078),#1427,.F.) ;
#15167 = ADVANCED_FACE('',(#2079),#1428,.T.) ;
#15168 = ADVANCED_FACE('',(#2080),#984,.T.) ;
#15169 = ADVANCED_FACE('',(#2081),#985,.F.) ;
#15170 = ADVANCED_FACE('',(#2082),#1429,.T.) ;
#15171 = ADVANCED_FACE('',(#2083),#1430,.F.) ;
#15172 = ADVANCED_FACE('',(#2084),#1431,.T.) ;
#15173 = ADVANCED_FACE('',(#2085),#986,.T.) ;
#15174 = ADVANCED_FACE('',(#2086),#987,.F.) ;
#15175 = ADVANCED_FACE('',(#2087),#1432,.T.) ;
#15176 = ADVANCED_FACE('',(#2088),#1433,.F.) ;
#15177 = ADVANCED_FACE('',(#2089),#1434,.T.) ;
#15178 = ADVANCED_FACE('',(#2090),#988,.T.) ;
#15179 = ADVANCED_FACE('',(#2091),#989,.F.) ;
#15180 = ADVANCED_FACE('',(#2092),#1435,.T.) ;
#15181 = ADVANCED_FACE('',(#2093),#1436,.F.) ;
#15182 = ADVANCED_FACE('',(#2094),#1437,.T.) ;
#15183 = ADVANCED_FACE('',(#2095),#990,.T.) ;
#15184 = ADVANCED_FACE('',(#2096),#991,.F.) ;
#15185 = ADVANCED_FACE('',(#2097),#1438,.T.) ;
#15186 = ADVANCED_FACE('',(#2098),#1439,.F.) ;
#15187 = ADVANCED_FACE('',(#2099),#1440,.T.) ;
#15188 = ADVANCED_FACE('',(#2100),#992,.T.) ;
#15189 = ADVANCED_FACE('',(#2101),#993,.F.) ;
#15190 = ADVANCED_FACE('',(#2102),#1441,.T.) ;
#15191 = ADVANCED_FACE('',(#2103),#1442,.F.) ;
#15192 = ADVANCED_FACE('',(#2104),#1443,.T.) ;
#15193 = ADVANCED_FACE('',(#2105),#994,.T.) ;
#15194 = ADVANCED_FACE('',(#2106),#995,.F.) ;
#15195 = ADVANCED_FACE('',(#2107),#1444,.T.) ;
#15196 = ADVANCED_FACE('',(#2108),#1445,.F.) ;
#15197 = ADVANCED_FACE('',(#2109),#1446,.T.) ;
#15198 = ADVANCED_FACE('',(#2110),#996,.T.) ;
#15199 = ADVANCED_FACE('',(#2111),#997,.F.) ;
#15200 = ADVANCED_FACE('',(#2112),#1447,.T.) ;
#15201 = ADVANCED_FACE('',(#2113),#1448,.F.) ;
#15202 = ADVANCED_FACE('',(#2114),#1449,.T.) ;
#15203 = ADVANCED_FACE('',(#2115),#998,.T.) ;
#15204 = ADVANCED_FACE('',(#2116),#999,.F.) ;
#15205 = ADVANCED_FACE('',(#2117),#1450,.T.) ;
#15206 = ADVANCED_FACE('',(#2118),#1451,.F.) ;
#15207 = ADVANCED_FACE('',(#2119),#1452,.T.) ;
#15208 = ADVANCED_FACE('',(#2120),#1000,.T.) ;
#15209 = ADVANCED_FACE('',(#2121),#1001,.F.) ;
#15210 = ADVANCED_FACE('',(#2122),#1453,.T.) ;
#15211 = ADVANCED_FACE('',(#2123),#1454,.F.) ;
#15212 = ADVANCED_FACE('',(#2124),#1455,.T.) ;
#15213 = ADVANCED_FACE('',(#2125),#1002,.T.) ;
#15214 = ADVANCED_FACE('',(#2126),#1003,.F.) ;
#15215 = ADVANCED_FACE('',(#2127),#1456,.T.) ;
#15216 = ADVANCED_FACE('',(#2128),#1457,.F.) ;
#15217 = ADVANCED_FACE('',(#2129),#1458,.T.) ;
#15218 = ADVANCED_FACE('',(#2130),#1004,.T.) ;
#15219 = ADVANCED_FACE('',(#2131),#1005,.F.) ;
#15220 = ADVANCED_FACE('',(#2132),#1459,.T.) ;
#15221 = ADVANCED_FACE('',(#2133),#1460,.F.) ;
#15222 = ADVANCED_FACE('',(#2134),#1461,.T.) ;
#15223 = ADVANCED_FACE('',(#2135),#1006,.T.) ;
#15224 = ADVANCED_FACE('',(#2136),#1007,.F.) ;
#15225 = ADVANCED_FACE('',(#2137),#1462,.T.) ;
#15226 = ADVANCED_FACE('',(#2138),#1463,.F.) ;
#15227 = ADVANCED_FACE('',(#2139),#1464,.T.) ;
#15228 = ADVANCED_FACE('',(#2140),#1008,.T.) ;
#15229 = ADVANCED_FACE('',(#2141),#1009,.F.) ;
#15230 = ADVANCED_FACE('',(#2142),#1465,.T.) ;
#15231 = ADVANCED_FACE('',(#2143),#1466,.F.) ;
#15232 = ADVANCED_FACE('',(#2144),#1467,.T.) ;
#15233 = ADVANCED_FACE('',(#2145),#1010,.T.) ;
#15234 = ADVANCED_FACE('',(#2146),#1011,.F.) ;
#15235 = ADVANCED_FACE('',(#2147),#1468,.T.) ;
#15236 = ADVANCED_FACE('',(#2148),#1469,.F.) ;
#15237 = ADVANCED_FACE('',(#2149),#1470,.T.) ;
#15238 = ADVANCED_FACE('',(#2150),#1012,.T.) ;
#15239 = ADVANCED_FACE('',(#2151),#1013,.F.) ;
#15240 = ADVANCED_FACE('',(#2152),#1471,.T.) ;
#15241 = ADVANCED_FACE('',(#2153),#1472,.F.) ;
#15242 = ADVANCED_FACE('',(#2154),#1473,.T.) ;
#15243 = ADVANCED_FACE('',(#2155),#1014,.T.) ;
#15244 = ADVANCED_FACE('',(#2156),#1015,.F.) ;
#15245 = ADVANCED_FACE('',(#2157),#1474,.T.) ;
#15246 = ADVANCED_FACE('',(#2158),#1475,.F.) ;
#15247 = ADVANCED_FACE('',(#2159),#1476,.T.) ;
#15248 = ADVANCED_FACE('',(#2160),#1016,.T.) ;
#15249 = ADVANCED_FACE('',(#2161),#1017,.F.) ;
#15250 = ADVANCED_FACE('',(#2162),#1477,.T.) ;
#15251 = ADVANCED_FACE('',(#2163),#1478,.F.) ;
#15252 = ADVANCED_FACE('',(#2164),#1479,.T.) ;
#15253 = ADVANCED_FACE('',(#2165),#1018,.T.) ;
#15254 = ADVANCED_FACE('',(#2166),#1019,.F.) ;
#15255 = ADVANCED_FACE('',(#2167),#1480,.T.) ;
#15256 = ADVANCED_FACE('',(#2168),#1481,.F.) ;
#15257 = ADVANCED_FACE('',(#2169),#1482,.T.) ;
#15258 = ADVANCED_FACE('',(#2170),#1020,.T.) ;
#15259 = ADVANCED_FACE('',(#2171),#1021,.F.) ;
#15260 = ADVANCED_FACE('',(#2172),#1483,.T.) ;
#15261 = ADVANCED_FACE('',(#2173),#1484,.F.) ;
#15262 = ADVANCED_FACE('',(#2174),#1485,.T.) ;
#15263 = ADVANCED_FACE('',(#2175),#1022,.T.) ;
#15264 = ADVANCED_FACE('',(#2176),#1023,.F.) ;
#15265 = ADVANCED_FACE('',(#2177),#1486,.T.) ;
#15266 = ADVANCED_FACE('',(#2178),#1487,.F.) ;
#15267 = ADVANCED_FACE('',(#2179),#1488,.T.) ;
#15268 = ADVANCED_FACE('',(#2180),#1024,.T.) ;
#15269 = ADVANCED_FACE('',(#2181),#1025,.F.) ;
#15270 = ADVANCED_FACE('',(#2182),#1489,.T.) ;
#15271 = ADVANCED_FACE('',(#2183),#1490,.F.) ;
#15272 = ADVANCED_FACE('',(#2184),#1491,.T.) ;
#15273 = ADVANCED_FACE('',(#2185),#1026,.T.) ;
#15274 = ADVANCED_FACE('',(#2186),#1027,.F.) ;
#15275 = ADVANCED_FACE('',(#2187),#1492,.T.) ;
#15276 = ADVANCED_FACE('',(#2188),#1493,.F.) ;
#15277 = ADVANCED_FACE('',(#2189),#1494,.T.) ;
#15278 = ADVANCED_FACE('',(#2190),#1028,.T.) ;
#15279 = ADVANCED_FACE('',(#2191),#1029,.F.) ;
#15280 = ADVANCED_FACE('',(#2192),#1495,.T.) ;
#15281 = ADVANCED_FACE('',(#2193),#1496,.F.) ;
#15282 = ADVANCED_FACE('',(#2194),#1497,.T.) ;
#15283 = ADVANCED_FACE('',(#2195),#1030,.T.) ;
#15284 = ADVANCED_FACE('',(#2196),#1031,.F.) ;
#15285 = ADVANCED_FACE('',(#2197),#1498,.T.) ;
#15286 = ADVANCED_FACE('',(#2198),#1499,.F.) ;
#15287 = ADVANCED_FACE('',(#2199),#1500,.T.) ;
#15288 = ADVANCED_FACE('',(#2200),#1032,.T.) ;
#15289 = ADVANCED_FACE('',(#2201),#1033,.F.) ;
#15290 = ADVANCED_FACE('',(#2202),#1501,.T.) ;
#15291 = ADVANCED_FACE('',(#2203),#1502,.F.) ;
#15292 = ADVANCED_FACE('',(#2204),#1503,.T.) ;
#15293 = ADVANCED_FACE('',(#2205),#1034,.T.) ;
#15294 = ADVANCED_FACE('',(#2206),#1035,.F.) ;
#15295 = ADVANCED_FACE('',(#2207),#1504,.T.) ;
#15296 = ADVANCED_FACE('',(#2208),#1505,.F.) ;
#15297 = ADVANCED_FACE('',(#2209),#1506,.T.) ;
#15298 = ADVANCED_FACE('',(#2210),#1507,.F.) ;
#15299 = ADVANCED_FACE('',(#2211),#1508,.F.) ;
#15300 = ADVANCED_FACE('',(#2212),#14559,.F.) ;
#15301 = ADVANCED_FACE('',(#2213,#755),#1036,.T.) ;
#15302 = ADVANCED_FACE('',(#2214),#14560,.T.) ;
#15303 = ADVANCED_FACE('',(#2215),#1509,.T.) ;
#15304 = ADVANCED_FACE('',(#2216),#14561,.T.) ;
#15305 = ADVANCED_FACE('',(#2217,#756),#1037,.T.) ;
#15306 = ADVANCED_FACE('',(#2218),#14562,.F.) ;
#15307 = ADVANCED_FACE('',(#2219),#1038,.F.) ;
#15308 = ADVANCED_FACE('',(#2220),#1039,.F.) ;
#15309 = ADVANCED_FACE('',(#2221),#1510,.T.) ;
#15310 = ADVANCED_FACE('',(#2222,#757),#1040,.F.) ;
#15311 = ADVANCED_FACE('',(#2223),#1511,.T.) ;
#15312 = ADVANCED_FACE('',(#2224),#14563,.T.) ;
#15313 = ADVANCED_FACE('',(#2225),#1041,.F.) ;
#15314 = ADVANCED_FACE('',(#2226),#1042,.F.) ;
#15315 = ADVANCED_FACE('',(#2227),#1512,.T.) ;
#15316 = ADVANCED_FACE('',(#2228),#1513,.T.) ;
#15317 = ADVANCED_FACE('',(#2229),#14564,.T.) ;
#15318 = ADVANCED_FACE('',(#2230),#1043,.F.) ;
#15319 = ADVANCED_FACE('',(#2231),#1044,.F.) ;
#15320 = ADVANCED_FACE('',(#2232),#1514,.T.) ;
#15321 = ADVANCED_FACE('',(#2233),#1515,.T.) ;
#15322 = ADVANCED_FACE('',(#2234),#14565,.T.) ;
#15323 = ADVANCED_FACE('',(#2235),#1045,.F.) ;
#15324 = ADVANCED_FACE('',(#2236),#1046,.F.) ;
#15325 = ADVANCED_FACE('',(#2237),#1516,.T.) ;
#15326 = ADVANCED_FACE('',(#2238),#14566,.T.) ;
#15327 = ADVANCED_FACE('',(#2239),#1517,.T.) ;
#15328 = ADVANCED_FACE('',(#2240,#758),#1047,.T.) ;
#15329 = ADVANCED_FACE('',(#2241),#1518,.F.) ;
#15330 = ADVANCED_FACE('',(#2242),#14567,.F.) ;
#15331 = ADVANCED_FACE('',(#2243,#759,#760),#14568,.T.) ;
#15332 = ADVANCED_FACE('',(#2244),#1519,.T.) ;
#15333 = ADVANCED_FACE('',(#2245,#761,#762,#763,#764,#765,#766,#767,#768,
#769,#770,#771,#772,#773,#774,#775,#776,#777,#778,#779,#780,#781,#782,#783,
#784,#785,#786,#787,#788,#789),#14569,.F.) ;
#15334 = ADVANCED_FACE('',(#2246),#1520,.T.) ;
#15335 = ADVANCED_FACE('',(#2247),#79,.T.) ;
#15336 = ADVANCED_FACE('',(#2248),#80,.T.) ;
#15337 = ADVANCED_FACE('',(#2249),#81,.T.) ;
#15338 = ADVANCED_FACE('',(#2250),#1521,.F.) ;
#15339 = ADVANCED_FACE('',(#2251),#82,.T.) ;
#15340 = ADVANCED_FACE('',(#2252),#1522,.T.) ;
#15341 = ADVANCED_FACE('',(#2253,#790),#1048,.T.) ;
#15342 = ADVANCED_FACE('',(#2254,#791),#1049,.T.) ;
#15343 = ADVANCED_FACE('',(#2255,#792),#1050,.T.) ;
#15344 = ADVANCED_FACE('',(#2256),#1051,.T.) ;
#15345 = ADVANCED_FACE('',(#2257),#1052,.T.) ;
#15346 = ADVANCED_FACE('',(#2258),#1053,.T.) ;
#15347 = ADVANCED_FACE('',(#2259),#1054,.T.) ;
#15348 = ADVANCED_FACE('',(#2260),#1055,.T.) ;
#15349 = ADVANCED_FACE('',(#2261),#1056,.T.) ;
#15350 = ADVANCED_FACE('',(#2262),#1057,.T.) ;
#15351 = ADVANCED_FACE('',(#2263),#1058,.T.) ;
#15352 = ADVANCED_FACE('',(#2264),#1059,.T.) ;
#15353 = ADVANCED_FACE('',(#2265),#1060,.T.) ;
#15354 = ADVANCED_FACE('',(#2266),#1061,.T.) ;
#15355 = ADVANCED_FACE('',(#2267),#1062,.T.) ;
#15356 = ADVANCED_FACE('',(#2268),#1063,.T.) ;
#15357 = ADVANCED_FACE('',(#2269),#1064,.T.) ;
#15358 = ADVANCED_FACE('',(#2270),#1065,.T.) ;
#15359 = ADVANCED_FACE('',(#2271),#1066,.T.) ;
#15360 = ADVANCED_FACE('',(#2272),#1067,.T.) ;
#15361 = ADVANCED_FACE('',(#2273),#1068,.T.) ;
#15362 = ADVANCED_FACE('',(#2274),#1069,.T.) ;
#15363 = ADVANCED_FACE('',(#2275),#1070,.T.) ;
#15364 = ADVANCED_FACE('',(#2276),#1071,.T.) ;
#15365 = ADVANCED_FACE('',(#2277),#1072,.T.) ;
#15366 = ADVANCED_FACE('',(#2278),#1073,.T.) ;
#15367 = ADVANCED_FACE('',(#2279),#1074,.T.) ;
#15368 = ADVANCED_FACE('',(#2280),#1075,.T.) ;
#15369 = ADVANCED_FACE('',(#2281),#1076,.T.) ;
#15370 = ADVANCED_FACE('',(#2282),#1077,.T.) ;
#15371 = ADVANCED_FACE('',(#2283),#1078,.T.) ;
#15372 = ADVANCED_FACE('',(#2284,#793),#1079,.T.) ;
#15373 = ADVANCED_FACE('',(#2285),#1080,.T.) ;
#15374 = ADVANCED_FACE('',(#2286),#14570,.T.) ;
#15375 = ADVANCED_FACE('',(#2287),#14571,.T.) ;
#15376 = ADVANCED_FACE('',(#2288),#1081,.T.) ;
#15377 = ADVANCED_FACE('',(#2289),#14572,.T.) ;
#15378 = ADVANCED_FACE('',(#2290),#14573,.T.) ;
#15379 = ADVANCED_FACE('',(#2291),#1082,.T.) ;
#15380 = ADVANCED_FACE('',(#2292),#14574,.T.) ;
#15381 = ADVANCED_FACE('',(#2293),#14575,.T.) ;
#15382 = ADVANCED_FACE('',(#2294),#1083,.T.) ;
#15383 = ADVANCED_FACE('',(#2295),#14576,.T.) ;
#15384 = ADVANCED_FACE('',(#2296),#14577,.T.) ;
#15385 = ADVANCED_FACE('',(#2297),#1084,.T.) ;
#15386 = ADVANCED_FACE('',(#2298),#14578,.T.) ;
#15387 = ADVANCED_FACE('',(#2299),#14579,.T.) ;
#15388 = ADVANCED_FACE('',(#2300),#1085,.T.) ;
#15389 = ADVANCED_FACE('',(#2301),#14580,.T.) ;
#15390 = ADVANCED_FACE('',(#2302),#14581,.T.) ;
#15391 = ADVANCED_FACE('',(#2303),#1086,.T.) ;
#15392 = ADVANCED_FACE('',(#2304),#14582,.T.) ;
#15393 = ADVANCED_FACE('',(#2305),#14583,.T.) ;
#15394 = ADVANCED_FACE('',(#2306),#1087,.T.) ;
#15395 = ADVANCED_FACE('',(#2307),#14584,.T.) ;
#15396 = ADVANCED_FACE('',(#2308),#14585,.T.) ;
#15397 = ADVANCED_FACE('',(#2309),#1088,.T.) ;
#15398 = ADVANCED_FACE('',(#2310),#14586,.T.) ;
#15399 = ADVANCED_FACE('',(#2311),#14587,.T.) ;
#15400 = ADVANCED_FACE('',(#2312),#1089,.T.) ;
#15401 = ADVANCED_FACE('',(#2313),#14588,.T.) ;
#15402 = ADVANCED_FACE('',(#2314),#14589,.T.) ;
#15403 = ADVANCED_FACE('',(#2315),#1090,.T.) ;
#15404 = ADVANCED_FACE('',(#2316),#14590,.T.) ;
#15405 = ADVANCED_FACE('',(#2317),#14591,.T.) ;
#15406 = ADVANCED_FACE('',(#2318),#1091,.T.) ;
#15407 = ADVANCED_FACE('',(#2319),#14592,.T.) ;
#15408 = ADVANCED_FACE('',(#2320),#14593,.T.) ;
#15409 = ADVANCED_FACE('',(#2321),#1092,.T.) ;
#15410 = ADVANCED_FACE('',(#2322),#14594,.T.) ;
#15411 = ADVANCED_FACE('',(#2323),#14595,.T.) ;
#15412 = ADVANCED_FACE('',(#2324),#1093,.T.) ;
#15413 = ADVANCED_FACE('',(#2325),#14596,.T.) ;
#15414 = ADVANCED_FACE('',(#2326),#14597,.T.) ;
#15415 = ADVANCED_FACE('',(#2327),#1094,.T.) ;
#15416 = ADVANCED_FACE('',(#2328),#14598,.T.) ;
#15417 = ADVANCED_FACE('',(#2329),#14599,.T.) ;
#15418 = ADVANCED_FACE('',(#2330),#1095,.T.) ;
#15419 = ADVANCED_FACE('',(#2331),#14600,.T.) ;
#15420 = ADVANCED_FACE('',(#2332),#14601,.T.) ;
#15421 = ADVANCED_FACE('',(#2333),#1096,.T.) ;
#15422 = ADVANCED_FACE('',(#2334),#14602,.T.) ;
#15423 = ADVANCED_FACE('',(#2335),#14603,.T.) ;
#15424 = ADVANCED_FACE('',(#2336),#1097,.T.) ;
#15425 = ADVANCED_FACE('',(#2337),#14604,.T.) ;
#15426 = ADVANCED_FACE('',(#2338),#14605,.T.) ;
#15427 = ADVANCED_FACE('',(#2339),#1098,.T.) ;
#15428 = ADVANCED_FACE('',(#2340),#14606,.T.) ;
#15429 = ADVANCED_FACE('',(#2341),#14607,.T.) ;
#15430 = ADVANCED_FACE('',(#2342),#1099,.T.) ;
#15431 = ADVANCED_FACE('',(#2343),#14608,.T.) ;
#15432 = ADVANCED_FACE('',(#2344),#14609,.T.) ;
#15433 = ADVANCED_FACE('',(#2345),#1100,.T.) ;
#15434 = ADVANCED_FACE('',(#2346),#14610,.T.) ;
#15435 = ADVANCED_FACE('',(#2347),#14611,.T.) ;
#15436 = ADVANCED_FACE('',(#2348),#1101,.T.) ;
#15437 = ADVANCED_FACE('',(#2349),#14612,.T.) ;
#15438 = ADVANCED_FACE('',(#2350),#14613,.T.) ;
#15439 = ADVANCED_FACE('',(#2351),#1102,.T.) ;
#15440 = ADVANCED_FACE('',(#2352),#14614,.T.) ;
#15441 = ADVANCED_FACE('',(#2353),#14615,.T.) ;
#15442 = ADVANCED_FACE('',(#2354),#1103,.T.) ;
#15443 = ADVANCED_FACE('',(#2355),#14616,.T.) ;
#15444 = ADVANCED_FACE('',(#2356),#14617,.T.) ;
#15445 = ADVANCED_FACE('',(#2357),#1104,.T.) ;
#15446 = ADVANCED_FACE('',(#2358),#14618,.T.) ;
#15447 = ADVANCED_FACE('',(#2359),#14619,.T.) ;
#15448 = ADVANCED_FACE('',(#2360),#1105,.T.) ;
#15449 = ADVANCED_FACE('',(#2361),#14620,.T.) ;
#15450 = ADVANCED_FACE('',(#2362),#14621,.T.) ;
#15451 = ADVANCED_FACE('',(#2363),#1106,.T.) ;
#15452 = ADVANCED_FACE('',(#2364),#14622,.T.) ;
#15453 = ADVANCED_FACE('',(#2365),#14623,.T.) ;
#15454 = ADVANCED_FACE('',(#2366),#1107,.T.) ;
#15455 = ADVANCED_FACE('',(#2367),#14624,.T.) ;
#15456 = ADVANCED_FACE('',(#2368),#14625,.T.) ;
#15457 = ADVANCED_FACE('',(#2369),#1108,.T.) ;
#15458 = ADVANCED_FACE('',(#2370),#14626,.T.) ;
#15459 = ADVANCED_FACE('',(#2371),#14627,.T.) ;
#15460 = ADVANCED_FACE('',(#2372),#1109,.T.) ;
#15461 = ADVANCED_FACE('',(#2373),#14628,.T.) ;
#15462 = ADVANCED_FACE('',(#2374),#14629,.T.) ;
#15463 = ADVANCED_FACE('',(#2375,#794),#1110,.F.) ;
#15464 = ADVANCED_FACE('',(#2376),#1523,.T.) ;
#15465 = ADVANCED_FACE('',(#2377),#14630,.F.) ;
#15466 = ADVANCED_FACE('',(#2378),#1524,.F.) ;
#15467 = ADVANCED_FACE('',(#2379),#14631,.T.) ;
#15468 = ADVANCED_FACE('',(#2380,#795),#1111,.T.) ;
#15469 = ADVANCED_FACE('',(#2381),#14632,.F.) ;
#15470 = ADVANCED_FACE('',(#2382),#1525,.F.) ;
#15471 = ADVANCED_FACE('',(#2383),#1526,.F.) ;
#15472 = ADVANCED_FACE('',(#2384),#1527,.F.) ;
#15473 = ADVANCED_FACE('',(#2385),#1528,.F.) ;
#15474 = ADVANCED_FACE('',(#2386),#1529,.F.) ;
#15475 = ADVANCED_FACE('',(#2387),#1530,.F.) ;
#15476 = ADVANCED_FACE('',(#2388),#1531,.F.) ;
#15477 = ADVANCED_FACE('',(#2389),#1532,.F.) ;
#15478 = ADVANCED_FACE('',(#2390),#1533,.F.) ;
#15479 = ADVANCED_FACE('',(#2391),#1534,.T.) ;
#15480 = ADVANCED_FACE('',(#2392,#796,#797,#798,#799,#800,#801,#802,#803,
#804),#1112,.F.) ;
#15481 = ADVANCED_FACE('',(#2393,#805,#806,#807,#808,#809,#810,#811,#812,
#813),#1113,.T.) ;
#15482 = ADVANCED_FACE('',(#2394),#1535,.F.) ;
#15483 = ADVANCED_FACE('',(#2395),#1536,.F.) ;
#15484 = ADVANCED_FACE('',(#2396),#1537,.F.) ;
#15485 = ADVANCED_FACE('',(#2397),#1538,.F.) ;
#15486 = ADVANCED_FACE('',(#2398),#1539,.F.) ;
#15487 = ADVANCED_FACE('',(#2399),#1540,.F.) ;
#15488 = ADVANCED_FACE('',(#2400),#1541,.F.) ;
#15489 = ADVANCED_FACE('',(#2401),#1542,.F.) ;
#15490 = ADVANCED_FACE('',(#2402),#1543,.F.) ;
#15491 = ADVANCED_FACE('',(#2403),#1544,.T.) ;
#15492 = ADVANCED_FACE('',(#2404,#814,#815,#816,#817,#818,#819,#820,#821,
#822),#1114,.T.) ;
#15493 = ADVANCED_FACE('',(#2405,#823,#824,#825,#826,#827,#828,#829,#830,
#831),#1115,.F.) ;
#15494 = CLOSED_SHELL('',(#14633,#14634,#14635,#14636,#14637,#14638,#14639,
#14640,#14641,#14642,#14643,#14644,#14645,#14646,#14647,#14648,#14649,#14650,
#14651,#14652,#14653,#14654,#14655,#14656,#14657,#14658,#14659,#14660,#14661,
#14662,#14663,#14664,#14665,#14666,#14667,#14668,#14669,#14670,#14671,#14672,
#14673,#14674,#14675)) ;
#15495 = CLOSED_SHELL('',(#14676,#14677,#14678,#14679,#14680,#14681,#14682,
#14683,#14684,#14685,#14686,#14687,#14688,#14689,#14690,#14691,#14692,#14693,
#14694,#14695,#14696,#14697,#14698,#14699,#14700,#14701,#14702,#14703,#14704,
#14705,#14706,#14707,#14708,#14709,#14710,#14711,#14712,#14713,#14714,#14715,
#14716,#14717)) ;
#15496 = CLOSED_SHELL('',(#14718,#14719,#14720,#14721,#14722,#14723,#14724,
#14725,#14726,#14727,#14728,#14729,#14730,#14731,#14732,#14733,#14734,#14735,
#14736,#14737,#14738,#14739)) ;
#15497 = CLOSED_SHELL('',(#14740,#14741,#14742,#14743,#14744,#14745,#14746,
#14747,#14748,#14749,#14750,#14751,#14752,#14753,#14754,#14755,#14756,#14757,
#14758,#14759,#14760,#14761,#14762,#14763,#14764,#14765,#14766,#14767,#14768,
#14769,#14770,#14771,#14772,#14773,#14774,#14775,#14776,#14777,#14778,#14779,
#14780,#14781,#14782,#14783,#14784,#14785,#14786)) ;
#15498 = CLOSED_SHELL('',(#14787,#14788,#14789,#14790,#14791,#14792,#14793,
#14794,#14795,#14796,#14797,#14798,#14799,#14800,#14801,#14802,#14803,#14804,
#14805,#14806,#14807,#14808)) ;
#15499 = CLOSED_SHELL('',(#14809,#14810,#14811,#14812,#14813,#14814,#14815,
#14816,#14817,#14818,#14819,#14820,#14821,#14822,#14823,#14824,#14825,#14826,
#14827,#14828,#14829,#14830,#14831,#14832,#14833,#14834,#14835,#14836,#14837,
#14838,#14839,#14840,#14841,#14842,#14843,#14844,#14845,#14846,#14847,#14848,
#14849,#14850,#14851,#14852,#14853,#14854,#14855,#14856,#14857,#14858,#14859,
#14860,#14861,#14862,#14863,#14864,#14865,#14866,#14867,#14868,#14869,#14870,
#14871,#14872,#14873,#14874,#14875,#14876,#14877,#14878,#14879,#14880,#14881,
#14882,#14883,#14884,#14885,#14886,#14887,#14888,#14889,#14890,#14891,#14892,
#14893,#14894,#14895,#14896,#14897,#14898,#14899,#14900,#14901,#14902)) ;
#15500 = CLOSED_SHELL('',(#14903,#14904,#14905,#14906,#14907,#14908,#14909,
#14910,#14911,#14912)) ;
#15501 = CLOSED_SHELL('',(#14913,#14914,#14915,#14916,#14917,#14918,#14919,
#14920)) ;
#15502 = CLOSED_SHELL('',(#14921,#14922,#14923,#14924,#14925,#14926,#14927,
#14928,#14929,#14930,#14931,#14932,#14933,#14934,#14935,#14936,#14937,#14938,
#14939,#14940,#14941,#14942,#14943,#14944,#14945,#14946,#14947,#14948,#14949,
#14950,#14951,#14952,#14953,#14954,#14955,#14956,#14957,#14958,#14959,#14960,
#14961,#14962,#14963,#14964,#14965,#14966,#14967,#14968,#14969,#14970,#14971,
#14972,#14973,#14974,#14975,#14976,#14977,#14978,#14979,#14980,#14981,#14982,
#14983,#14984,#14985,#14986,#14987,#14988,#14989,#14990,#14991,#14992,#14993,
#14994,#14995,#14996,#14997,#14998,#14999,#15000,#15001,#15002,#15003,#15004,
#15005,#15006,#15007,#15008,#15009,#15010,#15011,#15012,#15013,#15014,#15015,
#15016,#15017,#15018,#15019,#15020,#15021,#15022,#15023,#15024,#15025,#15026,
#15027,#15028,#15029,#15030,#15031,#15032,#15033,#15034,#15035,#15036,#15037,
#15038,#15039,#15040,#15041,#15042,#15043,#15044,#15045,#15046,#15047,#15048,
#15049,#15050,#15051,#15052,#15053,#15054,#15055,#15056,#15057,#15058,#15059,
#15060,#15061,#15062,#15063,#15064,#15065,#15066,#15067,#15068,#15069,#15070,
#15071,#15072,#15073,#15074,#15075,#15076,#15077,#15078,#15079,#15080,#15081,
#15082,#15083,#15084,#15085,#15086,#15087,#15088,#15089,#15090,#15091,#15092,
#15093,#15094,#15095,#15096,#15097,#15098,#15099,#15100,#15101,#15102,#15103,
#15104,#15105,#15106,#15107,#15108,#15109,#15110,#15111,#15112,#15113,#15114,
#15115,#15116,#15117,#15118,#15119,#15120,#15121,#15122,#15123,#15124,#15125,
#15126,#15127,#15128,#15129,#15130,#15131,#15132,#15133,#15134,#15135,#15136,
#15137,#15138,#15139,#15140,#15141,#15142,#15143,#15144,#15145,#15146,#15147,
#15148,#15149,#15150,#15151,#15152,#15153,#15154,#15155,#15156,#15157,#15158,
#15159,#15160,#15161,#15162,#15163,#15164,#15165,#15166,#15167,#15168,#15169,
#15170,#15171,#15172,#15173,#15174,#15175,#15176,#15177,#15178,#15179,#15180,
#15181,#15182,#15183,#15184,#15185,#15186,#15187,#15188,#15189,#15190,#15191,
#15192,#15193,#15194,#15195,#15196,#15197,#15198,#15199,#15200,#15201,#15202,
#15203,#15204,#15205,#15206,#15207,#15208,#15209,#15210,#15211,#15212,#15213,
#15214,#15215,#15216,#15217,#15218,#15219,#15220,#15221,#15222,#15223,#15224,
#15225,#15226,#15227,#15228,#15229,#15230,#15231,#15232,#15233,#15234,#15235,
#15236,#15237,#15238,#15239,#15240,#15241,#15242,#15243,#15244,#15245,#15246,
#15247,#15248,#15249,#15250,#15251,#15252,#15253,#15254,#15255,#15256,#15257,
#15258,#15259,#15260,#15261,#15262,#15263,#15264,#15265,#15266,#15267,#15268,
#15269,#15270,#15271,#15272,#15273,#15274,#15275,#15276,#15277,#15278,#15279,
#15280,#15281,#15282,#15283,#15284,#15285,#15286,#15287,#15288,#15289,#15290,
#15291,#15292,#15293,#15294,#15295,#15296,#15297,#15298)) ;
#15503 = CLOSED_SHELL('',(#15299,#15300,#15301,#15302,#15303,#15304,#15305,
#15306)) ;
#15504 = CLOSED_SHELL('',(#15307,#15308,#15309,#15310,#15311,#15312,#15313,
#15314,#15315,#15316,#15317,#15318,#15319,#15320,#15321,#15322,#15323,#15324,
#15325,#15326,#15327,#15328,#15329)) ;
#15505 = CLOSED_SHELL('',(#15330,#15331,#15332,#15333,#15334,#15335,#15336,
#15337,#15338,#15339,#15340,#15341,#15342,#15343,#15344,#15345,#15346,#15347,
#15348,#15349,#15350,#15351,#15352,#15353,#15354,#15355,#15356,#15357,#15358,
#15359,#15360,#15361,#15362,#15363,#15364,#15365,#15366,#15367,#15368,#15369,
#15370,#15371,#15372,#15373,#15374,#15375,#15376,#15377,#15378,#15379,#15380,
#15381,#15382,#15383,#15384,#15385,#15386,#15387,#15388,#15389,#15390,#15391,
#15392,#15393,#15394,#15395,#15396,#15397,#15398,#15399,#15400,#15401,#15402,
#15403,#15404,#15405,#15406,#15407,#15408,#15409,#15410,#15411,#15412,#15413,
#15414,#15415,#15416,#15417,#15418,#15419,#15420,#15421,#15422,#15423,#15424,
#15425,#15426,#15427,#15428,#15429,#15430,#15431,#15432,#15433,#15434,#15435,
#15436,#15437,#15438,#15439,#15440,#15441,#15442,#15443,#15444,#15445,#15446,
#15447,#15448,#15449,#15450,#15451,#15452,#15453,#15454,#15455,#15456,#15457,
#15458,#15459,#15460,#15461)) ;
#15506 = CLOSED_SHELL('',(#15462,#15463,#15464,#15465,#15466,#15467,#15468,
#15469)) ;
#15507 = CLOSED_SHELL('',(#15470,#15471,#15472,#15473,#15474,#15475,#15476,
#15477,#15478,#15479,#15480,#15481)) ;
#15508 = CLOSED_SHELL('',(#15482,#15483,#15484,#15485,#15486,#15487,#15488,
#15489,#15490,#15491,#15492,#15493)) ;
#15509 = DERIVED_UNIT_ELEMENT(#15539,1.) ;
#15510 = DERIVED_UNIT_ELEMENT(#63826,-3.) ;
#15511 = DERIVED_UNIT_ELEMENT(#15539,1.) ;
#15512 = DERIVED_UNIT_ELEMENT(#63826,-3.) ;
#15513 = DERIVED_UNIT_ELEMENT(#15539,1.) ;
#15514 = DERIVED_UNIT_ELEMENT(#63826,-3.) ;
#15515 = DERIVED_UNIT_ELEMENT(#15539,1.) ;
#15516 = DERIVED_UNIT_ELEMENT(#63826,-3.) ;
#15517 = DERIVED_UNIT_ELEMENT(#15539,1.) ;
#15518 = DERIVED_UNIT_ELEMENT(#63826,-3.) ;
#15519 = DERIVED_UNIT_ELEMENT(#15539,1.) ;
#15520 = DERIVED_UNIT_ELEMENT(#63826,-3.) ;
#15521 = DERIVED_UNIT_ELEMENT(#15539,1.) ;
#15522 = DERIVED_UNIT_ELEMENT(#63826,-3.) ;
#15523 = DERIVED_UNIT_ELEMENT(#15539,1.) ;
#15524 = DERIVED_UNIT_ELEMENT(#63826,-3.) ;
#15525 = DERIVED_UNIT_ELEMENT(#15539,1.) ;
#15526 = DERIVED_UNIT_ELEMENT(#63826,-3.) ;
#15527 = DERIVED_UNIT_ELEMENT(#15539,1.) ;
#15528 = DERIVED_UNIT_ELEMENT(#63826,-3.) ;
#15529 = DERIVED_UNIT_ELEMENT(#15539,1.) ;
#15530 = DERIVED_UNIT_ELEMENT(#63826,-3.) ;
#15531 = DERIVED_UNIT_ELEMENT(#15539,1.) ;
#15532 = DERIVED_UNIT_ELEMENT(#63826,-3.) ;
#15533 = DERIVED_UNIT_ELEMENT(#15539,1.) ;
#15534 = DERIVED_UNIT_ELEMENT(#63826,-3.) ;
#15535 = DERIVED_UNIT_ELEMENT(#15539,1.) ;
#15536 = DERIVED_UNIT_ELEMENT(#63826,-3.) ;
#15537 = DERIVED_UNIT_ELEMENT(#15539,1.) ;
#15538 = DERIVED_UNIT_ELEMENT(#63826,-3.) ;
#15539 = (
MASS_UNIT()
NAMED_UNIT(*)
SI_UNIT(.KILO.,.GRAM.)
) ;
#15540 = DERIVED_UNIT((#15509,#15510)) ;
#15541 = DERIVED_UNIT((#15511,#15512)) ;
#15542 = DERIVED_UNIT((#15513,#15514)) ;
#15543 = DERIVED_UNIT((#15515,#15516)) ;
#15544 = DERIVED_UNIT((#15517,#15518)) ;
#15545 = DERIVED_UNIT((#15519,#15520)) ;
#15546 = DERIVED_UNIT((#15521,#15522)) ;
#15547 = DERIVED_UNIT((#15523,#15524)) ;
#15548 = DERIVED_UNIT((#15525,#15526)) ;
#15549 = DERIVED_UNIT((#15527,#15528)) ;
#15550 = DERIVED_UNIT((#15529,#15530)) ;
#15551 = DERIVED_UNIT((#15531,#15532)) ;
#15552 = DERIVED_UNIT((#15533,#15534)) ;
#15553 = DERIVED_UNIT((#15535,#15536)) ;
#15554 = DERIVED_UNIT((#15537,#15538)) ;
#15555 = MEASURE_REPRESENTATION_ITEM('density measure',
POSITIVE_RATIO_MEASURE(7850.),#15540) ;
#15556 = MEASURE_REPRESENTATION_ITEM('density measure',
POSITIVE_RATIO_MEASURE(7850.),#15541) ;
#15557 = MEASURE_REPRESENTATION_ITEM('density measure',
POSITIVE_RATIO_MEASURE(7850.),#15542) ;
#15558 = MEASURE_REPRESENTATION_ITEM('density measure',
POSITIVE_RATIO_MEASURE(7850.),#15543) ;
#15559 = MEASURE_REPRESENTATION_ITEM('density measure',
POSITIVE_RATIO_MEASURE(7850.),#15544) ;
#15560 = MEASURE_REPRESENTATION_ITEM('density measure',
POSITIVE_RATIO_MEASURE(7850.),#15545) ;
#15561 = MEASURE_REPRESENTATION_ITEM('density measure',
POSITIVE_RATIO_MEASURE(7850.),#15546) ;
#15562 = MEASURE_REPRESENTATION_ITEM('density measure',
POSITIVE_RATIO_MEASURE(7850.),#15547) ;
#15563 = MEASURE_REPRESENTATION_ITEM('density measure',
POSITIVE_RATIO_MEASURE(2700.),#15548) ;
#15564 = MEASURE_REPRESENTATION_ITEM('density measure',
POSITIVE_RATIO_MEASURE(7850.),#15549) ;
#15565 = MEASURE_REPRESENTATION_ITEM('density measure',
POSITIVE_RATIO_MEASURE(7850.),#15550) ;
#15566 = MEASURE_REPRESENTATION_ITEM('density measure',
POSITIVE_RATIO_MEASURE(7850.),#15551) ;
#15567 = MEASURE_REPRESENTATION_ITEM('density measure',
POSITIVE_RATIO_MEASURE(7850.),#15552) ;
#15568 = MEASURE_REPRESENTATION_ITEM('density measure',
POSITIVE_RATIO_MEASURE(7850.),#15553) ;
#15569 = MEASURE_REPRESENTATION_ITEM('density measure',
POSITIVE_RATIO_MEASURE(7850.),#15554) ;
#15570 = PROPERTY_DEFINITION_REPRESENTATION(#15645,#15600) ;
#15571 = PROPERTY_DEFINITION_REPRESENTATION(#15646,#15601) ;
#15572 = PROPERTY_DEFINITION_REPRESENTATION(#15647,#15602) ;
#15573 = PROPERTY_DEFINITION_REPRESENTATION(#15648,#15603) ;
#15574 = PROPERTY_DEFINITION_REPRESENTATION(#15649,#15604) ;
#15575 = PROPERTY_DEFINITION_REPRESENTATION(#15650,#15605) ;
#15576 = PROPERTY_DEFINITION_REPRESENTATION(#15651,#15606) ;
#15577 = PROPERTY_DEFINITION_REPRESENTATION(#15652,#15607) ;
#15578 = PROPERTY_DEFINITION_REPRESENTATION(#15653,#15608) ;
#15579 = PROPERTY_DEFINITION_REPRESENTATION(#15654,#15609) ;
#15580 = PROPERTY_DEFINITION_REPRESENTATION(#15655,#15610) ;
#15581 = PROPERTY_DEFINITION_REPRESENTATION(#15656,#15611) ;
#15582 = PROPERTY_DEFINITION_REPRESENTATION(#15657,#15612) ;
#15583 = PROPERTY_DEFINITION_REPRESENTATION(#15658,#15613) ;
#15584 = PROPERTY_DEFINITION_REPRESENTATION(#15659,#15614) ;
#15585 = PROPERTY_DEFINITION_REPRESENTATION(#15660,#15615) ;
#15586 = PROPERTY_DEFINITION_REPRESENTATION(#15661,#15616) ;
#15587 = PROPERTY_DEFINITION_REPRESENTATION(#15662,#15617) ;
#15588 = PROPERTY_DEFINITION_REPRESENTATION(#15663,#15618) ;
#15589 = PROPERTY_DEFINITION_REPRESENTATION(#15664,#15619) ;
#15590 = PROPERTY_DEFINITION_REPRESENTATION(#15665,#15620) ;
#15591 = PROPERTY_DEFINITION_REPRESENTATION(#15666,#15621) ;
#15592 = PROPERTY_DEFINITION_REPRESENTATION(#15667,#15622) ;
#15593 = PROPERTY_DEFINITION_REPRESENTATION(#15668,#15623) ;
#15594 = PROPERTY_DEFINITION_REPRESENTATION(#15669,#15624) ;
#15595 = PROPERTY_DEFINITION_REPRESENTATION(#15670,#15625) ;
#15596 = PROPERTY_DEFINITION_REPRESENTATION(#15671,#15626) ;
#15597 = PROPERTY_DEFINITION_REPRESENTATION(#15672,#15627) ;
#15598 = PROPERTY_DEFINITION_REPRESENTATION(#15673,#15628) ;
#15599 = PROPERTY_DEFINITION_REPRESENTATION(#15674,#15629) ;
#15600 = REPRESENTATION('material name',(#15630),#63809) ;
#15601 = REPRESENTATION('density',(#15555),#63809) ;
#15602 = REPRESENTATION('material name',(#15631),#63810) ;
#15603 = REPRESENTATION('density',(#15556),#63810) ;
#15604 = REPRESENTATION('material name',(#15632),#63811) ;
#15605 = REPRESENTATION('density',(#15557),#63811) ;
#15606 = REPRESENTATION('material name',(#15633),#63812) ;
#15607 = REPRESENTATION('density',(#15558),#63812) ;
#15608 = REPRESENTATION('material name',(#15634),#63813) ;
#15609 = REPRESENTATION('density',(#15559),#63813) ;
#15610 = REPRESENTATION('material name',(#15635),#63814) ;
#15611 = REPRESENTATION('density',(#15560),#63814) ;
#15612 = REPRESENTATION('material name',(#15636),#63815) ;
#15613 = REPRESENTATION('density',(#15561),#63815) ;
#15614 = REPRESENTATION('material name',(#15637),#63816) ;
#15615 = REPRESENTATION('density',(#15562),#63816) ;
#15616 = REPRESENTATION('material name',(#15638),#63817) ;
#15617 = REPRESENTATION('density',(#15563),#63817) ;
#15618 = REPRESENTATION('material name',(#15639),#63818) ;
#15619 = REPRESENTATION('density',(#15564),#63818) ;
#15620 = REPRESENTATION('material name',(#15640),#63819) ;
#15621 = REPRESENTATION('density',(#15565),#63819) ;
#15622 = REPRESENTATION('material name',(#15641),#63820) ;
#15623 = REPRESENTATION('density',(#15566),#63820) ;
#15624 = REPRESENTATION('material name',(#15642),#63821) ;
#15625 = REPRESENTATION('density',(#15567),#63821) ;
#15626 = REPRESENTATION('material name',(#15643),#63822) ;
#15627 = REPRESENTATION('density',(#15568),#63822) ;
#15628 = REPRESENTATION('material name',(#15644),#63823) ;
#15629 = REPRESENTATION('density',(#15569),#63823) ;
#15630 = DESCRIPTIVE_REPRESENTATION_ITEM('Steel','Steel') ;
#15631 = DESCRIPTIVE_REPRESENTATION_ITEM('Steel','Steel') ;
#15632 = DESCRIPTIVE_REPRESENTATION_ITEM('Steel','Steel') ;
#15633 = DESCRIPTIVE_REPRESENTATION_ITEM('Steel','Steel') ;
#15634 = DESCRIPTIVE_REPRESENTATION_ITEM('Steel','Steel') ;
#15635 = DESCRIPTIVE_REPRESENTATION_ITEM('Steel','Steel') ;
#15636 = DESCRIPTIVE_REPRESENTATION_ITEM('Steel','Steel') ;
#15637 = DESCRIPTIVE_REPRESENTATION_ITEM('Steel','Steel') ;
#15638 = DESCRIPTIVE_REPRESENTATION_ITEM('Aluminum','Aluminum') ;
#15639 = DESCRIPTIVE_REPRESENTATION_ITEM('Steel','Steel') ;
#15640 = DESCRIPTIVE_REPRESENTATION_ITEM('Steel','Steel') ;
#15641 = DESCRIPTIVE_REPRESENTATION_ITEM('Steel','Steel') ;
#15642 = DESCRIPTIVE_REPRESENTATION_ITEM('Steel','Steel') ;
#15643 = DESCRIPTIVE_REPRESENTATION_ITEM('Steel','Steel') ;
#15644 = DESCRIPTIVE_REPRESENTATION_ITEM('Steel','Steel') ;
#15645 = PROPERTY_DEFINITION('material property','material name',#63896) ;
#15646 = PROPERTY_DEFINITION('material property','density of part',#63896) ;
#15647 = PROPERTY_DEFINITION('material property','material name',#63897) ;
#15648 = PROPERTY_DEFINITION('material property','density of part',#63897) ;
#15649 = PROPERTY_DEFINITION('material property','material name',#63898) ;
#15650 = PROPERTY_DEFINITION('material property','density of part',#63898) ;
#15651 = PROPERTY_DEFINITION('material property','material name',#63899) ;
#15652 = PROPERTY_DEFINITION('material property','density of part',#63899) ;
#15653 = PROPERTY_DEFINITION('material property','material name',#63900) ;
#15654 = PROPERTY_DEFINITION('material property','density of part',#63900) ;
#15655 = PROPERTY_DEFINITION('material property','material name',#63901) ;
#15656 = PROPERTY_DEFINITION('material property','density of part',#63901) ;
#15657 = PROPERTY_DEFINITION('material property','material name',#63902) ;
#15658 = PROPERTY_DEFINITION('material property','density of part',#63902) ;
#15659 = PROPERTY_DEFINITION('material property','material name',#63903) ;
#15660 = PROPERTY_DEFINITION('material property','density of part',#63903) ;
#15661 = PROPERTY_DEFINITION('material property','material name',#63904) ;
#15662 = PROPERTY_DEFINITION('material property','density of part',#63904) ;
#15663 = PROPERTY_DEFINITION('material property','material name',#63905) ;
#15664 = PROPERTY_DEFINITION('material property','density of part',#63905) ;
#15665 = PROPERTY_DEFINITION('material property','material name',#63906) ;
#15666 = PROPERTY_DEFINITION('material property','density of part',#63906) ;
#15667 = PROPERTY_DEFINITION('material property','material name',#63907) ;
#15668 = PROPERTY_DEFINITION('material property','density of part',#63907) ;
#15669 = PROPERTY_DEFINITION('material property','material name',#63908) ;
#15670 = PROPERTY_DEFINITION('material property','density of part',#63908) ;
#15671 = PROPERTY_DEFINITION('material property','material name',#63909) ;
#15672 = PROPERTY_DEFINITION('material property','density of part',#63909) ;
#15673 = PROPERTY_DEFINITION('material property','material name',#63910) ;
#15674 = PROPERTY_DEFINITION('material property','density of part',#63910) ;
#15675 = AXIS2_PLACEMENT_3D('',#23012,#17902,#17903) ;
#15676 = AXIS2_PLACEMENT_3D('',#23013,#17904,#17905) ;
#15677 = AXIS2_PLACEMENT_3D('',#23014,#17906,#17907) ;
#15678 = AXIS2_PLACEMENT_3D('',#23018,#17909,#17910) ;
#15679 = AXIS2_PLACEMENT_3D('',#23019,#17911,#17912) ;
#15680 = AXIS2_PLACEMENT_3D('',#23021,#17913,#17914) ;
#15681 = AXIS2_PLACEMENT_3D('',#23023,#17916,#17917) ;
#15682 = AXIS2_PLACEMENT_3D('',#23027,#17919,#17920) ;
#15683 = AXIS2_PLACEMENT_3D('',#23028,#17921,#17922) ;
#15684 = AXIS2_PLACEMENT_3D('',#23030,#17923,#17924) ;
#15685 = AXIS2_PLACEMENT_3D('',#23032,#17926,#17927) ;
#15686 = AXIS2_PLACEMENT_3D('',#23036,#17929,#17930) ;
#15687 = AXIS2_PLACEMENT_3D('',#23037,#17931,#17932) ;
#15688 = AXIS2_PLACEMENT_3D('',#23039,#17933,#17934) ;
#15689 = AXIS2_PLACEMENT_3D('',#23041,#17936,#17937) ;
#15690 = AXIS2_PLACEMENT_3D('',#23045,#17939,#17940) ;
#15691 = AXIS2_PLACEMENT_3D('',#23046,#17941,#17942) ;
#15692 = AXIS2_PLACEMENT_3D('',#23048,#17943,#17944) ;
#15693 = AXIS2_PLACEMENT_3D('',#23050,#17946,#17947) ;
#15694 = AXIS2_PLACEMENT_3D('',#23052,#17948,#17949) ;
#15695 = AXIS2_PLACEMENT_3D('',#23054,#17950,#17951) ;
#15696 = AXIS2_PLACEMENT_3D('',#23055,#17952,#17953) ;
#15697 = AXIS2_PLACEMENT_3D('',#23057,#17954,#17955) ;
#15698 = AXIS2_PLACEMENT_3D('',#23059,#17957,#17958) ;
#15699 = AXIS2_PLACEMENT_3D('',#23062,#17960,#17961) ;
#15700 = AXIS2_PLACEMENT_3D('',#23063,#17962,#17963) ;
#15701 = AXIS2_PLACEMENT_3D('',#23065,#17964,#17965) ;
#15702 = AXIS2_PLACEMENT_3D('',#23067,#17966,#17967) ;
#15703 = AXIS2_PLACEMENT_3D('',#23068,#17968,#17969) ;
#15704 = AXIS2_PLACEMENT_3D('',#23070,#17970,#17971) ;
#15705 = AXIS2_PLACEMENT_3D('',#23072,#17973,#17974) ;
#15706 = AXIS2_PLACEMENT_3D('',#23075,#17976,#17977) ;
#15707 = AXIS2_PLACEMENT_3D('',#23076,#17978,#17979) ;
#15708 = AXIS2_PLACEMENT_3D('',#23078,#17980,#17981) ;
#15709 = AXIS2_PLACEMENT_3D('',#23080,#17982,#17983) ;
#15710 = AXIS2_PLACEMENT_3D('',#23081,#17984,#17985) ;
#15711 = AXIS2_PLACEMENT_3D('',#23083,#17986,#17987) ;
#15712 = AXIS2_PLACEMENT_3D('',#23085,#17989,#17990) ;
#15713 = AXIS2_PLACEMENT_3D('',#23088,#17992,#17993) ;
#15714 = AXIS2_PLACEMENT_3D('',#23089,#17994,#17995) ;
#15715 = AXIS2_PLACEMENT_3D('',#23091,#17996,#17997) ;
#15716 = AXIS2_PLACEMENT_3D('',#23093,#17998,#17999) ;
#15717 = AXIS2_PLACEMENT_3D('',#23094,#18000,#18001) ;
#15718 = AXIS2_PLACEMENT_3D('',#23096,#18002,#18003) ;
#15719 = AXIS2_PLACEMENT_3D('',#23098,#18005,#18006) ;
#15720 = AXIS2_PLACEMENT_3D('',#23101,#18008,#18009) ;
#15721 = AXIS2_PLACEMENT_3D('',#23102,#18010,#18011) ;
#15722 = AXIS2_PLACEMENT_3D('',#23106,#18013,#18014) ;
#15723 = AXIS2_PLACEMENT_3D('',#23107,#18015,#18016) ;
#15724 = AXIS2_PLACEMENT_3D('',#23109,#18017,#18018) ;
#15725 = AXIS2_PLACEMENT_3D('',#23111,#18020,#18021) ;
#15726 = AXIS2_PLACEMENT_3D('',#23115,#18023,#18024) ;
#15727 = AXIS2_PLACEMENT_3D('',#23116,#18025,#18026) ;
#15728 = AXIS2_PLACEMENT_3D('',#23118,#18027,#18028) ;
#15729 = AXIS2_PLACEMENT_3D('',#23120,#18030,#18031) ;
#15730 = AXIS2_PLACEMENT_3D('',#23124,#18033,#18034) ;
#15731 = AXIS2_PLACEMENT_3D('',#23125,#18035,#18036) ;
#15732 = AXIS2_PLACEMENT_3D('',#23127,#18037,#18038) ;
#15733 = AXIS2_PLACEMENT_3D('',#23129,#18040,#18041) ;
#15734 = AXIS2_PLACEMENT_3D('',#23133,#18043,#18044) ;
#15735 = AXIS2_PLACEMENT_3D('',#23134,#18045,#18046) ;
#15736 = AXIS2_PLACEMENT_3D('',#23136,#18047,#18048) ;
#15737 = AXIS2_PLACEMENT_3D('',#23138,#18050,#18051) ;
#15738 = AXIS2_PLACEMENT_3D('',#23142,#18053,#18054) ;
#15739 = AXIS2_PLACEMENT_3D('',#23143,#18055,#18056) ;
#15740 = AXIS2_PLACEMENT_3D('',#23145,#18057,#18058) ;
#15741 = AXIS2_PLACEMENT_3D('',#23147,#18060,#18061) ;
#15742 = AXIS2_PLACEMENT_3D('',#23151,#18063,#18064) ;
#15743 = AXIS2_PLACEMENT_3D('',#23152,#18065,#18066) ;
#15744 = AXIS2_PLACEMENT_3D('',#23154,#18067,#18068) ;
#15745 = AXIS2_PLACEMENT_3D('',#23156,#18070,#18071) ;
#15746 = AXIS2_PLACEMENT_3D('',#23160,#18073,#18074) ;
#15747 = AXIS2_PLACEMENT_3D('',#23161,#18075,#18076) ;
#15748 = AXIS2_PLACEMENT_3D('',#23163,#18077,#18078) ;
#15749 = AXIS2_PLACEMENT_3D('',#23165,#18080,#18081) ;
#15750 = AXIS2_PLACEMENT_3D('',#23169,#18083,#18084) ;
#15751 = AXIS2_PLACEMENT_3D('',#23170,#18085,#18086) ;
#15752 = AXIS2_PLACEMENT_3D('',#23172,#18087,#18088) ;
#15753 = AXIS2_PLACEMENT_3D('',#23174,#18090,#18091) ;
#15754 = AXIS2_PLACEMENT_3D('',#23176,#18092,#18093) ;
#15755 = AXIS2_PLACEMENT_3D('',#23179,#18095,#18096) ;
#15756 = AXIS2_PLACEMENT_3D('',#23180,#18097,#18098) ;
#15757 = AXIS2_PLACEMENT_3D('',#23189,#18103,#18104) ;
#15758 = AXIS2_PLACEMENT_3D('',#23195,#18108,#18109) ;
#15759 = AXIS2_PLACEMENT_3D('',#23201,#18113,#18114) ;
#15760 = AXIS2_PLACEMENT_3D('',#23204,#18117,#18118) ;
#15761 = AXIS2_PLACEMENT_3D('',#23205,#18119,#18120) ;
#15762 = AXIS2_PLACEMENT_3D('',#23206,#18121,#18122) ;
#15763 = AXIS2_PLACEMENT_3D('',#23207,#18123,#18124) ;
#15764 = AXIS2_PLACEMENT_3D('',#23209,#18125,#18126) ;
#15765 = AXIS2_PLACEMENT_3D('',#23211,#18127,#18128) ;
#15766 = AXIS2_PLACEMENT_3D('',#23212,#18129,#18130) ;
#15767 = AXIS2_PLACEMENT_3D('',#23214,#18131,#18132) ;
#15768 = AXIS2_PLACEMENT_3D('',#23216,#18134,#18135) ;
#15769 = AXIS2_PLACEMENT_3D('',#23219,#18137,#18138) ;
#15770 = AXIS2_PLACEMENT_3D('',#23220,#18139,#18140) ;
#15771 = AXIS2_PLACEMENT_3D('',#23222,#18141,#18142) ;
#15772 = AXIS2_PLACEMENT_3D('',#23224,#18143,#18144) ;
#15773 = AXIS2_PLACEMENT_3D('',#23225,#18145,#18146) ;
#15774 = AXIS2_PLACEMENT_3D('',#23227,#18147,#18148) ;
#15775 = AXIS2_PLACEMENT_3D('',#23229,#18150,#18151) ;
#15776 = AXIS2_PLACEMENT_3D('',#23232,#18153,#18154) ;
#15777 = AXIS2_PLACEMENT_3D('',#23233,#18155,#18156) ;
#15778 = AXIS2_PLACEMENT_3D('',#23235,#18157,#18158) ;
#15779 = AXIS2_PLACEMENT_3D('',#23237,#18159,#18160) ;
#15780 = AXIS2_PLACEMENT_3D('',#23238,#18161,#18162) ;
#15781 = AXIS2_PLACEMENT_3D('',#23240,#18163,#18164) ;
#15782 = AXIS2_PLACEMENT_3D('',#23242,#18166,#18167) ;
#15783 = AXIS2_PLACEMENT_3D('',#23245,#18169,#18170) ;
#15784 = AXIS2_PLACEMENT_3D('',#23246,#18171,#18172) ;
#15785 = AXIS2_PLACEMENT_3D('',#23248,#18173,#18174) ;
#15786 = AXIS2_PLACEMENT_3D('',#23250,#18175,#18176) ;
#15787 = AXIS2_PLACEMENT_3D('',#23251,#18177,#18178) ;
#15788 = AXIS2_PLACEMENT_3D('',#23253,#18179,#18180) ;
#15789 = AXIS2_PLACEMENT_3D('',#23255,#18182,#18183) ;
#15790 = AXIS2_PLACEMENT_3D('',#23258,#18185,#18186) ;
#15791 = AXIS2_PLACEMENT_3D('',#23259,#18187,#18188) ;
#15792 = AXIS2_PLACEMENT_3D('',#23261,#18189,#18190) ;
#15793 = AXIS2_PLACEMENT_3D('',#23263,#18191,#18192) ;
#15794 = AXIS2_PLACEMENT_3D('',#23264,#18193,#18194) ;
#15795 = AXIS2_PLACEMENT_3D('',#23266,#18195,#18196) ;
#15796 = AXIS2_PLACEMENT_3D('',#23268,#18198,#18199) ;
#15797 = AXIS2_PLACEMENT_3D('',#23271,#18201,#18202) ;
#15798 = AXIS2_PLACEMENT_3D('',#23272,#18203,#18204) ;
#15799 = AXIS2_PLACEMENT_3D('',#23274,#18205,#18206) ;
#15800 = AXIS2_PLACEMENT_3D('',#23276,#18207,#18208) ;
#15801 = AXIS2_PLACEMENT_3D('',#23277,#18209,#18210) ;
#15802 = AXIS2_PLACEMENT_3D('',#23279,#18211,#18212) ;
#15803 = AXIS2_PLACEMENT_3D('',#23281,#18214,#18215) ;
#15804 = AXIS2_PLACEMENT_3D('',#23284,#18217,#18218) ;
#15805 = AXIS2_PLACEMENT_3D('',#23285,#18219,#18220) ;
#15806 = AXIS2_PLACEMENT_3D('',#23287,#18221,#18222) ;
#15807 = AXIS2_PLACEMENT_3D('',#23289,#18223,#18224) ;
#15808 = AXIS2_PLACEMENT_3D('',#23290,#18225,#18226) ;
#15809 = AXIS2_PLACEMENT_3D('',#23292,#18227,#18228) ;
#15810 = AXIS2_PLACEMENT_3D('',#23294,#18230,#18231) ;
#15811 = AXIS2_PLACEMENT_3D('',#23297,#18233,#18234) ;
#15812 = AXIS2_PLACEMENT_3D('',#23298,#18235,#18236) ;
#15813 = AXIS2_PLACEMENT_3D('',#23300,#18237,#18238) ;
#15814 = AXIS2_PLACEMENT_3D('',#23302,#18239,#18240) ;
#15815 = AXIS2_PLACEMENT_3D('',#23303,#18241,#18242) ;
#15816 = AXIS2_PLACEMENT_3D('',#23305,#18243,#18244) ;
#15817 = AXIS2_PLACEMENT_3D('',#23307,#18246,#18247) ;
#15818 = AXIS2_PLACEMENT_3D('',#23310,#18249,#18250) ;
#15819 = AXIS2_PLACEMENT_3D('',#23311,#18251,#18252) ;
#15820 = AXIS2_PLACEMENT_3D('',#23313,#18253,#18254) ;
#15821 = AXIS2_PLACEMENT_3D('',#23315,#18255,#18256) ;
#15822 = AXIS2_PLACEMENT_3D('',#23316,#18257,#18258) ;
#15823 = AXIS2_PLACEMENT_3D('',#23318,#18259,#18260) ;
#15824 = AXIS2_PLACEMENT_3D('',#23320,#18262,#18263) ;
#15825 = AXIS2_PLACEMENT_3D('',#23323,#18265,#18266) ;
#15826 = AXIS2_PLACEMENT_3D('',#23324,#18267,#18268) ;
#15827 = AXIS2_PLACEMENT_3D('',#23326,#18269,#18270) ;
#15828 = AXIS2_PLACEMENT_3D('',#23328,#18271,#18272) ;
#15829 = AXIS2_PLACEMENT_3D('',#23329,#18273,#18274) ;
#15830 = AXIS2_PLACEMENT_3D('',#23331,#18275,#18276) ;
#15831 = AXIS2_PLACEMENT_3D('',#23333,#18278,#18279) ;
#15832 = AXIS2_PLACEMENT_3D('',#23336,#18281,#18282) ;
#15833 = AXIS2_PLACEMENT_3D('',#23337,#18283,#18284) ;
#15834 = AXIS2_PLACEMENT_3D('',#23339,#18285,#18286) ;
#15835 = AXIS2_PLACEMENT_3D('',#23341,#18287,#18288) ;
#15836 = AXIS2_PLACEMENT_3D('',#23342,#18289,#18290) ;
#15837 = AXIS2_PLACEMENT_3D('',#23344,#18291,#18292) ;
#15838 = AXIS2_PLACEMENT_3D('',#23346,#18294,#18295) ;
#15839 = AXIS2_PLACEMENT_3D('',#23349,#18297,#18298) ;
#15840 = AXIS2_PLACEMENT_3D('',#23350,#18299,#18300) ;
#15841 = AXIS2_PLACEMENT_3D('',#23352,#18301,#18302) ;
#15842 = AXIS2_PLACEMENT_3D('',#23354,#18303,#18304) ;
#15843 = AXIS2_PLACEMENT_3D('',#23355,#18305,#18306) ;
#15844 = AXIS2_PLACEMENT_3D('',#23357,#18307,#18308) ;
#15845 = AXIS2_PLACEMENT_3D('',#23359,#18310,#18311) ;
#15846 = AXIS2_PLACEMENT_3D('',#23362,#18313,#18314) ;
#15847 = AXIS2_PLACEMENT_3D('',#23363,#18315,#18316) ;
#15848 = AXIS2_PLACEMENT_3D('',#23372,#18321,#18322) ;
#15849 = AXIS2_PLACEMENT_3D('',#23378,#18326,#18327) ;
#15850 = AXIS2_PLACEMENT_3D('',#23384,#18331,#18332) ;
#15851 = AXIS2_PLACEMENT_3D('',#23387,#18335,#18336) ;
#15852 = AXIS2_PLACEMENT_3D('',#23388,#18337,#18338) ;
#15853 = AXIS2_PLACEMENT_3D('',#23389,#18339,#18340) ;
#15854 = AXIS2_PLACEMENT_3D('',#23390,#18341,#18342) ;
#15855 = AXIS2_PLACEMENT_3D('',#23394,#18344,#18345) ;
#15856 = AXIS2_PLACEMENT_3D('',#23395,#18346,#18347) ;
#15857 = AXIS2_PLACEMENT_3D('',#23397,#18348,#18349) ;
#15858 = AXIS2_PLACEMENT_3D('',#23399,#18351,#18352) ;
#15859 = AXIS2_PLACEMENT_3D('',#23403,#18354,#18355) ;
#15860 = AXIS2_PLACEMENT_3D('',#23404,#18356,#18357) ;
#15861 = AXIS2_PLACEMENT_3D('',#23406,#18358,#18359) ;
#15862 = AXIS2_PLACEMENT_3D('',#23408,#18361,#18362) ;
#15863 = AXIS2_PLACEMENT_3D('',#23412,#18364,#18365) ;
#15864 = AXIS2_PLACEMENT_3D('',#23413,#18366,#18367) ;
#15865 = AXIS2_PLACEMENT_3D('',#23415,#18368,#18369) ;
#15866 = AXIS2_PLACEMENT_3D('',#23417,#18371,#18372) ;
#15867 = AXIS2_PLACEMENT_3D('',#23421,#18374,#18375) ;
#15868 = AXIS2_PLACEMENT_3D('',#23422,#18376,#18377) ;
#15869 = AXIS2_PLACEMENT_3D('',#23424,#18378,#18379) ;
#15870 = AXIS2_PLACEMENT_3D('',#23426,#18381,#18382) ;
#15871 = AXIS2_PLACEMENT_3D('',#23430,#18384,#18385) ;
#15872 = AXIS2_PLACEMENT_3D('',#23431,#18386,#18387) ;
#15873 = AXIS2_PLACEMENT_3D('',#23434,#18389,#18390) ;
#15874 = AXIS2_PLACEMENT_3D('',#23435,#18391,#18392) ;
#15875 = AXIS2_PLACEMENT_3D('',#23439,#18394,#18395) ;
#15876 = AXIS2_PLACEMENT_3D('',#23440,#18396,#18397) ;
#15877 = AXIS2_PLACEMENT_3D('',#23443,#18399,#18400) ;
#15878 = AXIS2_PLACEMENT_3D('',#23444,#18401,#18402) ;
#15879 = AXIS2_PLACEMENT_3D('',#23453,#18407,#18408) ;
#15880 = AXIS2_PLACEMENT_3D('',#23457,#18410,#18411) ;
#15881 = AXIS2_PLACEMENT_3D('',#23458,#18412,#18413) ;
#15882 = AXIS2_PLACEMENT_3D('',#23460,#18414,#18415) ;
#15883 = AXIS2_PLACEMENT_3D('',#23462,#18417,#18418) ;
#15884 = AXIS2_PLACEMENT_3D('',#23466,#18420,#18421) ;
#15885 = AXIS2_PLACEMENT_3D('',#23467,#18422,#18423) ;
#15886 = AXIS2_PLACEMENT_3D('',#23469,#18424,#18425) ;
#15887 = AXIS2_PLACEMENT_3D('',#23471,#18427,#18428) ;
#15888 = AXIS2_PLACEMENT_3D('',#23477,#18432,#18433) ;
#15889 = AXIS2_PLACEMENT_3D('',#23481,#18436,#18437) ;
#15890 = AXIS2_PLACEMENT_3D('',#23485,#18440,#18441) ;
#15891 = AXIS2_PLACEMENT_3D('',#23487,#18443,#18444) ;
#15892 = AXIS2_PLACEMENT_3D('',#23488,#18445,#18446) ;
#15893 = AXIS2_PLACEMENT_3D('',#23489,#18447,#18448) ;
#15894 = AXIS2_PLACEMENT_3D('',#23493,#18450,#18451) ;
#15895 = AXIS2_PLACEMENT_3D('',#23494,#18452,#18453) ;
#15896 = AXIS2_PLACEMENT_3D('',#23496,#18454,#18455) ;
#15897 = AXIS2_PLACEMENT_3D('',#23498,#18457,#18458) ;
#15898 = AXIS2_PLACEMENT_3D('',#23502,#18460,#18461) ;
#15899 = AXIS2_PLACEMENT_3D('',#23503,#18462,#18463) ;
#15900 = AXIS2_PLACEMENT_3D('',#23505,#18464,#18465) ;
#15901 = AXIS2_PLACEMENT_3D('',#23507,#18467,#18468) ;
#15902 = AXIS2_PLACEMENT_3D('',#23511,#18470,#18471) ;
#15903 = AXIS2_PLACEMENT_3D('',#23512,#18472,#18473) ;
#15904 = AXIS2_PLACEMENT_3D('',#23514,#18474,#18475) ;
#15905 = AXIS2_PLACEMENT_3D('',#23516,#18477,#18478) ;
#15906 = AXIS2_PLACEMENT_3D('',#23520,#18480,#18481) ;
#15907 = AXIS2_PLACEMENT_3D('',#23521,#18482,#18483) ;
#15908 = AXIS2_PLACEMENT_3D('',#23523,#18484,#18485) ;
#15909 = AXIS2_PLACEMENT_3D('',#23525,#18487,#18488) ;
#15910 = AXIS2_PLACEMENT_3D('',#23529,#18490,#18491) ;
#15911 = AXIS2_PLACEMENT_3D('',#23530,#18492,#18493) ;
#15912 = AXIS2_PLACEMENT_3D('',#23532,#18494,#18495) ;
#15913 = AXIS2_PLACEMENT_3D('',#23534,#18497,#18498) ;
#15914 = AXIS2_PLACEMENT_3D('',#23538,#18500,#18501) ;
#15915 = AXIS2_PLACEMENT_3D('',#23539,#18502,#18503) ;
#15916 = AXIS2_PLACEMENT_3D('',#23541,#18504,#18505) ;
#15917 = AXIS2_PLACEMENT_3D('',#23543,#18507,#18508) ;
#15918 = AXIS2_PLACEMENT_3D('',#23545,#18509,#18510) ;
#15919 = AXIS2_PLACEMENT_3D('',#23547,#18511,#18512) ;
#15920 = AXIS2_PLACEMENT_3D('',#23548,#18513,#18514) ;
#15921 = AXIS2_PLACEMENT_3D('',#23551,#18516,#18517) ;
#15922 = AXIS2_PLACEMENT_3D('',#23552,#18518,#18519) ;
#15923 = AXIS2_PLACEMENT_3D('',#23554,#18520,#18521) ;
#15924 = AXIS2_PLACEMENT_3D('',#23556,#18523,#18524) ;
#15925 = AXIS2_PLACEMENT_3D('',#23558,#18525,#18526) ;
#15926 = AXIS2_PLACEMENT_3D('',#23560,#18527,#18528) ;
#15927 = AXIS2_PLACEMENT_3D('',#23561,#18529,#18530) ;
#15928 = AXIS2_PLACEMENT_3D('',#23564,#18532,#18533) ;
#15929 = AXIS2_PLACEMENT_3D('',#23565,#18534,#18535) ;
#15930 = AXIS2_PLACEMENT_3D('',#23567,#18536,#18537) ;
#15931 = AXIS2_PLACEMENT_3D('',#23569,#18539,#18540) ;
#15932 = AXIS2_PLACEMENT_3D('',#23571,#18541,#18542) ;
#15933 = AXIS2_PLACEMENT_3D('',#23573,#18543,#18544) ;
#15934 = AXIS2_PLACEMENT_3D('',#23574,#18545,#18546) ;
#15935 = AXIS2_PLACEMENT_3D('',#23577,#18548,#18549) ;
#15936 = AXIS2_PLACEMENT_3D('',#23578,#18550,#18551) ;
#15937 = AXIS2_PLACEMENT_3D('',#23580,#18552,#18553) ;
#15938 = AXIS2_PLACEMENT_3D('',#23582,#18555,#18556) ;
#15939 = AXIS2_PLACEMENT_3D('',#23584,#18557,#18558) ;
#15940 = AXIS2_PLACEMENT_3D('',#23586,#18559,#18560) ;
#15941 = AXIS2_PLACEMENT_3D('',#23587,#18561,#18562) ;
#15942 = AXIS2_PLACEMENT_3D('',#23590,#18564,#18565) ;
#15943 = AXIS2_PLACEMENT_3D('',#23591,#18566,#18567) ;
#15944 = AXIS2_PLACEMENT_3D('',#23593,#18568,#18569) ;
#15945 = AXIS2_PLACEMENT_3D('',#23595,#18571,#18572) ;
#15946 = AXIS2_PLACEMENT_3D('',#23599,#18574,#18575) ;
#15947 = AXIS2_PLACEMENT_3D('',#23600,#18576,#18577) ;
#15948 = AXIS2_PLACEMENT_3D('',#23603,#18579,#18580) ;
#15949 = AXIS2_PLACEMENT_3D('',#23604,#18581,#18582) ;
#15950 = AXIS2_PLACEMENT_3D('',#23608,#18584,#18585) ;
#15951 = AXIS2_PLACEMENT_3D('',#23609,#18586,#18587) ;
#15952 = AXIS2_PLACEMENT_3D('',#23612,#18589,#18590) ;
#15953 = AXIS2_PLACEMENT_3D('',#23613,#18591,#18592) ;
#15954 = AXIS2_PLACEMENT_3D('',#23617,#18594,#18595) ;
#15955 = AXIS2_PLACEMENT_3D('',#23618,#18596,#18597) ;
#15956 = AXIS2_PLACEMENT_3D('',#23621,#18599,#18600) ;
#15957 = AXIS2_PLACEMENT_3D('',#23622,#18601,#18602) ;
#15958 = AXIS2_PLACEMENT_3D('',#23626,#18604,#18605) ;
#15959 = AXIS2_PLACEMENT_3D('',#23627,#18606,#18607) ;
#15960 = AXIS2_PLACEMENT_3D('',#23630,#18609,#18610) ;
#15961 = AXIS2_PLACEMENT_3D('',#23631,#18611,#18612) ;
#15962 = AXIS2_PLACEMENT_3D('',#23635,#18614,#18615) ;
#15963 = AXIS2_PLACEMENT_3D('',#23636,#18616,#18617) ;
#15964 = AXIS2_PLACEMENT_3D('',#23639,#18619,#18620) ;
#15965 = AXIS2_PLACEMENT_3D('',#23640,#18621,#18622) ;
#15966 = AXIS2_PLACEMENT_3D('',#23644,#18624,#18625) ;
#15967 = AXIS2_PLACEMENT_3D('',#23645,#18626,#18627) ;
#15968 = AXIS2_PLACEMENT_3D('',#23648,#18629,#18630) ;
#15969 = AXIS2_PLACEMENT_3D('',#23649,#18631,#18632) ;
#15970 = AXIS2_PLACEMENT_3D('',#23653,#18634,#18635) ;
#15971 = AXIS2_PLACEMENT_3D('',#23654,#18636,#18637) ;
#15972 = AXIS2_PLACEMENT_3D('',#23657,#18639,#18640) ;
#15973 = AXIS2_PLACEMENT_3D('',#23658,#18641,#18642) ;
#15974 = AXIS2_PLACEMENT_3D('',#23662,#18644,#18645) ;
#15975 = AXIS2_PLACEMENT_3D('',#23663,#18646,#18647) ;
#15976 = AXIS2_PLACEMENT_3D('',#23666,#18649,#18650) ;
#15977 = AXIS2_PLACEMENT_3D('',#23667,#18651,#18652) ;
#15978 = AXIS2_PLACEMENT_3D('',#23669,#18653,#18654) ;
#15979 = AXIS2_PLACEMENT_3D('',#23672,#18656,#18657) ;
#15980 = AXIS2_PLACEMENT_3D('',#23673,#18658,#18659) ;
#15981 = AXIS2_PLACEMENT_3D('',#23682,#18664,#18665) ;
#15982 = AXIS2_PLACEMENT_3D('',#23688,#18669,#18670) ;
#15983 = AXIS2_PLACEMENT_3D('',#23694,#18674,#18675) ;
#15984 = AXIS2_PLACEMENT_3D('',#23697,#18678,#18679) ;
#15985 = AXIS2_PLACEMENT_3D('',#23698,#18680,#18681) ;
#15986 = AXIS2_PLACEMENT_3D('',#23699,#18682,#18683) ;
#15987 = AXIS2_PLACEMENT_3D('',#23700,#18684,#18685) ;
#15988 = AXIS2_PLACEMENT_3D('',#23704,#18687,#18688) ;
#15989 = AXIS2_PLACEMENT_3D('',#23705,#18689,#18690) ;
#15990 = AXIS2_PLACEMENT_3D('',#23707,#18691,#18692) ;
#15991 = AXIS2_PLACEMENT_3D('',#23709,#18694,#18695) ;
#15992 = AXIS2_PLACEMENT_3D('',#23713,#18697,#18698) ;
#15993 = AXIS2_PLACEMENT_3D('',#23714,#18699,#18700) ;
#15994 = AXIS2_PLACEMENT_3D('',#23716,#18701,#18702) ;
#15995 = AXIS2_PLACEMENT_3D('',#23718,#18704,#18705) ;
#15996 = AXIS2_PLACEMENT_3D('',#23722,#18707,#18708) ;
#15997 = AXIS2_PLACEMENT_3D('',#23723,#18709,#18710) ;
#15998 = AXIS2_PLACEMENT_3D('',#23725,#18711,#18712) ;
#15999 = AXIS2_PLACEMENT_3D('',#23727,#18714,#18715) ;
#16000 = AXIS2_PLACEMENT_3D('',#23731,#18717,#18718) ;
#16001 = AXIS2_PLACEMENT_3D('',#23732,#18719,#18720) ;
#16002 = AXIS2_PLACEMENT_3D('',#23734,#18721,#18722) ;
#16003 = AXIS2_PLACEMENT_3D('',#23736,#18724,#18725) ;
#16004 = AXIS2_PLACEMENT_3D('',#23740,#18727,#18728) ;
#16005 = AXIS2_PLACEMENT_3D('',#23741,#18729,#18730) ;
#16006 = AXIS2_PLACEMENT_3D('',#23743,#18731,#18732) ;
#16007 = AXIS2_PLACEMENT_3D('',#23745,#18734,#18735) ;
#16008 = AXIS2_PLACEMENT_3D('',#23749,#18737,#18738) ;
#16009 = AXIS2_PLACEMENT_3D('',#23750,#18739,#18740) ;
#16010 = AXIS2_PLACEMENT_3D('',#23752,#18741,#18742) ;
#16011 = AXIS2_PLACEMENT_3D('',#23754,#18744,#18745) ;
#16012 = AXIS2_PLACEMENT_3D('',#23763,#18750,#18751) ;
#16013 = AXIS2_PLACEMENT_3D('',#23767,#18753,#18754) ;
#16014 = AXIS2_PLACEMENT_3D('',#23768,#18755,#18756) ;
#16015 = AXIS2_PLACEMENT_3D('',#23771,#18758,#18759) ;
#16016 = AXIS2_PLACEMENT_3D('',#23772,#18760,#18761) ;
#16017 = AXIS2_PLACEMENT_3D('',#23776,#18763,#18764) ;
#16018 = AXIS2_PLACEMENT_3D('',#23777,#18765,#18766) ;
#16019 = AXIS2_PLACEMENT_3D('',#23780,#18768,#18769) ;
#16020 = AXIS2_PLACEMENT_3D('',#23781,#18770,#18771) ;
#16021 = AXIS2_PLACEMENT_3D('',#23787,#18775,#18776) ;
#16022 = AXIS2_PLACEMENT_3D('',#23791,#18779,#18780) ;
#16023 = AXIS2_PLACEMENT_3D('',#23795,#18783,#18784) ;
#16024 = AXIS2_PLACEMENT_3D('',#23797,#18786,#18787) ;
#16025 = AXIS2_PLACEMENT_3D('',#23798,#18788,#18789) ;
#16026 = AXIS2_PLACEMENT_3D('',#23799,#18790,#18791) ;
#16027 = AXIS2_PLACEMENT_3D('',#23937,#18793,#18794) ;
#16028 = AXIS2_PLACEMENT_3D('',#24010,#18795,#18796) ;
#16029 = AXIS2_PLACEMENT_3D('',#24708,#18798,#18799) ;
#16030 = AXIS2_PLACEMENT_3D('',#25406,#18801,#18802) ;
#16031 = AXIS2_PLACEMENT_3D('',#26236,#18804,#18805) ;
#16032 = AXIS2_PLACEMENT_3D('',#27004,#18807,#18808) ;
#16033 = AXIS2_PLACEMENT_3D('',#27734,#18810,#18811) ;
#16034 = AXIS2_PLACEMENT_3D('',#28440,#18813,#18814) ;
#16035 = AXIS2_PLACEMENT_3D('',#29108,#18816,#18817) ;
#16036 = AXIS2_PLACEMENT_3D('',#29810,#18819,#18820) ;
#16037 = AXIS2_PLACEMENT_3D('',#30596,#18822,#18823) ;
#16038 = AXIS2_PLACEMENT_3D('',#31374,#18825,#18826) ;
#16039 = AXIS2_PLACEMENT_3D('',#32052,#18828,#18829) ;
#16040 = AXIS2_PLACEMENT_3D('',#32744,#18831,#18832) ;
#16041 = AXIS2_PLACEMENT_3D('',#32800,#18834,#18835) ;
#16042 = AXIS2_PLACEMENT_3D('',#32833,#18836,#18837) ;
#16043 = AXIS2_PLACEMENT_3D('',#33143,#18839,#18840) ;
#16044 = AXIS2_PLACEMENT_3D('',#33459,#18842,#18843) ;
#16045 = AXIS2_PLACEMENT_3D('',#33773,#18845,#18846) ;
#16046 = AXIS2_PLACEMENT_3D('',#34457,#18848,#18849) ;
#16047 = AXIS2_PLACEMENT_3D('',#35153,#18851,#18852) ;
#16048 = AXIS2_PLACEMENT_3D('',#35158,#18854,#18855) ;
#16049 = AXIS2_PLACEMENT_3D('',#35836,#18856,#18857) ;
#16050 = AXIS2_PLACEMENT_3D('',#35940,#18859,#18860) ;
#16051 = AXIS2_PLACEMENT_3D('',#36013,#18861,#18862) ;
#16052 = AXIS2_PLACEMENT_3D('',#36313,#18864,#18865) ;
#16053 = AXIS2_PLACEMENT_3D('',#36613,#18867,#18868) ;
#16054 = AXIS2_PLACEMENT_3D('',#36903,#18870,#18871) ;
#16055 = AXIS2_PLACEMENT_3D('',#37203,#18873,#18874) ;
#16056 = AXIS2_PLACEMENT_3D('',#37509,#18876,#18877) ;
#16057 = AXIS2_PLACEMENT_3D('',#37755,#18879,#18880) ;
#16058 = AXIS2_PLACEMENT_3D('',#37904,#18881,#18882) ;
#16059 = AXIS2_PLACEMENT_3D('',#38596,#18884,#18885) ;
#16060 = AXIS2_PLACEMENT_3D('',#39384,#18887,#18888) ;
#16061 = AXIS2_PLACEMENT_3D('',#40179,#18890,#18891) ;
#16062 = AXIS2_PLACEMENT_3D('',#40869,#18893,#18894) ;
#16063 = AXIS2_PLACEMENT_3D('',#41617,#18896,#18897) ;
#16064 = AXIS2_PLACEMENT_3D('',#42333,#18899,#18900) ;
#16065 = AXIS2_PLACEMENT_3D('',#43025,#18902,#18903) ;
#16066 = AXIS2_PLACEMENT_3D('',#43885,#18905,#18906) ;
#16067 = AXIS2_PLACEMENT_3D('',#44569,#18908,#18909) ;
#16068 = AXIS2_PLACEMENT_3D('',#45318,#18911,#18912) ;
#16069 = AXIS2_PLACEMENT_3D('',#46022,#18914,#18915) ;
#16070 = AXIS2_PLACEMENT_3D('',#46706,#18917,#18918) ;
#16071 = AXIS2_PLACEMENT_3D('',#47049,#18919,#18920) ;
#16072 = AXIS2_PLACEMENT_3D('',#47252,#18921,#18922) ;
#16073 = AXIS2_PLACEMENT_3D('',#47367,#18923,#18924) ;
#16074 = AXIS2_PLACEMENT_3D('',#47458,#18925,#18926) ;
#16075 = AXIS2_PLACEMENT_3D('',#47500,#18927,#18928) ;
#16076 = AXIS2_PLACEMENT_3D('',#47501,#18929,#18930) ;
#16077 = AXIS2_PLACEMENT_3D('',#47878,#18931,#18932) ;
#16078 = AXIS2_PLACEMENT_3D('',#48138,#18933,#18934) ;
#16079 = AXIS2_PLACEMENT_3D('',#48141,#18935,#18936) ;
#16080 = AXIS2_PLACEMENT_3D('',#48144,#18938,#18939) ;
#16081 = AXIS2_PLACEMENT_3D('',#48145,#18940,#18941) ;
#16082 = AXIS2_PLACEMENT_3D('',#48146,#18942,#18943) ;
#16083 = AXIS2_PLACEMENT_3D('',#48148,#18944,#18945) ;
#16084 = AXIS2_PLACEMENT_3D('',#48149,#18946,#18947) ;
#16085 = AXIS2_PLACEMENT_3D('',#48151,#18948,#18949) ;
#16086 = AXIS2_PLACEMENT_3D('',#48153,#18951,#18952) ;
#16087 = AXIS2_PLACEMENT_3D('',#48156,#18953,#18954) ;
#16088 = AXIS2_PLACEMENT_3D('',#48158,#18956,#18957) ;
#16089 = AXIS2_PLACEMENT_3D('',#48159,#18958,#18959) ;
#16090 = AXIS2_PLACEMENT_3D('',#48162,#18961,#18962) ;
#16091 = AXIS2_PLACEMENT_3D('',#48163,#18963,#18964) ;
#16092 = AXIS2_PLACEMENT_3D('',#48166,#18965,#18966) ;
#16093 = AXIS2_PLACEMENT_3D('',#48169,#18968,#18969) ;
#16094 = AXIS2_PLACEMENT_3D('',#48170,#18970,#18971) ;
#16095 = AXIS2_PLACEMENT_3D('',#48171,#18972,#18973) ;
#16096 = AXIS2_PLACEMENT_3D('',#48174,#18975,#18976) ;
#16097 = AXIS2_PLACEMENT_3D('',#48217,#18979,#18980) ;
#16098 = AXIS2_PLACEMENT_3D('',#48219,#18981,#18982) ;
#16099 = AXIS2_PLACEMENT_3D('',#48220,#18983,#18984) ;
#16100 = AXIS2_PLACEMENT_3D('',#48223,#18985,#18986) ;
#16101 = AXIS2_PLACEMENT_3D('',#48226,#18988,#18989) ;
#16102 = AXIS2_PLACEMENT_3D('',#48227,#18990,#18991) ;
#16103 = AXIS2_PLACEMENT_3D('',#48228,#18992,#18993) ;
#16104 = AXIS2_PLACEMENT_3D('',#48231,#18995,#18996) ;
#16105 = AXIS2_PLACEMENT_3D('',#48232,#18997,#18998) ;
#16106 = AXIS2_PLACEMENT_3D('',#48233,#18999,#19000) ;
#16107 = AXIS2_PLACEMENT_3D('',#48236,#19001,#19002) ;
#16108 = AXIS2_PLACEMENT_3D('',#48240,#19004,#19005) ;
#16109 = AXIS2_PLACEMENT_3D('',#48241,#19006,#19007) ;
#16110 = AXIS2_PLACEMENT_3D('',#48242,#19008,#19009) ;
#16111 = AXIS2_PLACEMENT_3D('',#48243,#19010,#19011) ;
#16112 = AXIS2_PLACEMENT_3D('',#48247,#19013,#19014) ;
#16113 = AXIS2_PLACEMENT_3D('',#48248,#19015,#19016) ;
#16114 = AXIS2_PLACEMENT_3D('',#48249,#19017,#19018) ;
#16115 = AXIS2_PLACEMENT_3D('',#48252,#19020,#19021) ;
#16116 = AXIS2_PLACEMENT_3D('',#48253,#19022,#19023) ;
#16117 = AXIS2_PLACEMENT_3D('',#48256,#19025,#19026) ;
#16118 = AXIS2_PLACEMENT_3D('',#48257,#19027,#19028) ;
#16119 = AXIS2_PLACEMENT_3D('',#48259,#19029,#19030) ;
#16120 = AXIS2_PLACEMENT_3D('',#48260,#19031,#19032) ;
#16121 = AXIS2_PLACEMENT_3D('',#48263,#19033,#19034) ;
#16122 = AXIS2_PLACEMENT_3D('',#48266,#19036,#19037) ;
#16123 = AXIS2_PLACEMENT_3D('',#48267,#19038,#19039) ;
#16124 = AXIS2_PLACEMENT_3D('',#48268,#19040,#19041) ;
#16125 = AXIS2_PLACEMENT_3D('',#48270,#19043,#19044) ;
#16126 = AXIS2_PLACEMENT_3D('',#48415,#19045,#19046) ;
#16127 = AXIS2_PLACEMENT_3D('',#48418,#19047,#19048) ;
#16128 = AXIS2_PLACEMENT_3D('',#48421,#19050,#19051) ;
#16129 = AXIS2_PLACEMENT_3D('',#48422,#19052,#19053) ;
#16130 = AXIS2_PLACEMENT_3D('',#48423,#19054,#19055) ;
#16131 = AXIS2_PLACEMENT_3D('',#48427,#19057,#19058) ;
#16132 = AXIS2_PLACEMENT_3D('',#48428,#19059,#19060) ;
#16133 = AXIS2_PLACEMENT_3D('',#48534,#19061,#19062) ;
#16134 = AXIS2_PLACEMENT_3D('',#48536,#19063,#19064) ;
#16135 = AXIS2_PLACEMENT_3D('',#48537,#19065,#19066) ;
#16136 = AXIS2_PLACEMENT_3D('',#48540,#19068,#19069) ;
#16137 = AXIS2_PLACEMENT_3D('',#48541,#19070,#19071) ;
#16138 = AXIS2_PLACEMENT_3D('',#48543,#19072,#19073) ;
#16139 = AXIS2_PLACEMENT_3D('',#48670,#19074,#19075) ;
#16140 = AXIS2_PLACEMENT_3D('',#48797,#19076,#19077) ;
#16141 = AXIS2_PLACEMENT_3D('',#48924,#19078,#19079) ;
#16142 = AXIS2_PLACEMENT_3D('',#50860,#19080,#19081) ;
#16143 = AXIS2_PLACEMENT_3D('',#51819,#19082,#19083) ;
#16144 = AXIS2_PLACEMENT_3D('',#51821,#19084,#19085) ;
#16145 = AXIS2_PLACEMENT_3D('',#51822,#19086,#19087) ;
#16146 = AXIS2_PLACEMENT_3D('',#51828,#19091,#19092) ;
#16147 = AXIS2_PLACEMENT_3D('',#51830,#19093,#19094) ;
#16148 = AXIS2_PLACEMENT_3D('',#51832,#19096,#19097) ;
#16149 = AXIS2_PLACEMENT_3D('',#51836,#19100,#19101) ;
#16150 = AXIS2_PLACEMENT_3D('',#51837,#19102,#19103) ;
#16151 = AXIS2_PLACEMENT_3D('',#51838,#19104,#19105) ;
#16152 = AXIS2_PLACEMENT_3D('',#51839,#19106,#19107) ;
#16153 = AXIS2_PLACEMENT_3D('',#51841,#19108,#19109) ;
#16154 = AXIS2_PLACEMENT_3D('',#51843,#19111,#19112) ;
#16155 = AXIS2_PLACEMENT_3D('',#51845,#19113,#19114) ;
#16156 = AXIS2_PLACEMENT_3D('',#51846,#19115,#19116) ;
#16157 = AXIS2_PLACEMENT_3D('',#51848,#19118,#19119) ;
#16158 = AXIS2_PLACEMENT_3D('',#51850,#19121,#19122) ;
#16159 = AXIS2_PLACEMENT_3D('',#51852,#19123,#19124) ;
#16160 = AXIS2_PLACEMENT_3D('',#51854,#19126,#19127) ;
#16161 = AXIS2_PLACEMENT_3D('',#51856,#19128,#19129) ;
#16162 = AXIS2_PLACEMENT_3D('',#51857,#19130,#19131) ;
#16163 = AXIS2_PLACEMENT_3D('',#51859,#19132,#19133) ;
#16164 = AXIS2_PLACEMENT_3D('',#51861,#19135,#19136) ;
#16165 = AXIS2_PLACEMENT_3D('',#51862,#19137,#19138) ;
#16166 = AXIS2_PLACEMENT_3D('',#51864,#19139,#19140) ;
#16167 = AXIS2_PLACEMENT_3D('',#51866,#19142,#19143) ;
#16168 = AXIS2_PLACEMENT_3D('',#51867,#19144,#19145) ;
#16169 = AXIS2_PLACEMENT_3D('',#51868,#19146,#19147) ;
#16170 = AXIS2_PLACEMENT_3D('',#51871,#19148,#19149) ;
#16171 = AXIS2_PLACEMENT_3D('',#51873,#19150,#19151) ;
#16172 = AXIS2_PLACEMENT_3D('',#51877,#19153,#19154) ;
#16173 = AXIS2_PLACEMENT_3D('',#51879,#19155,#19156) ;
#16174 = AXIS2_PLACEMENT_3D('',#51881,#19157,#19158) ;
#16175 = AXIS2_PLACEMENT_3D('',#51884,#19160,#19161) ;
#16176 = AXIS2_PLACEMENT_3D('',#51885,#19162,#19163) ;
#16177 = AXIS2_PLACEMENT_3D('',#51891,#19167,#19168) ;
#16178 = AXIS2_PLACEMENT_3D('',#51896,#19170,#19171) ;
#16179 = AXIS2_PLACEMENT_3D('',#51898,#19172,#19173) ;
#16180 = AXIS2_PLACEMENT_3D('',#51899,#19174,#19175) ;
#16181 = AXIS2_PLACEMENT_3D('',#51901,#19176,#19177) ;
#16182 = AXIS2_PLACEMENT_3D('',#51903,#19178,#19179) ;
#16183 = AXIS2_PLACEMENT_3D('',#51904,#19180,#19181) ;
#16184 = AXIS2_PLACEMENT_3D('',#51905,#19182,#19183) ;
#16185 = AXIS2_PLACEMENT_3D('',#51908,#19186,#19187) ;
#16186 = AXIS2_PLACEMENT_3D('',#51911,#19190,#19191) ;
#16187 = AXIS2_PLACEMENT_3D('',#51914,#19194,#19195) ;
#16188 = AXIS2_PLACEMENT_3D('',#51915,#19196,#19197) ;
#16189 = AXIS2_PLACEMENT_3D('',#51916,#19198,#19199) ;
#16190 = AXIS2_PLACEMENT_3D('',#51917,#19200,#19201) ;
#16191 = AXIS2_PLACEMENT_3D('',#51918,#19202,#19203) ;
#16192 = AXIS2_PLACEMENT_3D('',#51919,#19204,#19205) ;
#16193 = AXIS2_PLACEMENT_3D('',#51921,#19206,#19207) ;
#16194 = AXIS2_PLACEMENT_3D('',#51924,#19209,#19210) ;
#16195 = AXIS2_PLACEMENT_3D('',#51925,#19211,#19212) ;
#16196 = AXIS2_PLACEMENT_3D('',#51927,#19213,#19214) ;
#16197 = AXIS2_PLACEMENT_3D('',#51928,#19215,#19216) ;
#16198 = AXIS2_PLACEMENT_3D('',#51930,#19217,#19218) ;
#16199 = AXIS2_PLACEMENT_3D('',#51932,#19220,#19221) ;
#16200 = AXIS2_PLACEMENT_3D('',#51934,#19222,#19223) ;
#16201 = AXIS2_PLACEMENT_3D('',#51936,#19225,#19226) ;
#16202 = AXIS2_PLACEMENT_3D('',#51939,#19228,#19229) ;
#16203 = AXIS2_PLACEMENT_3D('',#51940,#19230,#19231) ;
#16204 = AXIS2_PLACEMENT_3D('',#51943,#19233,#19234) ;
#16205 = AXIS2_PLACEMENT_3D('',#51944,#19235,#19236) ;
#16206 = AXIS2_PLACEMENT_3D('',#51946,#19237,#19238) ;
#16207 = AXIS2_PLACEMENT_3D('',#51947,#19239,#19240) ;
#16208 = AXIS2_PLACEMENT_3D('',#51949,#19242,#19243) ;
#16209 = AXIS2_PLACEMENT_3D('',#51950,#19244,#19245) ;
#16210 = AXIS2_PLACEMENT_3D('',#51959,#19250,#19251) ;
#16211 = AXIS2_PLACEMENT_3D('',#51965,#19255,#19256) ;
#16212 = AXIS2_PLACEMENT_3D('',#51971,#19260,#19261) ;
#16213 = AXIS2_PLACEMENT_3D('',#51973,#19262,#19263) ;
#16214 = AXIS2_PLACEMENT_3D('',#51974,#19264,#19265) ;
#16215 = AXIS2_PLACEMENT_3D('',#51975,#19266,#19267) ;
#16216 = AXIS2_PLACEMENT_3D('',#51980,#19269,#19270) ;
#16217 = AXIS2_PLACEMENT_3D('',#51983,#19272,#19273) ;
#16218 = AXIS2_PLACEMENT_3D('',#51984,#19274,#19275) ;
#16219 = AXIS2_PLACEMENT_3D('',#51987,#19276,#19277) ;
#16220 = AXIS2_PLACEMENT_3D('',#51991,#19279,#19280) ;
#16221 = AXIS2_PLACEMENT_3D('',#51993,#19282,#19283) ;
#16222 = AXIS2_PLACEMENT_3D('',#51996,#19284,#19285) ;
#16223 = AXIS2_PLACEMENT_3D('',#52000,#19287,#19288) ;
#16224 = AXIS2_PLACEMENT_3D('',#52002,#19290,#19291) ;
#16225 = AXIS2_PLACEMENT_3D('',#52005,#19292,#19293) ;
#16226 = AXIS2_PLACEMENT_3D('',#52009,#19295,#19296) ;
#16227 = AXIS2_PLACEMENT_3D('',#52011,#19298,#19299) ;
#16228 = AXIS2_PLACEMENT_3D('',#52016,#19301,#19302) ;
#16229 = AXIS2_PLACEMENT_3D('',#52019,#19304,#19305) ;
#16230 = AXIS2_PLACEMENT_3D('',#52020,#19306,#19307) ;
#16231 = AXIS2_PLACEMENT_3D('',#52025,#19309,#19310) ;
#16232 = AXIS2_PLACEMENT_3D('',#52028,#19312,#19313) ;
#16233 = AXIS2_PLACEMENT_3D('',#52029,#19314,#19315) ;
#16234 = AXIS2_PLACEMENT_3D('',#52034,#19317,#19318) ;
#16235 = AXIS2_PLACEMENT_3D('',#52037,#19320,#19321) ;
#16236 = AXIS2_PLACEMENT_3D('',#52038,#19322,#19323) ;
#16237 = AXIS2_PLACEMENT_3D('',#52041,#19324,#19325) ;
#16238 = AXIS2_PLACEMENT_3D('',#52045,#19327,#19328) ;
#16239 = AXIS2_PLACEMENT_3D('',#52047,#19330,#19331) ;
#16240 = AXIS2_PLACEMENT_3D('',#52050,#19332,#19333) ;
#16241 = AXIS2_PLACEMENT_3D('',#52054,#19335,#19336) ;
#16242 = AXIS2_PLACEMENT_3D('',#52056,#19338,#19339) ;
#16243 = AXIS2_PLACEMENT_3D('',#52059,#19340,#19341) ;
#16244 = AXIS2_PLACEMENT_3D('',#52063,#19343,#19344) ;
#16245 = AXIS2_PLACEMENT_3D('',#52065,#19346,#19347) ;
#16246 = AXIS2_PLACEMENT_3D('',#52068,#19348,#19349) ;
#16247 = AXIS2_PLACEMENT_3D('',#52072,#19351,#19352) ;
#16248 = AXIS2_PLACEMENT_3D('',#52074,#19354,#19355) ;
#16249 = AXIS2_PLACEMENT_3D('',#52077,#19356,#19357) ;
#16250 = AXIS2_PLACEMENT_3D('',#52081,#19359,#19360) ;
#16251 = AXIS2_PLACEMENT_3D('',#52083,#19362,#19363) ;
#16252 = AXIS2_PLACEMENT_3D('',#52086,#19364,#19365) ;
#16253 = AXIS2_PLACEMENT_3D('',#52090,#19367,#19368) ;
#16254 = AXIS2_PLACEMENT_3D('',#52092,#19370,#19371) ;
#16255 = AXIS2_PLACEMENT_3D('',#52095,#19372,#19373) ;
#16256 = AXIS2_PLACEMENT_3D('',#52099,#19375,#19376) ;
#16257 = AXIS2_PLACEMENT_3D('',#52101,#19378,#19379) ;
#16258 = AXIS2_PLACEMENT_3D('',#52104,#19380,#19381) ;
#16259 = AXIS2_PLACEMENT_3D('',#52108,#19383,#19384) ;
#16260 = AXIS2_PLACEMENT_3D('',#52110,#19386,#19387) ;
#16261 = AXIS2_PLACEMENT_3D('',#52113,#19388,#19389) ;
#16262 = AXIS2_PLACEMENT_3D('',#52117,#19391,#19392) ;
#16263 = AXIS2_PLACEMENT_3D('',#52119,#19394,#19395) ;
#16264 = AXIS2_PLACEMENT_3D('',#52122,#19396,#19397) ;
#16265 = AXIS2_PLACEMENT_3D('',#52126,#19399,#19400) ;
#16266 = AXIS2_PLACEMENT_3D('',#52128,#19402,#19403) ;
#16267 = AXIS2_PLACEMENT_3D('',#52131,#19404,#19405) ;
#16268 = AXIS2_PLACEMENT_3D('',#52135,#19407,#19408) ;
#16269 = AXIS2_PLACEMENT_3D('',#52137,#19410,#19411) ;
#16270 = AXIS2_PLACEMENT_3D('',#52140,#19412,#19413) ;
#16271 = AXIS2_PLACEMENT_3D('',#52144,#19415,#19416) ;
#16272 = AXIS2_PLACEMENT_3D('',#52146,#19418,#19419) ;
#16273 = AXIS2_PLACEMENT_3D('',#52149,#19420,#19421) ;
#16274 = AXIS2_PLACEMENT_3D('',#52153,#19423,#19424) ;
#16275 = AXIS2_PLACEMENT_3D('',#52155,#19426,#19427) ;
#16276 = AXIS2_PLACEMENT_3D('',#52160,#19429,#19430) ;
#16277 = AXIS2_PLACEMENT_3D('',#52163,#19432,#19433) ;
#16278 = AXIS2_PLACEMENT_3D('',#52164,#19434,#19435) ;
#16279 = AXIS2_PLACEMENT_3D('',#52167,#19436,#19437) ;
#16280 = AXIS2_PLACEMENT_3D('',#52171,#19439,#19440) ;
#16281 = AXIS2_PLACEMENT_3D('',#52173,#19442,#19443) ;
#16282 = AXIS2_PLACEMENT_3D('',#52176,#19444,#19445) ;
#16283 = AXIS2_PLACEMENT_3D('',#52180,#19447,#19448) ;
#16284 = AXIS2_PLACEMENT_3D('',#52182,#19450,#19451) ;
#16285 = AXIS2_PLACEMENT_3D('',#52185,#19452,#19453) ;
#16286 = AXIS2_PLACEMENT_3D('',#52189,#19455,#19456) ;
#16287 = AXIS2_PLACEMENT_3D('',#52191,#19458,#19459) ;
#16288 = AXIS2_PLACEMENT_3D('',#52194,#19460,#19461) ;
#16289 = AXIS2_PLACEMENT_3D('',#52198,#19463,#19464) ;
#16290 = AXIS2_PLACEMENT_3D('',#52200,#19466,#19467) ;
#16291 = AXIS2_PLACEMENT_3D('',#52203,#19468,#19469) ;
#16292 = AXIS2_PLACEMENT_3D('',#52207,#19471,#19472) ;
#16293 = AXIS2_PLACEMENT_3D('',#52209,#19474,#19475) ;
#16294 = AXIS2_PLACEMENT_3D('',#52212,#19476,#19477) ;
#16295 = AXIS2_PLACEMENT_3D('',#52216,#19479,#19480) ;
#16296 = AXIS2_PLACEMENT_3D('',#52218,#19482,#19483) ;
#16297 = AXIS2_PLACEMENT_3D('',#52221,#19484,#19485) ;
#16298 = AXIS2_PLACEMENT_3D('',#52225,#19487,#19488) ;
#16299 = AXIS2_PLACEMENT_3D('',#52227,#19490,#19491) ;
#16300 = AXIS2_PLACEMENT_3D('',#52230,#19492,#19493) ;
#16301 = AXIS2_PLACEMENT_3D('',#52234,#19495,#19496) ;
#16302 = AXIS2_PLACEMENT_3D('',#52236,#19498,#19499) ;
#16303 = AXIS2_PLACEMENT_3D('',#52239,#19500,#19501) ;
#16304 = AXIS2_PLACEMENT_3D('',#52243,#19503,#19504) ;
#16305 = AXIS2_PLACEMENT_3D('',#52245,#19506,#19507) ;
#16306 = AXIS2_PLACEMENT_3D('',#52248,#19508,#19509) ;
#16307 = AXIS2_PLACEMENT_3D('',#52252,#19511,#19512) ;
#16308 = AXIS2_PLACEMENT_3D('',#52254,#19514,#19515) ;
#16309 = AXIS2_PLACEMENT_3D('',#52257,#19516,#19517) ;
#16310 = AXIS2_PLACEMENT_3D('',#52261,#19519,#19520) ;
#16311 = AXIS2_PLACEMENT_3D('',#52263,#19522,#19523) ;
#16312 = AXIS2_PLACEMENT_3D('',#52268,#19525,#19526) ;
#16313 = AXIS2_PLACEMENT_3D('',#52271,#19528,#19529) ;
#16314 = AXIS2_PLACEMENT_3D('',#52272,#19530,#19531) ;
#16315 = AXIS2_PLACEMENT_3D('',#52277,#19533,#19534) ;
#16316 = AXIS2_PLACEMENT_3D('',#52280,#19536,#19537) ;
#16317 = AXIS2_PLACEMENT_3D('',#52281,#19538,#19539) ;
#16318 = AXIS2_PLACEMENT_3D('',#52286,#19541,#19542) ;
#16319 = AXIS2_PLACEMENT_3D('',#52289,#19544,#19545) ;
#16320 = AXIS2_PLACEMENT_3D('',#52290,#19546,#19547) ;
#16321 = AXIS2_PLACEMENT_3D('',#52295,#19549,#19550) ;
#16322 = AXIS2_PLACEMENT_3D('',#52298,#19552,#19553) ;
#16323 = AXIS2_PLACEMENT_3D('',#52299,#19554,#19555) ;
#16324 = AXIS2_PLACEMENT_3D('',#52304,#19557,#19558) ;
#16325 = AXIS2_PLACEMENT_3D('',#52307,#19560,#19561) ;
#16326 = AXIS2_PLACEMENT_3D('',#52308,#19562,#19563) ;
#16327 = AXIS2_PLACEMENT_3D('',#52313,#19565,#19566) ;
#16328 = AXIS2_PLACEMENT_3D('',#52316,#19568,#19569) ;
#16329 = AXIS2_PLACEMENT_3D('',#52317,#19570,#19571) ;
#16330 = AXIS2_PLACEMENT_3D('',#52322,#19573,#19574) ;
#16331 = AXIS2_PLACEMENT_3D('',#52325,#19576,#19577) ;
#16332 = AXIS2_PLACEMENT_3D('',#52326,#19578,#19579) ;
#16333 = AXIS2_PLACEMENT_3D('',#52329,#19580,#19581) ;
#16334 = AXIS2_PLACEMENT_3D('',#52333,#19583,#19584) ;
#16335 = AXIS2_PLACEMENT_3D('',#52335,#19586,#19587) ;
#16336 = AXIS2_PLACEMENT_3D('',#52338,#19588,#19589) ;
#16337 = AXIS2_PLACEMENT_3D('',#52342,#19591,#19592) ;
#16338 = AXIS2_PLACEMENT_3D('',#52344,#19594,#19595) ;
#16339 = AXIS2_PLACEMENT_3D('',#52347,#19596,#19597) ;
#16340 = AXIS2_PLACEMENT_3D('',#52351,#19599,#19600) ;
#16341 = AXIS2_PLACEMENT_3D('',#52353,#19602,#19603) ;
#16342 = AXIS2_PLACEMENT_3D('',#52356,#19604,#19605) ;
#16343 = AXIS2_PLACEMENT_3D('',#52360,#19607,#19608) ;
#16344 = AXIS2_PLACEMENT_3D('',#52362,#19610,#19611) ;
#16345 = AXIS2_PLACEMENT_3D('',#52365,#19612,#19613) ;
#16346 = AXIS2_PLACEMENT_3D('',#52369,#19615,#19616) ;
#16347 = AXIS2_PLACEMENT_3D('',#52371,#19618,#19619) ;
#16348 = AXIS2_PLACEMENT_3D('',#52374,#19620,#19621) ;
#16349 = AXIS2_PLACEMENT_3D('',#52378,#19623,#19624) ;
#16350 = AXIS2_PLACEMENT_3D('',#52380,#19626,#19627) ;
#16351 = AXIS2_PLACEMENT_3D('',#52383,#19628,#19629) ;
#16352 = AXIS2_PLACEMENT_3D('',#52387,#19631,#19632) ;
#16353 = AXIS2_PLACEMENT_3D('',#52389,#19634,#19635) ;
#16354 = AXIS2_PLACEMENT_3D('',#52392,#19636,#19637) ;
#16355 = AXIS2_PLACEMENT_3D('',#52396,#19639,#19640) ;
#16356 = AXIS2_PLACEMENT_3D('',#52398,#19642,#19643) ;
#16357 = AXIS2_PLACEMENT_3D('',#52401,#19644,#19645) ;
#16358 = AXIS2_PLACEMENT_3D('',#52405,#19647,#19648) ;
#16359 = AXIS2_PLACEMENT_3D('',#52407,#19650,#19651) ;
#16360 = AXIS2_PLACEMENT_3D('',#52410,#19652,#19653) ;
#16361 = AXIS2_PLACEMENT_3D('',#52414,#19655,#19656) ;
#16362 = AXIS2_PLACEMENT_3D('',#52416,#19658,#19659) ;
#16363 = AXIS2_PLACEMENT_3D('',#52419,#19660,#19661) ;
#16364 = AXIS2_PLACEMENT_3D('',#52423,#19663,#19664) ;
#16365 = AXIS2_PLACEMENT_3D('',#52425,#19666,#19667) ;
#16366 = AXIS2_PLACEMENT_3D('',#52430,#19669,#19670) ;
#16367 = AXIS2_PLACEMENT_3D('',#52433,#19672,#19673) ;
#16368 = AXIS2_PLACEMENT_3D('',#52434,#19674,#19675) ;
#16369 = AXIS2_PLACEMENT_3D('',#52437,#19676,#19677) ;
#16370 = AXIS2_PLACEMENT_3D('',#52441,#19679,#19680) ;
#16371 = AXIS2_PLACEMENT_3D('',#52443,#19682,#19683) ;
#16372 = AXIS2_PLACEMENT_3D('',#52446,#19684,#19685) ;
#16373 = AXIS2_PLACEMENT_3D('',#52450,#19687,#19688) ;
#16374 = AXIS2_PLACEMENT_3D('',#52452,#19690,#19691) ;
#16375 = AXIS2_PLACEMENT_3D('',#52455,#19692,#19693) ;
#16376 = AXIS2_PLACEMENT_3D('',#52459,#19695,#19696) ;
#16377 = AXIS2_PLACEMENT_3D('',#52461,#19698,#19699) ;
#16378 = AXIS2_PLACEMENT_3D('',#52464,#19700,#19701) ;
#16379 = AXIS2_PLACEMENT_3D('',#52468,#19703,#19704) ;
#16380 = AXIS2_PLACEMENT_3D('',#52470,#19706,#19707) ;
#16381 = AXIS2_PLACEMENT_3D('',#52473,#19708,#19709) ;
#16382 = AXIS2_PLACEMENT_3D('',#52477,#19711,#19712) ;
#16383 = AXIS2_PLACEMENT_3D('',#52479,#19714,#19715) ;
#16384 = AXIS2_PLACEMENT_3D('',#52482,#19716,#19717) ;
#16385 = AXIS2_PLACEMENT_3D('',#52486,#19719,#19720) ;
#16386 = AXIS2_PLACEMENT_3D('',#52488,#19722,#19723) ;
#16387 = AXIS2_PLACEMENT_3D('',#52491,#19724,#19725) ;
#16388 = AXIS2_PLACEMENT_3D('',#52495,#19727,#19728) ;
#16389 = AXIS2_PLACEMENT_3D('',#52497,#19730,#19731) ;
#16390 = AXIS2_PLACEMENT_3D('',#52502,#19733,#19734) ;
#16391 = AXIS2_PLACEMENT_3D('',#52505,#19736,#19737) ;
#16392 = AXIS2_PLACEMENT_3D('',#52506,#19738,#19739) ;
#16393 = AXIS2_PLACEMENT_3D('',#52509,#19740,#19741) ;
#16394 = AXIS2_PLACEMENT_3D('',#52513,#19743,#19744) ;
#16395 = AXIS2_PLACEMENT_3D('',#52515,#19746,#19747) ;
#16396 = AXIS2_PLACEMENT_3D('',#52517,#19748,#19749) ;
#16397 = AXIS2_PLACEMENT_3D('',#52519,#19751,#19752) ;
#16398 = AXIS2_PLACEMENT_3D('',#52521,#19753,#19754) ;
#16399 = AXIS2_PLACEMENT_3D('',#52522,#19755,#19756) ;
#16400 = AXIS2_PLACEMENT_3D('',#52526,#19758,#19759) ;
#16401 = AXIS2_PLACEMENT_3D('',#52527,#19760,#19761) ;
#16402 = AXIS2_PLACEMENT_3D('',#52528,#19762,#19763) ;
#16403 = AXIS2_PLACEMENT_3D('',#52531,#19764,#19765) ;
#16404 = AXIS2_PLACEMENT_3D('',#52532,#19766,#19767) ;
#16405 = AXIS2_PLACEMENT_3D('',#52534,#19769,#19770) ;
#16406 = AXIS2_PLACEMENT_3D('',#52537,#19772,#19773) ;
#16407 = AXIS2_PLACEMENT_3D('',#52538,#19774,#19775) ;
#16408 = AXIS2_PLACEMENT_3D('',#52539,#19776,#19777) ;
#16409 = AXIS2_PLACEMENT_3D('',#52540,#19778,#19779) ;
#16410 = AXIS2_PLACEMENT_3D('',#52541,#19780,#19781) ;
#16411 = AXIS2_PLACEMENT_3D('',#52542,#19782,#19783) ;
#16412 = AXIS2_PLACEMENT_3D('',#52543,#19784,#19785) ;
#16413 = AXIS2_PLACEMENT_3D('',#52544,#19786,#19787) ;
#16414 = AXIS2_PLACEMENT_3D('',#52545,#19788,#19789) ;
#16415 = AXIS2_PLACEMENT_3D('',#52546,#19790,#19791) ;
#16416 = AXIS2_PLACEMENT_3D('',#52547,#19792,#19793) ;
#16417 = AXIS2_PLACEMENT_3D('',#52548,#19794,#19795) ;
#16418 = AXIS2_PLACEMENT_3D('',#52549,#19796,#19797) ;
#16419 = AXIS2_PLACEMENT_3D('',#52550,#19798,#19799) ;
#16420 = AXIS2_PLACEMENT_3D('',#52551,#19800,#19801) ;
#16421 = AXIS2_PLACEMENT_3D('',#52552,#19802,#19803) ;
#16422 = AXIS2_PLACEMENT_3D('',#52553,#19804,#19805) ;
#16423 = AXIS2_PLACEMENT_3D('',#52554,#19806,#19807) ;
#16424 = AXIS2_PLACEMENT_3D('',#52555,#19808,#19809) ;
#16425 = AXIS2_PLACEMENT_3D('',#52556,#19810,#19811) ;
#16426 = AXIS2_PLACEMENT_3D('',#52557,#19812,#19813) ;
#16427 = AXIS2_PLACEMENT_3D('',#52558,#19814,#19815) ;
#16428 = AXIS2_PLACEMENT_3D('',#52559,#19816,#19817) ;
#16429 = AXIS2_PLACEMENT_3D('',#52560,#19818,#19819) ;
#16430 = AXIS2_PLACEMENT_3D('',#52561,#19820,#19821) ;
#16431 = AXIS2_PLACEMENT_3D('',#52562,#19822,#19823) ;
#16432 = AXIS2_PLACEMENT_3D('',#52563,#19824,#19825) ;
#16433 = AXIS2_PLACEMENT_3D('',#52564,#19826,#19827) ;
#16434 = AXIS2_PLACEMENT_3D('',#52565,#19828,#19829) ;
#16435 = AXIS2_PLACEMENT_3D('',#52566,#19830,#19831) ;
#16436 = AXIS2_PLACEMENT_3D('',#52567,#19832,#19833) ;
#16437 = AXIS2_PLACEMENT_3D('',#52568,#19834,#19835) ;
#16438 = AXIS2_PLACEMENT_3D('',#52569,#19836,#19837) ;
#16439 = AXIS2_PLACEMENT_3D('',#52570,#19838,#19839) ;
#16440 = AXIS2_PLACEMENT_3D('',#52571,#19840,#19841) ;
#16441 = AXIS2_PLACEMENT_3D('',#52572,#19842,#19843) ;
#16442 = AXIS2_PLACEMENT_3D('',#52573,#19844,#19845) ;
#16443 = AXIS2_PLACEMENT_3D('',#52574,#19846,#19847) ;
#16444 = AXIS2_PLACEMENT_3D('',#52575,#19848,#19849) ;
#16445 = AXIS2_PLACEMENT_3D('',#52576,#19850,#19851) ;
#16446 = AXIS2_PLACEMENT_3D('',#52577,#19852,#19853) ;
#16447 = AXIS2_PLACEMENT_3D('',#52578,#19854,#19855) ;
#16448 = AXIS2_PLACEMENT_3D('',#52579,#19856,#19857) ;
#16449 = AXIS2_PLACEMENT_3D('',#52580,#19858,#19859) ;
#16450 = AXIS2_PLACEMENT_3D('',#52581,#19860,#19861) ;
#16451 = AXIS2_PLACEMENT_3D('',#52582,#19862,#19863) ;
#16452 = AXIS2_PLACEMENT_3D('',#52583,#19864,#19865) ;
#16453 = AXIS2_PLACEMENT_3D('',#52584,#19866,#19867) ;
#16454 = AXIS2_PLACEMENT_3D('',#52585,#19868,#19869) ;
#16455 = AXIS2_PLACEMENT_3D('',#52586,#19870,#19871) ;
#16456 = AXIS2_PLACEMENT_3D('',#52587,#19872,#19873) ;
#16457 = AXIS2_PLACEMENT_3D('',#52588,#19874,#19875) ;
#16458 = AXIS2_PLACEMENT_3D('',#52589,#19876,#19877) ;
#16459 = AXIS2_PLACEMENT_3D('',#52590,#19878,#19879) ;
#16460 = AXIS2_PLACEMENT_3D('',#52591,#19880,#19881) ;
#16461 = AXIS2_PLACEMENT_3D('',#52592,#19882,#19883) ;
#16462 = AXIS2_PLACEMENT_3D('',#52593,#19884,#19885) ;
#16463 = AXIS2_PLACEMENT_3D('',#52594,#19886,#19887) ;
#16464 = AXIS2_PLACEMENT_3D('',#52595,#19888,#19889) ;
#16465 = AXIS2_PLACEMENT_3D('',#52596,#19890,#19891) ;
#16466 = AXIS2_PLACEMENT_3D('',#52597,#19892,#19893) ;
#16467 = AXIS2_PLACEMENT_3D('',#52598,#19894,#19895) ;
#16468 = AXIS2_PLACEMENT_3D('',#52601,#19896,#19897) ;
#16469 = AXIS2_PLACEMENT_3D('',#52602,#19898,#19899) ;
#16470 = AXIS2_PLACEMENT_3D('',#52605,#19901,#19902) ;
#16471 = AXIS2_PLACEMENT_3D('',#52606,#19903,#19904) ;
#16472 = AXIS2_PLACEMENT_3D('',#52607,#19905,#19906) ;
#16473 = AXIS2_PLACEMENT_3D('',#52608,#19907,#19908) ;
#16474 = AXIS2_PLACEMENT_3D('',#52609,#19909,#19910) ;
#16475 = AXIS2_PLACEMENT_3D('',#52610,#19911,#19912) ;
#16476 = AXIS2_PLACEMENT_3D('',#52611,#19913,#19914) ;
#16477 = AXIS2_PLACEMENT_3D('',#52612,#19915,#19916) ;
#16478 = AXIS2_PLACEMENT_3D('',#52613,#19917,#19918) ;
#16479 = AXIS2_PLACEMENT_3D('',#52614,#19919,#19920) ;
#16480 = AXIS2_PLACEMENT_3D('',#52615,#19921,#19922) ;
#16481 = AXIS2_PLACEMENT_3D('',#52616,#19923,#19924) ;
#16482 = AXIS2_PLACEMENT_3D('',#52617,#19925,#19926) ;
#16483 = AXIS2_PLACEMENT_3D('',#52618,#19927,#19928) ;
#16484 = AXIS2_PLACEMENT_3D('',#52619,#19929,#19930) ;
#16485 = AXIS2_PLACEMENT_3D('',#52620,#19931,#19932) ;
#16486 = AXIS2_PLACEMENT_3D('',#52621,#19933,#19934) ;
#16487 = AXIS2_PLACEMENT_3D('',#52622,#19935,#19936) ;
#16488 = AXIS2_PLACEMENT_3D('',#52623,#19937,#19938) ;
#16489 = AXIS2_PLACEMENT_3D('',#52624,#19939,#19940) ;
#16490 = AXIS2_PLACEMENT_3D('',#52625,#19941,#19942) ;
#16491 = AXIS2_PLACEMENT_3D('',#52626,#19943,#19944) ;
#16492 = AXIS2_PLACEMENT_3D('',#52627,#19945,#19946) ;
#16493 = AXIS2_PLACEMENT_3D('',#52628,#19947,#19948) ;
#16494 = AXIS2_PLACEMENT_3D('',#52629,#19949,#19950) ;
#16495 = AXIS2_PLACEMENT_3D('',#52630,#19951,#19952) ;
#16496 = AXIS2_PLACEMENT_3D('',#52631,#19953,#19954) ;
#16497 = AXIS2_PLACEMENT_3D('',#52632,#19955,#19956) ;
#16498 = AXIS2_PLACEMENT_3D('',#52633,#19957,#19958) ;
#16499 = AXIS2_PLACEMENT_3D('',#52634,#19959,#19960) ;
#16500 = AXIS2_PLACEMENT_3D('',#52635,#19961,#19962) ;
#16501 = AXIS2_PLACEMENT_3D('',#52636,#19963,#19964) ;
#16502 = AXIS2_PLACEMENT_3D('',#52637,#19965,#19966) ;
#16503 = AXIS2_PLACEMENT_3D('',#52638,#19967,#19968) ;
#16504 = AXIS2_PLACEMENT_3D('',#52639,#19969,#19970) ;
#16505 = AXIS2_PLACEMENT_3D('',#52640,#19971,#19972) ;
#16506 = AXIS2_PLACEMENT_3D('',#52641,#19973,#19974) ;
#16507 = AXIS2_PLACEMENT_3D('',#52642,#19975,#19976) ;
#16508 = AXIS2_PLACEMENT_3D('',#52643,#19977,#19978) ;
#16509 = AXIS2_PLACEMENT_3D('',#52644,#19979,#19980) ;
#16510 = AXIS2_PLACEMENT_3D('',#52645,#19981,#19982) ;
#16511 = AXIS2_PLACEMENT_3D('',#52646,#19983,#19984) ;
#16512 = AXIS2_PLACEMENT_3D('',#52647,#19985,#19986) ;
#16513 = AXIS2_PLACEMENT_3D('',#52648,#19987,#19988) ;
#16514 = AXIS2_PLACEMENT_3D('',#52649,#19989,#19990) ;
#16515 = AXIS2_PLACEMENT_3D('',#52650,#19991,#19992) ;
#16516 = AXIS2_PLACEMENT_3D('',#52651,#19993,#19994) ;
#16517 = AXIS2_PLACEMENT_3D('',#52652,#19995,#19996) ;
#16518 = AXIS2_PLACEMENT_3D('',#52653,#19997,#19998) ;
#16519 = AXIS2_PLACEMENT_3D('',#52654,#19999,#20000) ;
#16520 = AXIS2_PLACEMENT_3D('',#52655,#20001,#20002) ;
#16521 = AXIS2_PLACEMENT_3D('',#52656,#20003,#20004) ;
#16522 = AXIS2_PLACEMENT_3D('',#52657,#20005,#20006) ;
#16523 = AXIS2_PLACEMENT_3D('',#52658,#20007,#20008) ;
#16524 = AXIS2_PLACEMENT_3D('',#52659,#20009,#20010) ;
#16525 = AXIS2_PLACEMENT_3D('',#52660,#20011,#20012) ;
#16526 = AXIS2_PLACEMENT_3D('',#52661,#20013,#20014) ;
#16527 = AXIS2_PLACEMENT_3D('',#52662,#20015,#20016) ;
#16528 = AXIS2_PLACEMENT_3D('',#52663,#20017,#20018) ;
#16529 = AXIS2_PLACEMENT_3D('',#52664,#20019,#20020) ;
#16530 = AXIS2_PLACEMENT_3D('',#52665,#20021,#20022) ;
#16531 = AXIS2_PLACEMENT_3D('',#52666,#20023,#20024) ;
#16532 = AXIS2_PLACEMENT_3D('',#52670,#20026,#20027) ;
#16533 = AXIS2_PLACEMENT_3D('',#52671,#20028,#20029) ;
#16534 = AXIS2_PLACEMENT_3D('',#52672,#20030,#20031) ;
#16535 = AXIS2_PLACEMENT_3D('',#52674,#20032,#20033) ;
#16536 = AXIS2_PLACEMENT_3D('',#52676,#20035,#20036) ;
#16537 = AXIS2_PLACEMENT_3D('',#52678,#20037,#20038) ;
#16538 = AXIS2_PLACEMENT_3D('',#52679,#20039,#20040) ;
#16539 = AXIS2_PLACEMENT_3D('',#52681,#20041,#20042) ;
#16540 = AXIS2_PLACEMENT_3D('',#52683,#20044,#20045) ;
#16541 = AXIS2_PLACEMENT_3D('',#52685,#20046,#20047) ;
#16542 = AXIS2_PLACEMENT_3D('',#52686,#20048,#20049) ;
#16543 = AXIS2_PLACEMENT_3D('',#52688,#20050,#20051) ;
#16544 = AXIS2_PLACEMENT_3D('',#52690,#20053,#20054) ;
#16545 = AXIS2_PLACEMENT_3D('',#52691,#20055,#20056) ;
#16546 = AXIS2_PLACEMENT_3D('',#52692,#20057,#20058) ;
#16547 = AXIS2_PLACEMENT_3D('',#52694,#20059,#20060) ;
#16548 = AXIS2_PLACEMENT_3D('',#52696,#20061,#20062) ;
#16549 = AXIS2_PLACEMENT_3D('',#52697,#20063,#20064) ;
#16550 = AXIS2_PLACEMENT_3D('',#52698,#20065,#20066) ;
#16551 = AXIS2_PLACEMENT_3D('',#52700,#20067,#20068) ;
#16552 = AXIS2_PLACEMENT_3D('',#52702,#20069,#20070) ;
#16553 = AXIS2_PLACEMENT_3D('',#52703,#20071,#20072) ;
#16554 = AXIS2_PLACEMENT_3D('',#52704,#20073,#20074) ;
#16555 = AXIS2_PLACEMENT_3D('',#52706,#20076,#20077) ;
#16556 = AXIS2_PLACEMENT_3D('',#52708,#20079,#20080) ;
#16557 = AXIS2_PLACEMENT_3D('',#52709,#20081,#20082) ;
#16558 = AXIS2_PLACEMENT_3D('',#52711,#20083,#20084) ;
#16559 = AXIS2_PLACEMENT_3D('',#52713,#20085,#20086) ;
#16560 = AXIS2_PLACEMENT_3D('',#52714,#20087,#20088) ;
#16561 = AXIS2_PLACEMENT_3D('',#52715,#20089,#20090) ;
#16562 = AXIS2_PLACEMENT_3D('',#52717,#20091,#20092) ;
#16563 = AXIS2_PLACEMENT_3D('',#52719,#20093,#20094) ;
#16564 = AXIS2_PLACEMENT_3D('',#52720,#20095,#20096) ;
#16565 = AXIS2_PLACEMENT_3D('',#52721,#20097,#20098) ;
#16566 = AXIS2_PLACEMENT_3D('',#52723,#20100,#20101) ;
#16567 = AXIS2_PLACEMENT_3D('',#52725,#20103,#20104) ;
#16568 = AXIS2_PLACEMENT_3D('',#52726,#20105,#20106) ;
#16569 = AXIS2_PLACEMENT_3D('',#52728,#20107,#20108) ;
#16570 = AXIS2_PLACEMENT_3D('',#52730,#20109,#20110) ;
#16571 = AXIS2_PLACEMENT_3D('',#52731,#20111,#20112) ;
#16572 = AXIS2_PLACEMENT_3D('',#52732,#20113,#20114) ;
#16573 = AXIS2_PLACEMENT_3D('',#52734,#20115,#20116) ;
#16574 = AXIS2_PLACEMENT_3D('',#52736,#20117,#20118) ;
#16575 = AXIS2_PLACEMENT_3D('',#52737,#20119,#20120) ;
#16576 = AXIS2_PLACEMENT_3D('',#52738,#20121,#20122) ;
#16577 = AXIS2_PLACEMENT_3D('',#52740,#20124,#20125) ;
#16578 = AXIS2_PLACEMENT_3D('',#52742,#20127,#20128) ;
#16579 = AXIS2_PLACEMENT_3D('',#52743,#20129,#20130) ;
#16580 = AXIS2_PLACEMENT_3D('',#52745,#20131,#20132) ;
#16581 = AXIS2_PLACEMENT_3D('',#52747,#20133,#20134) ;
#16582 = AXIS2_PLACEMENT_3D('',#52748,#20135,#20136) ;
#16583 = AXIS2_PLACEMENT_3D('',#52749,#20137,#20138) ;
#16584 = AXIS2_PLACEMENT_3D('',#52751,#20139,#20140) ;
#16585 = AXIS2_PLACEMENT_3D('',#52753,#20141,#20142) ;
#16586 = AXIS2_PLACEMENT_3D('',#52754,#20143,#20144) ;
#16587 = AXIS2_PLACEMENT_3D('',#52755,#20145,#20146) ;
#16588 = AXIS2_PLACEMENT_3D('',#52757,#20148,#20149) ;
#16589 = AXIS2_PLACEMENT_3D('',#52759,#20151,#20152) ;
#16590 = AXIS2_PLACEMENT_3D('',#52760,#20153,#20154) ;
#16591 = AXIS2_PLACEMENT_3D('',#52762,#20155,#20156) ;
#16592 = AXIS2_PLACEMENT_3D('',#52764,#20157,#20158) ;
#16593 = AXIS2_PLACEMENT_3D('',#52765,#20159,#20160) ;
#16594 = AXIS2_PLACEMENT_3D('',#52766,#20161,#20162) ;
#16595 = AXIS2_PLACEMENT_3D('',#52768,#20163,#20164) ;
#16596 = AXIS2_PLACEMENT_3D('',#52770,#20165,#20166) ;
#16597 = AXIS2_PLACEMENT_3D('',#52771,#20167,#20168) ;
#16598 = AXIS2_PLACEMENT_3D('',#52772,#20169,#20170) ;
#16599 = AXIS2_PLACEMENT_3D('',#52774,#20172,#20173) ;
#16600 = AXIS2_PLACEMENT_3D('',#52776,#20175,#20176) ;
#16601 = AXIS2_PLACEMENT_3D('',#52777,#20177,#20178) ;
#16602 = AXIS2_PLACEMENT_3D('',#52779,#20179,#20180) ;
#16603 = AXIS2_PLACEMENT_3D('',#52781,#20181,#20182) ;
#16604 = AXIS2_PLACEMENT_3D('',#52782,#20183,#20184) ;
#16605 = AXIS2_PLACEMENT_3D('',#52783,#20185,#20186) ;
#16606 = AXIS2_PLACEMENT_3D('',#52785,#20187,#20188) ;
#16607 = AXIS2_PLACEMENT_3D('',#52787,#20189,#20190) ;
#16608 = AXIS2_PLACEMENT_3D('',#52788,#20191,#20192) ;
#16609 = AXIS2_PLACEMENT_3D('',#52789,#20193,#20194) ;
#16610 = AXIS2_PLACEMENT_3D('',#52791,#20196,#20197) ;
#16611 = AXIS2_PLACEMENT_3D('',#52793,#20199,#20200) ;
#16612 = AXIS2_PLACEMENT_3D('',#52794,#20201,#20202) ;
#16613 = AXIS2_PLACEMENT_3D('',#52796,#20203,#20204) ;
#16614 = AXIS2_PLACEMENT_3D('',#52798,#20205,#20206) ;
#16615 = AXIS2_PLACEMENT_3D('',#52799,#20207,#20208) ;
#16616 = AXIS2_PLACEMENT_3D('',#52800,#20209,#20210) ;
#16617 = AXIS2_PLACEMENT_3D('',#52802,#20211,#20212) ;
#16618 = AXIS2_PLACEMENT_3D('',#52804,#20213,#20214) ;
#16619 = AXIS2_PLACEMENT_3D('',#52805,#20215,#20216) ;
#16620 = AXIS2_PLACEMENT_3D('',#52806,#20217,#20218) ;
#16621 = AXIS2_PLACEMENT_3D('',#52808,#20220,#20221) ;
#16622 = AXIS2_PLACEMENT_3D('',#52810,#20223,#20224) ;
#16623 = AXIS2_PLACEMENT_3D('',#52811,#20225,#20226) ;
#16624 = AXIS2_PLACEMENT_3D('',#52813,#20227,#20228) ;
#16625 = AXIS2_PLACEMENT_3D('',#52815,#20229,#20230) ;
#16626 = AXIS2_PLACEMENT_3D('',#52816,#20231,#20232) ;
#16627 = AXIS2_PLACEMENT_3D('',#52817,#20233,#20234) ;
#16628 = AXIS2_PLACEMENT_3D('',#52819,#20235,#20236) ;
#16629 = AXIS2_PLACEMENT_3D('',#52821,#20237,#20238) ;
#16630 = AXIS2_PLACEMENT_3D('',#52822,#20239,#20240) ;
#16631 = AXIS2_PLACEMENT_3D('',#52823,#20241,#20242) ;
#16632 = AXIS2_PLACEMENT_3D('',#52825,#20244,#20245) ;
#16633 = AXIS2_PLACEMENT_3D('',#52827,#20247,#20248) ;
#16634 = AXIS2_PLACEMENT_3D('',#52828,#20249,#20250) ;
#16635 = AXIS2_PLACEMENT_3D('',#52830,#20251,#20252) ;
#16636 = AXIS2_PLACEMENT_3D('',#52832,#20253,#20254) ;
#16637 = AXIS2_PLACEMENT_3D('',#52833,#20255,#20256) ;
#16638 = AXIS2_PLACEMENT_3D('',#52834,#20257,#20258) ;
#16639 = AXIS2_PLACEMENT_3D('',#52836,#20259,#20260) ;
#16640 = AXIS2_PLACEMENT_3D('',#52838,#20261,#20262) ;
#16641 = AXIS2_PLACEMENT_3D('',#52839,#20263,#20264) ;
#16642 = AXIS2_PLACEMENT_3D('',#52840,#20265,#20266) ;
#16643 = AXIS2_PLACEMENT_3D('',#52842,#20268,#20269) ;
#16644 = AXIS2_PLACEMENT_3D('',#52844,#20271,#20272) ;
#16645 = AXIS2_PLACEMENT_3D('',#52845,#20273,#20274) ;
#16646 = AXIS2_PLACEMENT_3D('',#52847,#20275,#20276) ;
#16647 = AXIS2_PLACEMENT_3D('',#52849,#20277,#20278) ;
#16648 = AXIS2_PLACEMENT_3D('',#52850,#20279,#20280) ;
#16649 = AXIS2_PLACEMENT_3D('',#52851,#20281,#20282) ;
#16650 = AXIS2_PLACEMENT_3D('',#52853,#20283,#20284) ;
#16651 = AXIS2_PLACEMENT_3D('',#52855,#20285,#20286) ;
#16652 = AXIS2_PLACEMENT_3D('',#52856,#20287,#20288) ;
#16653 = AXIS2_PLACEMENT_3D('',#52857,#20289,#20290) ;
#16654 = AXIS2_PLACEMENT_3D('',#52859,#20292,#20293) ;
#16655 = AXIS2_PLACEMENT_3D('',#52861,#20295,#20296) ;
#16656 = AXIS2_PLACEMENT_3D('',#52862,#20297,#20298) ;
#16657 = AXIS2_PLACEMENT_3D('',#52864,#20299,#20300) ;
#16658 = AXIS2_PLACEMENT_3D('',#52866,#20301,#20302) ;
#16659 = AXIS2_PLACEMENT_3D('',#52867,#20303,#20304) ;
#16660 = AXIS2_PLACEMENT_3D('',#52868,#20305,#20306) ;
#16661 = AXIS2_PLACEMENT_3D('',#52870,#20307,#20308) ;
#16662 = AXIS2_PLACEMENT_3D('',#52872,#20309,#20310) ;
#16663 = AXIS2_PLACEMENT_3D('',#52873,#20311,#20312) ;
#16664 = AXIS2_PLACEMENT_3D('',#52874,#20313,#20314) ;
#16665 = AXIS2_PLACEMENT_3D('',#52876,#20316,#20317) ;
#16666 = AXIS2_PLACEMENT_3D('',#52878,#20319,#20320) ;
#16667 = AXIS2_PLACEMENT_3D('',#52879,#20321,#20322) ;
#16668 = AXIS2_PLACEMENT_3D('',#52881,#20323,#20324) ;
#16669 = AXIS2_PLACEMENT_3D('',#52883,#20325,#20326) ;
#16670 = AXIS2_PLACEMENT_3D('',#52884,#20327,#20328) ;
#16671 = AXIS2_PLACEMENT_3D('',#52885,#20329,#20330) ;
#16672 = AXIS2_PLACEMENT_3D('',#52887,#20331,#20332) ;
#16673 = AXIS2_PLACEMENT_3D('',#52889,#20333,#20334) ;
#16674 = AXIS2_PLACEMENT_3D('',#52890,#20335,#20336) ;
#16675 = AXIS2_PLACEMENT_3D('',#52891,#20337,#20338) ;
#16676 = AXIS2_PLACEMENT_3D('',#52893,#20340,#20341) ;
#16677 = AXIS2_PLACEMENT_3D('',#52895,#20343,#20344) ;
#16678 = AXIS2_PLACEMENT_3D('',#52896,#20345,#20346) ;
#16679 = AXIS2_PLACEMENT_3D('',#52898,#20347,#20348) ;
#16680 = AXIS2_PLACEMENT_3D('',#52900,#20349,#20350) ;
#16681 = AXIS2_PLACEMENT_3D('',#52901,#20351,#20352) ;
#16682 = AXIS2_PLACEMENT_3D('',#52902,#20353,#20354) ;
#16683 = AXIS2_PLACEMENT_3D('',#52904,#20355,#20356) ;
#16684 = AXIS2_PLACEMENT_3D('',#52906,#20357,#20358) ;
#16685 = AXIS2_PLACEMENT_3D('',#52907,#20359,#20360) ;
#16686 = AXIS2_PLACEMENT_3D('',#52908,#20361,#20362) ;
#16687 = AXIS2_PLACEMENT_3D('',#52910,#20364,#20365) ;
#16688 = AXIS2_PLACEMENT_3D('',#52912,#20367,#20368) ;
#16689 = AXIS2_PLACEMENT_3D('',#52913,#20369,#20370) ;
#16690 = AXIS2_PLACEMENT_3D('',#52915,#20371,#20372) ;
#16691 = AXIS2_PLACEMENT_3D('',#52917,#20373,#20374) ;
#16692 = AXIS2_PLACEMENT_3D('',#52918,#20375,#20376) ;
#16693 = AXIS2_PLACEMENT_3D('',#52919,#20377,#20378) ;
#16694 = AXIS2_PLACEMENT_3D('',#52921,#20379,#20380) ;
#16695 = AXIS2_PLACEMENT_3D('',#52923,#20381,#20382) ;
#16696 = AXIS2_PLACEMENT_3D('',#52924,#20383,#20384) ;
#16697 = AXIS2_PLACEMENT_3D('',#52925,#20385,#20386) ;
#16698 = AXIS2_PLACEMENT_3D('',#52927,#20388,#20389) ;
#16699 = AXIS2_PLACEMENT_3D('',#52929,#20391,#20392) ;
#16700 = AXIS2_PLACEMENT_3D('',#52930,#20393,#20394) ;
#16701 = AXIS2_PLACEMENT_3D('',#52932,#20395,#20396) ;
#16702 = AXIS2_PLACEMENT_3D('',#52934,#20397,#20398) ;
#16703 = AXIS2_PLACEMENT_3D('',#52935,#20399,#20400) ;
#16704 = AXIS2_PLACEMENT_3D('',#52936,#20401,#20402) ;
#16705 = AXIS2_PLACEMENT_3D('',#52938,#20403,#20404) ;
#16706 = AXIS2_PLACEMENT_3D('',#52940,#20405,#20406) ;
#16707 = AXIS2_PLACEMENT_3D('',#52941,#20407,#20408) ;
#16708 = AXIS2_PLACEMENT_3D('',#52942,#20409,#20410) ;
#16709 = AXIS2_PLACEMENT_3D('',#52944,#20412,#20413) ;
#16710 = AXIS2_PLACEMENT_3D('',#52946,#20415,#20416) ;
#16711 = AXIS2_PLACEMENT_3D('',#52947,#20417,#20418) ;
#16712 = AXIS2_PLACEMENT_3D('',#52949,#20419,#20420) ;
#16713 = AXIS2_PLACEMENT_3D('',#52951,#20421,#20422) ;
#16714 = AXIS2_PLACEMENT_3D('',#52952,#20423,#20424) ;
#16715 = AXIS2_PLACEMENT_3D('',#52953,#20425,#20426) ;
#16716 = AXIS2_PLACEMENT_3D('',#52955,#20427,#20428) ;
#16717 = AXIS2_PLACEMENT_3D('',#52957,#20429,#20430) ;
#16718 = AXIS2_PLACEMENT_3D('',#52958,#20431,#20432) ;
#16719 = AXIS2_PLACEMENT_3D('',#52959,#20433,#20434) ;
#16720 = AXIS2_PLACEMENT_3D('',#52961,#20436,#20437) ;
#16721 = AXIS2_PLACEMENT_3D('',#52963,#20439,#20440) ;
#16722 = AXIS2_PLACEMENT_3D('',#52964,#20441,#20442) ;
#16723 = AXIS2_PLACEMENT_3D('',#52966,#20443,#20444) ;
#16724 = AXIS2_PLACEMENT_3D('',#52968,#20445,#20446) ;
#16725 = AXIS2_PLACEMENT_3D('',#52969,#20447,#20448) ;
#16726 = AXIS2_PLACEMENT_3D('',#52970,#20449,#20450) ;
#16727 = AXIS2_PLACEMENT_3D('',#52972,#20451,#20452) ;
#16728 = AXIS2_PLACEMENT_3D('',#52974,#20453,#20454) ;
#16729 = AXIS2_PLACEMENT_3D('',#52975,#20455,#20456) ;
#16730 = AXIS2_PLACEMENT_3D('',#52976,#20457,#20458) ;
#16731 = AXIS2_PLACEMENT_3D('',#52978,#20460,#20461) ;
#16732 = AXIS2_PLACEMENT_3D('',#52980,#20463,#20464) ;
#16733 = AXIS2_PLACEMENT_3D('',#52981,#20465,#20466) ;
#16734 = AXIS2_PLACEMENT_3D('',#52983,#20467,#20468) ;
#16735 = AXIS2_PLACEMENT_3D('',#52985,#20469,#20470) ;
#16736 = AXIS2_PLACEMENT_3D('',#52986,#20471,#20472) ;
#16737 = AXIS2_PLACEMENT_3D('',#52987,#20473,#20474) ;
#16738 = AXIS2_PLACEMENT_3D('',#52989,#20475,#20476) ;
#16739 = AXIS2_PLACEMENT_3D('',#52991,#20477,#20478) ;
#16740 = AXIS2_PLACEMENT_3D('',#52992,#20479,#20480) ;
#16741 = AXIS2_PLACEMENT_3D('',#52993,#20481,#20482) ;
#16742 = AXIS2_PLACEMENT_3D('',#52995,#20484,#20485) ;
#16743 = AXIS2_PLACEMENT_3D('',#52997,#20487,#20488) ;
#16744 = AXIS2_PLACEMENT_3D('',#52998,#20489,#20490) ;
#16745 = AXIS2_PLACEMENT_3D('',#53000,#20491,#20492) ;
#16746 = AXIS2_PLACEMENT_3D('',#53002,#20493,#20494) ;
#16747 = AXIS2_PLACEMENT_3D('',#53003,#20495,#20496) ;
#16748 = AXIS2_PLACEMENT_3D('',#53004,#20497,#20498) ;
#16749 = AXIS2_PLACEMENT_3D('',#53006,#20499,#20500) ;
#16750 = AXIS2_PLACEMENT_3D('',#53008,#20501,#20502) ;
#16751 = AXIS2_PLACEMENT_3D('',#53009,#20503,#20504) ;
#16752 = AXIS2_PLACEMENT_3D('',#53010,#20505,#20506) ;
#16753 = AXIS2_PLACEMENT_3D('',#53012,#20508,#20509) ;
#16754 = AXIS2_PLACEMENT_3D('',#53014,#20511,#20512) ;
#16755 = AXIS2_PLACEMENT_3D('',#53015,#20513,#20514) ;
#16756 = AXIS2_PLACEMENT_3D('',#53017,#20515,#20516) ;
#16757 = AXIS2_PLACEMENT_3D('',#53019,#20517,#20518) ;
#16758 = AXIS2_PLACEMENT_3D('',#53020,#20519,#20520) ;
#16759 = AXIS2_PLACEMENT_3D('',#53021,#20521,#20522) ;
#16760 = AXIS2_PLACEMENT_3D('',#53023,#20523,#20524) ;
#16761 = AXIS2_PLACEMENT_3D('',#53025,#20525,#20526) ;
#16762 = AXIS2_PLACEMENT_3D('',#53026,#20527,#20528) ;
#16763 = AXIS2_PLACEMENT_3D('',#53027,#20529,#20530) ;
#16764 = AXIS2_PLACEMENT_3D('',#53029,#20532,#20533) ;
#16765 = AXIS2_PLACEMENT_3D('',#53031,#20535,#20536) ;
#16766 = AXIS2_PLACEMENT_3D('',#53032,#20537,#20538) ;
#16767 = AXIS2_PLACEMENT_3D('',#53034,#20539,#20540) ;
#16768 = AXIS2_PLACEMENT_3D('',#53036,#20541,#20542) ;
#16769 = AXIS2_PLACEMENT_3D('',#53037,#20543,#20544) ;
#16770 = AXIS2_PLACEMENT_3D('',#53038,#20545,#20546) ;
#16771 = AXIS2_PLACEMENT_3D('',#53040,#20547,#20548) ;
#16772 = AXIS2_PLACEMENT_3D('',#53042,#20549,#20550) ;
#16773 = AXIS2_PLACEMENT_3D('',#53043,#20551,#20552) ;
#16774 = AXIS2_PLACEMENT_3D('',#53044,#20553,#20554) ;
#16775 = AXIS2_PLACEMENT_3D('',#53046,#20556,#20557) ;
#16776 = AXIS2_PLACEMENT_3D('',#53048,#20559,#20560) ;
#16777 = AXIS2_PLACEMENT_3D('',#53049,#20561,#20562) ;
#16778 = AXIS2_PLACEMENT_3D('',#53051,#20563,#20564) ;
#16779 = AXIS2_PLACEMENT_3D('',#53053,#20565,#20566) ;
#16780 = AXIS2_PLACEMENT_3D('',#53054,#20567,#20568) ;
#16781 = AXIS2_PLACEMENT_3D('',#53055,#20569,#20570) ;
#16782 = AXIS2_PLACEMENT_3D('',#53057,#20571,#20572) ;
#16783 = AXIS2_PLACEMENT_3D('',#53059,#20573,#20574) ;
#16784 = AXIS2_PLACEMENT_3D('',#53060,#20575,#20576) ;
#16785 = AXIS2_PLACEMENT_3D('',#53061,#20577,#20578) ;
#16786 = AXIS2_PLACEMENT_3D('',#53063,#20580,#20581) ;
#16787 = AXIS2_PLACEMENT_3D('',#53065,#20583,#20584) ;
#16788 = AXIS2_PLACEMENT_3D('',#53066,#20585,#20586) ;
#16789 = AXIS2_PLACEMENT_3D('',#53068,#20587,#20588) ;
#16790 = AXIS2_PLACEMENT_3D('',#53070,#20589,#20590) ;
#16791 = AXIS2_PLACEMENT_3D('',#53071,#20591,#20592) ;
#16792 = AXIS2_PLACEMENT_3D('',#53072,#20593,#20594) ;
#16793 = AXIS2_PLACEMENT_3D('',#53074,#20595,#20596) ;
#16794 = AXIS2_PLACEMENT_3D('',#53076,#20597,#20598) ;
#16795 = AXIS2_PLACEMENT_3D('',#53077,#20599,#20600) ;
#16796 = AXIS2_PLACEMENT_3D('',#53078,#20601,#20602) ;
#16797 = AXIS2_PLACEMENT_3D('',#53080,#20604,#20605) ;
#16798 = AXIS2_PLACEMENT_3D('',#53082,#20607,#20608) ;
#16799 = AXIS2_PLACEMENT_3D('',#53083,#20609,#20610) ;
#16800 = AXIS2_PLACEMENT_3D('',#53085,#20611,#20612) ;
#16801 = AXIS2_PLACEMENT_3D('',#53087,#20613,#20614) ;
#16802 = AXIS2_PLACEMENT_3D('',#53088,#20615,#20616) ;
#16803 = AXIS2_PLACEMENT_3D('',#53089,#20617,#20618) ;
#16804 = AXIS2_PLACEMENT_3D('',#53091,#20619,#20620) ;
#16805 = AXIS2_PLACEMENT_3D('',#53093,#20621,#20622) ;
#16806 = AXIS2_PLACEMENT_3D('',#53094,#20623,#20624) ;
#16807 = AXIS2_PLACEMENT_3D('',#53095,#20625,#20626) ;
#16808 = AXIS2_PLACEMENT_3D('',#53097,#20628,#20629) ;
#16809 = AXIS2_PLACEMENT_3D('',#53099,#20631,#20632) ;
#16810 = AXIS2_PLACEMENT_3D('',#53100,#20633,#20634) ;
#16811 = AXIS2_PLACEMENT_3D('',#53102,#20635,#20636) ;
#16812 = AXIS2_PLACEMENT_3D('',#53104,#20637,#20638) ;
#16813 = AXIS2_PLACEMENT_3D('',#53105,#20639,#20640) ;
#16814 = AXIS2_PLACEMENT_3D('',#53106,#20641,#20642) ;
#16815 = AXIS2_PLACEMENT_3D('',#53108,#20643,#20644) ;
#16816 = AXIS2_PLACEMENT_3D('',#53110,#20645,#20646) ;
#16817 = AXIS2_PLACEMENT_3D('',#53111,#20647,#20648) ;
#16818 = AXIS2_PLACEMENT_3D('',#53112,#20649,#20650) ;
#16819 = AXIS2_PLACEMENT_3D('',#53114,#20652,#20653) ;
#16820 = AXIS2_PLACEMENT_3D('',#53116,#20655,#20656) ;
#16821 = AXIS2_PLACEMENT_3D('',#53117,#20657,#20658) ;
#16822 = AXIS2_PLACEMENT_3D('',#53119,#20659,#20660) ;
#16823 = AXIS2_PLACEMENT_3D('',#53121,#20661,#20662) ;
#16824 = AXIS2_PLACEMENT_3D('',#53122,#20663,#20664) ;
#16825 = AXIS2_PLACEMENT_3D('',#53123,#20665,#20666) ;
#16826 = AXIS2_PLACEMENT_3D('',#53125,#20667,#20668) ;
#16827 = AXIS2_PLACEMENT_3D('',#53127,#20669,#20670) ;
#16828 = AXIS2_PLACEMENT_3D('',#53128,#20671,#20672) ;
#16829 = AXIS2_PLACEMENT_3D('',#53129,#20673,#20674) ;
#16830 = AXIS2_PLACEMENT_3D('',#53131,#20676,#20677) ;
#16831 = AXIS2_PLACEMENT_3D('',#53133,#20679,#20680) ;
#16832 = AXIS2_PLACEMENT_3D('',#53134,#20681,#20682) ;
#16833 = AXIS2_PLACEMENT_3D('',#53136,#20683,#20684) ;
#16834 = AXIS2_PLACEMENT_3D('',#53138,#20685,#20686) ;
#16835 = AXIS2_PLACEMENT_3D('',#53139,#20687,#20688) ;
#16836 = AXIS2_PLACEMENT_3D('',#53140,#20689,#20690) ;
#16837 = AXIS2_PLACEMENT_3D('',#53142,#20691,#20692) ;
#16838 = AXIS2_PLACEMENT_3D('',#53144,#20693,#20694) ;
#16839 = AXIS2_PLACEMENT_3D('',#53145,#20695,#20696) ;
#16840 = AXIS2_PLACEMENT_3D('',#53146,#20697,#20698) ;
#16841 = AXIS2_PLACEMENT_3D('',#53148,#20700,#20701) ;
#16842 = AXIS2_PLACEMENT_3D('',#53150,#20703,#20704) ;
#16843 = AXIS2_PLACEMENT_3D('',#53151,#20705,#20706) ;
#16844 = AXIS2_PLACEMENT_3D('',#53153,#20707,#20708) ;
#16845 = AXIS2_PLACEMENT_3D('',#53155,#20709,#20710) ;
#16846 = AXIS2_PLACEMENT_3D('',#53156,#20711,#20712) ;
#16847 = AXIS2_PLACEMENT_3D('',#53157,#20713,#20714) ;
#16848 = AXIS2_PLACEMENT_3D('',#53159,#20715,#20716) ;
#16849 = AXIS2_PLACEMENT_3D('',#53161,#20717,#20718) ;
#16850 = AXIS2_PLACEMENT_3D('',#53162,#20719,#20720) ;
#16851 = AXIS2_PLACEMENT_3D('',#53163,#20721,#20722) ;
#16852 = AXIS2_PLACEMENT_3D('',#53165,#20724,#20725) ;
#16853 = AXIS2_PLACEMENT_3D('',#53167,#20727,#20728) ;
#16854 = AXIS2_PLACEMENT_3D('',#53168,#20729,#20730) ;
#16855 = AXIS2_PLACEMENT_3D('',#53170,#20731,#20732) ;
#16856 = AXIS2_PLACEMENT_3D('',#53172,#20733,#20734) ;
#16857 = AXIS2_PLACEMENT_3D('',#53173,#20735,#20736) ;
#16858 = AXIS2_PLACEMENT_3D('',#53174,#20737,#20738) ;
#16859 = AXIS2_PLACEMENT_3D('',#53176,#20739,#20740) ;
#16860 = AXIS2_PLACEMENT_3D('',#53178,#20741,#20742) ;
#16861 = AXIS2_PLACEMENT_3D('',#53179,#20743,#20744) ;
#16862 = AXIS2_PLACEMENT_3D('',#53180,#20745,#20746) ;
#16863 = AXIS2_PLACEMENT_3D('',#53182,#20748,#20749) ;
#16864 = AXIS2_PLACEMENT_3D('',#53184,#20751,#20752) ;
#16865 = AXIS2_PLACEMENT_3D('',#53185,#20753,#20754) ;
#16866 = AXIS2_PLACEMENT_3D('',#53187,#20755,#20756) ;
#16867 = AXIS2_PLACEMENT_3D('',#53189,#20757,#20758) ;
#16868 = AXIS2_PLACEMENT_3D('',#53190,#20759,#20760) ;
#16869 = AXIS2_PLACEMENT_3D('',#53191,#20761,#20762) ;
#16870 = AXIS2_PLACEMENT_3D('',#53193,#20763,#20764) ;
#16871 = AXIS2_PLACEMENT_3D('',#53195,#20765,#20766) ;
#16872 = AXIS2_PLACEMENT_3D('',#53196,#20767,#20768) ;
#16873 = AXIS2_PLACEMENT_3D('',#53197,#20769,#20770) ;
#16874 = AXIS2_PLACEMENT_3D('',#53199,#20772,#20773) ;
#16875 = AXIS2_PLACEMENT_3D('',#53201,#20775,#20776) ;
#16876 = AXIS2_PLACEMENT_3D('',#53202,#20777,#20778) ;
#16877 = AXIS2_PLACEMENT_3D('',#53204,#20779,#20780) ;
#16878 = AXIS2_PLACEMENT_3D('',#53206,#20781,#20782) ;
#16879 = AXIS2_PLACEMENT_3D('',#53207,#20783,#20784) ;
#16880 = AXIS2_PLACEMENT_3D('',#53208,#20785,#20786) ;
#16881 = AXIS2_PLACEMENT_3D('',#53210,#20787,#20788) ;
#16882 = AXIS2_PLACEMENT_3D('',#53212,#20789,#20790) ;
#16883 = AXIS2_PLACEMENT_3D('',#53213,#20791,#20792) ;
#16884 = AXIS2_PLACEMENT_3D('',#53214,#20793,#20794) ;
#16885 = AXIS2_PLACEMENT_3D('',#53216,#20796,#20797) ;
#16886 = AXIS2_PLACEMENT_3D('',#53218,#20799,#20800) ;
#16887 = AXIS2_PLACEMENT_3D('',#53219,#20801,#20802) ;
#16888 = AXIS2_PLACEMENT_3D('',#53221,#20803,#20804) ;
#16889 = AXIS2_PLACEMENT_3D('',#53223,#20805,#20806) ;
#16890 = AXIS2_PLACEMENT_3D('',#53224,#20807,#20808) ;
#16891 = AXIS2_PLACEMENT_3D('',#53225,#20809,#20810) ;
#16892 = AXIS2_PLACEMENT_3D('',#53227,#20811,#20812) ;
#16893 = AXIS2_PLACEMENT_3D('',#53229,#20813,#20814) ;
#16894 = AXIS2_PLACEMENT_3D('',#53230,#20815,#20816) ;
#16895 = AXIS2_PLACEMENT_3D('',#53231,#20817,#20818) ;
#16896 = AXIS2_PLACEMENT_3D('',#53233,#20820,#20821) ;
#16897 = AXIS2_PLACEMENT_3D('',#53235,#20823,#20824) ;
#16898 = AXIS2_PLACEMENT_3D('',#53236,#20825,#20826) ;
#16899 = AXIS2_PLACEMENT_3D('',#53238,#20827,#20828) ;
#16900 = AXIS2_PLACEMENT_3D('',#53240,#20829,#20830) ;
#16901 = AXIS2_PLACEMENT_3D('',#53241,#20831,#20832) ;
#16902 = AXIS2_PLACEMENT_3D('',#53242,#20833,#20834) ;
#16903 = AXIS2_PLACEMENT_3D('',#53244,#20835,#20836) ;
#16904 = AXIS2_PLACEMENT_3D('',#53246,#20837,#20838) ;
#16905 = AXIS2_PLACEMENT_3D('',#53247,#20839,#20840) ;
#16906 = AXIS2_PLACEMENT_3D('',#53248,#20841,#20842) ;
#16907 = AXIS2_PLACEMENT_3D('',#53250,#20844,#20845) ;
#16908 = AXIS2_PLACEMENT_3D('',#53252,#20847,#20848) ;
#16909 = AXIS2_PLACEMENT_3D('',#53253,#20849,#20850) ;
#16910 = AXIS2_PLACEMENT_3D('',#53255,#20851,#20852) ;
#16911 = AXIS2_PLACEMENT_3D('',#53257,#20853,#20854) ;
#16912 = AXIS2_PLACEMENT_3D('',#53258,#20855,#20856) ;
#16913 = AXIS2_PLACEMENT_3D('',#53259,#20857,#20858) ;
#16914 = AXIS2_PLACEMENT_3D('',#53261,#20859,#20860) ;
#16915 = AXIS2_PLACEMENT_3D('',#53263,#20861,#20862) ;
#16916 = AXIS2_PLACEMENT_3D('',#53264,#20863,#20864) ;
#16917 = AXIS2_PLACEMENT_3D('',#53265,#20865,#20866) ;
#16918 = AXIS2_PLACEMENT_3D('',#53267,#20868,#20869) ;
#16919 = AXIS2_PLACEMENT_3D('',#53269,#20871,#20872) ;
#16920 = AXIS2_PLACEMENT_3D('',#53270,#20873,#20874) ;
#16921 = AXIS2_PLACEMENT_3D('',#53272,#20875,#20876) ;
#16922 = AXIS2_PLACEMENT_3D('',#53274,#20877,#20878) ;
#16923 = AXIS2_PLACEMENT_3D('',#53275,#20879,#20880) ;
#16924 = AXIS2_PLACEMENT_3D('',#53276,#20881,#20882) ;
#16925 = AXIS2_PLACEMENT_3D('',#53278,#20883,#20884) ;
#16926 = AXIS2_PLACEMENT_3D('',#53280,#20885,#20886) ;
#16927 = AXIS2_PLACEMENT_3D('',#53281,#20887,#20888) ;
#16928 = AXIS2_PLACEMENT_3D('',#53282,#20889,#20890) ;
#16929 = AXIS2_PLACEMENT_3D('',#53284,#20892,#20893) ;
#16930 = AXIS2_PLACEMENT_3D('',#53286,#20895,#20896) ;
#16931 = AXIS2_PLACEMENT_3D('',#53287,#20897,#20898) ;
#16932 = AXIS2_PLACEMENT_3D('',#53289,#20899,#20900) ;
#16933 = AXIS2_PLACEMENT_3D('',#53291,#20901,#20902) ;
#16934 = AXIS2_PLACEMENT_3D('',#53292,#20903,#20904) ;
#16935 = AXIS2_PLACEMENT_3D('',#53293,#20905,#20906) ;
#16936 = AXIS2_PLACEMENT_3D('',#53295,#20907,#20908) ;
#16937 = AXIS2_PLACEMENT_3D('',#53297,#20909,#20910) ;
#16938 = AXIS2_PLACEMENT_3D('',#53298,#20911,#20912) ;
#16939 = AXIS2_PLACEMENT_3D('',#53299,#20913,#20914) ;
#16940 = AXIS2_PLACEMENT_3D('',#53301,#20916,#20917) ;
#16941 = AXIS2_PLACEMENT_3D('',#53303,#20919,#20920) ;
#16942 = AXIS2_PLACEMENT_3D('',#53304,#20921,#20922) ;
#16943 = AXIS2_PLACEMENT_3D('',#53306,#20923,#20924) ;
#16944 = AXIS2_PLACEMENT_3D('',#53308,#20925,#20926) ;
#16945 = AXIS2_PLACEMENT_3D('',#53309,#20927,#20928) ;
#16946 = AXIS2_PLACEMENT_3D('',#53310,#20929,#20930) ;
#16947 = AXIS2_PLACEMENT_3D('',#53312,#20931,#20932) ;
#16948 = AXIS2_PLACEMENT_3D('',#53314,#20933,#20934) ;
#16949 = AXIS2_PLACEMENT_3D('',#53315,#20935,#20936) ;
#16950 = AXIS2_PLACEMENT_3D('',#53316,#20937,#20938) ;
#16951 = AXIS2_PLACEMENT_3D('',#53318,#20940,#20941) ;
#16952 = AXIS2_PLACEMENT_3D('',#53320,#20943,#20944) ;
#16953 = AXIS2_PLACEMENT_3D('',#53321,#20945,#20946) ;
#16954 = AXIS2_PLACEMENT_3D('',#53323,#20947,#20948) ;
#16955 = AXIS2_PLACEMENT_3D('',#53325,#20949,#20950) ;
#16956 = AXIS2_PLACEMENT_3D('',#53326,#20951,#20952) ;
#16957 = AXIS2_PLACEMENT_3D('',#53327,#20953,#20954) ;
#16958 = AXIS2_PLACEMENT_3D('',#53329,#20955,#20956) ;
#16959 = AXIS2_PLACEMENT_3D('',#53331,#20957,#20958) ;
#16960 = AXIS2_PLACEMENT_3D('',#53332,#20959,#20960) ;
#16961 = AXIS2_PLACEMENT_3D('',#53333,#20961,#20962) ;
#16962 = AXIS2_PLACEMENT_3D('',#53335,#20964,#20965) ;
#16963 = AXIS2_PLACEMENT_3D('',#53337,#20967,#20968) ;
#16964 = AXIS2_PLACEMENT_3D('',#53338,#20969,#20970) ;
#16965 = AXIS2_PLACEMENT_3D('',#53340,#20971,#20972) ;
#16966 = AXIS2_PLACEMENT_3D('',#53342,#20973,#20974) ;
#16967 = AXIS2_PLACEMENT_3D('',#53343,#20975,#20976) ;
#16968 = AXIS2_PLACEMENT_3D('',#53344,#20977,#20978) ;
#16969 = AXIS2_PLACEMENT_3D('',#53346,#20979,#20980) ;
#16970 = AXIS2_PLACEMENT_3D('',#53348,#20981,#20982) ;
#16971 = AXIS2_PLACEMENT_3D('',#53349,#20983,#20984) ;
#16972 = AXIS2_PLACEMENT_3D('',#53350,#20985,#20986) ;
#16973 = AXIS2_PLACEMENT_3D('',#53352,#20988,#20989) ;
#16974 = AXIS2_PLACEMENT_3D('',#53354,#20991,#20992) ;
#16975 = AXIS2_PLACEMENT_3D('',#53355,#20993,#20994) ;
#16976 = AXIS2_PLACEMENT_3D('',#53357,#20995,#20996) ;
#16977 = AXIS2_PLACEMENT_3D('',#53359,#20997,#20998) ;
#16978 = AXIS2_PLACEMENT_3D('',#53360,#20999,#21000) ;
#16979 = AXIS2_PLACEMENT_3D('',#53361,#21001,#21002) ;
#16980 = AXIS2_PLACEMENT_3D('',#53363,#21003,#21004) ;
#16981 = AXIS2_PLACEMENT_3D('',#53365,#21005,#21006) ;
#16982 = AXIS2_PLACEMENT_3D('',#53366,#21007,#21008) ;
#16983 = AXIS2_PLACEMENT_3D('',#53367,#21009,#21010) ;
#16984 = AXIS2_PLACEMENT_3D('',#53369,#21012,#21013) ;
#16985 = AXIS2_PLACEMENT_3D('',#53371,#21015,#21016) ;
#16986 = AXIS2_PLACEMENT_3D('',#53372,#21017,#21018) ;
#16987 = AXIS2_PLACEMENT_3D('',#53374,#21019,#21020) ;
#16988 = AXIS2_PLACEMENT_3D('',#53376,#21021,#21022) ;
#16989 = AXIS2_PLACEMENT_3D('',#53377,#21023,#21024) ;
#16990 = AXIS2_PLACEMENT_3D('',#53378,#21025,#21026) ;
#16991 = AXIS2_PLACEMENT_3D('',#53380,#21027,#21028) ;
#16992 = AXIS2_PLACEMENT_3D('',#53382,#21029,#21030) ;
#16993 = AXIS2_PLACEMENT_3D('',#53383,#21031,#21032) ;
#16994 = AXIS2_PLACEMENT_3D('',#53384,#21033,#21034) ;
#16995 = AXIS2_PLACEMENT_3D('',#53386,#21036,#21037) ;
#16996 = AXIS2_PLACEMENT_3D('',#53388,#21039,#21040) ;
#16997 = AXIS2_PLACEMENT_3D('',#53389,#21041,#21042) ;
#16998 = AXIS2_PLACEMENT_3D('',#53391,#21043,#21044) ;
#16999 = AXIS2_PLACEMENT_3D('',#53393,#21045,#21046) ;
#17000 = AXIS2_PLACEMENT_3D('',#53394,#21047,#21048) ;
#17001 = AXIS2_PLACEMENT_3D('',#53395,#21049,#21050) ;
#17002 = AXIS2_PLACEMENT_3D('',#53397,#21051,#21052) ;
#17003 = AXIS2_PLACEMENT_3D('',#53399,#21053,#21054) ;
#17004 = AXIS2_PLACEMENT_3D('',#53400,#21055,#21056) ;
#17005 = AXIS2_PLACEMENT_3D('',#53401,#21057,#21058) ;
#17006 = AXIS2_PLACEMENT_3D('',#53403,#21060,#21061) ;
#17007 = AXIS2_PLACEMENT_3D('',#53405,#21063,#21064) ;
#17008 = AXIS2_PLACEMENT_3D('',#53406,#21065,#21066) ;
#17009 = AXIS2_PLACEMENT_3D('',#53408,#21067,#21068) ;
#17010 = AXIS2_PLACEMENT_3D('',#53410,#21069,#21070) ;
#17011 = AXIS2_PLACEMENT_3D('',#53411,#21071,#21072) ;
#17012 = AXIS2_PLACEMENT_3D('',#53412,#21073,#21074) ;
#17013 = AXIS2_PLACEMENT_3D('',#53414,#21075,#21076) ;
#17014 = AXIS2_PLACEMENT_3D('',#53416,#21077,#21078) ;
#17015 = AXIS2_PLACEMENT_3D('',#53417,#21079,#21080) ;
#17016 = AXIS2_PLACEMENT_3D('',#53418,#21081,#21082) ;
#17017 = AXIS2_PLACEMENT_3D('',#53420,#21084,#21085) ;
#17018 = AXIS2_PLACEMENT_3D('',#53422,#21087,#21088) ;
#17019 = AXIS2_PLACEMENT_3D('',#53423,#21089,#21090) ;
#17020 = AXIS2_PLACEMENT_3D('',#53425,#21091,#21092) ;
#17021 = AXIS2_PLACEMENT_3D('',#53427,#21093,#21094) ;
#17022 = AXIS2_PLACEMENT_3D('',#53428,#21095,#21096) ;
#17023 = AXIS2_PLACEMENT_3D('',#53429,#21097,#21098) ;
#17024 = AXIS2_PLACEMENT_3D('',#53431,#21099,#21100) ;
#17025 = AXIS2_PLACEMENT_3D('',#53433,#21101,#21102) ;
#17026 = AXIS2_PLACEMENT_3D('',#53434,#21103,#21104) ;
#17027 = AXIS2_PLACEMENT_3D('',#53435,#21105,#21106) ;
#17028 = AXIS2_PLACEMENT_3D('',#53437,#21108,#21109) ;
#17029 = AXIS2_PLACEMENT_3D('',#53439,#21111,#21112) ;
#17030 = AXIS2_PLACEMENT_3D('',#53440,#21113,#21114) ;
#17031 = AXIS2_PLACEMENT_3D('',#53442,#21115,#21116) ;
#17032 = AXIS2_PLACEMENT_3D('',#53444,#21117,#21118) ;
#17033 = AXIS2_PLACEMENT_3D('',#53445,#21119,#21120) ;
#17034 = AXIS2_PLACEMENT_3D('',#53446,#21121,#21122) ;
#17035 = AXIS2_PLACEMENT_3D('',#53448,#21123,#21124) ;
#17036 = AXIS2_PLACEMENT_3D('',#53450,#21125,#21126) ;
#17037 = AXIS2_PLACEMENT_3D('',#53451,#21127,#21128) ;
#17038 = AXIS2_PLACEMENT_3D('',#53452,#21129,#21130) ;
#17039 = AXIS2_PLACEMENT_3D('',#53454,#21132,#21133) ;
#17040 = AXIS2_PLACEMENT_3D('',#53456,#21135,#21136) ;
#17041 = AXIS2_PLACEMENT_3D('',#53457,#21137,#21138) ;
#17042 = AXIS2_PLACEMENT_3D('',#53459,#21139,#21140) ;
#17043 = AXIS2_PLACEMENT_3D('',#53461,#21141,#21142) ;
#17044 = AXIS2_PLACEMENT_3D('',#53462,#21143,#21144) ;
#17045 = AXIS2_PLACEMENT_3D('',#53463,#21145,#21146) ;
#17046 = AXIS2_PLACEMENT_3D('',#53465,#21147,#21148) ;
#17047 = AXIS2_PLACEMENT_3D('',#53467,#21149,#21150) ;
#17048 = AXIS2_PLACEMENT_3D('',#53468,#21151,#21152) ;
#17049 = AXIS2_PLACEMENT_3D('',#53469,#21153,#21154) ;
#17050 = AXIS2_PLACEMENT_3D('',#53471,#21156,#21157) ;
#17051 = AXIS2_PLACEMENT_3D('',#53473,#21159,#21160) ;
#17052 = AXIS2_PLACEMENT_3D('',#53474,#21161,#21162) ;
#17053 = AXIS2_PLACEMENT_3D('',#53476,#21163,#21164) ;
#17054 = AXIS2_PLACEMENT_3D('',#53478,#21165,#21166) ;
#17055 = AXIS2_PLACEMENT_3D('',#53479,#21167,#21168) ;
#17056 = AXIS2_PLACEMENT_3D('',#53480,#21169,#21170) ;
#17057 = AXIS2_PLACEMENT_3D('',#53482,#21171,#21172) ;
#17058 = AXIS2_PLACEMENT_3D('',#53484,#21173,#21174) ;
#17059 = AXIS2_PLACEMENT_3D('',#53485,#21175,#21176) ;
#17060 = AXIS2_PLACEMENT_3D('',#53486,#21177,#21178) ;
#17061 = AXIS2_PLACEMENT_3D('',#53488,#21180,#21181) ;
#17062 = AXIS2_PLACEMENT_3D('',#53490,#21183,#21184) ;
#17063 = AXIS2_PLACEMENT_3D('',#53491,#21185,#21186) ;
#17064 = AXIS2_PLACEMENT_3D('',#53493,#21187,#21188) ;
#17065 = AXIS2_PLACEMENT_3D('',#53495,#21189,#21190) ;
#17066 = AXIS2_PLACEMENT_3D('',#53496,#21191,#21192) ;
#17067 = AXIS2_PLACEMENT_3D('',#53497,#21193,#21194) ;
#17068 = AXIS2_PLACEMENT_3D('',#53499,#21195,#21196) ;
#17069 = AXIS2_PLACEMENT_3D('',#53501,#21197,#21198) ;
#17070 = AXIS2_PLACEMENT_3D('',#53502,#21199,#21200) ;
#17071 = AXIS2_PLACEMENT_3D('',#53503,#21201,#21202) ;
#17072 = AXIS2_PLACEMENT_3D('',#53505,#21204,#21205) ;
#17073 = AXIS2_PLACEMENT_3D('',#53507,#21207,#21208) ;
#17074 = AXIS2_PLACEMENT_3D('',#53508,#21209,#21210) ;
#17075 = AXIS2_PLACEMENT_3D('',#53510,#21211,#21212) ;
#17076 = AXIS2_PLACEMENT_3D('',#53512,#21213,#21214) ;
#17077 = AXIS2_PLACEMENT_3D('',#53513,#21215,#21216) ;
#17078 = AXIS2_PLACEMENT_3D('',#53514,#21217,#21218) ;
#17079 = AXIS2_PLACEMENT_3D('',#53516,#21219,#21220) ;
#17080 = AXIS2_PLACEMENT_3D('',#53518,#21221,#21222) ;
#17081 = AXIS2_PLACEMENT_3D('',#53519,#21223,#21224) ;
#17082 = AXIS2_PLACEMENT_3D('',#53520,#21225,#21226) ;
#17083 = AXIS2_PLACEMENT_3D('',#53522,#21228,#21229) ;
#17084 = AXIS2_PLACEMENT_3D('',#53524,#21231,#21232) ;
#17085 = AXIS2_PLACEMENT_3D('',#53525,#21233,#21234) ;
#17086 = AXIS2_PLACEMENT_3D('',#53527,#21235,#21236) ;
#17087 = AXIS2_PLACEMENT_3D('',#53529,#21237,#21238) ;
#17088 = AXIS2_PLACEMENT_3D('',#53530,#21239,#21240) ;
#17089 = AXIS2_PLACEMENT_3D('',#53531,#21241,#21242) ;
#17090 = AXIS2_PLACEMENT_3D('',#53533,#21243,#21244) ;
#17091 = AXIS2_PLACEMENT_3D('',#53535,#21245,#21246) ;
#17092 = AXIS2_PLACEMENT_3D('',#53536,#21247,#21248) ;
#17093 = AXIS2_PLACEMENT_3D('',#53537,#21249,#21250) ;
#17094 = AXIS2_PLACEMENT_3D('',#53539,#21252,#21253) ;
#17095 = AXIS2_PLACEMENT_3D('',#53541,#21255,#21256) ;
#17096 = AXIS2_PLACEMENT_3D('',#53542,#21257,#21258) ;
#17097 = AXIS2_PLACEMENT_3D('',#53544,#21259,#21260) ;
#17098 = AXIS2_PLACEMENT_3D('',#53546,#21261,#21262) ;
#17099 = AXIS2_PLACEMENT_3D('',#53547,#21263,#21264) ;
#17100 = AXIS2_PLACEMENT_3D('',#53548,#21265,#21266) ;
#17101 = AXIS2_PLACEMENT_3D('',#53550,#21267,#21268) ;
#17102 = AXIS2_PLACEMENT_3D('',#53552,#21269,#21270) ;
#17103 = AXIS2_PLACEMENT_3D('',#53553,#21271,#21272) ;
#17104 = AXIS2_PLACEMENT_3D('',#53554,#21273,#21274) ;
#17105 = AXIS2_PLACEMENT_3D('',#53556,#21276,#21277) ;
#17106 = AXIS2_PLACEMENT_3D('',#53558,#21279,#21280) ;
#17107 = AXIS2_PLACEMENT_3D('',#53559,#21281,#21282) ;
#17108 = AXIS2_PLACEMENT_3D('',#53561,#21283,#21284) ;
#17109 = AXIS2_PLACEMENT_3D('',#53563,#21285,#21286) ;
#17110 = AXIS2_PLACEMENT_3D('',#53564,#21287,#21288) ;
#17111 = AXIS2_PLACEMENT_3D('',#53565,#21289,#21290) ;
#17112 = AXIS2_PLACEMENT_3D('',#53567,#21291,#21292) ;
#17113 = AXIS2_PLACEMENT_3D('',#53569,#21293,#21294) ;
#17114 = AXIS2_PLACEMENT_3D('',#53570,#21295,#21296) ;
#17115 = AXIS2_PLACEMENT_3D('',#53571,#21297,#21298) ;
#17116 = AXIS2_PLACEMENT_3D('',#53573,#21300,#21301) ;
#17117 = AXIS2_PLACEMENT_3D('',#53575,#21303,#21304) ;
#17118 = AXIS2_PLACEMENT_3D('',#53576,#21305,#21306) ;
#17119 = AXIS2_PLACEMENT_3D('',#53578,#21307,#21308) ;
#17120 = AXIS2_PLACEMENT_3D('',#53580,#21309,#21310) ;
#17121 = AXIS2_PLACEMENT_3D('',#53581,#21311,#21312) ;
#17122 = AXIS2_PLACEMENT_3D('',#53582,#21313,#21314) ;
#17123 = AXIS2_PLACEMENT_3D('',#53584,#21315,#21316) ;
#17124 = AXIS2_PLACEMENT_3D('',#53586,#21317,#21318) ;
#17125 = AXIS2_PLACEMENT_3D('',#53587,#21319,#21320) ;
#17126 = AXIS2_PLACEMENT_3D('',#53588,#21321,#21322) ;
#17127 = AXIS2_PLACEMENT_3D('',#53590,#21324,#21325) ;
#17128 = AXIS2_PLACEMENT_3D('',#53592,#21327,#21328) ;
#17129 = AXIS2_PLACEMENT_3D('',#53593,#21329,#21330) ;
#17130 = AXIS2_PLACEMENT_3D('',#53595,#21331,#21332) ;
#17131 = AXIS2_PLACEMENT_3D('',#53597,#21333,#21334) ;
#17132 = AXIS2_PLACEMENT_3D('',#53598,#21335,#21336) ;
#17133 = AXIS2_PLACEMENT_3D('',#53599,#21337,#21338) ;
#17134 = AXIS2_PLACEMENT_3D('',#53601,#21339,#21340) ;
#17135 = AXIS2_PLACEMENT_3D('',#53603,#21341,#21342) ;
#17136 = AXIS2_PLACEMENT_3D('',#53604,#21343,#21344) ;
#17137 = AXIS2_PLACEMENT_3D('',#53605,#21345,#21346) ;
#17138 = AXIS2_PLACEMENT_3D('',#53607,#21348,#21349) ;
#17139 = AXIS2_PLACEMENT_3D('',#53609,#21351,#21352) ;
#17140 = AXIS2_PLACEMENT_3D('',#53610,#21353,#21354) ;
#17141 = AXIS2_PLACEMENT_3D('',#53612,#21355,#21356) ;
#17142 = AXIS2_PLACEMENT_3D('',#53614,#21357,#21358) ;
#17143 = AXIS2_PLACEMENT_3D('',#53615,#21359,#21360) ;
#17144 = AXIS2_PLACEMENT_3D('',#53616,#21361,#21362) ;
#17145 = AXIS2_PLACEMENT_3D('',#53618,#21363,#21364) ;
#17146 = AXIS2_PLACEMENT_3D('',#53620,#21365,#21366) ;
#17147 = AXIS2_PLACEMENT_3D('',#53621,#21367,#21368) ;
#17148 = AXIS2_PLACEMENT_3D('',#53622,#21369,#21370) ;
#17149 = AXIS2_PLACEMENT_3D('',#53624,#21372,#21373) ;
#17150 = AXIS2_PLACEMENT_3D('',#53626,#21375,#21376) ;
#17151 = AXIS2_PLACEMENT_3D('',#53627,#21377,#21378) ;
#17152 = AXIS2_PLACEMENT_3D('',#53629,#21379,#21380) ;
#17153 = AXIS2_PLACEMENT_3D('',#53631,#21381,#21382) ;
#17154 = AXIS2_PLACEMENT_3D('',#53632,#21383,#21384) ;
#17155 = AXIS2_PLACEMENT_3D('',#53633,#21385,#21386) ;
#17156 = AXIS2_PLACEMENT_3D('',#53635,#21387,#21388) ;
#17157 = AXIS2_PLACEMENT_3D('',#53637,#21389,#21390) ;
#17158 = AXIS2_PLACEMENT_3D('',#53638,#21391,#21392) ;
#17159 = AXIS2_PLACEMENT_3D('',#53639,#21393,#21394) ;
#17160 = AXIS2_PLACEMENT_3D('',#53641,#21396,#21397) ;
#17161 = AXIS2_PLACEMENT_3D('',#53643,#21399,#21400) ;
#17162 = AXIS2_PLACEMENT_3D('',#53644,#21401,#21402) ;
#17163 = AXIS2_PLACEMENT_3D('',#53646,#21403,#21404) ;
#17164 = AXIS2_PLACEMENT_3D('',#53648,#21405,#21406) ;
#17165 = AXIS2_PLACEMENT_3D('',#53649,#21407,#21408) ;
#17166 = AXIS2_PLACEMENT_3D('',#53650,#21409,#21410) ;
#17167 = AXIS2_PLACEMENT_3D('',#53652,#21411,#21412) ;
#17168 = AXIS2_PLACEMENT_3D('',#53654,#21413,#21414) ;
#17169 = AXIS2_PLACEMENT_3D('',#53655,#21415,#21416) ;
#17170 = AXIS2_PLACEMENT_3D('',#53656,#21417,#21418) ;
#17171 = AXIS2_PLACEMENT_3D('',#53658,#21420,#21421) ;
#17172 = AXIS2_PLACEMENT_3D('',#53660,#21423,#21424) ;
#17173 = AXIS2_PLACEMENT_3D('',#53661,#21425,#21426) ;
#17174 = AXIS2_PLACEMENT_3D('',#53663,#21427,#21428) ;
#17175 = AXIS2_PLACEMENT_3D('',#53665,#21429,#21430) ;
#17176 = AXIS2_PLACEMENT_3D('',#53666,#21431,#21432) ;
#17177 = AXIS2_PLACEMENT_3D('',#53667,#21433,#21434) ;
#17178 = AXIS2_PLACEMENT_3D('',#53669,#21435,#21436) ;
#17179 = AXIS2_PLACEMENT_3D('',#53671,#21437,#21438) ;
#17180 = AXIS2_PLACEMENT_3D('',#53672,#21439,#21440) ;
#17181 = AXIS2_PLACEMENT_3D('',#53673,#21441,#21442) ;
#17182 = AXIS2_PLACEMENT_3D('',#53675,#21444,#21445) ;
#17183 = AXIS2_PLACEMENT_3D('',#53677,#21447,#21448) ;
#17184 = AXIS2_PLACEMENT_3D('',#53678,#21449,#21450) ;
#17185 = AXIS2_PLACEMENT_3D('',#53680,#21451,#21452) ;
#17186 = AXIS2_PLACEMENT_3D('',#53682,#21453,#21454) ;
#17187 = AXIS2_PLACEMENT_3D('',#53683,#21455,#21456) ;
#17188 = AXIS2_PLACEMENT_3D('',#53684,#21457,#21458) ;
#17189 = AXIS2_PLACEMENT_3D('',#53686,#21459,#21460) ;
#17190 = AXIS2_PLACEMENT_3D('',#53688,#21461,#21462) ;
#17191 = AXIS2_PLACEMENT_3D('',#53689,#21463,#21464) ;
#17192 = AXIS2_PLACEMENT_3D('',#53690,#21465,#21466) ;
#17193 = AXIS2_PLACEMENT_3D('',#53692,#21468,#21469) ;
#17194 = AXIS2_PLACEMENT_3D('',#53694,#21471,#21472) ;
#17195 = AXIS2_PLACEMENT_3D('',#53695,#21473,#21474) ;
#17196 = AXIS2_PLACEMENT_3D('',#53697,#21475,#21476) ;
#17197 = AXIS2_PLACEMENT_3D('',#53699,#21477,#21478) ;
#17198 = AXIS2_PLACEMENT_3D('',#53700,#21479,#21480) ;
#17199 = AXIS2_PLACEMENT_3D('',#53701,#21481,#21482) ;
#17200 = AXIS2_PLACEMENT_3D('',#53703,#21483,#21484) ;
#17201 = AXIS2_PLACEMENT_3D('',#53705,#21485,#21486) ;
#17202 = AXIS2_PLACEMENT_3D('',#53706,#21487,#21488) ;
#17203 = AXIS2_PLACEMENT_3D('',#53707,#21489,#21490) ;
#17204 = AXIS2_PLACEMENT_3D('',#53709,#21492,#21493) ;
#17205 = AXIS2_PLACEMENT_3D('',#53711,#21495,#21496) ;
#17206 = AXIS2_PLACEMENT_3D('',#53712,#21497,#21498) ;
#17207 = AXIS2_PLACEMENT_3D('',#53713,#21499,#21500) ;
#17208 = AXIS2_PLACEMENT_3D('',#53714,#21501,#21502) ;
#17209 = AXIS2_PLACEMENT_3D('',#53717,#21503,#21504) ;
#17210 = AXIS2_PLACEMENT_3D('',#53718,#21505,#21506) ;
#17211 = AXIS2_PLACEMENT_3D('',#53721,#21508,#21509) ;
#17212 = AXIS2_PLACEMENT_3D('',#53722,#21510,#21511) ;
#17213 = AXIS2_PLACEMENT_3D('',#53725,#21513,#21514) ;
#17214 = AXIS2_PLACEMENT_3D('',#53726,#21515,#21516) ;
#17215 = AXIS2_PLACEMENT_3D('',#53728,#21517,#21518) ;
#17216 = AXIS2_PLACEMENT_3D('',#53729,#21519,#21520) ;
#17217 = AXIS2_PLACEMENT_3D('',#53732,#21521,#21522) ;
#17218 = AXIS2_PLACEMENT_3D('',#53734,#21524,#21525) ;
#17219 = AXIS2_PLACEMENT_3D('',#53735,#21526,#21527) ;
#17220 = AXIS2_PLACEMENT_3D('',#53738,#21529,#21530) ;
#17221 = AXIS2_PLACEMENT_3D('',#53739,#21531,#21532) ;
#17222 = AXIS2_PLACEMENT_3D('',#53742,#21534,#21535) ;
#17223 = AXIS2_PLACEMENT_3D('',#53743,#21536,#21537) ;
#17224 = AXIS2_PLACEMENT_3D('',#53745,#21538,#21539) ;
#17225 = AXIS2_PLACEMENT_3D('',#53746,#21540,#21541) ;
#17226 = AXIS2_PLACEMENT_3D('',#53748,#21543,#21544) ;
#17227 = AXIS2_PLACEMENT_3D('',#53749,#21545,#21546) ;
#17228 = AXIS2_PLACEMENT_3D('',#53760,#21550,#21551) ;
#17229 = AXIS2_PLACEMENT_3D('',#53771,#21555,#21556) ;
#17230 = AXIS2_PLACEMENT_3D('',#53772,#21557,#21558) ;
#17231 = AXIS2_PLACEMENT_3D('',#53773,#21559,#21560) ;
#17232 = AXIS2_PLACEMENT_3D('',#53774,#21561,#21562) ;
#17233 = AXIS2_PLACEMENT_3D('',#53776,#21563,#21564) ;
#17234 = AXIS2_PLACEMENT_3D('',#53780,#21566,#21567) ;
#17235 = AXIS2_PLACEMENT_3D('',#53784,#21569,#21570) ;
#17236 = AXIS2_PLACEMENT_3D('',#53788,#21572,#21573) ;
#17237 = AXIS2_PLACEMENT_3D('',#53792,#21575,#21576) ;
#17238 = AXIS2_PLACEMENT_3D('',#53796,#21578,#21579) ;
#17239 = AXIS2_PLACEMENT_3D('',#53799,#21581,#21582) ;
#17240 = AXIS2_PLACEMENT_3D('',#53801,#21583,#21584) ;
#17241 = AXIS2_PLACEMENT_3D('',#53802,#21585,#21586) ;
#17242 = AXIS2_PLACEMENT_3D('',#53804,#21587,#21588) ;
#17243 = AXIS2_PLACEMENT_3D('',#53806,#21590,#21591) ;
#17244 = AXIS2_PLACEMENT_3D('',#53808,#21592,#21593) ;
#17245 = AXIS2_PLACEMENT_3D('',#53812,#21594,#21595) ;
#17246 = AXIS2_PLACEMENT_3D('',#53820,#21598,#21599) ;
#17247 = AXIS2_PLACEMENT_3D('',#53822,#21601,#21602) ;
#17248 = AXIS2_PLACEMENT_3D('',#53823,#21603,#21604) ;
#17249 = AXIS2_PLACEMENT_3D('',#53824,#21605,#21606) ;
#17250 = AXIS2_PLACEMENT_3D('',#53826,#21607,#21608) ;
#17251 = AXIS2_PLACEMENT_3D('',#53828,#21610,#21611) ;
#17252 = AXIS2_PLACEMENT_3D('',#53830,#21612,#21613) ;
#17253 = AXIS2_PLACEMENT_3D('',#53834,#21614,#21615) ;
#17254 = AXIS2_PLACEMENT_3D('',#53842,#21618,#21619) ;
#17255 = AXIS2_PLACEMENT_3D('',#53844,#21621,#21622) ;
#17256 = AXIS2_PLACEMENT_3D('',#53845,#21623,#21624) ;
#17257 = AXIS2_PLACEMENT_3D('',#53846,#21625,#21626) ;
#17258 = AXIS2_PLACEMENT_3D('',#53848,#21627,#21628) ;
#17259 = AXIS2_PLACEMENT_3D('',#53850,#21630,#21631) ;
#17260 = AXIS2_PLACEMENT_3D('',#53852,#21632,#21633) ;
#17261 = AXIS2_PLACEMENT_3D('',#53856,#21634,#21635) ;
#17262 = AXIS2_PLACEMENT_3D('',#53864,#21638,#21639) ;
#17263 = AXIS2_PLACEMENT_3D('',#53866,#21641,#21642) ;
#17264 = AXIS2_PLACEMENT_3D('',#53867,#21643,#21644) ;
#17265 = AXIS2_PLACEMENT_3D('',#53868,#21645,#21646) ;
#17266 = AXIS2_PLACEMENT_3D('',#53869,#21647,#21648) ;
#17267 = AXIS2_PLACEMENT_3D('',#53870,#21649,#21650) ;
#17268 = AXIS2_PLACEMENT_3D('',#53871,#21651,#21652) ;
#17269 = AXIS2_PLACEMENT_3D('',#53872,#21653,#21654) ;
#17270 = AXIS2_PLACEMENT_3D('',#53874,#21655,#21656) ;
#17271 = AXIS2_PLACEMENT_3D('',#53875,#21657,#21658) ;
#17272 = AXIS2_PLACEMENT_3D('',#53877,#21660,#21661) ;
#17273 = AXIS2_PLACEMENT_3D('',#53878,#21662,#21663) ;
#17274 = AXIS2_PLACEMENT_3D('',#53880,#21664,#21665) ;
#17275 = AXIS2_PLACEMENT_3D('',#53884,#21667,#21668) ;
#17276 = AXIS2_PLACEMENT_3D('',#53931,#21669,#21670) ;
#17277 = AXIS2_PLACEMENT_3D('',#53978,#21671,#21672) ;
#17278 = AXIS2_PLACEMENT_3D('',#54025,#21673,#21674) ;
#17279 = AXIS2_PLACEMENT_3D('',#54072,#21675,#21676) ;
#17280 = AXIS2_PLACEMENT_3D('',#54119,#21677,#21678) ;
#17281 = AXIS2_PLACEMENT_3D('',#54166,#21679,#21680) ;
#17282 = AXIS2_PLACEMENT_3D('',#54213,#21681,#21682) ;
#17283 = AXIS2_PLACEMENT_3D('',#54260,#21683,#21684) ;
#17284 = AXIS2_PLACEMENT_3D('',#54307,#21685,#21686) ;
#17285 = AXIS2_PLACEMENT_3D('',#54354,#21687,#21688) ;
#17286 = AXIS2_PLACEMENT_3D('',#54401,#21689,#21690) ;
#17287 = AXIS2_PLACEMENT_3D('',#54448,#21691,#21692) ;
#17288 = AXIS2_PLACEMENT_3D('',#54495,#21693,#21694) ;
#17289 = AXIS2_PLACEMENT_3D('',#54542,#21695,#21696) ;
#17290 = AXIS2_PLACEMENT_3D('',#54589,#21697,#21698) ;
#17291 = AXIS2_PLACEMENT_3D('',#54636,#21699,#21700) ;
#17292 = AXIS2_PLACEMENT_3D('',#54683,#21701,#21702) ;
#17293 = AXIS2_PLACEMENT_3D('',#54730,#21703,#21704) ;
#17294 = AXIS2_PLACEMENT_3D('',#54777,#21705,#21706) ;
#17295 = AXIS2_PLACEMENT_3D('',#54824,#21707,#21708) ;
#17296 = AXIS2_PLACEMENT_3D('',#54871,#21709,#21710) ;
#17297 = AXIS2_PLACEMENT_3D('',#54918,#21711,#21712) ;
#17298 = AXIS2_PLACEMENT_3D('',#54965,#21713,#21714) ;
#17299 = AXIS2_PLACEMENT_3D('',#55012,#21715,#21716) ;
#17300 = AXIS2_PLACEMENT_3D('',#55059,#21717,#21718) ;
#17301 = AXIS2_PLACEMENT_3D('',#55106,#21719,#21720) ;
#17302 = AXIS2_PLACEMENT_3D('',#55153,#21721,#21722) ;
#17303 = AXIS2_PLACEMENT_3D('',#55200,#21723,#21724) ;
#17304 = AXIS2_PLACEMENT_3D('',#55247,#21725,#21726) ;
#17305 = AXIS2_PLACEMENT_3D('',#55294,#21727,#21728) ;
#17306 = AXIS2_PLACEMENT_3D('',#55341,#21729,#21730) ;
#17307 = AXIS2_PLACEMENT_3D('',#55388,#21731,#21732) ;
#17308 = AXIS2_PLACEMENT_3D('',#55435,#21733,#21734) ;
#17309 = AXIS2_PLACEMENT_3D('',#55482,#21735,#21736) ;
#17310 = AXIS2_PLACEMENT_3D('',#55529,#21737,#21738) ;
#17311 = AXIS2_PLACEMENT_3D('',#55576,#21739,#21740) ;
#17312 = AXIS2_PLACEMENT_3D('',#55623,#21741,#21742) ;
#17313 = AXIS2_PLACEMENT_3D('',#55670,#21743,#21744) ;
#17314 = AXIS2_PLACEMENT_3D('',#55717,#21745,#21746) ;
#17315 = AXIS2_PLACEMENT_3D('',#55764,#21747,#21748) ;
#17316 = AXIS2_PLACEMENT_3D('',#55811,#21749,#21750) ;
#17317 = AXIS2_PLACEMENT_3D('',#55858,#21751,#21752) ;
#17318 = AXIS2_PLACEMENT_3D('',#55905,#21753,#21754) ;
#17319 = AXIS2_PLACEMENT_3D('',#55952,#21755,#21756) ;
#17320 = AXIS2_PLACEMENT_3D('',#55999,#21757,#21758) ;
#17321 = AXIS2_PLACEMENT_3D('',#56046,#21759,#21760) ;
#17322 = AXIS2_PLACEMENT_3D('',#56093,#21761,#21762) ;
#17323 = AXIS2_PLACEMENT_3D('',#56140,#21763,#21764) ;
#17324 = AXIS2_PLACEMENT_3D('',#56187,#21765,#21766) ;
#17325 = AXIS2_PLACEMENT_3D('',#56234,#21767,#21768) ;
#17326 = AXIS2_PLACEMENT_3D('',#56281,#21769,#21770) ;
#17327 = AXIS2_PLACEMENT_3D('',#56328,#21771,#21772) ;
#17328 = AXIS2_PLACEMENT_3D('',#56375,#21773,#21774) ;
#17329 = AXIS2_PLACEMENT_3D('',#56422,#21775,#21776) ;
#17330 = AXIS2_PLACEMENT_3D('',#56469,#21777,#21778) ;
#17331 = AXIS2_PLACEMENT_3D('',#56516,#21779,#21780) ;
#17332 = AXIS2_PLACEMENT_3D('',#56563,#21781,#21782) ;
#17333 = AXIS2_PLACEMENT_3D('',#56609,#21783,#21784) ;
#17334 = AXIS2_PLACEMENT_3D('',#56610,#21785,#21786) ;
#17335 = AXIS2_PLACEMENT_3D('',#56614,#21788,#21789) ;
#17336 = AXIS2_PLACEMENT_3D('',#56639,#21790,#21791) ;
#17337 = AXIS2_PLACEMENT_3D('',#56651,#21792,#21793) ;
#17338 = AXIS2_PLACEMENT_3D('',#56676,#21794,#21795) ;
#17339 = AXIS2_PLACEMENT_3D('',#56690,#21796,#21797) ;
#17340 = AXIS2_PLACEMENT_3D('',#56715,#21798,#21799) ;
#17341 = AXIS2_PLACEMENT_3D('',#56727,#21800,#21801) ;
#17342 = AXIS2_PLACEMENT_3D('',#56752,#21802,#21803) ;
#17343 = AXIS2_PLACEMENT_3D('',#56766,#21804,#21805) ;
#17344 = AXIS2_PLACEMENT_3D('',#56791,#21806,#21807) ;
#17345 = AXIS2_PLACEMENT_3D('',#56803,#21808,#21809) ;
#17346 = AXIS2_PLACEMENT_3D('',#56828,#21810,#21811) ;
#17347 = AXIS2_PLACEMENT_3D('',#56858,#21812,#21813) ;
#17348 = AXIS2_PLACEMENT_3D('',#56883,#21814,#21815) ;
#17349 = AXIS2_PLACEMENT_3D('',#56895,#21816,#21817) ;
#17350 = AXIS2_PLACEMENT_3D('',#56920,#21818,#21819) ;
#17351 = AXIS2_PLACEMENT_3D('',#56934,#21820,#21821) ;
#17352 = AXIS2_PLACEMENT_3D('',#56936,#21822,#21823) ;
#17353 = AXIS2_PLACEMENT_3D('',#56961,#21824,#21825) ;
#17354 = AXIS2_PLACEMENT_3D('',#56973,#21826,#21827) ;
#17355 = AXIS2_PLACEMENT_3D('',#56998,#21828,#21829) ;
#17356 = AXIS2_PLACEMENT_3D('',#57016,#21830,#21831) ;
#17357 = AXIS2_PLACEMENT_3D('',#57041,#21832,#21833) ;
#17358 = AXIS2_PLACEMENT_3D('',#57055,#21834,#21835) ;
#17359 = AXIS2_PLACEMENT_3D('',#57080,#21836,#21837) ;
#17360 = AXIS2_PLACEMENT_3D('',#57092,#21838,#21839) ;
#17361 = AXIS2_PLACEMENT_3D('',#57094,#21840,#21841) ;
#17362 = AXIS2_PLACEMENT_3D('',#57119,#21842,#21843) ;
#17363 = AXIS2_PLACEMENT_3D('',#57133,#21844,#21845) ;
#17364 = AXIS2_PLACEMENT_3D('',#57162,#21846,#21847) ;
#17365 = AXIS2_PLACEMENT_3D('',#57184,#21848,#21849) ;
#17366 = AXIS2_PLACEMENT_3D('',#57209,#21850,#21851) ;
#17367 = AXIS2_PLACEMENT_3D('',#57221,#21852,#21853) ;
#17368 = AXIS2_PLACEMENT_3D('',#57246,#21854,#21855) ;
#17369 = AXIS2_PLACEMENT_3D('',#57260,#21856,#21857) ;
#17370 = AXIS2_PLACEMENT_3D('',#57285,#21858,#21859) ;
#17371 = AXIS2_PLACEMENT_3D('',#57299,#21860,#21861) ;
#17372 = AXIS2_PLACEMENT_3D('',#57324,#21862,#21863) ;
#17373 = AXIS2_PLACEMENT_3D('',#57344,#21864,#21865) ;
#17374 = AXIS2_PLACEMENT_3D('',#57375,#21866,#21867) ;
#17375 = AXIS2_PLACEMENT_3D('',#57395,#21868,#21869) ;
#17376 = AXIS2_PLACEMENT_3D('',#57420,#21870,#21871) ;
#17377 = AXIS2_PLACEMENT_3D('',#57434,#21872,#21873) ;
#17378 = AXIS2_PLACEMENT_3D('',#57459,#21874,#21875) ;
#17379 = AXIS2_PLACEMENT_3D('',#57471,#21876,#21877) ;
#17380 = AXIS2_PLACEMENT_3D('',#57496,#21878,#21879) ;
#17381 = AXIS2_PLACEMENT_3D('',#57510,#21880,#21881) ;
#17382 = AXIS2_PLACEMENT_3D('',#57535,#21882,#21883) ;
#17383 = AXIS2_PLACEMENT_3D('',#57547,#21884,#21885) ;
#17384 = AXIS2_PLACEMENT_3D('',#57572,#21886,#21887) ;
#17385 = AXIS2_PLACEMENT_3D('',#57586,#21888,#21889) ;
#17386 = AXIS2_PLACEMENT_3D('',#57611,#21890,#21891) ;
#17387 = AXIS2_PLACEMENT_3D('',#57623,#21892,#21893) ;
#17388 = AXIS2_PLACEMENT_3D('',#57648,#21894,#21895) ;
#17389 = AXIS2_PLACEMENT_3D('',#57662,#21896,#21897) ;
#17390 = AXIS2_PLACEMENT_3D('',#57687,#21898,#21899) ;
#17391 = AXIS2_PLACEMENT_3D('',#57700,#21900,#21901) ;
#17392 = AXIS2_PLACEMENT_3D('',#57729,#21902,#21903) ;
#17393 = AXIS2_PLACEMENT_3D('',#57780,#21904,#21905) ;
#17394 = AXIS2_PLACEMENT_3D('',#57801,#21906,#21907) ;
#17395 = AXIS2_PLACEMENT_3D('',#57804,#21909,#21910) ;
#17396 = AXIS2_PLACEMENT_3D('',#57806,#21911,#21912) ;
#17397 = AXIS2_PLACEMENT_3D('',#57810,#21915,#21916) ;
#17398 = AXIS2_PLACEMENT_3D('',#57812,#21917,#21918) ;
#17399 = AXIS2_PLACEMENT_3D('',#57816,#21921,#21922) ;
#17400 = AXIS2_PLACEMENT_3D('',#57818,#21923,#21924) ;
#17401 = AXIS2_PLACEMENT_3D('',#57822,#21927,#21928) ;
#17402 = AXIS2_PLACEMENT_3D('',#57824,#21929,#21930) ;
#17403 = AXIS2_PLACEMENT_3D('',#57828,#21933,#21934) ;
#17404 = AXIS2_PLACEMENT_3D('',#57830,#21935,#21936) ;
#17405 = AXIS2_PLACEMENT_3D('',#57834,#21939,#21940) ;
#17406 = AXIS2_PLACEMENT_3D('',#57836,#21941,#21942) ;
#17407 = AXIS2_PLACEMENT_3D('',#57840,#21945,#21946) ;
#17408 = AXIS2_PLACEMENT_3D('',#57842,#21947,#21948) ;
#17409 = AXIS2_PLACEMENT_3D('',#57846,#21951,#21952) ;
#17410 = AXIS2_PLACEMENT_3D('',#57848,#21953,#21954) ;
#17411 = AXIS2_PLACEMENT_3D('',#57852,#21957,#21958) ;
#17412 = AXIS2_PLACEMENT_3D('',#57854,#21959,#21960) ;
#17413 = AXIS2_PLACEMENT_3D('',#57858,#21963,#21964) ;
#17414 = AXIS2_PLACEMENT_3D('',#57860,#21965,#21966) ;
#17415 = AXIS2_PLACEMENT_3D('',#57864,#21969,#21970) ;
#17416 = AXIS2_PLACEMENT_3D('',#57866,#21971,#21972) ;
#17417 = AXIS2_PLACEMENT_3D('',#57870,#21975,#21976) ;
#17418 = AXIS2_PLACEMENT_3D('',#57872,#21977,#21978) ;
#17419 = AXIS2_PLACEMENT_3D('',#57876,#21981,#21982) ;
#17420 = AXIS2_PLACEMENT_3D('',#57878,#21983,#21984) ;
#17421 = AXIS2_PLACEMENT_3D('',#57882,#21987,#21988) ;
#17422 = AXIS2_PLACEMENT_3D('',#57884,#21989,#21990) ;
#17423 = AXIS2_PLACEMENT_3D('',#57888,#21993,#21994) ;
#17424 = AXIS2_PLACEMENT_3D('',#57890,#21995,#21996) ;
#17425 = AXIS2_PLACEMENT_3D('',#57894,#21999,#22000) ;
#17426 = AXIS2_PLACEMENT_3D('',#57896,#22001,#22002) ;
#17427 = AXIS2_PLACEMENT_3D('',#57900,#22005,#22006) ;
#17428 = AXIS2_PLACEMENT_3D('',#57902,#22007,#22008) ;
#17429 = AXIS2_PLACEMENT_3D('',#57906,#22011,#22012) ;
#17430 = AXIS2_PLACEMENT_3D('',#57908,#22013,#22014) ;
#17431 = AXIS2_PLACEMENT_3D('',#57912,#22017,#22018) ;
#17432 = AXIS2_PLACEMENT_3D('',#57914,#22019,#22020) ;
#17433 = AXIS2_PLACEMENT_3D('',#57918,#22023,#22024) ;
#17434 = AXIS2_PLACEMENT_3D('',#57920,#22025,#22026) ;
#17435 = AXIS2_PLACEMENT_3D('',#57924,#22029,#22030) ;
#17436 = AXIS2_PLACEMENT_3D('',#57926,#22031,#22032) ;
#17437 = AXIS2_PLACEMENT_3D('',#57930,#22035,#22036) ;
#17438 = AXIS2_PLACEMENT_3D('',#57932,#22037,#22038) ;
#17439 = AXIS2_PLACEMENT_3D('',#57936,#22041,#22042) ;
#17440 = AXIS2_PLACEMENT_3D('',#57938,#22043,#22044) ;
#17441 = AXIS2_PLACEMENT_3D('',#57942,#22047,#22048) ;
#17442 = AXIS2_PLACEMENT_3D('',#57944,#22049,#22050) ;
#17443 = AXIS2_PLACEMENT_3D('',#57948,#22053,#22054) ;
#17444 = AXIS2_PLACEMENT_3D('',#57950,#22055,#22056) ;
#17445 = AXIS2_PLACEMENT_3D('',#57954,#22059,#22060) ;
#17446 = AXIS2_PLACEMENT_3D('',#57956,#22061,#22062) ;
#17447 = AXIS2_PLACEMENT_3D('',#57960,#22065,#22066) ;
#17448 = AXIS2_PLACEMENT_3D('',#57962,#22067,#22068) ;
#17449 = AXIS2_PLACEMENT_3D('',#57966,#22071,#22072) ;
#17450 = AXIS2_PLACEMENT_3D('',#57968,#22073,#22074) ;
#17451 = AXIS2_PLACEMENT_3D('',#57972,#22077,#22078) ;
#17452 = AXIS2_PLACEMENT_3D('',#57974,#22079,#22080) ;
#17453 = AXIS2_PLACEMENT_3D('',#57978,#22083,#22084) ;
#17454 = AXIS2_PLACEMENT_3D('',#57979,#22085,#22086) ;
#17455 = AXIS2_PLACEMENT_3D('',#57981,#22087,#22088) ;
#17456 = AXIS2_PLACEMENT_3D('',#57984,#22090,#22091) ;
#17457 = AXIS2_PLACEMENT_3D('',#58078,#22092,#22093) ;
#17458 = AXIS2_PLACEMENT_3D('',#58171,#22094,#22095) ;
#17459 = AXIS2_PLACEMENT_3D('',#58353,#22096,#22097) ;
#17460 = AXIS2_PLACEMENT_3D('',#58535,#22098,#22099) ;
#17461 = AXIS2_PLACEMENT_3D('',#58718,#22100,#22101) ;
#17462 = AXIS2_PLACEMENT_3D('',#58902,#22102,#22103) ;
#17463 = AXIS2_PLACEMENT_3D('',#59084,#22104,#22105) ;
#17464 = AXIS2_PLACEMENT_3D('',#59266,#22106,#22107) ;
#17465 = AXIS2_PLACEMENT_3D('',#59450,#22108,#22109) ;
#17466 = AXIS2_PLACEMENT_3D('',#59633,#22110,#22111) ;
#17467 = AXIS2_PLACEMENT_3D('',#59815,#22112,#22113) ;
#17468 = AXIS2_PLACEMENT_3D('',#59998,#22114,#22115) ;
#17469 = AXIS2_PLACEMENT_3D('',#60182,#22116,#22117) ;
#17470 = AXIS2_PLACEMENT_3D('',#60364,#22118,#22119) ;
#17471 = AXIS2_PLACEMENT_3D('',#60546,#22120,#22121) ;
#17472 = AXIS2_PLACEMENT_3D('',#60730,#22122,#22123) ;
#17473 = AXIS2_PLACEMENT_3D('',#60912,#22124,#22125) ;
#17474 = AXIS2_PLACEMENT_3D('',#61094,#22126,#22127) ;
#17475 = AXIS2_PLACEMENT_3D('',#61277,#22128,#22129) ;
#17476 = AXIS2_PLACEMENT_3D('',#61461,#22130,#22131) ;
#17477 = AXIS2_PLACEMENT_3D('',#61643,#22132,#22133) ;
#17478 = AXIS2_PLACEMENT_3D('',#61825,#22134,#22135) ;
#17479 = AXIS2_PLACEMENT_3D('',#62009,#22136,#22137) ;
#17480 = AXIS2_PLACEMENT_3D('',#62192,#22138,#22139) ;
#17481 = AXIS2_PLACEMENT_3D('',#62374,#22140,#22141) ;
#17482 = AXIS2_PLACEMENT_3D('',#62557,#22142,#22143) ;
#17483 = AXIS2_PLACEMENT_3D('',#62741,#22144,#22145) ;
#17484 = AXIS2_PLACEMENT_3D('',#62923,#22146,#22147) ;
#17485 = AXIS2_PLACEMENT_3D('',#63105,#22148,#22149) ;
#17486 = AXIS2_PLACEMENT_3D('',#63287,#22150,#22151) ;
#17487 = AXIS2_PLACEMENT_3D('',#63289,#22152,#22153) ;
#17488 = AXIS2_PLACEMENT_3D('',#63292,#22155,#22156) ;
#17489 = AXIS2_PLACEMENT_3D('',#63293,#22157,#22158) ;
#17490 = AXIS2_PLACEMENT_3D('',#63295,#22159,#22160) ;
#17491 = AXIS2_PLACEMENT_3D('',#63297,#22161,#22162) ;
#17492 = AXIS2_PLACEMENT_3D('',#63298,#22163,#22164) ;
#17493 = AXIS2_PLACEMENT_3D('',#63299,#22165,#22166) ;
#17494 = AXIS2_PLACEMENT_3D('',#63301,#22167,#22168) ;
#17495 = AXIS2_PLACEMENT_3D('',#63303,#22169,#22170) ;
#17496 = AXIS2_PLACEMENT_3D('',#63304,#22171,#22172) ;
#17497 = AXIS2_PLACEMENT_3D('',#63305,#22173,#22174) ;
#17498 = AXIS2_PLACEMENT_3D('',#63307,#22175,#22176) ;
#17499 = AXIS2_PLACEMENT_3D('',#63309,#22177,#22178) ;
#17500 = AXIS2_PLACEMENT_3D('',#63310,#22179,#22180) ;
#17501 = AXIS2_PLACEMENT_3D('',#63311,#22181,#22182) ;
#17502 = AXIS2_PLACEMENT_3D('',#63314,#22184,#22185) ;
#17503 = AXIS2_PLACEMENT_3D('',#63315,#22186,#22187) ;
#17504 = AXIS2_PLACEMENT_3D('',#63317,#22188,#22189) ;
#17505 = AXIS2_PLACEMENT_3D('',#63318,#22190,#22191) ;
#17506 = AXIS2_PLACEMENT_3D('',#63319,#22192,#22193) ;
#17507 = AXIS2_PLACEMENT_3D('',#63321,#22195,#22196) ;
#17508 = AXIS2_PLACEMENT_3D('',#63322,#22197,#22198) ;
#17509 = AXIS2_PLACEMENT_3D('',#63323,#22199,#22200) ;
#17510 = AXIS2_PLACEMENT_3D('',#63324,#22201,#22202) ;
#17511 = AXIS2_PLACEMENT_3D('',#63325,#22203,#22204) ;
#17512 = AXIS2_PLACEMENT_3D('',#63326,#22205,#22206) ;
#17513 = AXIS2_PLACEMENT_3D('',#63327,#22207,#22208) ;
#17514 = AXIS2_PLACEMENT_3D('',#63328,#22209,#22210) ;
#17515 = AXIS2_PLACEMENT_3D('',#63329,#22211,#22212) ;
#17516 = AXIS2_PLACEMENT_3D('',#63330,#22213,#22214) ;
#17517 = AXIS2_PLACEMENT_3D('',#63331,#22215,#22216) ;
#17518 = AXIS2_PLACEMENT_3D('',#63332,#22217,#22218) ;
#17519 = AXIS2_PLACEMENT_3D('',#63333,#22219,#22220) ;
#17520 = AXIS2_PLACEMENT_3D('',#63334,#22221,#22222) ;
#17521 = AXIS2_PLACEMENT_3D('',#63335,#22223,#22224) ;
#17522 = AXIS2_PLACEMENT_3D('',#63336,#22225,#22226) ;
#17523 = AXIS2_PLACEMENT_3D('',#63337,#22227,#22228) ;
#17524 = AXIS2_PLACEMENT_3D('',#63338,#22229,#22230) ;
#17525 = AXIS2_PLACEMENT_3D('',#63339,#22231,#22232) ;
#17526 = AXIS2_PLACEMENT_3D('',#63340,#22233,#22234) ;
#17527 = AXIS2_PLACEMENT_3D('',#63341,#22235,#22236) ;
#17528 = AXIS2_PLACEMENT_3D('',#63342,#22237,#22238) ;
#17529 = AXIS2_PLACEMENT_3D('',#63343,#22239,#22240) ;
#17530 = AXIS2_PLACEMENT_3D('',#63344,#22241,#22242) ;
#17531 = AXIS2_PLACEMENT_3D('',#63345,#22243,#22244) ;
#17532 = AXIS2_PLACEMENT_3D('',#63346,#22245,#22246) ;
#17533 = AXIS2_PLACEMENT_3D('',#63347,#22247,#22248) ;
#17534 = AXIS2_PLACEMENT_3D('',#63348,#22249,#22250) ;
#17535 = AXIS2_PLACEMENT_3D('',#63349,#22251,#22252) ;
#17536 = AXIS2_PLACEMENT_3D('',#63350,#22253,#22254) ;
#17537 = AXIS2_PLACEMENT_3D('',#63351,#22255,#22256) ;
#17538 = AXIS2_PLACEMENT_3D('',#63352,#22257,#22258) ;
#17539 = AXIS2_PLACEMENT_3D('',#63353,#22259,#22260) ;
#17540 = AXIS2_PLACEMENT_3D('',#63354,#22261,#22262) ;
#17541 = AXIS2_PLACEMENT_3D('',#63355,#22263,#22264) ;
#17542 = AXIS2_PLACEMENT_3D('',#63356,#22265,#22266) ;
#17543 = AXIS2_PLACEMENT_3D('',#63357,#22267,#22268) ;
#17544 = AXIS2_PLACEMENT_3D('',#63358,#22269,#22270) ;
#17545 = AXIS2_PLACEMENT_3D('',#63359,#22271,#22272) ;
#17546 = AXIS2_PLACEMENT_3D('',#63360,#22273,#22274) ;
#17547 = AXIS2_PLACEMENT_3D('',#63361,#22275,#22276) ;
#17548 = AXIS2_PLACEMENT_3D('',#63362,#22277,#22278) ;
#17549 = AXIS2_PLACEMENT_3D('',#63363,#22279,#22280) ;
#17550 = AXIS2_PLACEMENT_3D('',#63364,#22281,#22282) ;
#17551 = AXIS2_PLACEMENT_3D('',#63365,#22283,#22284) ;
#17552 = AXIS2_PLACEMENT_3D('',#63366,#22285,#22286) ;
#17553 = AXIS2_PLACEMENT_3D('',#63367,#22287,#22288) ;
#17554 = AXIS2_PLACEMENT_3D('',#63368,#22289,#22290) ;
#17555 = AXIS2_PLACEMENT_3D('',#63369,#22291,#22292) ;
#17556 = AXIS2_PLACEMENT_3D('',#63370,#22293,#22294) ;
#17557 = AXIS2_PLACEMENT_3D('',#63371,#22295,#22296) ;
#17558 = AXIS2_PLACEMENT_3D('',#63372,#22297,#22298) ;
#17559 = AXIS2_PLACEMENT_3D('',#63373,#22299,#22300) ;
#17560 = AXIS2_PLACEMENT_3D('',#63374,#22301,#22302) ;
#17561 = AXIS2_PLACEMENT_3D('',#63375,#22303,#22304) ;
#17562 = AXIS2_PLACEMENT_3D('',#63376,#22305,#22306) ;
#17563 = AXIS2_PLACEMENT_3D('',#63377,#22307,#22308) ;
#17564 = AXIS2_PLACEMENT_3D('',#63378,#22309,#22310) ;
#17565 = AXIS2_PLACEMENT_3D('',#63379,#22311,#22312) ;
#17566 = AXIS2_PLACEMENT_3D('',#63380,#22313,#22314) ;
#17567 = AXIS2_PLACEMENT_3D('',#63381,#22315,#22316) ;
#17568 = AXIS2_PLACEMENT_3D('',#63382,#22317,#22318) ;
#17569 = AXIS2_PLACEMENT_3D('',#63383,#22319,#22320) ;
#17570 = AXIS2_PLACEMENT_3D('',#63384,#22321,#22322) ;
#17571 = AXIS2_PLACEMENT_3D('',#63385,#22323,#22324) ;
#17572 = AXIS2_PLACEMENT_3D('',#63386,#22325,#22326) ;
#17573 = AXIS2_PLACEMENT_3D('',#63387,#22327,#22328) ;
#17574 = AXIS2_PLACEMENT_3D('',#63388,#22329,#22330) ;
#17575 = AXIS2_PLACEMENT_3D('',#63389,#22331,#22332) ;
#17576 = AXIS2_PLACEMENT_3D('',#63390,#22333,#22334) ;
#17577 = AXIS2_PLACEMENT_3D('',#63391,#22335,#22336) ;
#17578 = AXIS2_PLACEMENT_3D('',#63392,#22337,#22338) ;
#17579 = AXIS2_PLACEMENT_3D('',#63393,#22339,#22340) ;
#17580 = AXIS2_PLACEMENT_3D('',#63394,#22341,#22342) ;
#17581 = AXIS2_PLACEMENT_3D('',#63395,#22343,#22344) ;
#17582 = AXIS2_PLACEMENT_3D('',#63396,#22345,#22346) ;
#17583 = AXIS2_PLACEMENT_3D('',#63397,#22347,#22348) ;
#17584 = AXIS2_PLACEMENT_3D('',#63398,#22349,#22350) ;
#17585 = AXIS2_PLACEMENT_3D('',#63399,#22351,#22352) ;
#17586 = AXIS2_PLACEMENT_3D('',#63400,#22353,#22354) ;
#17587 = AXIS2_PLACEMENT_3D('',#63401,#22355,#22356) ;
#17588 = AXIS2_PLACEMENT_3D('',#63402,#22357,#22358) ;
#17589 = AXIS2_PLACEMENT_3D('',#63403,#22359,#22360) ;
#17590 = AXIS2_PLACEMENT_3D('',#63404,#22361,#22362) ;
#17591 = AXIS2_PLACEMENT_3D('',#63405,#22363,#22364) ;
#17592 = AXIS2_PLACEMENT_3D('',#63406,#22365,#22366) ;
#17593 = AXIS2_PLACEMENT_3D('',#63407,#22367,#22368) ;
#17594 = AXIS2_PLACEMENT_3D('',#63408,#22369,#22370) ;
#17595 = AXIS2_PLACEMENT_3D('',#63409,#22371,#22372) ;
#17596 = AXIS2_PLACEMENT_3D('',#63410,#22373,#22374) ;
#17597 = AXIS2_PLACEMENT_3D('',#63411,#22375,#22376) ;
#17598 = AXIS2_PLACEMENT_3D('',#63412,#22377,#22378) ;
#17599 = AXIS2_PLACEMENT_3D('',#63414,#22380,#22381) ;
#17600 = AXIS2_PLACEMENT_3D('',#63415,#22382,#22383) ;
#17601 = AXIS2_PLACEMENT_3D('',#63416,#22384,#22385) ;
#17602 = AXIS2_PLACEMENT_3D('',#63417,#22386,#22387) ;
#17603 = AXIS2_PLACEMENT_3D('',#63418,#22388,#22389) ;
#17604 = AXIS2_PLACEMENT_3D('',#63419,#22390,#22391) ;
#17605 = AXIS2_PLACEMENT_3D('',#63420,#22392,#22393) ;
#17606 = AXIS2_PLACEMENT_3D('',#63421,#22394,#22395) ;
#17607 = AXIS2_PLACEMENT_3D('',#63422,#22396,#22397) ;
#17608 = AXIS2_PLACEMENT_3D('',#63423,#22398,#22399) ;
#17609 = AXIS2_PLACEMENT_3D('',#63424,#22400,#22401) ;
#17610 = AXIS2_PLACEMENT_3D('',#63425,#22402,#22403) ;
#17611 = AXIS2_PLACEMENT_3D('',#63426,#22404,#22405) ;
#17612 = AXIS2_PLACEMENT_3D('',#63427,#22406,#22407) ;
#17613 = AXIS2_PLACEMENT_3D('',#63428,#22408,#22409) ;
#17614 = AXIS2_PLACEMENT_3D('',#63429,#22410,#22411) ;
#17615 = AXIS2_PLACEMENT_3D('',#63430,#22412,#22413) ;
#17616 = AXIS2_PLACEMENT_3D('',#63431,#22414,#22415) ;
#17617 = AXIS2_PLACEMENT_3D('',#63432,#22416,#22417) ;
#17618 = AXIS2_PLACEMENT_3D('',#63433,#22418,#22419) ;
#17619 = AXIS2_PLACEMENT_3D('',#63434,#22420,#22421) ;
#17620 = AXIS2_PLACEMENT_3D('',#63435,#22422,#22423) ;
#17621 = AXIS2_PLACEMENT_3D('',#63436,#22424,#22425) ;
#17622 = AXIS2_PLACEMENT_3D('',#63437,#22426,#22427) ;
#17623 = AXIS2_PLACEMENT_3D('',#63438,#22428,#22429) ;
#17624 = AXIS2_PLACEMENT_3D('',#63439,#22430,#22431) ;
#17625 = AXIS2_PLACEMENT_3D('',#63440,#22432,#22433) ;
#17626 = AXIS2_PLACEMENT_3D('',#63441,#22434,#22435) ;
#17627 = AXIS2_PLACEMENT_3D('',#63442,#22436,#22437) ;
#17628 = AXIS2_PLACEMENT_3D('',#63443,#22438,#22439) ;
#17629 = AXIS2_PLACEMENT_3D('',#63444,#22440,#22441) ;
#17630 = AXIS2_PLACEMENT_3D('',#63445,#22442,#22443) ;
#17631 = AXIS2_PLACEMENT_3D('',#63446,#22444,#22445) ;
#17632 = AXIS2_PLACEMENT_3D('',#63447,#22446,#22447) ;
#17633 = AXIS2_PLACEMENT_3D('',#63448,#22448,#22449) ;
#17634 = AXIS2_PLACEMENT_3D('',#63449,#22450,#22451) ;
#17635 = AXIS2_PLACEMENT_3D('',#63450,#22452,#22453) ;
#17636 = AXIS2_PLACEMENT_3D('',#63451,#22454,#22455) ;
#17637 = AXIS2_PLACEMENT_3D('',#63452,#22456,#22457) ;
#17638 = AXIS2_PLACEMENT_3D('',#63453,#22458,#22459) ;
#17639 = AXIS2_PLACEMENT_3D('',#63454,#22460,#22461) ;
#17640 = AXIS2_PLACEMENT_3D('',#63455,#22462,#22463) ;
#17641 = AXIS2_PLACEMENT_3D('',#63456,#22464,#22465) ;
#17642 = AXIS2_PLACEMENT_3D('',#63457,#22466,#22467) ;
#17643 = AXIS2_PLACEMENT_3D('',#63458,#22468,#22469) ;
#17644 = AXIS2_PLACEMENT_3D('',#63459,#22470,#22471) ;
#17645 = AXIS2_PLACEMENT_3D('',#63460,#22472,#22473) ;
#17646 = AXIS2_PLACEMENT_3D('',#63461,#22474,#22475) ;
#17647 = AXIS2_PLACEMENT_3D('',#63462,#22476,#22477) ;
#17648 = AXIS2_PLACEMENT_3D('',#63463,#22478,#22479) ;
#17649 = AXIS2_PLACEMENT_3D('',#63464,#22480,#22481) ;
#17650 = AXIS2_PLACEMENT_3D('',#63465,#22482,#22483) ;
#17651 = AXIS2_PLACEMENT_3D('',#63466,#22484,#22485) ;
#17652 = AXIS2_PLACEMENT_3D('',#63467,#22486,#22487) ;
#17653 = AXIS2_PLACEMENT_3D('',#63468,#22488,#22489) ;
#17654 = AXIS2_PLACEMENT_3D('',#63469,#22490,#22491) ;
#17655 = AXIS2_PLACEMENT_3D('',#63470,#22492,#22493) ;
#17656 = AXIS2_PLACEMENT_3D('',#63471,#22494,#22495) ;
#17657 = AXIS2_PLACEMENT_3D('',#63472,#22496,#22497) ;
#17658 = AXIS2_PLACEMENT_3D('',#63473,#22498,#22499) ;
#17659 = AXIS2_PLACEMENT_3D('',#63474,#22500,#22501) ;
#17660 = AXIS2_PLACEMENT_3D('',#63475,#22502,#22503) ;
#17661 = AXIS2_PLACEMENT_3D('',#63476,#22504,#22505) ;
#17662 = AXIS2_PLACEMENT_3D('',#63477,#22506,#22507) ;
#17663 = AXIS2_PLACEMENT_3D('',#63478,#22508,#22509) ;
#17664 = AXIS2_PLACEMENT_3D('',#63479,#22510,#22511) ;
#17665 = AXIS2_PLACEMENT_3D('',#63480,#22512,#22513) ;
#17666 = AXIS2_PLACEMENT_3D('',#63481,#22514,#22515) ;
#17667 = AXIS2_PLACEMENT_3D('',#63482,#22516,#22517) ;
#17668 = AXIS2_PLACEMENT_3D('',#63483,#22518,#22519) ;
#17669 = AXIS2_PLACEMENT_3D('',#63484,#22520,#22521) ;
#17670 = AXIS2_PLACEMENT_3D('',#63485,#22522,#22523) ;
#17671 = AXIS2_PLACEMENT_3D('',#63486,#22524,#22525) ;
#17672 = AXIS2_PLACEMENT_3D('',#63487,#22526,#22527) ;
#17673 = AXIS2_PLACEMENT_3D('',#63488,#22528,#22529) ;
#17674 = AXIS2_PLACEMENT_3D('',#63489,#22530,#22531) ;
#17675 = AXIS2_PLACEMENT_3D('',#63490,#22532,#22533) ;
#17676 = AXIS2_PLACEMENT_3D('',#63491,#22534,#22535) ;
#17677 = AXIS2_PLACEMENT_3D('',#63492,#22536,#22537) ;
#17678 = AXIS2_PLACEMENT_3D('',#63493,#22538,#22539) ;
#17679 = AXIS2_PLACEMENT_3D('',#63494,#22540,#22541) ;
#17680 = AXIS2_PLACEMENT_3D('',#63495,#22542,#22543) ;
#17681 = AXIS2_PLACEMENT_3D('',#63496,#22544,#22545) ;
#17682 = AXIS2_PLACEMENT_3D('',#63497,#22546,#22547) ;
#17683 = AXIS2_PLACEMENT_3D('',#63498,#22548,#22549) ;
#17684 = AXIS2_PLACEMENT_3D('',#63499,#22550,#22551) ;
#17685 = AXIS2_PLACEMENT_3D('',#63500,#22552,#22553) ;
#17686 = AXIS2_PLACEMENT_3D('',#63501,#22554,#22555) ;
#17687 = AXIS2_PLACEMENT_3D('',#63502,#22556,#22557) ;
#17688 = AXIS2_PLACEMENT_3D('',#63503,#22558,#22559) ;
#17689 = AXIS2_PLACEMENT_3D('',#63504,#22560,#22561) ;
#17690 = AXIS2_PLACEMENT_3D('',#63505,#22562,#22563) ;
#17691 = AXIS2_PLACEMENT_3D('',#63506,#22564,#22565) ;
#17692 = AXIS2_PLACEMENT_3D('',#63507,#22566,#22567) ;
#17693 = AXIS2_PLACEMENT_3D('',#63508,#22568,#22569) ;
#17694 = AXIS2_PLACEMENT_3D('',#63509,#22570,#22571) ;
#17695 = AXIS2_PLACEMENT_3D('',#63510,#22572,#22573) ;
#17696 = AXIS2_PLACEMENT_3D('',#63511,#22574,#22575) ;
#17697 = AXIS2_PLACEMENT_3D('',#63512,#22576,#22577) ;
#17698 = AXIS2_PLACEMENT_3D('',#63513,#22578,#22579) ;
#17699 = AXIS2_PLACEMENT_3D('',#63514,#22580,#22581) ;
#17700 = AXIS2_PLACEMENT_3D('',#63515,#22582,#22583) ;
#17701 = AXIS2_PLACEMENT_3D('',#63516,#22584,#22585) ;
#17702 = AXIS2_PLACEMENT_3D('',#63517,#22586,#22587) ;
#17703 = AXIS2_PLACEMENT_3D('',#63518,#22588,#22589) ;
#17704 = AXIS2_PLACEMENT_3D('',#63519,#22590,#22591) ;
#17705 = AXIS2_PLACEMENT_3D('',#63520,#22592,#22593) ;
#17706 = AXIS2_PLACEMENT_3D('',#63521,#22594,#22595) ;
#17707 = AXIS2_PLACEMENT_3D('',#63522,#22596,#22597) ;
#17708 = AXIS2_PLACEMENT_3D('',#63523,#22598,#22599) ;
#17709 = AXIS2_PLACEMENT_3D('',#63524,#22600,#22601) ;
#17710 = AXIS2_PLACEMENT_3D('',#63525,#22602,#22603) ;
#17711 = AXIS2_PLACEMENT_3D('',#63526,#22604,#22605) ;
#17712 = AXIS2_PLACEMENT_3D('',#63527,#22606,#22607) ;
#17713 = AXIS2_PLACEMENT_3D('',#63528,#22608,#22609) ;
#17714 = AXIS2_PLACEMENT_3D('',#63529,#22610,#22611) ;
#17715 = AXIS2_PLACEMENT_3D('',#63530,#22612,#22613) ;
#17716 = AXIS2_PLACEMENT_3D('',#63531,#22614,#22615) ;
#17717 = AXIS2_PLACEMENT_3D('',#63532,#22616,#22617) ;
#17718 = AXIS2_PLACEMENT_3D('',#63533,#22618,#22619) ;
#17719 = AXIS2_PLACEMENT_3D('',#63534,#22620,#22621) ;
#17720 = AXIS2_PLACEMENT_3D('',#63535,#22622,#22623) ;
#17721 = AXIS2_PLACEMENT_3D('',#63536,#22624,#22625) ;
#17722 = AXIS2_PLACEMENT_3D('',#63537,#22626,#22627) ;
#17723 = AXIS2_PLACEMENT_3D('',#63538,#22628,#22629) ;
#17724 = AXIS2_PLACEMENT_3D('',#63539,#22630,#22631) ;
#17725 = AXIS2_PLACEMENT_3D('',#63540,#22632,#22633) ;
#17726 = AXIS2_PLACEMENT_3D('',#63541,#22634,#22635) ;
#17727 = AXIS2_PLACEMENT_3D('',#63542,#22636,#22637) ;
#17728 = AXIS2_PLACEMENT_3D('',#63543,#22638,#22639) ;
#17729 = AXIS2_PLACEMENT_3D('',#63544,#22640,#22641) ;
#17730 = AXIS2_PLACEMENT_3D('',#63545,#22642,#22643) ;
#17731 = AXIS2_PLACEMENT_3D('',#63546,#22644,#22645) ;
#17732 = AXIS2_PLACEMENT_3D('',#63547,#22646,#22647) ;
#17733 = AXIS2_PLACEMENT_3D('',#63548,#22648,#22649) ;
#17734 = AXIS2_PLACEMENT_3D('',#63549,#22650,#22651) ;
#17735 = AXIS2_PLACEMENT_3D('',#63550,#22652,#22653) ;
#17736 = AXIS2_PLACEMENT_3D('',#63551,#22654,#22655) ;
#17737 = AXIS2_PLACEMENT_3D('',#63552,#22656,#22657) ;
#17738 = AXIS2_PLACEMENT_3D('',#63553,#22658,#22659) ;
#17739 = AXIS2_PLACEMENT_3D('',#63554,#22660,#22661) ;
#17740 = AXIS2_PLACEMENT_3D('',#63555,#22662,#22663) ;
#17741 = AXIS2_PLACEMENT_3D('',#63556,#22664,#22665) ;
#17742 = AXIS2_PLACEMENT_3D('',#63557,#22666,#22667) ;
#17743 = AXIS2_PLACEMENT_3D('',#63558,#22668,#22669) ;
#17744 = AXIS2_PLACEMENT_3D('',#63559,#22670,#22671) ;
#17745 = AXIS2_PLACEMENT_3D('',#63560,#22672,#22673) ;
#17746 = AXIS2_PLACEMENT_3D('',#63561,#22674,#22675) ;
#17747 = AXIS2_PLACEMENT_3D('',#63562,#22676,#22677) ;
#17748 = AXIS2_PLACEMENT_3D('',#63563,#22678,#22679) ;
#17749 = AXIS2_PLACEMENT_3D('',#63564,#22680,#22681) ;
#17750 = AXIS2_PLACEMENT_3D('',#63565,#22682,#22683) ;
#17751 = AXIS2_PLACEMENT_3D('',#63566,#22684,#22685) ;
#17752 = AXIS2_PLACEMENT_3D('',#63567,#22686,#22687) ;
#17753 = AXIS2_PLACEMENT_3D('',#63568,#22688,#22689) ;
#17754 = AXIS2_PLACEMENT_3D('',#63569,#22690,#22691) ;
#17755 = AXIS2_PLACEMENT_3D('',#63570,#22692,#22693) ;
#17756 = AXIS2_PLACEMENT_3D('',#63571,#22694,#22695) ;
#17757 = AXIS2_PLACEMENT_3D('',#63572,#22696,#22697) ;
#17758 = AXIS2_PLACEMENT_3D('',#63573,#22698,#22699) ;
#17759 = AXIS2_PLACEMENT_3D('',#63574,#22700,#22701) ;
#17760 = AXIS2_PLACEMENT_3D('',#63575,#22702,#22703) ;
#17761 = AXIS2_PLACEMENT_3D('',#63576,#22704,#22705) ;
#17762 = AXIS2_PLACEMENT_3D('',#63577,#22706,#22707) ;
#17763 = AXIS2_PLACEMENT_3D('',#63578,#22708,#22709) ;
#17764 = AXIS2_PLACEMENT_3D('',#63579,#22710,#22711) ;
#17765 = AXIS2_PLACEMENT_3D('',#63580,#22712,#22713) ;
#17766 = AXIS2_PLACEMENT_3D('',#63581,#22714,#22715) ;
#17767 = AXIS2_PLACEMENT_3D('',#63582,#22716,#22717) ;
#17768 = AXIS2_PLACEMENT_3D('',#63583,#22718,#22719) ;
#17769 = AXIS2_PLACEMENT_3D('',#63584,#22720,#22721) ;
#17770 = AXIS2_PLACEMENT_3D('',#63585,#22722,#22723) ;
#17771 = AXIS2_PLACEMENT_3D('',#63586,#22724,#22725) ;
#17772 = AXIS2_PLACEMENT_3D('',#63587,#22726,#22727) ;
#17773 = AXIS2_PLACEMENT_3D('',#63588,#22728,#22729) ;
#17774 = AXIS2_PLACEMENT_3D('',#63589,#22730,#22731) ;
#17775 = AXIS2_PLACEMENT_3D('',#63590,#22732,#22733) ;
#17776 = AXIS2_PLACEMENT_3D('',#63591,#22734,#22735) ;
#17777 = AXIS2_PLACEMENT_3D('',#63592,#22736,#22737) ;
#17778 = AXIS2_PLACEMENT_3D('',#63593,#22738,#22739) ;
#17779 = AXIS2_PLACEMENT_3D('',#63594,#22740,#22741) ;
#17780 = AXIS2_PLACEMENT_3D('',#63595,#22742,#22743) ;
#17781 = AXIS2_PLACEMENT_3D('',#63596,#22744,#22745) ;
#17782 = AXIS2_PLACEMENT_3D('',#63597,#22746,#22747) ;
#17783 = AXIS2_PLACEMENT_3D('',#63598,#22748,#22749) ;
#17784 = AXIS2_PLACEMENT_3D('',#63599,#22750,#22751) ;
#17785 = AXIS2_PLACEMENT_3D('',#63600,#22752,#22753) ;
#17786 = AXIS2_PLACEMENT_3D('',#63601,#22754,#22755) ;
#17787 = AXIS2_PLACEMENT_3D('',#63602,#22756,#22757) ;
#17788 = AXIS2_PLACEMENT_3D('',#63603,#22758,#22759) ;
#17789 = AXIS2_PLACEMENT_3D('',#63604,#22760,#22761) ;
#17790 = AXIS2_PLACEMENT_3D('',#63605,#22762,#22763) ;
#17791 = AXIS2_PLACEMENT_3D('',#63606,#22764,#22765) ;
#17792 = AXIS2_PLACEMENT_3D('',#63607,#22766,#22767) ;
#17793 = AXIS2_PLACEMENT_3D('',#63608,#22768,#22769) ;
#17794 = AXIS2_PLACEMENT_3D('',#63609,#22770,#22771) ;
#17795 = AXIS2_PLACEMENT_3D('',#63610,#22772,#22773) ;
#17796 = AXIS2_PLACEMENT_3D('',#63611,#22774,#22775) ;
#17797 = AXIS2_PLACEMENT_3D('',#63612,#22776,#22777) ;
#17798 = AXIS2_PLACEMENT_3D('',#63613,#22778,#22779) ;
#17799 = AXIS2_PLACEMENT_3D('',#63614,#22780,#22781) ;
#17800 = AXIS2_PLACEMENT_3D('',#63615,#22782,#22783) ;
#17801 = AXIS2_PLACEMENT_3D('',#63616,#22784,#22785) ;
#17802 = AXIS2_PLACEMENT_3D('',#63617,#22786,#22787) ;
#17803 = AXIS2_PLACEMENT_3D('',#63618,#22788,#22789) ;
#17804 = AXIS2_PLACEMENT_3D('',#63620,#22790,#22791) ;
#17805 = AXIS2_PLACEMENT_3D('',#63623,#22793,#22794) ;
#17806 = AXIS2_PLACEMENT_3D('',#63624,#22795,#22796) ;
#17807 = AXIS2_PLACEMENT_3D('',#63626,#22797,#22798) ;
#17808 = AXIS2_PLACEMENT_3D('',#63627,#22799,#22800) ;
#17809 = AXIS2_PLACEMENT_3D('',#63629,#22801,#22802) ;
#17810 = AXIS2_PLACEMENT_3D('',#63631,#22804,#22805) ;
#17811 = AXIS2_PLACEMENT_3D('',#63633,#22806,#22807) ;
#17812 = AXIS2_PLACEMENT_3D('',#63635,#22809,#22810) ;
#17813 = AXIS2_PLACEMENT_3D('',#63638,#22812,#22813) ;
#17814 = AXIS2_PLACEMENT_3D('',#63639,#22814,#22815) ;
#17815 = AXIS2_PLACEMENT_3D('',#63642,#22817,#22818) ;
#17816 = AXIS2_PLACEMENT_3D('',#63643,#22819,#22820) ;
#17817 = AXIS2_PLACEMENT_3D('',#63645,#22821,#22822) ;
#17818 = AXIS2_PLACEMENT_3D('',#63646,#22823,#22824) ;
#17819 = AXIS2_PLACEMENT_3D('',#63648,#22826,#22827) ;
#17820 = AXIS2_PLACEMENT_3D('',#63649,#22828,#22829) ;
#17821 = AXIS2_PLACEMENT_3D('',#63651,#22830,#22831) ;
#17822 = AXIS2_PLACEMENT_3D('',#63654,#22833,#22834) ;
#17823 = AXIS2_PLACEMENT_3D('',#63655,#22835,#22836) ;
#17824 = AXIS2_PLACEMENT_3D('',#63657,#22837,#22838) ;
#17825 = AXIS2_PLACEMENT_3D('',#63660,#22840,#22841) ;
#17826 = AXIS2_PLACEMENT_3D('',#63661,#22842,#22843) ;
#17827 = AXIS2_PLACEMENT_3D('',#63663,#22844,#22845) ;
#17828 = AXIS2_PLACEMENT_3D('',#63666,#22847,#22848) ;
#17829 = AXIS2_PLACEMENT_3D('',#63667,#22849,#22850) ;
#17830 = AXIS2_PLACEMENT_3D('',#63669,#22851,#22852) ;
#17831 = AXIS2_PLACEMENT_3D('',#63672,#22854,#22855) ;
#17832 = AXIS2_PLACEMENT_3D('',#63673,#22856,#22857) ;
#17833 = AXIS2_PLACEMENT_3D('',#63675,#22858,#22859) ;
#17834 = AXIS2_PLACEMENT_3D('',#63678,#22861,#22862) ;
#17835 = AXIS2_PLACEMENT_3D('',#63679,#22863,#22864) ;
#17836 = AXIS2_PLACEMENT_3D('',#63681,#22865,#22866) ;
#17837 = AXIS2_PLACEMENT_3D('',#63684,#22868,#22869) ;
#17838 = AXIS2_PLACEMENT_3D('',#63685,#22870,#22871) ;
#17839 = AXIS2_PLACEMENT_3D('',#63687,#22872,#22873) ;
#17840 = AXIS2_PLACEMENT_3D('',#63690,#22875,#22876) ;
#17841 = AXIS2_PLACEMENT_3D('',#63691,#22877,#22878) ;
#17842 = AXIS2_PLACEMENT_3D('',#63693,#22879,#22880) ;
#17843 = AXIS2_PLACEMENT_3D('',#63696,#22882,#22883) ;
#17844 = AXIS2_PLACEMENT_3D('',#63697,#22884,#22885) ;
#17845 = AXIS2_PLACEMENT_3D('',#63699,#22886,#22887) ;
#17846 = AXIS2_PLACEMENT_3D('',#63702,#22889,#22890) ;
#17847 = AXIS2_PLACEMENT_3D('',#63703,#22891,#22892) ;
#17848 = AXIS2_PLACEMENT_3D('',#63705,#22893,#22894) ;
#17849 = AXIS2_PLACEMENT_3D('',#63708,#22896,#22897) ;
#17850 = AXIS2_PLACEMENT_3D('',#63709,#22898,#22899) ;
#17851 = AXIS2_PLACEMENT_3D('',#63710,#22900,#22901) ;
#17852 = AXIS2_PLACEMENT_3D('',#63711,#22902,#22903) ;
#17853 = AXIS2_PLACEMENT_3D('',#63712,#22904,#22905) ;
#17854 = AXIS2_PLACEMENT_3D('',#63714,#22906,#22907) ;
#17855 = AXIS2_PLACEMENT_3D('',#63717,#22909,#22910) ;
#17856 = AXIS2_PLACEMENT_3D('',#63718,#22911,#22912) ;
#17857 = AXIS2_PLACEMENT_3D('',#63720,#22913,#22914) ;
#17858 = AXIS2_PLACEMENT_3D('',#63723,#22916,#22917) ;
#17859 = AXIS2_PLACEMENT_3D('',#63724,#22918,#22919) ;
#17860 = AXIS2_PLACEMENT_3D('',#63726,#22920,#22921) ;
#17861 = AXIS2_PLACEMENT_3D('',#63729,#22923,#22924) ;
#17862 = AXIS2_PLACEMENT_3D('',#63730,#22925,#22926) ;
#17863 = AXIS2_PLACEMENT_3D('',#63732,#22927,#22928) ;
#17864 = AXIS2_PLACEMENT_3D('',#63735,#22930,#22931) ;
#17865 = AXIS2_PLACEMENT_3D('',#63736,#22932,#22933) ;
#17866 = AXIS2_PLACEMENT_3D('',#63738,#22934,#22935) ;
#17867 = AXIS2_PLACEMENT_3D('',#63741,#22937,#22938) ;
#17868 = AXIS2_PLACEMENT_3D('',#63742,#22939,#22940) ;
#17869 = AXIS2_PLACEMENT_3D('',#63744,#22941,#22942) ;
#17870 = AXIS2_PLACEMENT_3D('',#63747,#22944,#22945) ;
#17871 = AXIS2_PLACEMENT_3D('',#63748,#22946,#22947) ;
#17872 = AXIS2_PLACEMENT_3D('',#63750,#22948,#22949) ;
#17873 = AXIS2_PLACEMENT_3D('',#63753,#22951,#22952) ;
#17874 = AXIS2_PLACEMENT_3D('',#63754,#22953,#22954) ;
#17875 = AXIS2_PLACEMENT_3D('',#63756,#22955,#22956) ;
#17876 = AXIS2_PLACEMENT_3D('',#63759,#22958,#22959) ;
#17877 = AXIS2_PLACEMENT_3D('',#63760,#22960,#22961) ;
#17878 = AXIS2_PLACEMENT_3D('',#63762,#22962,#22963) ;
#17879 = AXIS2_PLACEMENT_3D('',#63765,#22965,#22966) ;
#17880 = AXIS2_PLACEMENT_3D('',#63766,#22967,#22968) ;
#17881 = AXIS2_PLACEMENT_3D('',#63768,#22969,#22970) ;
#17882 = AXIS2_PLACEMENT_3D('',#63771,#22972,#22973) ;
#17883 = AXIS2_PLACEMENT_3D('',#63772,#22974,#22975) ;
#17884 = AXIS2_PLACEMENT_3D('',#63773,#22976,#22977) ;
#17885 = AXIS2_PLACEMENT_3D('',#63774,#22978,#22979) ;
#17886 = AXIS2_PLACEMENT_3D('',#63775,#22980,#22981) ;
#17887 = AXIS2_PLACEMENT_3D('',#63776,#22982,#22983) ;
#17888 = AXIS2_PLACEMENT_3D('',#63777,#22984,#22985) ;
#17889 = AXIS2_PLACEMENT_3D('',#63778,#22986,#22987) ;
#17890 = AXIS2_PLACEMENT_3D('',#63779,#22988,#22989) ;
#17891 = AXIS2_PLACEMENT_3D('',#63780,#22990,#22991) ;
#17892 = AXIS2_PLACEMENT_3D('',#63781,#22992,#22993) ;
#17893 = AXIS2_PLACEMENT_3D('',#63782,#22994,#22995) ;
#17894 = AXIS2_PLACEMENT_3D('',#63783,#22996,#22997) ;
#17895 = AXIS2_PLACEMENT_3D('',#63784,#22998,#22999) ;
#17896 = AXIS2_PLACEMENT_3D('',#63785,#23000,#23001) ;
#17897 = AXIS2_PLACEMENT_3D('',#63786,#23002,#23003) ;
#17898 = AXIS2_PLACEMENT_3D('',#63787,#23004,#23005) ;
#17899 = AXIS2_PLACEMENT_3D('',#63788,#23006,#23007) ;
#17900 = AXIS2_PLACEMENT_3D('',#63789,#23008,#23009) ;
#17901 = AXIS2_PLACEMENT_3D('',#63790,#23010,#23011) ;
#17902 = DIRECTION('axis',(0.,0.,1.)) ;
#17903 = DIRECTION('refdir',(1.,0.,0.)) ;
#17904 = DIRECTION('axis',(0.,0.,1.)) ;
#17905 = DIRECTION('refdir',(1.,0.,0.)) ;
#17906 = DIRECTION('center_axis',(-9.473903143468E-16,1.,0.)) ;
#17907 = DIRECTION('ref_axis',(0.,0.,1.)) ;
#17908 = DIRECTION('',(-5.92914802803472E-16,0.515038074910058,-0.85716730070211)) ;
#17909 = DIRECTION('center_axis',(9.473903143468E-16,-1.,0.)) ;
#17910 = DIRECTION('ref_axis',(0.,0.,1.)) ;
#17911 = DIRECTION('center_axis',(9.473903143468E-16,-1.,0.)) ;
#17912 = DIRECTION('ref_axis',(0.,0.,1.)) ;
#17913 = DIRECTION('center_axis',(9.47390314346801E-16,-1.,0.)) ;
#17914 = DIRECTION('ref_axis',(0.,0.,1.)) ;
#17915 = DIRECTION('',(9.473903143468E-16,-1.,0.)) ;
#17916 = DIRECTION('center_axis',(-9.473903143468E-16,1.,0.)) ;
#17917 = DIRECTION('ref_axis',(0.,0.,1.)) ;
#17918 = DIRECTION('',(-5.92914802803472E-16,0.515038074910058,-0.85716730070211)) ;
#17919 = DIRECTION('center_axis',(9.473903143468E-16,-1.,0.)) ;
#17920 = DIRECTION('ref_axis',(0.,0.,1.)) ;
#17921 = DIRECTION('center_axis',(9.473903143468E-16,-1.,0.)) ;
#17922 = DIRECTION('ref_axis',(0.,0.,1.)) ;
#17923 = DIRECTION('center_axis',(9.47390314346801E-16,-1.,0.)) ;
#17924 = DIRECTION('ref_axis',(0.,0.,1.)) ;
#17925 = DIRECTION('',(9.473903143468E-16,-1.,0.)) ;
#17926 = DIRECTION('center_axis',(-3.5527136788005E-16,-1.,0.)) ;
#17927 = DIRECTION('ref_axis',(0.,0.,-1.)) ;
#17928 = DIRECTION('',(-2.87951000497466E-16,-0.515038074910058,0.85716730070211)) ;
#17929 = DIRECTION('center_axis',(3.5527136788005E-16,1.,0.)) ;
#17930 = DIRECTION('ref_axis',(0.,0.,-1.)) ;
#17931 = DIRECTION('center_axis',(3.5527136788005E-16,1.,0.)) ;
#17932 = DIRECTION('ref_axis',(0.,0.,-1.)) ;
#17933 = DIRECTION('center_axis',(4.2632564145606E-15,1.,0.)) ;
#17934 = DIRECTION('ref_axis',(0.,0.,-1.)) ;
#17935 = DIRECTION('',(3.5527136788005E-16,1.,0.)) ;
#17936 = DIRECTION('center_axis',(-3.5527136788005E-16,-1.,0.)) ;
#17937 = DIRECTION('ref_axis',(0.,0.,-1.)) ;
#17938 = DIRECTION('',(-2.87951000497466E-16,-0.515038074910058,0.85716730070211)) ;
#17939 = DIRECTION('center_axis',(3.5527136788005E-16,1.,0.)) ;
#17940 = DIRECTION('ref_axis',(0.,0.,-1.)) ;
#17941 = DIRECTION('center_axis',(3.5527136788005E-16,1.,0.)) ;
#17942 = DIRECTION('ref_axis',(0.,0.,-1.)) ;
#17943 = DIRECTION('center_axis',(4.2632564145606E-15,1.,0.)) ;
#17944 = DIRECTION('ref_axis',(0.,0.,-1.)) ;
#17945 = DIRECTION('',(3.5527136788005E-16,1.,0.)) ;
#17946 = DIRECTION('center_axis',(0.,0.,-1.)) ;
#17947 = DIRECTION('ref_axis',(1.,0.,0.)) ;
#17948 = DIRECTION('center_axis',(0.,0.,-1.)) ;
#17949 = DIRECTION('ref_axis',(1.,0.,0.)) ;
#17950 = DIRECTION('center_axis',(0.,0.,-1.)) ;
#17951 = DIRECTION('ref_axis',(1.,0.,0.)) ;
#17952 = DIRECTION('center_axis',(0.,0.,-1.)) ;
#17953 = DIRECTION('ref_axis',(1.,0.,0.)) ;
#17954 = DIRECTION('center_axis',(0.,0.,-1.)) ;
#17955 = DIRECTION('ref_axis',(1.,0.,0.)) ;
#17956 = DIRECTION('',(0.,0.,-1.)) ;
#17957 = DIRECTION('center_axis',(0.,0.,-1.)) ;
#17958 = DIRECTION('ref_axis',(1.,0.,0.)) ;
#17959 = DIRECTION('',(0.,0.,-1.)) ;
#17960 = DIRECTION('center_axis',(0.,0.,1.)) ;
#17961 = DIRECTION('ref_axis',(1.,0.,0.)) ;
#17962 = DIRECTION('center_axis',(0.,0.,-1.)) ;
#17963 = DIRECTION('ref_axis',(1.,0.,0.)) ;
#17964 = DIRECTION('center_axis',(0.,0.,-1.)) ;
#17965 = DIRECTION('ref_axis',(1.,0.,0.)) ;
#17966 = DIRECTION('center_axis',(0.,0.,-1.)) ;
#17967 = DIRECTION('ref_axis',(1.,0.,0.)) ;
#17968 = DIRECTION('center_axis',(0.,0.,-1.)) ;
#17969 = DIRECTION('ref_axis',(1.,0.,0.)) ;
#17970 = DIRECTION('center_axis',(0.,0.,-1.)) ;
#17971 = DIRECTION('ref_axis',(1.,0.,0.)) ;
#17972 = DIRECTION('',(0.,0.,-1.)) ;
#17973 = DIRECTION('center_axis',(0.,0.,-1.)) ;
#17974 = DIRECTION('ref_axis',(1.,0.,0.)) ;
#17975 = DIRECTION('',(0.,0.,-1.)) ;
#17976 = DIRECTION('center_axis',(0.,0.,1.)) ;
#17977 = DIRECTION('ref_axis',(1.,0.,0.)) ;
#17978 = DIRECTION('center_axis',(0.,0.,-1.)) ;
#17979 = DIRECTION('ref_axis',(1.,0.,0.)) ;
#17980 = DIRECTION('center_axis',(0.,0.,-1.)) ;
#17981 = DIRECTION('ref_axis',(1.,0.,0.)) ;
#17982 = DIRECTION('center_axis',(0.,0.,-1.)) ;
#17983 = DIRECTION('ref_axis',(1.,0.,0.)) ;
#17984 = DIRECTION('center_axis',(0.,0.,-1.)) ;
#17985 = DIRECTION('ref_axis',(1.,0.,0.)) ;
#17986 = DIRECTION('center_axis',(0.,0.,-1.)) ;
#17987 = DIRECTION('ref_axis',(1.,0.,0.)) ;
#17988 = DIRECTION('',(0.,0.,-1.)) ;
#17989 = DIRECTION('center_axis',(0.,0.,-1.)) ;
#17990 = DIRECTION('ref_axis',(1.,0.,0.)) ;
#17991 = DIRECTION('',(0.,0.,-1.)) ;
#17992 = DIRECTION('center_axis',(0.,0.,1.)) ;
#17993 = DIRECTION('ref_axis',(1.,0.,0.)) ;
#17994 = DIRECTION('center_axis',(0.,0.,-1.)) ;
#17995 = DIRECTION('ref_axis',(1.,0.,0.)) ;
#17996 = DIRECTION('center_axis',(0.,0.,-1.)) ;
#17997 = DIRECTION('ref_axis',(1.,0.,0.)) ;
#17998 = DIRECTION('center_axis',(0.,0.,-1.)) ;
#17999 = DIRECTION('ref_axis',(1.,0.,0.)) ;
#18000 = DIRECTION('center_axis',(0.,0.,-1.)) ;
#18001 = DIRECTION('ref_axis',(1.,0.,0.)) ;
#18002 = DIRECTION('center_axis',(0.,0.,-1.)) ;
#18003 = DIRECTION('ref_axis',(1.,0.,0.)) ;
#18004 = DIRECTION('',(0.,0.,-1.)) ;
#18005 = DIRECTION('center_axis',(0.,0.,-1.)) ;
#18006 = DIRECTION('ref_axis',(1.,0.,0.)) ;
#18007 = DIRECTION('',(0.,0.,-1.)) ;
#18008 = DIRECTION('center_axis',(0.,0.,1.)) ;
#18009 = DIRECTION('ref_axis',(1.,0.,0.)) ;
#18010 = DIRECTION('center_axis',(0.,0.,-1.)) ;
#18011 = DIRECTION('ref_axis',(-1.,0.,0.)) ;
#18012 = DIRECTION('',(0.85716730070211,-1.04972719113862E-16,-0.515038074910058)) ;
#18013 = DIRECTION('center_axis',(0.,0.,1.)) ;
#18014 = DIRECTION('ref_axis',(-1.,0.,0.)) ;
#18015 = DIRECTION('center_axis',(0.,0.,1.)) ;
#18016 = DIRECTION('ref_axis',(-1.,0.,0.)) ;
#18017 = DIRECTION('center_axis',(0.,0.,1.)) ;
#18018 = DIRECTION('ref_axis',(-1.,0.,0.)) ;
#18019 = DIRECTION('',(0.,0.,1.)) ;
#18020 = DIRECTION('center_axis',(0.,0.,-1.)) ;
#18021 = DIRECTION('ref_axis',(-1.,0.,0.)) ;
#18022 = DIRECTION('',(0.85716730070211,-1.04972719113862E-16,-0.515038074910058)) ;
#18023 = DIRECTION('center_axis',(0.,0.,1.)) ;
#18024 = DIRECTION('ref_axis',(-1.,0.,0.)) ;
#18025 = DIRECTION('center_axis',(0.,0.,1.)) ;
#18026 = DIRECTION('ref_axis',(-1.,0.,0.)) ;
#18027 = DIRECTION('center_axis',(0.,0.,-1.)) ;
#18028 = DIRECTION('ref_axis',(-1.,0.,0.)) ;
#18029 = DIRECTION('',(0.,0.,1.)) ;
#18030 = DIRECTION('center_axis',(0.,0.,-1.)) ;
#18031 = DIRECTION('ref_axis',(-1.,0.,0.)) ;
#18032 = DIRECTION('',(0.85716730070211,-1.04972719113862E-16,-0.515038074910058)) ;
#18033 = DIRECTION('center_axis',(0.,0.,1.)) ;
#18034 = DIRECTION('ref_axis',(-1.,0.,0.)) ;
#18035 = DIRECTION('center_axis',(0.,0.,1.)) ;
#18036 = DIRECTION('ref_axis',(-1.,0.,0.)) ;
#18037 = DIRECTION('center_axis',(0.,0.,-1.)) ;
#18038 = DIRECTION('ref_axis',(-1.,0.,0.)) ;
#18039 = DIRECTION('',(0.,0.,1.)) ;
#18040 = DIRECTION('center_axis',(0.,0.,-1.)) ;
#18041 = DIRECTION('ref_axis',(-1.,0.,0.)) ;
#18042 = DIRECTION('',(0.85716730070211,-1.04972719113862E-16,-0.515038074910058)) ;
#18043 = DIRECTION('center_axis',(0.,0.,1.)) ;
#18044 = DIRECTION('ref_axis',(-1.,0.,0.)) ;
#18045 = DIRECTION('center_axis',(0.,0.,1.)) ;
#18046 = DIRECTION('ref_axis',(-1.,0.,0.)) ;
#18047 = DIRECTION('center_axis',(0.,0.,-1.)) ;
#18048 = DIRECTION('ref_axis',(-1.,0.,0.)) ;
#18049 = DIRECTION('',(0.,0.,1.)) ;
#18050 = DIRECTION('center_axis',(0.,0.,-1.)) ;
#18051 = DIRECTION('ref_axis',(-1.,0.,0.)) ;
#18052 = DIRECTION('',(0.85716730070211,-1.04972719113862E-16,-0.515038074910058)) ;
#18053 = DIRECTION('center_axis',(0.,0.,1.)) ;
#18054 = DIRECTION('ref_axis',(-1.,0.,0.)) ;
#18055 = DIRECTION('center_axis',(0.,0.,1.)) ;
#18056 = DIRECTION('ref_axis',(-1.,0.,0.)) ;
#18057 = DIRECTION('center_axis',(0.,0.,-1.)) ;
#18058 = DIRECTION('ref_axis',(-1.,0.,0.)) ;
#18059 = DIRECTION('',(0.,0.,1.)) ;
#18060 = DIRECTION('center_axis',(0.,0.,-1.)) ;
#18061 = DIRECTION('ref_axis',(-1.,0.,0.)) ;
#18062 = DIRECTION('',(0.85716730070211,-1.04972719113862E-16,-0.515038074910058)) ;
#18063 = DIRECTION('center_axis',(0.,0.,1.)) ;
#18064 = DIRECTION('ref_axis',(-1.,0.,0.)) ;
#18065 = DIRECTION('center_axis',(0.,0.,1.)) ;
#18066 = DIRECTION('ref_axis',(-1.,0.,0.)) ;
#18067 = DIRECTION('center_axis',(0.,0.,-1.)) ;
#18068 = DIRECTION('ref_axis',(-1.,0.,0.)) ;
#18069 = DIRECTION('',(0.,0.,1.)) ;
#18070 = DIRECTION('center_axis',(0.,0.,-1.)) ;
#18071 = DIRECTION('ref_axis',(-1.,0.,0.)) ;
#18072 = DIRECTION('',(0.85716730070211,-1.04972719113862E-16,-0.515038074910058)) ;
#18073 = DIRECTION('center_axis',(0.,0.,1.)) ;
#18074 = DIRECTION('ref_axis',(-1.,0.,0.)) ;
#18075 = DIRECTION('center_axis',(0.,0.,1.)) ;
#18076 = DIRECTION('ref_axis',(-1.,0.,0.)) ;
#18077 = DIRECTION('center_axis',(0.,0.,-1.)) ;
#18078 = DIRECTION('ref_axis',(-1.,0.,0.)) ;
#18079 = DIRECTION('',(0.,0.,1.)) ;
#18080 = DIRECTION('center_axis',(0.,0.,-1.)) ;
#18081 = DIRECTION('ref_axis',(-1.,0.,0.)) ;
#18082 = DIRECTION('',(0.85716730070211,-1.04972719113862E-16,-0.515038074910058)) ;
#18083 = DIRECTION('center_axis',(0.,0.,1.)) ;
#18084 = DIRECTION('ref_axis',(-1.,0.,0.)) ;
#18085 = DIRECTION('center_axis',(0.,0.,1.)) ;
#18086 = DIRECTION('ref_axis',(-1.,0.,0.)) ;
#18087 = DIRECTION('center_axis',(0.,0.,1.)) ;
#18088 = DIRECTION('ref_axis',(-1.,0.,0.)) ;
#18089 = DIRECTION('',(0.,0.,1.)) ;
#18090 = DIRECTION('center_axis',(0.,0.,-1.)) ;
#18091 = DIRECTION('ref_axis',(1.,0.,0.)) ;
#18092 = DIRECTION('center_axis',(0.,0.,-1.)) ;
#18093 = DIRECTION('ref_axis',(1.,0.,0.)) ;
#18094 = DIRECTION('',(0.,0.,-1.)) ;
#18095 = DIRECTION('center_axis',(0.,0.,1.)) ;
#18096 = DIRECTION('ref_axis',(1.,0.,0.)) ;
#18097 = DIRECTION('center_axis',(-4.2632564145606E-15,-1.,0.)) ;
#18098 = DIRECTION('ref_axis',(-1.,4.2632564145606E-15,0.)) ;
#18099 = DIRECTION('',(1.,-4.2632564145606E-15,0.)) ;
#18100 = DIRECTION('',(0.,0.,-1.)) ;
#18101 = DIRECTION('',(-1.,4.2632564145606E-15,0.)) ;
#18102 = DIRECTION('',(0.,0.,-1.)) ;
#18103 = DIRECTION('center_axis',(1.,-2.66453525910036E-16,0.)) ;
#18104 = DIRECTION('ref_axis',(-2.66453525910036E-16,-1.,0.)) ;
#18105 = DIRECTION('',(2.66453525910036E-16,1.,0.)) ;
#18106 = DIRECTION('',(-2.66453525910036E-16,-1.,0.)) ;
#18107 = DIRECTION('',(0.,0.,-1.)) ;
#18108 = DIRECTION('center_axis',(-9.47390314346801E-16,1.,0.)) ;
#18109 = DIRECTION('ref_axis',(1.,9.47390314346801E-16,0.)) ;
#18110 = DIRECTION('',(1.,9.47390314346801E-16,0.)) ;
#18111 = DIRECTION('',(1.,9.47390314346801E-16,0.)) ;
#18112 = DIRECTION('',(0.,0.,-1.)) ;
#18113 = DIRECTION('center_axis',(-1.,1.68753899743024E-15,0.)) ;
#18114 = DIRECTION('ref_axis',(1.68753899743024E-15,1.,0.)) ;
#18115 = DIRECTION('',(-1.68753899743024E-15,-1.,0.)) ;
#18116 = DIRECTION('',(1.68753899743024E-15,1.,0.)) ;
#18117 = DIRECTION('center_axis',(0.,0.,1.)) ;
#18118 = DIRECTION('ref_axis',(1.,0.,0.)) ;
#18119 = DIRECTION('center_axis',(0.,0.,1.)) ;
#18120 = DIRECTION('ref_axis',(1.,0.,0.)) ;
#18121 = DIRECTION('axis',(0.,0.,1.)) ;
#18122 = DIRECTION('refdir',(1.,0.,0.)) ;
#18123 = DIRECTION('center_axis',(3.5527136788005E-16,1.,0.)) ;
#18124 = DIRECTION('ref_axis',(0.,0.,-1.)) ;
#18125 = DIRECTION('center_axis',(3.5527136788005E-16,1.,0.)) ;
#18126 = DIRECTION('ref_axis',(0.,0.,-1.)) ;
#18127 = DIRECTION('center_axis',(3.5527136788005E-16,1.,0.)) ;
#18128 = DIRECTION('ref_axis',(0.,0.,-1.)) ;
#18129 = DIRECTION('center_axis',(3.5527136788005E-16,1.,0.)) ;
#18130 = DIRECTION('ref_axis',(0.,0.,-1.)) ;
#18131 = DIRECTION('center_axis',(3.5527136788005E-16,1.,0.)) ;
#18132 = DIRECTION('ref_axis',(0.,0.,-1.)) ;
#18133 = DIRECTION('',(3.5527136788005E-16,1.,0.)) ;
#18134 = DIRECTION('center_axis',(3.5527136788005E-16,1.,0.)) ;
#18135 = DIRECTION('ref_axis',(0.,0.,-1.)) ;
#18136 = DIRECTION('',(3.5527136788005E-16,1.,0.)) ;
#18137 = DIRECTION('center_axis',(-4.2632564145606E-15,-1.,0.)) ;
#18138 = DIRECTION('ref_axis',(0.,0.,-1.)) ;
#18139 = DIRECTION('center_axis',(3.5527136788005E-16,1.,0.)) ;
#18140 = DIRECTION('ref_axis',(0.,0.,-1.)) ;
#18141 = DIRECTION('center_axis',(3.5527136788005E-16,1.,0.)) ;
#18142 = DIRECTION('ref_axis',(0.,0.,-1.)) ;
#18143 = DIRECTION('center_axis',(3.5527136788005E-16,1.,0.)) ;
#18144 = DIRECTION('ref_axis',(0.,0.,-1.)) ;
#18145 = DIRECTION('center_axis',(3.5527136788005E-16,1.,0.)) ;
#18146 = DIRECTION('ref_axis',(0.,0.,-1.)) ;
#18147 = DIRECTION('center_axis',(3.5527136788005E-16,1.,0.)) ;
#18148 = DIRECTION('ref_axis',(0.,0.,-1.)) ;
#18149 = DIRECTION('',(3.5527136788005E-16,1.,0.)) ;
#18150 = DIRECTION('center_axis',(3.5527136788005E-16,1.,0.)) ;
#18151 = DIRECTION('ref_axis',(0.,0.,-1.)) ;
#18152 = DIRECTION('',(3.5527136788005E-16,1.,0.)) ;
#18153 = DIRECTION('center_axis',(-4.2632564145606E-15,-1.,0.)) ;
#18154 = DIRECTION('ref_axis',(0.,0.,-1.)) ;
#18155 = DIRECTION('center_axis',(3.5527136788005E-16,1.,0.)) ;
#18156 = DIRECTION('ref_axis',(0.,0.,-1.)) ;
#18157 = DIRECTION('center_axis',(3.5527136788005E-16,1.,0.)) ;
#18158 = DIRECTION('ref_axis',(0.,0.,-1.)) ;
#18159 = DIRECTION('center_axis',(3.5527136788005E-16,1.,0.)) ;
#18160 = DIRECTION('ref_axis',(0.,0.,-1.)) ;
#18161 = DIRECTION('center_axis',(3.5527136788005E-16,1.,0.)) ;
#18162 = DIRECTION('ref_axis',(0.,0.,-1.)) ;
#18163 = DIRECTION('center_axis',(3.5527136788005E-16,1.,0.)) ;
#18164 = DIRECTION('ref_axis',(0.,0.,-1.)) ;
#18165 = DIRECTION('',(3.5527136788005E-16,1.,0.)) ;
#18166 = DIRECTION('center_axis',(3.5527136788005E-16,1.,0.)) ;
#18167 = DIRECTION('ref_axis',(0.,0.,-1.)) ;
#18168 = DIRECTION('',(3.5527136788005E-16,1.,0.)) ;
#18169 = DIRECTION('center_axis',(-4.2632564145606E-15,-1.,0.)) ;
#18170 = DIRECTION('ref_axis',(0.,0.,-1.)) ;
#18171 = DIRECTION('center_axis',(3.5527136788005E-16,1.,0.)) ;
#18172 = DIRECTION('ref_axis',(0.,0.,-1.)) ;
#18173 = DIRECTION('center_axis',(3.5527136788005E-16,1.,0.)) ;
#18174 = DIRECTION('ref_axis',(0.,0.,-1.)) ;
#18175 = DIRECTION('center_axis',(3.5527136788005E-16,1.,0.)) ;
#18176 = DIRECTION('ref_axis',(0.,0.,-1.)) ;
#18177 = DIRECTION('center_axis',(3.5527136788005E-16,1.,0.)) ;
#18178 = DIRECTION('ref_axis',(0.,0.,-1.)) ;
#18179 = DIRECTION('center_axis',(3.5527136788005E-16,1.,0.)) ;
#18180 = DIRECTION('ref_axis',(0.,0.,-1.)) ;
#18181 = DIRECTION('',(3.5527136788005E-16,1.,0.)) ;
#18182 = DIRECTION('center_axis',(3.5527136788005E-16,1.,0.)) ;
#18183 = DIRECTION('ref_axis',(0.,0.,-1.)) ;
#18184 = DIRECTION('',(3.5527136788005E-16,1.,0.)) ;
#18185 = DIRECTION('center_axis',(-4.2632564145606E-15,-1.,0.)) ;
#18186 = DIRECTION('ref_axis',(0.,0.,-1.)) ;
#18187 = DIRECTION('center_axis',(3.5527136788005E-16,1.,0.)) ;
#18188 = DIRECTION('ref_axis',(0.,0.,-1.)) ;
#18189 = DIRECTION('center_axis',(3.5527136788005E-16,1.,0.)) ;
#18190 = DIRECTION('ref_axis',(0.,0.,-1.)) ;
#18191 = DIRECTION('center_axis',(3.5527136788005E-16,1.,0.)) ;
#18192 = DIRECTION('ref_axis',(0.,0.,-1.)) ;
#18193 = DIRECTION('center_axis',(3.5527136788005E-16,1.,0.)) ;
#18194 = DIRECTION('ref_axis',(0.,0.,-1.)) ;
#18195 = DIRECTION('center_axis',(3.5527136788005E-16,1.,0.)) ;
#18196 = DIRECTION('ref_axis',(0.,0.,-1.)) ;
#18197 = DIRECTION('',(3.5527136788005E-16,1.,0.)) ;
#18198 = DIRECTION('center_axis',(3.5527136788005E-16,1.,0.)) ;
#18199 = DIRECTION('ref_axis',(0.,0.,-1.)) ;
#18200 = DIRECTION('',(3.5527136788005E-16,1.,0.)) ;
#18201 = DIRECTION('center_axis',(-4.2632564145606E-15,-1.,0.)) ;
#18202 = DIRECTION('ref_axis',(0.,0.,-1.)) ;
#18203 = DIRECTION('center_axis',(3.5527136788005E-16,1.,0.)) ;
#18204 = DIRECTION('ref_axis',(0.,0.,-1.)) ;
#18205 = DIRECTION('center_axis',(3.5527136788005E-16,1.,0.)) ;
#18206 = DIRECTION('ref_axis',(0.,0.,-1.)) ;
#18207 = DIRECTION('center_axis',(3.5527136788005E-16,1.,0.)) ;
#18208 = DIRECTION('ref_axis',(0.,0.,-1.)) ;
#18209 = DIRECTION('center_axis',(3.5527136788005E-16,1.,0.)) ;
#18210 = DIRECTION('ref_axis',(0.,0.,-1.)) ;
#18211 = DIRECTION('center_axis',(3.5527136788005E-16,1.,0.)) ;
#18212 = DIRECTION('ref_axis',(0.,0.,-1.)) ;
#18213 = DIRECTION('',(3.5527136788005E-16,1.,0.)) ;
#18214 = DIRECTION('center_axis',(3.5527136788005E-16,1.,0.)) ;
#18215 = DIRECTION('ref_axis',(0.,0.,-1.)) ;
#18216 = DIRECTION('',(3.5527136788005E-16,1.,0.)) ;
#18217 = DIRECTION('center_axis',(-4.2632564145606E-15,-1.,0.)) ;
#18218 = DIRECTION('ref_axis',(0.,0.,-1.)) ;
#18219 = DIRECTION('center_axis',(3.5527136788005E-16,1.,0.)) ;
#18220 = DIRECTION('ref_axis',(0.,0.,-1.)) ;
#18221 = DIRECTION('center_axis',(3.5527136788005E-16,1.,0.)) ;
#18222 = DIRECTION('ref_axis',(0.,0.,-1.)) ;
#18223 = DIRECTION('center_axis',(3.5527136788005E-16,1.,0.)) ;
#18224 = DIRECTION('ref_axis',(0.,0.,-1.)) ;
#18225 = DIRECTION('center_axis',(3.5527136788005E-16,1.,0.)) ;
#18226 = DIRECTION('ref_axis',(0.,0.,-1.)) ;
#18227 = DIRECTION('center_axis',(3.5527136788005E-16,1.,0.)) ;
#18228 = DIRECTION('ref_axis',(0.,0.,-1.)) ;
#18229 = DIRECTION('',(3.5527136788005E-16,1.,0.)) ;
#18230 = DIRECTION('center_axis',(3.5527136788005E-16,1.,0.)) ;
#18231 = DIRECTION('ref_axis',(0.,0.,-1.)) ;
#18232 = DIRECTION('',(3.5527136788005E-16,1.,0.)) ;
#18233 = DIRECTION('center_axis',(-4.2632564145606E-15,-1.,0.)) ;
#18234 = DIRECTION('ref_axis',(0.,0.,-1.)) ;
#18235 = DIRECTION('center_axis',(3.5527136788005E-16,1.,0.)) ;
#18236 = DIRECTION('ref_axis',(0.,0.,-1.)) ;
#18237 = DIRECTION('center_axis',(3.5527136788005E-16,1.,0.)) ;
#18238 = DIRECTION('ref_axis',(0.,0.,-1.)) ;
#18239 = DIRECTION('center_axis',(3.5527136788005E-16,1.,0.)) ;
#18240 = DIRECTION('ref_axis',(0.,0.,-1.)) ;
#18241 = DIRECTION('center_axis',(3.5527136788005E-16,1.,0.)) ;
#18242 = DIRECTION('ref_axis',(0.,0.,-1.)) ;
#18243 = DIRECTION('center_axis',(3.5527136788005E-16,1.,0.)) ;
#18244 = DIRECTION('ref_axis',(0.,0.,-1.)) ;
#18245 = DIRECTION('',(3.5527136788005E-16,1.,0.)) ;
#18246 = DIRECTION('center_axis',(3.5527136788005E-16,1.,0.)) ;
#18247 = DIRECTION('ref_axis',(0.,0.,-1.)) ;
#18248 = DIRECTION('',(3.5527136788005E-16,1.,0.)) ;
#18249 = DIRECTION('center_axis',(-4.2632564145606E-15,-1.,0.)) ;
#18250 = DIRECTION('ref_axis',(0.,0.,-1.)) ;
#18251 = DIRECTION('center_axis',(1.77635683940025E-15,-1.,0.)) ;
#18252 = DIRECTION('ref_axis',(0.,0.,1.)) ;
#18253 = DIRECTION('center_axis',(1.77635683940025E-15,-1.,0.)) ;
#18254 = DIRECTION('ref_axis',(0.,0.,1.)) ;
#18255 = DIRECTION('center_axis',(1.77635683940025E-15,-1.,0.)) ;
#18256 = DIRECTION('ref_axis',(0.,0.,1.)) ;
#18257 = DIRECTION('center_axis',(1.77635683940025E-15,-1.,0.)) ;
#18258 = DIRECTION('ref_axis',(0.,0.,1.)) ;
#18259 = DIRECTION('center_axis',(-4.2632564145606E-15,-1.,0.)) ;
#18260 = DIRECTION('ref_axis',(0.,0.,1.)) ;
#18261 = DIRECTION('',(1.77635683940025E-15,-1.,0.)) ;
#18262 = DIRECTION('center_axis',(1.77635683940025E-15,-1.,0.)) ;
#18263 = DIRECTION('ref_axis',(0.,0.,1.)) ;
#18264 = DIRECTION('',(1.77635683940025E-15,-1.,0.)) ;
#18265 = DIRECTION('center_axis',(3.5527136788005E-16,1.,0.)) ;
#18266 = DIRECTION('ref_axis',(0.,0.,1.)) ;
#18267 = DIRECTION('center_axis',(1.77635683940025E-15,-1.,0.)) ;
#18268 = DIRECTION('ref_axis',(0.,0.,1.)) ;
#18269 = DIRECTION('center_axis',(1.77635683940025E-15,-1.,0.)) ;
#18270 = DIRECTION('ref_axis',(0.,0.,1.)) ;
#18271 = DIRECTION('center_axis',(1.77635683940025E-15,-1.,0.)) ;
#18272 = DIRECTION('ref_axis',(0.,0.,1.)) ;
#18273 = DIRECTION('center_axis',(1.77635683940025E-15,-1.,0.)) ;
#18274 = DIRECTION('ref_axis',(0.,0.,1.)) ;
#18275 = DIRECTION('center_axis',(-4.2632564145606E-15,-1.,0.)) ;
#18276 = DIRECTION('ref_axis',(0.,0.,1.)) ;
#18277 = DIRECTION('',(1.77635683940025E-15,-1.,0.)) ;
#18278 = DIRECTION('center_axis',(1.77635683940025E-15,-1.,0.)) ;
#18279 = DIRECTION('ref_axis',(0.,0.,1.)) ;
#18280 = DIRECTION('',(1.77635683940025E-15,-1.,0.)) ;
#18281 = DIRECTION('center_axis',(3.5527136788005E-16,1.,0.)) ;
#18282 = DIRECTION('ref_axis',(0.,0.,1.)) ;
#18283 = DIRECTION('center_axis',(1.77635683940025E-15,-1.,0.)) ;
#18284 = DIRECTION('ref_axis',(0.,0.,1.)) ;
#18285 = DIRECTION('center_axis',(1.77635683940025E-15,-1.,0.)) ;
#18286 = DIRECTION('ref_axis',(0.,0.,1.)) ;
#18287 = DIRECTION('center_axis',(1.77635683940025E-15,-1.,0.)) ;
#18288 = DIRECTION('ref_axis',(0.,0.,1.)) ;
#18289 = DIRECTION('center_axis',(1.77635683940025E-15,-1.,0.)) ;
#18290 = DIRECTION('ref_axis',(0.,0.,1.)) ;
#18291 = DIRECTION('center_axis',(-4.2632564145606E-15,-1.,0.)) ;
#18292 = DIRECTION('ref_axis',(0.,0.,1.)) ;
#18293 = DIRECTION('',(1.77635683940025E-15,-1.,0.)) ;
#18294 = DIRECTION('center_axis',(1.77635683940025E-15,-1.,0.)) ;
#18295 = DIRECTION('ref_axis',(0.,0.,1.)) ;
#18296 = DIRECTION('',(1.77635683940025E-15,-1.,0.)) ;
#18297 = DIRECTION('center_axis',(3.5527136788005E-16,1.,0.)) ;
#18298 = DIRECTION('ref_axis',(0.,0.,1.)) ;
#18299 = DIRECTION('center_axis',(1.77635683940025E-15,-1.,0.)) ;
#18300 = DIRECTION('ref_axis',(0.,0.,1.)) ;
#18301 = DIRECTION('center_axis',(1.77635683940025E-15,-1.,0.)) ;
#18302 = DIRECTION('ref_axis',(0.,0.,1.)) ;
#18303 = DIRECTION('center_axis',(1.77635683940025E-15,-1.,0.)) ;
#18304 = DIRECTION('ref_axis',(0.,0.,1.)) ;
#18305 = DIRECTION('center_axis',(1.77635683940025E-15,-1.,0.)) ;
#18306 = DIRECTION('ref_axis',(0.,0.,1.)) ;
#18307 = DIRECTION('center_axis',(-4.2632564145606E-15,-1.,0.)) ;
#18308 = DIRECTION('ref_axis',(0.,0.,1.)) ;
#18309 = DIRECTION('',(1.77635683940025E-15,-1.,0.)) ;
#18310 = DIRECTION('center_axis',(1.77635683940025E-15,-1.,0.)) ;
#18311 = DIRECTION('ref_axis',(0.,0.,1.)) ;
#18312 = DIRECTION('',(1.77635683940025E-15,-1.,0.)) ;
#18313 = DIRECTION('center_axis',(3.5527136788005E-16,1.,0.)) ;
#18314 = DIRECTION('ref_axis',(0.,0.,1.)) ;
#18315 = DIRECTION('center_axis',(4.2632564145606E-15,1.,0.)) ;
#18316 = DIRECTION('ref_axis',(1.,-4.2632564145606E-15,0.)) ;
#18317 = DIRECTION('',(-1.,4.2632564145606E-15,0.)) ;
#18318 = DIRECTION('',(0.,0.,-1.)) ;
#18319 = DIRECTION('',(1.,-4.2632564145606E-15,0.)) ;
#18320 = DIRECTION('',(0.,0.,-1.)) ;
#18321 = DIRECTION('center_axis',(-1.,-7.10542735760106E-15,0.)) ;
#18322 = DIRECTION('ref_axis',(-7.10542735760106E-15,1.,0.)) ;
#18323 = DIRECTION('',(7.10542735760106E-15,-1.,0.)) ;
#18324 = DIRECTION('',(0.,0.,-1.)) ;
#18325 = DIRECTION('',(-7.10542735760106E-15,1.,0.)) ;
#18326 = DIRECTION('center_axis',(-3.5527136788005E-16,-1.,0.)) ;
#18327 = DIRECTION('ref_axis',(-1.,3.5527136788005E-16,0.)) ;
#18328 = DIRECTION('',(1.,-3.5527136788005E-16,0.)) ;
#18329 = DIRECTION('',(0.,0.,-1.)) ;
#18330 = DIRECTION('',(-1.,3.5527136788005E-16,0.)) ;
#18331 = DIRECTION('center_axis',(1.,8.88178419700168E-16,0.)) ;
#18332 = DIRECTION('ref_axis',(8.88178419700168E-16,-1.,0.)) ;
#18333 = DIRECTION('',(-8.88178419700168E-16,1.,0.)) ;
#18334 = DIRECTION('',(8.88178419700168E-16,-1.,0.)) ;
#18335 = DIRECTION('center_axis',(0.,0.,1.)) ;
#18336 = DIRECTION('ref_axis',(1.,0.,0.)) ;
#18337 = DIRECTION('center_axis',(0.,0.,-1.)) ;
#18338 = DIRECTION('ref_axis',(-1.,0.,0.)) ;
#18339 = DIRECTION('axis',(0.,0.,1.)) ;
#18340 = DIRECTION('refdir',(1.,0.,0.)) ;
#18341 = DIRECTION('center_axis',(-9.473903143468E-16,1.,0.)) ;
#18342 = DIRECTION('ref_axis',(0.,0.,1.)) ;
#18343 = DIRECTION('',(-5.92914802803472E-16,0.515038074910058,-0.85716730070211)) ;
#18344 = DIRECTION('center_axis',(9.473903143468E-16,-1.,0.)) ;
#18345 = DIRECTION('ref_axis',(0.,0.,1.)) ;
#18346 = DIRECTION('center_axis',(9.473903143468E-16,-1.,0.)) ;
#18347 = DIRECTION('ref_axis',(0.,0.,1.)) ;
#18348 = DIRECTION('center_axis',(9.47390314346801E-16,-1.,0.)) ;
#18349 = DIRECTION('ref_axis',(0.,0.,1.)) ;
#18350 = DIRECTION('',(9.473903143468E-16,-1.,0.)) ;
#18351 = DIRECTION('center_axis',(-9.473903143468E-16,1.,0.)) ;
#18352 = DIRECTION('ref_axis',(0.,0.,1.)) ;
#18353 = DIRECTION('',(-5.92914802803472E-16,0.515038074910058,-0.85716730070211)) ;
#18354 = DIRECTION('center_axis',(9.473903143468E-16,-1.,0.)) ;
#18355 = DIRECTION('ref_axis',(0.,0.,1.)) ;
#18356 = DIRECTION('center_axis',(9.473903143468E-16,-1.,0.)) ;
#18357 = DIRECTION('ref_axis',(0.,0.,1.)) ;
#18358 = DIRECTION('center_axis',(9.47390314346801E-16,-1.,0.)) ;
#18359 = DIRECTION('ref_axis',(0.,0.,1.)) ;
#18360 = DIRECTION('',(9.473903143468E-16,-1.,0.)) ;
#18361 = DIRECTION('center_axis',(-3.5527136788005E-16,-1.,0.)) ;
#18362 = DIRECTION('ref_axis',(0.,0.,-1.)) ;
#18363 = DIRECTION('',(-2.87951000497466E-16,-0.515038074910058,0.85716730070211)) ;
#18364 = DIRECTION('center_axis',(3.5527136788005E-16,1.,0.)) ;
#18365 = DIRECTION('ref_axis',(0.,0.,-1.)) ;
#18366 = DIRECTION('center_axis',(3.5527136788005E-16,1.,0.)) ;
#18367 = DIRECTION('ref_axis',(0.,0.,-1.)) ;
#18368 = DIRECTION('center_axis',(4.2632564145606E-15,1.,0.)) ;
#18369 = DIRECTION('ref_axis',(0.,0.,-1.)) ;
#18370 = DIRECTION('',(3.5527136788005E-16,1.,0.)) ;
#18371 = DIRECTION('center_axis',(-3.5527136788005E-16,-1.,0.)) ;
#18372 = DIRECTION('ref_axis',(0.,0.,-1.)) ;
#18373 = DIRECTION('',(-2.87951000497466E-16,-0.515038074910058,0.85716730070211)) ;
#18374 = DIRECTION('center_axis',(3.5527136788005E-16,1.,0.)) ;
#18375 = DIRECTION('ref_axis',(0.,0.,-1.)) ;
#18376 = DIRECTION('center_axis',(3.5527136788005E-16,1.,0.)) ;
#18377 = DIRECTION('ref_axis',(0.,0.,-1.)) ;
#18378 = DIRECTION('center_axis',(4.2632564145606E-15,1.,0.)) ;
#18379 = DIRECTION('ref_axis',(0.,0.,-1.)) ;
#18380 = DIRECTION('',(3.5527136788005E-16,1.,0.)) ;
#18381 = DIRECTION('center_axis',(0.,0.,-1.)) ;
#18382 = DIRECTION('ref_axis',(1.,0.,0.)) ;
#18383 = DIRECTION('',(-0.85716730070211,1.04972719113862E-16,-0.515038074910058)) ;
#18384 = DIRECTION('center_axis',(0.,0.,-1.)) ;
#18385 = DIRECTION('ref_axis',(1.,0.,0.)) ;
#18386 = DIRECTION('center_axis',(0.,0.,-1.)) ;
#18387 = DIRECTION('ref_axis',(1.,0.,0.)) ;
#18388 = DIRECTION('',(0.,0.,-1.)) ;
#18389 = DIRECTION('center_axis',(0.,0.,1.)) ;
#18390 = DIRECTION('ref_axis',(1.,0.,0.)) ;
#18391 = DIRECTION('center_axis',(0.,0.,-1.)) ;
#18392 = DIRECTION('ref_axis',(1.,0.,0.)) ;
#18393 = DIRECTION('',(-0.85716730070211,1.04972719113862E-16,-0.515038074910058)) ;
#18394 = DIRECTION('center_axis',(0.,0.,-1.)) ;
#18395 = DIRECTION('ref_axis',(1.,0.,0.)) ;
#18396 = DIRECTION('center_axis',(0.,0.,-1.)) ;
#18397 = DIRECTION('ref_axis',(1.,0.,0.)) ;
#18398 = DIRECTION('',(0.,0.,-1.)) ;
#18399 = DIRECTION('center_axis',(0.,0.,1.)) ;
#18400 = DIRECTION('ref_axis',(1.,0.,0.)) ;
#18401 = DIRECTION('center_axis',(0.,0.,-1.)) ;
#18402 = DIRECTION('ref_axis',(-1.,0.,0.)) ;
#18403 = DIRECTION('',(1.,-4.2632564145606E-15,0.)) ;
#18404 = DIRECTION('',(1.02140518265514E-15,-1.,0.)) ;
#18405 = DIRECTION('',(-1.,-9.47390314346801E-16,0.)) ;
#18406 = DIRECTION('',(2.66453525910036E-16,1.,0.)) ;
#18407 = DIRECTION('center_axis',(0.,0.,1.)) ;
#18408 = DIRECTION('ref_axis',(1.,0.,0.)) ;
#18409 = DIRECTION('',(-0.85716730070211,-1.04972719113862E-16,0.515038074910058)) ;
#18410 = DIRECTION('center_axis',(0.,0.,-1.)) ;
#18411 = DIRECTION('ref_axis',(1.,0.,0.)) ;
#18412 = DIRECTION('center_axis',(0.,0.,-1.)) ;
#18413 = DIRECTION('ref_axis',(1.,0.,0.)) ;
#18414 = DIRECTION('center_axis',(0.,0.,1.)) ;
#18415 = DIRECTION('ref_axis',(1.,0.,0.)) ;
#18416 = DIRECTION('',(0.,0.,-1.)) ;
#18417 = DIRECTION('center_axis',(0.,0.,1.)) ;
#18418 = DIRECTION('ref_axis',(1.,0.,0.)) ;
#18419 = DIRECTION('',(-0.85716730070211,-1.04972719113862E-16,0.515038074910058)) ;
#18420 = DIRECTION('center_axis',(0.,0.,-1.)) ;
#18421 = DIRECTION('ref_axis',(1.,0.,0.)) ;
#18422 = DIRECTION('center_axis',(0.,0.,-1.)) ;
#18423 = DIRECTION('ref_axis',(1.,0.,0.)) ;
#18424 = DIRECTION('center_axis',(0.,0.,1.)) ;
#18425 = DIRECTION('ref_axis',(1.,0.,0.)) ;
#18426 = DIRECTION('',(0.,0.,-1.)) ;
#18427 = DIRECTION('center_axis',(1.,-2.66453525910036E-16,0.)) ;
#18428 = DIRECTION('ref_axis',(-2.66453525910036E-16,-1.,0.)) ;
#18429 = DIRECTION('',(2.66453525910036E-16,1.,0.)) ;
#18430 = DIRECTION('',(0.,0.,-1.)) ;
#18431 = DIRECTION('',(0.,0.,-1.)) ;
#18432 = DIRECTION('center_axis',(-9.47390314346801E-16,1.,0.)) ;
#18433 = DIRECTION('ref_axis',(1.,9.47390314346801E-16,0.)) ;
#18434 = DIRECTION('',(-1.,-9.47390314346801E-16,0.)) ;
#18435 = DIRECTION('',(0.,0.,-1.)) ;
#18436 = DIRECTION('center_axis',(-1.,-1.02140518265514E-15,0.)) ;
#18437 = DIRECTION('ref_axis',(-1.02140518265514E-15,1.,0.)) ;
#18438 = DIRECTION('',(1.02140518265514E-15,-1.,0.)) ;
#18439 = DIRECTION('',(0.,0.,-1.)) ;
#18440 = DIRECTION('center_axis',(-4.2632564145606E-15,-1.,0.)) ;
#18441 = DIRECTION('ref_axis',(-1.,4.2632564145606E-15,0.)) ;
#18442 = DIRECTION('',(1.,-4.2632564145606E-15,0.)) ;
#18443 = DIRECTION('center_axis',(0.,0.,-1.)) ;
#18444 = DIRECTION('ref_axis',(-1.,0.,0.)) ;
#18445 = DIRECTION('axis',(0.,0.,1.)) ;
#18446 = DIRECTION('refdir',(1.,0.,0.)) ;
#18447 = DIRECTION('center_axis',(0.,0.,-1.)) ;
#18448 = DIRECTION('ref_axis',(-1.,0.,0.)) ;
#18449 = DIRECTION('',(0.85716730070211,-1.04972719113862E-16,-0.515038074910058)) ;
#18450 = DIRECTION('center_axis',(0.,0.,1.)) ;
#18451 = DIRECTION('ref_axis',(-1.,0.,0.)) ;
#18452 = DIRECTION('center_axis',(0.,0.,1.)) ;
#18453 = DIRECTION('ref_axis',(-1.,0.,0.)) ;
#18454 = DIRECTION('center_axis',(0.,0.,1.)) ;
#18455 = DIRECTION('ref_axis',(-1.,0.,0.)) ;
#18456 = DIRECTION('',(0.,0.,1.)) ;
#18457 = DIRECTION('center_axis',(0.,0.,-1.)) ;
#18458 = DIRECTION('ref_axis',(-1.,0.,0.)) ;
#18459 = DIRECTION('',(0.85716730070211,-1.04972719113862E-16,-0.515038074910058)) ;
#18460 = DIRECTION('center_axis',(0.,0.,1.)) ;
#18461 = DIRECTION('ref_axis',(-1.,0.,0.)) ;
#18462 = DIRECTION('center_axis',(0.,0.,1.)) ;
#18463 = DIRECTION('ref_axis',(-1.,0.,0.)) ;
#18464 = DIRECTION('center_axis',(0.,0.,1.)) ;
#18465 = DIRECTION('ref_axis',(-1.,0.,0.)) ;
#18466 = DIRECTION('',(0.,0.,1.)) ;
#18467 = DIRECTION('center_axis',(-9.473903143468E-16,1.,0.)) ;
#18468 = DIRECTION('ref_axis',(0.,0.,1.)) ;
#18469 = DIRECTION('',(-5.92914802803472E-16,0.515038074910058,-0.85716730070211)) ;
#18470 = DIRECTION('center_axis',(9.473903143468E-16,-1.,0.)) ;
#18471 = DIRECTION('ref_axis',(0.,0.,1.)) ;
#18472 = DIRECTION('center_axis',(9.473903143468E-16,-1.,0.)) ;
#18473 = DIRECTION('ref_axis',(0.,0.,1.)) ;
#18474 = DIRECTION('center_axis',(9.47390314346801E-16,-1.,0.)) ;
#18475 = DIRECTION('ref_axis',(0.,0.,1.)) ;
#18476 = DIRECTION('',(9.473903143468E-16,-1.,0.)) ;
#18477 = DIRECTION('center_axis',(-9.473903143468E-16,1.,0.)) ;
#18478 = DIRECTION('ref_axis',(0.,0.,1.)) ;
#18479 = DIRECTION('',(-5.92914802803472E-16,0.515038074910058,-0.85716730070211)) ;
#18480 = DIRECTION('center_axis',(9.473903143468E-16,-1.,0.)) ;
#18481 = DIRECTION('ref_axis',(0.,0.,1.)) ;
#18482 = DIRECTION('center_axis',(9.473903143468E-16,-1.,0.)) ;
#18483 = DIRECTION('ref_axis',(0.,0.,1.)) ;
#18484 = DIRECTION('center_axis',(9.47390314346801E-16,-1.,0.)) ;
#18485 = DIRECTION('ref_axis',(0.,0.,1.)) ;
#18486 = DIRECTION('',(9.473903143468E-16,-1.,0.)) ;
#18487 = DIRECTION('center_axis',(-3.5527136788005E-16,-1.,0.)) ;
#18488 = DIRECTION('ref_axis',(0.,0.,-1.)) ;
#18489 = DIRECTION('',(-2.87951000497466E-16,-0.515038074910058,0.85716730070211)) ;
#18490 = DIRECTION('center_axis',(3.5527136788005E-16,1.,0.)) ;
#18491 = DIRECTION('ref_axis',(0.,0.,-1.)) ;
#18492 = DIRECTION('center_axis',(3.5527136788005E-16,1.,0.)) ;
#18493 = DIRECTION('ref_axis',(0.,0.,-1.)) ;
#18494 = DIRECTION('center_axis',(4.2632564145606E-15,1.,0.)) ;
#18495 = DIRECTION('ref_axis',(0.,0.,-1.)) ;
#18496 = DIRECTION('',(3.5527136788005E-16,1.,0.)) ;
#18497 = DIRECTION('center_axis',(-3.5527136788005E-16,-1.,0.)) ;
#18498 = DIRECTION('ref_axis',(0.,0.,-1.)) ;
#18499 = DIRECTION('',(-2.87951000497466E-16,-0.515038074910058,0.85716730070211)) ;
#18500 = DIRECTION('center_axis',(3.5527136788005E-16,1.,0.)) ;
#18501 = DIRECTION('ref_axis',(0.,0.,-1.)) ;
#18502 = DIRECTION('center_axis',(3.5527136788005E-16,1.,0.)) ;
#18503 = DIRECTION('ref_axis',(0.,0.,-1.)) ;
#18504 = DIRECTION('center_axis',(4.2632564145606E-15,1.,0.)) ;
#18505 = DIRECTION('ref_axis',(0.,0.,-1.)) ;
#18506 = DIRECTION('',(3.5527136788005E-16,1.,0.)) ;
#18507 = DIRECTION('center_axis',(0.,0.,-1.)) ;
#18508 = DIRECTION('ref_axis',(1.,0.,0.)) ;
#18509 = DIRECTION('center_axis',(0.,0.,-1.)) ;
#18510 = DIRECTION('ref_axis',(1.,0.,0.)) ;
#18511 = DIRECTION('center_axis',(0.,0.,-1.)) ;
#18512 = DIRECTION('ref_axis',(1.,0.,0.)) ;
#18513 = DIRECTION('center_axis',(0.,0.,-1.)) ;
#18514 = DIRECTION('ref_axis',(1.,0.,0.)) ;
#18515 = DIRECTION('',(0.,0.,-1.)) ;
#18516 = DIRECTION('center_axis',(0.,0.,-1.)) ;
#18517 = DIRECTION('ref_axis',(1.,0.,0.)) ;
#18518 = DIRECTION('center_axis',(0.,0.,-1.)) ;
#18519 = DIRECTION('ref_axis',(1.,0.,0.)) ;
#18520 = DIRECTION('center_axis',(0.,0.,1.)) ;
#18521 = DIRECTION('ref_axis',(1.,0.,0.)) ;
#18522 = DIRECTION('',(0.,0.,-1.)) ;
#18523 = DIRECTION('center_axis',(0.,0.,-1.)) ;
#18524 = DIRECTION('ref_axis',(1.,0.,0.)) ;
#18525 = DIRECTION('center_axis',(0.,0.,-1.)) ;
#18526 = DIRECTION('ref_axis',(1.,0.,0.)) ;
#18527 = DIRECTION('center_axis',(0.,0.,-1.)) ;
#18528 = DIRECTION('ref_axis',(1.,0.,0.)) ;
#18529 = DIRECTION('center_axis',(0.,0.,-1.)) ;
#18530 = DIRECTION('ref_axis',(1.,0.,0.)) ;
#18531 = DIRECTION('',(0.,0.,-1.)) ;
#18532 = DIRECTION('center_axis',(0.,0.,-1.)) ;
#18533 = DIRECTION('ref_axis',(1.,0.,0.)) ;
#18534 = DIRECTION('center_axis',(0.,0.,-1.)) ;
#18535 = DIRECTION('ref_axis',(1.,0.,0.)) ;
#18536 = DIRECTION('center_axis',(0.,0.,1.)) ;
#18537 = DIRECTION('ref_axis',(1.,0.,0.)) ;
#18538 = DIRECTION('',(0.,0.,-1.)) ;
#18539 = DIRECTION('center_axis',(0.,0.,-1.)) ;
#18540 = DIRECTION('ref_axis',(1.,0.,0.)) ;
#18541 = DIRECTION('center_axis',(0.,0.,-1.)) ;
#18542 = DIRECTION('ref_axis',(1.,0.,0.)) ;
#18543 = DIRECTION('center_axis',(0.,0.,-1.)) ;
#18544 = DIRECTION('ref_axis',(1.,0.,0.)) ;
#18545 = DIRECTION('center_axis',(0.,0.,-1.)) ;
#18546 = DIRECTION('ref_axis',(1.,0.,0.)) ;
#18547 = DIRECTION('',(0.,0.,-1.)) ;
#18548 = DIRECTION('center_axis',(0.,0.,-1.)) ;
#18549 = DIRECTION('ref_axis',(1.,0.,0.)) ;
#18550 = DIRECTION('center_axis',(0.,0.,-1.)) ;
#18551 = DIRECTION('ref_axis',(1.,0.,0.)) ;
#18552 = DIRECTION('center_axis',(0.,0.,1.)) ;
#18553 = DIRECTION('ref_axis',(1.,0.,0.)) ;
#18554 = DIRECTION('',(0.,0.,-1.)) ;
#18555 = DIRECTION('center_axis',(0.,0.,-1.)) ;
#18556 = DIRECTION('ref_axis',(1.,0.,0.)) ;
#18557 = DIRECTION('center_axis',(0.,0.,-1.)) ;
#18558 = DIRECTION('ref_axis',(1.,0.,0.)) ;
#18559 = DIRECTION('center_axis',(0.,0.,-1.)) ;
#18560 = DIRECTION('ref_axis',(1.,0.,0.)) ;
#18561 = DIRECTION('center_axis',(0.,0.,-1.)) ;
#18562 = DIRECTION('ref_axis',(1.,0.,0.)) ;
#18563 = DIRECTION('',(0.,0.,-1.)) ;
#18564 = DIRECTION('center_axis',(0.,0.,-1.)) ;
#18565 = DIRECTION('ref_axis',(1.,0.,0.)) ;
#18566 = DIRECTION('center_axis',(0.,0.,-1.)) ;
#18567 = DIRECTION('ref_axis',(1.,0.,0.)) ;
#18568 = DIRECTION('center_axis',(0.,0.,1.)) ;
#18569 = DIRECTION('ref_axis',(1.,0.,0.)) ;
#18570 = DIRECTION('',(0.,0.,-1.)) ;
#18571 = DIRECTION('center_axis',(0.,0.,1.)) ;
#18572 = DIRECTION('ref_axis',(-1.,0.,0.)) ;
#18573 = DIRECTION('',(0.85716730070211,1.04972719113862E-16,0.515038074910058)) ;
#18574 = DIRECTION('center_axis',(0.,0.,1.)) ;
#18575 = DIRECTION('ref_axis',(-1.,0.,0.)) ;
#18576 = DIRECTION('center_axis',(0.,0.,1.)) ;
#18577 = DIRECTION('ref_axis',(-1.,0.,0.)) ;
#18578 = DIRECTION('',(0.,0.,1.)) ;
#18579 = DIRECTION('center_axis',(0.,0.,1.)) ;
#18580 = DIRECTION('ref_axis',(-1.,0.,0.)) ;
#18581 = DIRECTION('center_axis',(0.,0.,1.)) ;
#18582 = DIRECTION('ref_axis',(-1.,0.,0.)) ;
#18583 = DIRECTION('',(0.85716730070211,1.04972719113862E-16,0.515038074910058)) ;
#18584 = DIRECTION('center_axis',(0.,0.,1.)) ;
#18585 = DIRECTION('ref_axis',(-1.,0.,0.)) ;
#18586 = DIRECTION('center_axis',(0.,0.,1.)) ;
#18587 = DIRECTION('ref_axis',(-1.,0.,0.)) ;
#18588 = DIRECTION('',(0.,0.,1.)) ;
#18589 = DIRECTION('center_axis',(0.,0.,-1.)) ;
#18590 = DIRECTION('ref_axis',(-1.,0.,0.)) ;
#18591 = DIRECTION('center_axis',(0.,0.,1.)) ;
#18592 = DIRECTION('ref_axis',(-1.,0.,0.)) ;
#18593 = DIRECTION('',(0.85716730070211,1.04972719113862E-16,0.515038074910058)) ;
#18594 = DIRECTION('center_axis',(0.,0.,1.)) ;
#18595 = DIRECTION('ref_axis',(-1.,0.,0.)) ;
#18596 = DIRECTION('center_axis',(0.,0.,1.)) ;
#18597 = DIRECTION('ref_axis',(-1.,0.,0.)) ;
#18598 = DIRECTION('',(0.,0.,1.)) ;
#18599 = DIRECTION('center_axis',(0.,0.,-1.)) ;
#18600 = DIRECTION('ref_axis',(-1.,0.,0.)) ;
#18601 = DIRECTION('center_axis',(0.,0.,1.)) ;
#18602 = DIRECTION('ref_axis',(-1.,0.,0.)) ;
#18603 = DIRECTION('',(0.85716730070211,1.04972719113862E-16,0.515038074910058)) ;
#18604 = DIRECTION('center_axis',(0.,0.,1.)) ;
#18605 = DIRECTION('ref_axis',(-1.,0.,0.)) ;
#18606 = DIRECTION('center_axis',(0.,0.,1.)) ;
#18607 = DIRECTION('ref_axis',(-1.,0.,0.)) ;
#18608 = DIRECTION('',(0.,0.,1.)) ;
#18609 = DIRECTION('center_axis',(0.,0.,-1.)) ;
#18610 = DIRECTION('ref_axis',(-1.,0.,0.)) ;
#18611 = DIRECTION('center_axis',(0.,0.,1.)) ;
#18612 = DIRECTION('ref_axis',(-1.,0.,0.)) ;
#18613 = DIRECTION('',(0.85716730070211,1.04972719113862E-16,0.515038074910058)) ;
#18614 = DIRECTION('center_axis',(0.,0.,1.)) ;
#18615 = DIRECTION('ref_axis',(-1.,0.,0.)) ;
#18616 = DIRECTION('center_axis',(0.,0.,1.)) ;
#18617 = DIRECTION('ref_axis',(-1.,0.,0.)) ;
#18618 = DIRECTION('',(0.,0.,1.)) ;
#18619 = DIRECTION('center_axis',(0.,0.,-1.)) ;
#18620 = DIRECTION('ref_axis',(-1.,0.,0.)) ;
#18621 = DIRECTION('center_axis',(0.,0.,1.)) ;
#18622 = DIRECTION('ref_axis',(-1.,0.,0.)) ;
#18623 = DIRECTION('',(0.85716730070211,1.04972719113862E-16,0.515038074910058)) ;
#18624 = DIRECTION('center_axis',(0.,0.,1.)) ;
#18625 = DIRECTION('ref_axis',(-1.,0.,0.)) ;
#18626 = DIRECTION('center_axis',(0.,0.,1.)) ;
#18627 = DIRECTION('ref_axis',(-1.,0.,0.)) ;
#18628 = DIRECTION('',(0.,0.,1.)) ;
#18629 = DIRECTION('center_axis',(0.,0.,-1.)) ;
#18630 = DIRECTION('ref_axis',(-1.,0.,0.)) ;
#18631 = DIRECTION('center_axis',(0.,0.,1.)) ;
#18632 = DIRECTION('ref_axis',(-1.,0.,0.)) ;
#18633 = DIRECTION('',(0.85716730070211,1.04972719113862E-16,0.515038074910058)) ;
#18634 = DIRECTION('center_axis',(0.,0.,1.)) ;
#18635 = DIRECTION('ref_axis',(-1.,0.,0.)) ;
#18636 = DIRECTION('center_axis',(0.,0.,1.)) ;
#18637 = DIRECTION('ref_axis',(-1.,0.,0.)) ;
#18638 = DIRECTION('',(0.,0.,1.)) ;
#18639 = DIRECTION('center_axis',(0.,0.,-1.)) ;
#18640 = DIRECTION('ref_axis',(-1.,0.,0.)) ;
#18641 = DIRECTION('center_axis',(0.,0.,1.)) ;
#18642 = DIRECTION('ref_axis',(-1.,0.,0.)) ;
#18643 = DIRECTION('',(0.85716730070211,1.04972719113862E-16,0.515038074910058)) ;
#18644 = DIRECTION('center_axis',(0.,0.,1.)) ;
#18645 = DIRECTION('ref_axis',(-1.,0.,0.)) ;
#18646 = DIRECTION('center_axis',(0.,0.,1.)) ;
#18647 = DIRECTION('ref_axis',(-1.,0.,0.)) ;
#18648 = DIRECTION('',(0.,0.,1.)) ;
#18649 = DIRECTION('center_axis',(0.,0.,1.)) ;
#18650 = DIRECTION('ref_axis',(-1.,0.,0.)) ;
#18651 = DIRECTION('center_axis',(0.,0.,-1.)) ;
#18652 = DIRECTION('ref_axis',(1.,0.,0.)) ;
#18653 = DIRECTION('center_axis',(0.,0.,1.)) ;
#18654 = DIRECTION('ref_axis',(1.,0.,0.)) ;
#18655 = DIRECTION('',(0.,0.,-1.)) ;
#18656 = DIRECTION('center_axis',(0.,0.,-1.)) ;
#18657 = DIRECTION('ref_axis',(1.,0.,0.)) ;
#18658 = DIRECTION('center_axis',(4.2632564145606E-15,1.,0.)) ;
#18659 = DIRECTION('ref_axis',(-1.,4.2632564145606E-15,0.)) ;
#18660 = DIRECTION('',(1.,-4.2632564145606E-15,0.)) ;
#18661 = DIRECTION('',(0.,0.,1.)) ;
#18662 = DIRECTION('',(-1.,4.2632564145606E-15,0.)) ;
#18663 = DIRECTION('',(0.,0.,1.)) ;
#18664 = DIRECTION('center_axis',(-1.,2.66453525910036E-16,0.)) ;
#18665 = DIRECTION('ref_axis',(-2.66453525910036E-16,-1.,0.)) ;
#18666 = DIRECTION('',(2.66453525910036E-16,1.,0.)) ;
#18667 = DIRECTION('',(0.,0.,1.)) ;
#18668 = DIRECTION('',(-2.66453525910036E-16,-1.,0.)) ;
#18669 = DIRECTION('center_axis',(9.47390314346801E-16,-1.,0.)) ;
#18670 = DIRECTION('ref_axis',(1.,9.47390314346801E-16,0.)) ;
#18671 = DIRECTION('',(1.,9.47390314346801E-16,0.)) ;
#18672 = DIRECTION('',(0.,0.,1.)) ;
#18673 = DIRECTION('',(1.,9.47390314346801E-16,0.)) ;
#18674 = DIRECTION('center_axis',(1.,-1.68753899743024E-15,0.)) ;
#18675 = DIRECTION('ref_axis',(1.68753899743024E-15,1.,0.)) ;
#18676 = DIRECTION('',(-1.68753899743024E-15,-1.,0.)) ;
#18677 = DIRECTION('',(1.68753899743024E-15,1.,0.)) ;
#18678 = DIRECTION('center_axis',(0.,0.,1.)) ;
#18679 = DIRECTION('ref_axis',(1.,0.,0.)) ;
#18680 = DIRECTION('center_axis',(0.,0.,1.)) ;
#18681 = DIRECTION('ref_axis',(1.,0.,0.)) ;
#18682 = DIRECTION('axis',(0.,0.,1.)) ;
#18683 = DIRECTION('refdir',(1.,0.,0.)) ;
#18684 = DIRECTION('center_axis',(9.473903143468E-16,1.,0.)) ;
#18685 = DIRECTION('ref_axis',(0.,0.,-1.)) ;
#18686 = DIRECTION('',(5.92914802803472E-16,0.515038074910058,0.85716730070211)) ;
#18687 = DIRECTION('center_axis',(-9.473903143468E-16,-1.,0.)) ;
#18688 = DIRECTION('ref_axis',(0.,0.,-1.)) ;
#18689 = DIRECTION('center_axis',(-9.473903143468E-16,-1.,0.)) ;
#18690 = DIRECTION('ref_axis',(0.,0.,-1.)) ;
#18691 = DIRECTION('center_axis',(9.47390314346801E-16,-1.,0.)) ;
#18692 = DIRECTION('ref_axis',(0.,0.,-1.)) ;
#18693 = DIRECTION('',(-9.473903143468E-16,-1.,0.)) ;
#18694 = DIRECTION('center_axis',(9.473903143468E-16,1.,0.)) ;
#18695 = DIRECTION('ref_axis',(0.,0.,-1.)) ;
#18696 = DIRECTION('',(5.92914802803472E-16,0.515038074910058,0.85716730070211)) ;
#18697 = DIRECTION('center_axis',(-9.473903143468E-16,-1.,0.)) ;
#18698 = DIRECTION('ref_axis',(0.,0.,-1.)) ;
#18699 = DIRECTION('center_axis',(-9.473903143468E-16,-1.,0.)) ;
#18700 = DIRECTION('ref_axis',(0.,0.,-1.)) ;
#18701 = DIRECTION('center_axis',(9.47390314346801E-16,-1.,0.)) ;
#18702 = DIRECTION('ref_axis',(0.,0.,-1.)) ;
#18703 = DIRECTION('',(-9.473903143468E-16,-1.,0.)) ;
#18704 = DIRECTION('center_axis',(3.5527136788005E-16,-1.,0.)) ;
#18705 = DIRECTION('ref_axis',(0.,0.,1.)) ;
#18706 = DIRECTION('',(2.87951000497466E-16,-0.515038074910058,-0.85716730070211)) ;
#18707 = DIRECTION('center_axis',(-3.5527136788005E-16,1.,0.)) ;
#18708 = DIRECTION('ref_axis',(0.,0.,1.)) ;
#18709 = DIRECTION('center_axis',(-3.5527136788005E-16,1.,0.)) ;
#18710 = DIRECTION('ref_axis',(0.,0.,1.)) ;
#18711 = DIRECTION('center_axis',(4.2632564145606E-15,1.,0.)) ;
#18712 = DIRECTION('ref_axis',(0.,0.,1.)) ;
#18713 = DIRECTION('',(-3.5527136788005E-16,1.,0.)) ;
#18714 = DIRECTION('center_axis',(3.5527136788005E-16,-1.,0.)) ;
#18715 = DIRECTION('ref_axis',(0.,0.,1.)) ;
#18716 = DIRECTION('',(2.87951000497466E-16,-0.515038074910058,-0.85716730070211)) ;
#18717 = DIRECTION('center_axis',(-3.5527136788005E-16,1.,0.)) ;
#18718 = DIRECTION('ref_axis',(0.,0.,1.)) ;
#18719 = DIRECTION('center_axis',(-3.5527136788005E-16,1.,0.)) ;
#18720 = DIRECTION('ref_axis',(0.,0.,1.)) ;
#18721 = DIRECTION('center_axis',(4.2632564145606E-15,1.,0.)) ;
#18722 = DIRECTION('ref_axis',(0.,0.,1.)) ;
#18723 = DIRECTION('',(-3.5527136788005E-16,1.,0.)) ;
#18724 = DIRECTION('center_axis',(0.,0.,1.)) ;
#18725 = DIRECTION('ref_axis',(1.,0.,0.)) ;
#18726 = DIRECTION('',(-0.85716730070211,-1.04972719113862E-16,0.515038074910058)) ;
#18727 = DIRECTION('center_axis',(0.,0.,-1.)) ;
#18728 = DIRECTION('ref_axis',(1.,0.,0.)) ;
#18729 = DIRECTION('center_axis',(0.,0.,-1.)) ;
#18730 = DIRECTION('ref_axis',(1.,0.,0.)) ;
#18731 = DIRECTION('center_axis',(0.,0.,1.)) ;
#18732 = DIRECTION('ref_axis',(1.,0.,0.)) ;
#18733 = DIRECTION('',(0.,0.,-1.)) ;
#18734 = DIRECTION('center_axis',(0.,0.,1.)) ;
#18735 = DIRECTION('ref_axis',(1.,0.,0.)) ;
#18736 = DIRECTION('',(-0.85716730070211,-1.04972719113862E-16,0.515038074910058)) ;
#18737 = DIRECTION('center_axis',(0.,0.,-1.)) ;
#18738 = DIRECTION('ref_axis',(1.,0.,0.)) ;
#18739 = DIRECTION('center_axis',(0.,0.,-1.)) ;
#18740 = DIRECTION('ref_axis',(1.,0.,0.)) ;
#18741 = DIRECTION('center_axis',(0.,0.,1.)) ;
#18742 = DIRECTION('ref_axis',(1.,0.,0.)) ;
#18743 = DIRECTION('',(0.,0.,-1.)) ;
#18744 = DIRECTION('center_axis',(0.,0.,-1.)) ;
#18745 = DIRECTION('ref_axis',(-1.,0.,0.)) ;
#18746 = DIRECTION('',(1.,-4.2632564145606E-15,0.)) ;
#18747 = DIRECTION('',(2.66453525910036E-16,1.,0.)) ;
#18748 = DIRECTION('',(-1.,-9.47390314346801E-16,0.)) ;
#18749 = DIRECTION('',(1.02140518265514E-15,-1.,0.)) ;
#18750 = DIRECTION('center_axis',(0.,0.,-1.)) ;
#18751 = DIRECTION('ref_axis',(1.,0.,0.)) ;
#18752 = DIRECTION('',(-0.85716730070211,1.04972719113862E-16,-0.515038074910058)) ;
#18753 = DIRECTION('center_axis',(0.,0.,-1.)) ;
#18754 = DIRECTION('ref_axis',(1.,0.,0.)) ;
#18755 = DIRECTION('center_axis',(0.,0.,-1.)) ;
#18756 = DIRECTION('ref_axis',(1.,0.,0.)) ;
#18757 = DIRECTION('',(0.,0.,-1.)) ;
#18758 = DIRECTION('center_axis',(0.,0.,1.)) ;
#18759 = DIRECTION('ref_axis',(1.,0.,0.)) ;
#18760 = DIRECTION('center_axis',(0.,0.,-1.)) ;
#18761 = DIRECTION('ref_axis',(1.,0.,0.)) ;
#18762 = DIRECTION('',(-0.85716730070211,1.04972719113862E-16,-0.515038074910058)) ;
#18763 = DIRECTION('center_axis',(0.,0.,-1.)) ;
#18764 = DIRECTION('ref_axis',(1.,0.,0.)) ;
#18765 = DIRECTION('center_axis',(0.,0.,-1.)) ;
#18766 = DIRECTION('ref_axis',(1.,0.,0.)) ;
#18767 = DIRECTION('',(0.,0.,-1.)) ;
#18768 = DIRECTION('center_axis',(0.,0.,1.)) ;
#18769 = DIRECTION('ref_axis',(1.,0.,0.)) ;
#18770 = DIRECTION('center_axis',(-1.,2.66453525910036E-16,0.)) ;
#18771 = DIRECTION('ref_axis',(-2.66453525910036E-16,-1.,0.)) ;
#18772 = DIRECTION('',(2.66453525910036E-16,1.,0.)) ;
#18773 = DIRECTION('',(0.,0.,1.)) ;
#18774 = DIRECTION('',(0.,0.,1.)) ;
#18775 = DIRECTION('center_axis',(9.47390314346801E-16,-1.,0.)) ;
#18776 = DIRECTION('ref_axis',(1.,9.47390314346801E-16,0.)) ;
#18777 = DIRECTION('',(-1.,-9.47390314346801E-16,0.)) ;
#18778 = DIRECTION('',(0.,0.,1.)) ;
#18779 = DIRECTION('center_axis',(1.,1.02140518265514E-15,0.)) ;
#18780 = DIRECTION('ref_axis',(-1.02140518265514E-15,1.,0.)) ;
#18781 = DIRECTION('',(1.02140518265514E-15,-1.,0.)) ;
#18782 = DIRECTION('',(0.,0.,1.)) ;
#18783 = DIRECTION('center_axis',(4.2632564145606E-15,1.,0.)) ;
#18784 = DIRECTION('ref_axis',(-1.,4.2632564145606E-15,0.)) ;
#18785 = DIRECTION('',(1.,-4.2632564145606E-15,0.)) ;
#18786 = DIRECTION('center_axis',(0.,0.,-1.)) ;
#18787 = DIRECTION('ref_axis',(-1.,0.,0.)) ;
#18788 = DIRECTION('axis',(0.,0.,1.)) ;
#18789 = DIRECTION('refdir',(1.,0.,0.)) ;
#18790 = DIRECTION('center_axis',(0.,0.,-1.)) ;
#18791 = DIRECTION('ref_axis',(0.,1.,0.)) ;
#18792 = DIRECTION('',(0.,0.,1.)) ;
#18793 = DIRECTION('center_axis',(0.,0.,-1.)) ;
#18794 = DIRECTION('ref_axis',(0.,1.,0.)) ;
#18795 = DIRECTION('center_axis',(0.,0.,-1.)) ;
#18796 = DIRECTION('ref_axis',(0.,1.,0.)) ;
#18797 = DIRECTION('',(0.,0.,1.)) ;
#18798 = DIRECTION('center_axis',(0.,0.,-1.)) ;
#18799 = DIRECTION('ref_axis',(0.,1.,0.)) ;
#18800 = DIRECTION('',(0.,0.,1.)) ;
#18801 = DIRECTION('center_axis',(0.,0.,-1.)) ;
#18802 = DIRECTION('ref_axis',(0.,1.,0.)) ;
#18803 = DIRECTION('',(0.,0.,1.)) ;
#18804 = DIRECTION('center_axis',(0.,0.,-1.)) ;
#18805 = DIRECTION('ref_axis',(0.,1.,0.)) ;
#18806 = DIRECTION('',(0.,0.,1.)) ;
#18807 = DIRECTION('center_axis',(0.,0.,-1.)) ;
#18808 = DIRECTION('ref_axis',(0.,1.,0.)) ;
#18809 = DIRECTION('',(0.,0.,1.)) ;
#18810 = DIRECTION('center_axis',(0.,0.,-1.)) ;
#18811 = DIRECTION('ref_axis',(0.,1.,0.)) ;
#18812 = DIRECTION('',(0.,0.,1.)) ;
#18813 = DIRECTION('center_axis',(0.,0.,-1.)) ;
#18814 = DIRECTION('ref_axis',(0.,1.,0.)) ;
#18815 = DIRECTION('',(0.,0.,1.)) ;
#18816 = DIRECTION('center_axis',(0.,0.,-1.)) ;
#18817 = DIRECTION('ref_axis',(0.,1.,0.)) ;
#18818 = DIRECTION('',(0.,0.,1.)) ;
#18819 = DIRECTION('center_axis',(0.,0.,-1.)) ;
#18820 = DIRECTION('ref_axis',(0.,1.,0.)) ;
#18821 = DIRECTION('',(0.,0.,1.)) ;
#18822 = DIRECTION('center_axis',(0.,0.,-1.)) ;
#18823 = DIRECTION('ref_axis',(0.,1.,0.)) ;
#18824 = DIRECTION('',(0.,0.,1.)) ;
#18825 = DIRECTION('center_axis',(0.,0.,-1.)) ;
#18826 = DIRECTION('ref_axis',(0.,1.,0.)) ;
#18827 = DIRECTION('',(0.,0.,1.)) ;
#18828 = DIRECTION('center_axis',(0.,0.,-1.)) ;
#18829 = DIRECTION('ref_axis',(0.,1.,0.)) ;
#18830 = DIRECTION('',(0.,0.,1.)) ;
#18831 = DIRECTION('center_axis',(0.,0.,-1.)) ;
#18832 = DIRECTION('ref_axis',(0.849891577299213,-0.526957594912394,0.)) ;
#18833 = DIRECTION('',(0.,0.,1.)) ;
#18834 = DIRECTION('center_axis',(0.,0.,-1.)) ;
#18835 = DIRECTION('ref_axis',(0.,1.,0.)) ;
#18836 = DIRECTION('center_axis',(0.,0.,-1.)) ;
#18837 = DIRECTION('ref_axis',(0.,1.,0.)) ;
#18838 = DIRECTION('',(0.,0.,1.)) ;
#18839 = DIRECTION('center_axis',(0.,0.,-1.)) ;
#18840 = DIRECTION('ref_axis',(0.,1.,0.)) ;
#18841 = DIRECTION('',(0.,0.,1.)) ;
#18842 = DIRECTION('center_axis',(0.,0.,-1.)) ;
#18843 = DIRECTION('ref_axis',(0.,1.,0.)) ;
#18844 = DIRECTION('',(0.,0.,1.)) ;
#18845 = DIRECTION('center_axis',(0.,0.,-1.)) ;
#18846 = DIRECTION('ref_axis',(0.,1.,0.)) ;
#18847 = DIRECTION('',(0.,0.,1.)) ;
#18848 = DIRECTION('center_axis',(0.,0.,-1.)) ;
#18849 = DIRECTION('ref_axis',(0.,1.,0.)) ;
#18850 = DIRECTION('',(0.,0.,1.)) ;
#18851 = DIRECTION('center_axis',(0.,0.,-1.)) ;
#18852 = DIRECTION('ref_axis',(0.,1.,0.)) ;
#18853 = DIRECTION('',(0.,0.,1.)) ;
#18854 = DIRECTION('center_axis',(0.,0.,1.)) ;
#18855 = DIRECTION('ref_axis',(0.,1.,0.)) ;
#18856 = DIRECTION('center_axis',(0.,0.,-1.)) ;
#18857 = DIRECTION('ref_axis',(-0.891629331176974,0.45276609389938,0.)) ;
#18858 = DIRECTION('',(0.,0.,1.)) ;
#18859 = DIRECTION('center_axis',(0.,0.,1.)) ;
#18860 = DIRECTION('ref_axis',(1.95976813240396E-14,1.,0.)) ;
#18861 = DIRECTION('center_axis',(0.,0.,-1.)) ;
#18862 = DIRECTION('ref_axis',(-0.891629331176974,0.45276609389938,0.)) ;
#18863 = DIRECTION('',(0.,0.,1.)) ;
#18864 = DIRECTION('center_axis',(0.,0.,-1.)) ;
#18865 = DIRECTION('ref_axis',(-0.891629331176974,0.45276609389938,0.)) ;
#18866 = DIRECTION('',(0.,0.,1.)) ;
#18867 = DIRECTION('center_axis',(0.,0.,-1.)) ;
#18868 = DIRECTION('ref_axis',(-0.891629331176974,0.45276609389938,0.)) ;
#18869 = DIRECTION('',(0.,0.,1.)) ;
#18870 = DIRECTION('center_axis',(0.,0.,-1.)) ;
#18871 = DIRECTION('ref_axis',(-0.891629331176974,0.45276609389938,0.)) ;
#18872 = DIRECTION('',(0.,0.,1.)) ;
#18873 = DIRECTION('center_axis',(0.,0.,-1.)) ;
#18874 = DIRECTION('ref_axis',(-0.891629331176974,0.45276609389938,0.)) ;
#18875 = DIRECTION('',(0.,0.,1.)) ;
#18876 = DIRECTION('center_axis',(0.,0.,-1.)) ;
#18877 = DIRECTION('ref_axis',(-0.998852985909418,0.04788227793077,0.)) ;
#18878 = DIRECTION('',(0.,0.,1.)) ;
#18879 = DIRECTION('center_axis',(0.,0.,1.)) ;
#18880 = DIRECTION('ref_axis',(7.83153288810636E-14,1.,0.)) ;
#18881 = DIRECTION('center_axis',(0.,0.,-1.)) ;
#18882 = DIRECTION('ref_axis',(-0.998852985909418,0.04788227793077,0.)) ;
#18883 = DIRECTION('',(0.,0.,1.)) ;
#18884 = DIRECTION('center_axis',(0.,0.,-1.)) ;
#18885 = DIRECTION('ref_axis',(-0.998852985909418,0.04788227793077,0.)) ;
#18886 = DIRECTION('',(0.,0.,1.)) ;
#18887 = DIRECTION('center_axis',(0.,0.,-1.)) ;
#18888 = DIRECTION('ref_axis',(-0.998852985909418,0.04788227793077,0.)) ;
#18889 = DIRECTION('',(0.,0.,1.)) ;
#18890 = DIRECTION('center_axis',(0.,0.,-1.)) ;
#18891 = DIRECTION('ref_axis',(-0.998852985909418,0.04788227793077,0.)) ;
#18892 = DIRECTION('',(0.,0.,1.)) ;
#18893 = DIRECTION('center_axis',(0.,0.,-1.)) ;
#18894 = DIRECTION('ref_axis',(-0.998852985909418,0.04788227793077,0.)) ;
#18895 = DIRECTION('',(0.,0.,1.)) ;
#18896 = DIRECTION('center_axis',(0.,0.,-1.)) ;
#18897 = DIRECTION('ref_axis',(-0.998852985909418,0.04788227793077,0.)) ;
#18898 = DIRECTION('',(0.,0.,1.)) ;
#18899 = DIRECTION('center_axis',(0.,0.,-1.)) ;
#18900 = DIRECTION('ref_axis',(-0.998852985909418,0.04788227793077,0.)) ;
#18901 = DIRECTION('',(0.,0.,1.)) ;
#18902 = DIRECTION('center_axis',(0.,0.,-1.)) ;
#18903 = DIRECTION('ref_axis',(-0.998852985909418,0.04788227793077,0.)) ;
#18904 = DIRECTION('',(0.,0.,1.)) ;
#18905 = DIRECTION('center_axis',(0.,0.,-1.)) ;
#18906 = DIRECTION('ref_axis',(-0.998852985909418,0.04788227793077,0.)) ;
#18907 = DIRECTION('',(0.,0.,1.)) ;
#18908 = DIRECTION('center_axis',(0.,0.,-1.)) ;
#18909 = DIRECTION('ref_axis',(-0.998852985909418,0.04788227793077,0.)) ;
#18910 = DIRECTION('',(0.,0.,1.)) ;
#18911 = DIRECTION('center_axis',(0.,0.,-1.)) ;
#18912 = DIRECTION('ref_axis',(-0.998852985909418,0.04788227793077,0.)) ;
#18913 = DIRECTION('',(0.,0.,1.)) ;
#18914 = DIRECTION('center_axis',(0.,0.,-1.)) ;
#18915 = DIRECTION('ref_axis',(-0.998852985909418,0.04788227793077,0.)) ;
#18916 = DIRECTION('',(0.,0.,1.)) ;
#18917 = DIRECTION('center_axis',(0.,0.,-1.)) ;
#18918 = DIRECTION('ref_axis',(-0.998852985909418,0.04788227793077,0.)) ;
#18919 = DIRECTION('center_axis',(0.,0.,-1.)) ;
#18920 = DIRECTION('ref_axis',(7.83153288810636E-14,1.,0.)) ;
#18921 = DIRECTION('center_axis',(0.,0.,-1.)) ;
#18922 = DIRECTION('ref_axis',(-0.891629331176974,0.45276609389938,0.)) ;
#18923 = DIRECTION('center_axis',(0.,0.,-1.)) ;
#18924 = DIRECTION('ref_axis',(1.95976813240396E-14,1.,0.)) ;
#18925 = DIRECTION('center_axis',(0.,0.,-1.)) ;
#18926 = DIRECTION('ref_axis',(0.,1.,0.)) ;
#18927 = DIRECTION('center_axis',(0.,0.,1.)) ;
#18928 = DIRECTION('ref_axis',(0.,1.,0.)) ;
#18929 = DIRECTION('center_axis',(0.,0.,-1.)) ;
#18930 = DIRECTION('ref_axis',(0.,1.,0.)) ;
#18931 = DIRECTION('center_axis',(0.,0.,1.)) ;
#18932 = DIRECTION('ref_axis',(0.,1.,0.)) ;
#18933 = DIRECTION('center_axis',(0.,0.,-1.)) ;
#18934 = DIRECTION('ref_axis',(0.,-1.,0.)) ;
#18935 = DIRECTION('center_axis',(0.,0.,1.)) ;
#18936 = DIRECTION('ref_axis',(0.,-1.,0.)) ;
#18937 = DIRECTION('',(8.65956056235593E-17,0.707106781186629,-0.707106781186466)) ;
#18938 = DIRECTION('center_axis',(0.,0.,-1.)) ;
#18939 = DIRECTION('ref_axis',(0.,-1.,0.)) ;
#18940 = DIRECTION('center_axis',(0.,0.,1.)) ;
#18941 = DIRECTION('ref_axis',(0.,-1.,0.)) ;
#18942 = DIRECTION('center_axis',(0.,0.,-1.)) ;
#18943 = DIRECTION('ref_axis',(-1.,0.,0.)) ;
#18944 = DIRECTION('center_axis',(0.,0.,1.)) ;
#18945 = DIRECTION('ref_axis',(0.,-1.,0.)) ;
#18946 = DIRECTION('center_axis',(0.,0.,-1.)) ;
#18947 = DIRECTION('ref_axis',(0.,1.,0.)) ;
#18948 = DIRECTION('center_axis',(0.,0.,-1.)) ;
#18949 = DIRECTION('ref_axis',(1.,0.,0.)) ;
#18950 = DIRECTION('',(0.,0.,-1.)) ;
#18951 = DIRECTION('center_axis',(0.,0.,1.)) ;
#18952 = DIRECTION('ref_axis',(0.,-1.,0.)) ;
#18953 = DIRECTION('center_axis',(0.,0.,-1.)) ;
#18954 = DIRECTION('ref_axis',(0.,-1.,0.)) ;
#18955 = DIRECTION('',(8.65956056235278E-17,-0.707106781186371,-0.707106781186724)) ;
#18956 = DIRECTION('center_axis',(0.,0.,-1.)) ;
#18957 = DIRECTION('ref_axis',(0.,-1.,0.)) ;
#18958 = DIRECTION('center_axis',(0.,0.,-1.)) ;
#18959 = DIRECTION('ref_axis',(0.,1.,0.)) ;
#18960 = DIRECTION('',(0.,0.,1.)) ;
#18961 = DIRECTION('center_axis',(0.,0.,-1.)) ;
#18962 = DIRECTION('ref_axis',(1.,0.,0.)) ;
#18963 = DIRECTION('center_axis',(0.,0.,1.)) ;
#18964 = DIRECTION('ref_axis',(0.,-1.,0.)) ;
#18965 = DIRECTION('center_axis',(0.,0.,-1.)) ;
#18966 = DIRECTION('ref_axis',(0.,-1.,0.)) ;
#18967 = DIRECTION('',(8.65956056235716E-17,-0.70710678118673,-0.707106781186365)) ;
#18968 = DIRECTION('center_axis',(0.,0.,1.)) ;
#18969 = DIRECTION('ref_axis',(0.,-1.,0.)) ;
#18970 = DIRECTION('center_axis',(0.,0.,-1.)) ;
#18971 = DIRECTION('ref_axis',(0.,-1.,0.)) ;
#18972 = DIRECTION('center_axis',(0.,0.,-1.)) ;
#18973 = DIRECTION('ref_axis',(0.,1.,0.)) ;
#18974 = DIRECTION('',(0.,0.,1.)) ;
#18975 = DIRECTION('center_axis',(0.,0.,-1.)) ;
#18976 = DIRECTION('ref_axis',(1.,0.,0.)) ;
#18977 = DIRECTION('',(0.,0.,1.)) ;
#18978 = DIRECTION('',(0.,0.,-1.)) ;
#18979 = DIRECTION('center_axis',(0.,0.,-1.)) ;
#18980 = DIRECTION('ref_axis',(-1.,0.,0.)) ;
#18981 = DIRECTION('center_axis',(0.,0.,-1.)) ;
#18982 = DIRECTION('ref_axis',(1.,0.,0.)) ;
#18983 = DIRECTION('center_axis',(0.,0.,1.)) ;
#18984 = DIRECTION('ref_axis',(0.,-1.,0.)) ;
#18985 = DIRECTION('center_axis',(0.,0.,-1.)) ;
#18986 = DIRECTION('ref_axis',(0.,-1.,0.)) ;
#18987 = DIRECTION('',(8.65956056235524E-17,-0.707106781186573,-0.707106781186522)) ;
#18988 = DIRECTION('center_axis',(0.,0.,1.)) ;
#18989 = DIRECTION('ref_axis',(0.,-1.,0.)) ;
#18990 = DIRECTION('center_axis',(0.,0.,-1.)) ;
#18991 = DIRECTION('ref_axis',(0.,-1.,0.)) ;
#18992 = DIRECTION('center_axis',(0.,0.,-1.)) ;
#18993 = DIRECTION('ref_axis',(0.,1.,0.)) ;
#18994 = DIRECTION('',(0.,0.,1.)) ;
#18995 = DIRECTION('center_axis',(0.,0.,-1.)) ;
#18996 = DIRECTION('ref_axis',(1.,0.,0.)) ;
#18997 = DIRECTION('center_axis',(0.,0.,-1.)) ;
#18998 = DIRECTION('ref_axis',(-1.,0.,0.)) ;
#18999 = DIRECTION('center_axis',(6.07670133222886E-15,0.,1.)) ;
#19000 = DIRECTION('ref_axis',(-3.05083907927506E-17,-1.,1.85390378974466E-31)) ;
#19001 = DIRECTION('center_axis',(0.,0.,-1.)) ;
#19002 = DIRECTION('ref_axis',(0.,-1.,0.)) ;
#19003 = DIRECTION('',(-4.92266285732438E-15,-0.57411334821253,-0.818775832205738)) ;
#19004 = DIRECTION('center_axis',(0.,0.,1.)) ;
#19005 = DIRECTION('ref_axis',(-6.12323399573677E-17,-1.,0.)) ;
#19006 = DIRECTION('center_axis',(0.,0.,1.)) ;
#19007 = DIRECTION('ref_axis',(-6.12323399573677E-17,-1.,0.)) ;
#19008 = DIRECTION('center_axis',(0.,0.,-1.)) ;
#19009 = DIRECTION('ref_axis',(0.,-1.,0.)) ;
#19010 = DIRECTION('center_axis',(0.,0.,-1.)) ;
#19011 = DIRECTION('ref_axis',(0.,1.,0.)) ;
#19012 = DIRECTION('',(0.,0.,1.)) ;
#19013 = DIRECTION('center_axis',(0.,0.,1.)) ;
#19014 = DIRECTION('ref_axis',(0.,-1.,0.)) ;
#19015 = DIRECTION('center_axis',(0.,0.,1.)) ;
#19016 = DIRECTION('ref_axis',(0.,-1.,0.)) ;
#19017 = DIRECTION('center_axis',(0.,0.,1.)) ;
#19018 = DIRECTION('ref_axis',(0.,1.,0.)) ;
#19019 = DIRECTION('',(-1.15133977109009E-16,0.940140268926269,-0.340787726808409)) ;
#19020 = DIRECTION('center_axis',(0.,0.,-1.)) ;
#19021 = DIRECTION('ref_axis',(1.,0.,0.)) ;
#19022 = DIRECTION('center_axis',(0.,0.,-1.)) ;
#19023 = DIRECTION('ref_axis',(0.,-1.,0.)) ;
#19024 = DIRECTION('',(-8.65956056235493E-17,-0.707106781186547,0.707106781186548)) ;
#19025 = DIRECTION('center_axis',(0.,0.,-1.)) ;
#19026 = DIRECTION('ref_axis',(0.,-1.,0.)) ;
#19027 = DIRECTION('center_axis',(0.,0.,1.)) ;
#19028 = DIRECTION('ref_axis',(1.,0.,0.)) ;
#19029 = DIRECTION('center_axis',(0.,0.,-1.)) ;
#19030 = DIRECTION('ref_axis',(1.,0.,0.)) ;
#19031 = DIRECTION('center_axis',(3.82880846191654E-15,0.,1.)) ;
#19032 = DIRECTION('ref_axis',(-3.03672668314921E-17,-1.,1.16270448209694E-31)) ;
#19033 = DIRECTION('center_axis',(0.,0.,-1.)) ;
#19034 = DIRECTION('ref_axis',(-6.12323399573677E-17,-1.,0.)) ;
#19035 = DIRECTION('',(2.60778271056638E-15,0.715792877193627,0.698312649863132)) ;
#19036 = DIRECTION('center_axis',(0.,0.,1.)) ;
#19037 = DIRECTION('ref_axis',(0.,-1.,0.)) ;
#19038 = DIRECTION('center_axis',(0.,0.,-1.)) ;
#19039 = DIRECTION('ref_axis',(-6.12323399573677E-17,-1.,0.)) ;
#19040 = DIRECTION('center_axis',(0.,0.,1.)) ;
#19041 = DIRECTION('ref_axis',(0.,1.,0.)) ;
#19042 = DIRECTION('',(3.02719047191673E-18,-0.0247188860822922,0.999694441652473)) ;
#19043 = DIRECTION('center_axis',(0.,0.,1.)) ;
#19044 = DIRECTION('ref_axis',(1.,0.,0.)) ;
#19045 = DIRECTION('center_axis',(0.,0.,1.)) ;
#19046 = DIRECTION('ref_axis',(0.,-1.,0.)) ;
#19047 = DIRECTION('center_axis',(0.,0.,-1.)) ;
#19048 = DIRECTION('ref_axis',(0.,-1.,0.)) ;
#19049 = DIRECTION('',(8.65956056235485E-17,-0.707106781186541,-0.707106781186554)) ;
#19050 = DIRECTION('center_axis',(0.,0.,1.)) ;
#19051 = DIRECTION('ref_axis',(0.,-1.,0.)) ;
#19052 = DIRECTION('center_axis',(0.,0.,-1.)) ;
#19053 = DIRECTION('ref_axis',(0.,-1.,0.)) ;
#19054 = DIRECTION('center_axis',(0.,0.,-1.)) ;
#19055 = DIRECTION('ref_axis',(0.,1.,0.)) ;
#19056 = DIRECTION('',(0.,0.,1.)) ;
#19057 = DIRECTION('center_axis',(0.,0.,1.)) ;
#19058 = DIRECTION('ref_axis',(0.,-1.,0.)) ;
#19059 = DIRECTION('center_axis',(0.,0.,1.)) ;
#19060 = DIRECTION('ref_axis',(0.,-1.,0.)) ;
#19061 = DIRECTION('center_axis',(0.,0.,-1.)) ;
#19062 = DIRECTION('ref_axis',(-1.,0.,0.)) ;
#19063 = DIRECTION('center_axis',(0.,0.,-1.)) ;
#19064 = DIRECTION('ref_axis',(1.,0.,0.)) ;
#19065 = DIRECTION('center_axis',(0.,0.,-1.)) ;
#19066 = DIRECTION('ref_axis',(0.,-1.,0.)) ;
#19067 = DIRECTION('',(-8.65956056235485E-17,-0.707106781186541,0.707106781186554)) ;
#19068 = DIRECTION('center_axis',(0.,0.,-1.)) ;
#19069 = DIRECTION('ref_axis',(0.,-1.,0.)) ;
#19070 = DIRECTION('center_axis',(0.,0.,1.)) ;
#19071 = DIRECTION('ref_axis',(1.,0.,0.)) ;
#19072 = DIRECTION('center_axis',(0.,0.,-1.)) ;
#19073 = DIRECTION('ref_axis',(1.,0.,0.)) ;
#19074 = DIRECTION('center_axis',(0.,0.,-1.)) ;
#19075 = DIRECTION('ref_axis',(0.,1.,0.)) ;
#19076 = DIRECTION('center_axis',(0.,0.,-1.)) ;
#19077 = DIRECTION('ref_axis',(0.,1.,0.)) ;
#19078 = DIRECTION('center_axis',(0.,0.,-1.)) ;
#19079 = DIRECTION('ref_axis',(0.,1.,0.)) ;
#19080 = DIRECTION('center_axis',(0.,0.,-1.)) ;
#19081 = DIRECTION('ref_axis',(-1.,0.,0.)) ;
#19082 = DIRECTION('center_axis',(0.,0.,-1.)) ;
#19083 = DIRECTION('ref_axis',(-1.,0.,0.)) ;
#19084 = DIRECTION('center_axis',(0.,0.,-1.)) ;
#19085 = DIRECTION('ref_axis',(1.,0.,0.)) ;
#19086 = DIRECTION('center_axis',(1.,0.,-7.40148683083438E-17)) ;
#19087 = DIRECTION('ref_axis',(-7.40148683083438E-17,0.,-1.)) ;
#19088 = DIRECTION('',(0.,1.,0.)) ;
#19089 = DIRECTION('',(-7.40148683083438E-17,0.,-1.)) ;
#19090 = DIRECTION('',(0.,1.,0.)) ;
#19091 = DIRECTION('center_axis',(0.,1.,0.)) ;
#19092 = DIRECTION('ref_axis',(-1.,0.,0.)) ;
#19093 = DIRECTION('center_axis',(0.,1.,0.)) ;
#19094 = DIRECTION('ref_axis',(-1.,0.,0.)) ;
#19095 = DIRECTION('',(0.,1.,0.)) ;
#19096 = DIRECTION('center_axis',(-1.,0.,-2.46716227694479E-17)) ;
#19097 = DIRECTION('ref_axis',(-2.46716227694479E-17,0.,1.)) ;
#19098 = DIRECTION('',(-2.46716227694479E-17,0.,1.)) ;
#19099 = DIRECTION('',(0.,1.,0.)) ;
#19100 = DIRECTION('center_axis',(0.,1.,0.)) ;
#19101 = DIRECTION('ref_axis',(1.,0.,0.)) ;
#19102 = DIRECTION('center_axis',(0.,1.,0.)) ;
#19103 = DIRECTION('ref_axis',(1.,0.,0.)) ;
#19104 = DIRECTION('center_axis',(0.,1.,0.)) ;
#19105 = DIRECTION('ref_axis',(1.,0.,0.)) ;
#19106 = DIRECTION('center_axis',(0.,0.,-1.)) ;
#19107 = DIRECTION('ref_axis',(0.,1.,0.)) ;
#19108 = DIRECTION('center_axis',(0.,0.,-1.)) ;
#19109 = DIRECTION('ref_axis',(1.,0.,0.)) ;
#19110 = DIRECTION('',(0.,0.,1.)) ;
#19111 = DIRECTION('center_axis',(0.,0.,1.)) ;
#19112 = DIRECTION('ref_axis',(1.,0.,0.)) ;
#19113 = DIRECTION('center_axis',(0.,0.,-1.)) ;
#19114 = DIRECTION('ref_axis',(1.,0.,0.)) ;
#19115 = DIRECTION('center_axis',(0.,0.,-1.)) ;
#19116 = DIRECTION('ref_axis',(0.,1.,0.)) ;
#19117 = DIRECTION('',(0.,0.,1.)) ;
#19118 = DIRECTION('center_axis',(0.,0.,-1.)) ;
#19119 = DIRECTION('ref_axis',(0.,1.,0.)) ;
#19120 = DIRECTION('',(0.,0.,1.)) ;
#19121 = DIRECTION('center_axis',(0.,0.,-1.)) ;
#19122 = DIRECTION('ref_axis',(0.,1.,0.)) ;
#19123 = DIRECTION('center_axis',(0.,0.,-1.)) ;
#19124 = DIRECTION('ref_axis',(1.,0.,0.)) ;
#19125 = DIRECTION('',(0.,0.,1.)) ;
#19126 = DIRECTION('center_axis',(0.,0.,-1.)) ;
#19127 = DIRECTION('ref_axis',(-1.,0.,0.)) ;
#19128 = DIRECTION('center_axis',(0.,0.,-1.)) ;
#19129 = DIRECTION('ref_axis',(1.,0.,0.)) ;
#19130 = DIRECTION('center_axis',(0.,0.,-1.)) ;
#19131 = DIRECTION('ref_axis',(0.,1.,0.)) ;
#19132 = DIRECTION('center_axis',(0.,0.,-1.)) ;
#19133 = DIRECTION('ref_axis',(1.,0.,0.)) ;
#19134 = DIRECTION('',(0.,0.,1.)) ;
#19135 = DIRECTION('center_axis',(0.,0.,1.)) ;
#19136 = DIRECTION('ref_axis',(1.,0.,0.)) ;
#19137 = DIRECTION('center_axis',(0.,0.,-1.)) ;
#19138 = DIRECTION('ref_axis',(0.,1.,0.)) ;
#19139 = DIRECTION('center_axis',(0.,0.,-1.)) ;
#19140 = DIRECTION('ref_axis',(1.,0.,0.)) ;
#19141 = DIRECTION('',(0.,0.,1.)) ;
#19142 = DIRECTION('center_axis',(0.,0.,1.)) ;
#19143 = DIRECTION('ref_axis',(1.,0.,0.)) ;
#19144 = DIRECTION('axis',(0.,0.,1.)) ;
#19145 = DIRECTION('refdir',(1.,0.,0.)) ;
#19146 = DIRECTION('center_axis',(0.,0.,-1.)) ;
#19147 = DIRECTION('ref_axis',(-1.,0.,0.)) ;
#19148 = DIRECTION('center_axis',(0.,0.,1.)) ;
#19149 = DIRECTION('ref_axis',(1.,0.,0.)) ;
#19150 = DIRECTION('center_axis',(0.,0.707106781186548,0.707106781186548)) ;
#19151 = DIRECTION('ref_axis',(0.,0.707106781186548,-0.707106781186548)) ;
#19152 = DIRECTION('',(0.,0.,-1.)) ;
#19153 = DIRECTION('center_axis',(0.,0.707106781186548,-0.707106781186547)) ;
#19154 = DIRECTION('ref_axis',(0.,-0.707106781186547,-0.707106781186548)) ;
#19155 = DIRECTION('center_axis',(0.,0.,1.)) ;
#19156 = DIRECTION('ref_axis',(1.,0.,0.)) ;
#19157 = DIRECTION('center_axis',(0.,-0.707106781186548,-0.707106781186548)) ;
#19158 = DIRECTION('ref_axis',(0.,0.707106781186548,-0.707106781186548)) ;
#19159 = DIRECTION('',(0.,0.,-1.)) ;
#19160 = DIRECTION('center_axis',(0.,-0.707106781186547,0.707106781186548)) ;
#19161 = DIRECTION('ref_axis',(0.,-0.707106781186548,-0.707106781186547)) ;
#19162 = DIRECTION('center_axis',(0.,1.,0.)) ;
#19163 = DIRECTION('ref_axis',(0.,0.,1.)) ;
#19164 = DIRECTION('',(-1.,0.,0.)) ;
#19165 = DIRECTION('',(0.,0.,-1.)) ;
#19166 = DIRECTION('',(-1.,0.,0.)) ;
#19167 = DIRECTION('center_axis',(0.,0.,-1.)) ;
#19168 = DIRECTION('ref_axis',(1.,1.22464679914735E-16,0.)) ;
#19169 = DIRECTION('',(0.,0.,-1.)) ;
#19170 = DIRECTION('center_axis',(0.,-0.707106781186548,-0.707106781186548)) ;
#19171 = DIRECTION('ref_axis',(0.,0.707106781186548,-0.707106781186548)) ;
#19172 = DIRECTION('center_axis',(0.,0.,1.)) ;
#19173 = DIRECTION('ref_axis',(1.,0.,0.)) ;
#19174 = DIRECTION('center_axis',(0.,0.707106781186548,-0.707106781186547)) ;
#19175 = DIRECTION('ref_axis',(0.,-0.707106781186547,-0.707106781186548)) ;
#19176 = DIRECTION('center_axis',(0.,0.707106781186548,0.707106781186548)) ;
#19177 = DIRECTION('ref_axis',(0.,0.707106781186548,-0.707106781186548)) ;
#19178 = DIRECTION('center_axis',(0.,0.,1.)) ;
#19179 = DIRECTION('ref_axis',(1.,0.,0.)) ;
#19180 = DIRECTION('center_axis',(0.,-0.707106781186547,0.707106781186548)) ;
#19181 = DIRECTION('ref_axis',(0.,-0.707106781186548,-0.707106781186547)) ;
#19182 = DIRECTION('center_axis',(0.,-1.,0.)) ;
#19183 = DIRECTION('ref_axis',(0.,0.,-1.)) ;
#19184 = DIRECTION('',(-1.,0.,0.)) ;
#19185 = DIRECTION('',(-1.,0.,0.)) ;
#19186 = DIRECTION('center_axis',(0.,0.,1.)) ;
#19187 = DIRECTION('ref_axis',(1.,0.,0.)) ;
#19188 = DIRECTION('',(1.,0.,0.)) ;
#19189 = DIRECTION('',(-1.,0.,0.)) ;
#19190 = DIRECTION('center_axis',(0.,0.,1.)) ;
#19191 = DIRECTION('ref_axis',(1.,0.,0.)) ;
#19192 = DIRECTION('',(1.,0.,0.)) ;
#19193 = DIRECTION('',(-1.,0.,0.)) ;
#19194 = DIRECTION('center_axis',(0.,0.707106781186548,0.707106781186548)) ;
#19195 = DIRECTION('ref_axis',(0.,-0.707106781186548,0.707106781186548)) ;
#19196 = DIRECTION('center_axis',(0.,-0.707106781186547,0.707106781186548)) ;
#19197 = DIRECTION('ref_axis',(0.,-0.707106781186548,-0.707106781186547)) ;
#19198 = DIRECTION('center_axis',(0.,0.707106781186548,-0.707106781186547)) ;
#19199 = DIRECTION('ref_axis',(0.,0.707106781186547,0.707106781186548)) ;
#19200 = DIRECTION('center_axis',(0.,-0.707106781186548,-0.707106781186548)) ;
#19201 = DIRECTION('ref_axis',(0.,0.707106781186548,-0.707106781186548)) ;
#19202 = DIRECTION('axis',(0.,0.,1.)) ;
#19203 = DIRECTION('refdir',(1.,0.,0.)) ;
#19204 = DIRECTION('center_axis',(0.,0.,1.)) ;
#19205 = DIRECTION('ref_axis',(1.,0.,0.)) ;
#19206 = DIRECTION('center_axis',(0.,0.,-1.)) ;
#19207 = DIRECTION('ref_axis',(1.,0.,0.)) ;
#19208 = DIRECTION('',(0.707106781186548,8.65956056235494E-17,-0.707106781186547)) ;
#19209 = DIRECTION('center_axis',(0.,0.,1.)) ;
#19210 = DIRECTION('ref_axis',(1.,0.,0.)) ;
#19211 = DIRECTION('center_axis',(0.,0.,1.)) ;
#19212 = DIRECTION('ref_axis',(1.,0.,0.)) ;
#19213 = DIRECTION('center_axis',(0.,0.,-1.)) ;
#19214 = DIRECTION('ref_axis',(1.,0.,0.)) ;
#19215 = DIRECTION('center_axis',(0.,0.,1.)) ;
#19216 = DIRECTION('ref_axis',(1.,0.,0.)) ;
#19217 = DIRECTION('center_axis',(0.,0.,1.)) ;
#19218 = DIRECTION('ref_axis',(1.,0.,0.)) ;
#19219 = DIRECTION('',(0.,0.,-1.)) ;
#19220 = DIRECTION('center_axis',(0.,0.,-1.)) ;
#19221 = DIRECTION('ref_axis',(1.,0.,0.)) ;
#19222 = DIRECTION('center_axis',(0.,0.,1.)) ;
#19223 = DIRECTION('ref_axis',(1.,0.,0.)) ;
#19224 = DIRECTION('',(-0.707106781186548,8.65956056235494E-17,-0.707106781186547)) ;
#19225 = DIRECTION('center_axis',(0.,0.,1.)) ;
#19226 = DIRECTION('ref_axis',(1.,0.,0.)) ;
#19227 = DIRECTION('',(0.,0.,1.)) ;
#19228 = DIRECTION('center_axis',(0.,0.,-1.)) ;
#19229 = DIRECTION('ref_axis',(1.,0.,0.)) ;
#19230 = DIRECTION('center_axis',(0.,0.,-1.)) ;
#19231 = DIRECTION('ref_axis',(1.,0.,0.)) ;
#19232 = DIRECTION('',(0.707106781186547,-8.65956056235493E-17,0.707106781186548)) ;
#19233 = DIRECTION('center_axis',(0.,0.,-1.)) ;
#19234 = DIRECTION('ref_axis',(1.,0.,0.)) ;
#19235 = DIRECTION('center_axis',(0.,0.,1.)) ;
#19236 = DIRECTION('ref_axis',(1.,0.,0.)) ;
#19237 = DIRECTION('center_axis',(0.,0.,1.)) ;
#19238 = DIRECTION('ref_axis',(1.,0.,0.)) ;
#19239 = DIRECTION('center_axis',(0.,0.,1.)) ;
#19240 = DIRECTION('ref_axis',(1.,0.,0.)) ;
#19241 = DIRECTION('',(-0.707106781186547,-8.65956056235493E-17,0.707106781186548)) ;
#19242 = DIRECTION('axis',(0.,0.,1.)) ;
#19243 = DIRECTION('refdir',(1.,0.,0.)) ;
#19244 = DIRECTION('center_axis',(0.,0.,1.)) ;
#19245 = DIRECTION('ref_axis',(0.,-1.,0.)) ;
#19246 = DIRECTION('',(1.,0.,0.)) ;
#19247 = DIRECTION('',(0.,-1.,0.)) ;
#19248 = DIRECTION('',(1.,0.,0.)) ;
#19249 = DIRECTION('',(0.,1.,0.)) ;
#19250 = DIRECTION('center_axis',(0.,1.,0.)) ;
#19251 = DIRECTION('ref_axis',(0.,0.,1.)) ;
#19252 = DIRECTION('',(0.,0.,1.)) ;
#19253 = DIRECTION('',(1.,0.,0.)) ;
#19254 = DIRECTION('',(0.,0.,-1.)) ;
#19255 = DIRECTION('center_axis',(0.,0.,-1.)) ;
#19256 = DIRECTION('ref_axis',(0.,1.,0.)) ;
#19257 = DIRECTION('',(-1.,0.,0.)) ;
#19258 = DIRECTION('',(0.,-1.,0.)) ;
#19259 = DIRECTION('',(0.,1.,0.)) ;
#19260 = DIRECTION('center_axis',(1.,0.,0.)) ;
#19261 = DIRECTION('ref_axis',(0.,0.,-1.)) ;
#19262 = DIRECTION('center_axis',(1.,0.,0.)) ;
#19263 = DIRECTION('ref_axis',(0.,0.,-1.)) ;
#19264 = DIRECTION('center_axis',(1.,0.,0.)) ;
#19265 = DIRECTION('ref_axis',(0.,0.,-1.)) ;
#19266 = DIRECTION('center_axis',(1.,0.,0.)) ;
#19267 = DIRECTION('ref_axis',(0.,0.,-1.)) ;
#19268 = DIRECTION('',(-1.,0.,0.)) ;
#19269 = DIRECTION('center_axis',(1.,0.,0.)) ;
#19270 = DIRECTION('ref_axis',(0.,0.,-1.)) ;
#19271 = DIRECTION('',(-1.,0.,0.)) ;
#19272 = DIRECTION('center_axis',(1.,0.,0.)) ;
#19273 = DIRECTION('ref_axis',(0.,0.,-1.)) ;
#19274 = DIRECTION('center_axis',(1.,0.,0.)) ;
#19275 = DIRECTION('ref_axis',(0.,0.,-1.)) ;
#19276 = DIRECTION('center_axis',(1.,0.,0.)) ;
#19277 = DIRECTION('ref_axis',(0.,0.,-1.)) ;
#19278 = DIRECTION('',(-1.,0.,0.)) ;
#19279 = DIRECTION('center_axis',(1.,0.,0.)) ;
#19280 = DIRECTION('ref_axis',(0.,0.,-1.)) ;
#19281 = DIRECTION('',(-1.,0.,0.)) ;
#19282 = DIRECTION('center_axis',(1.,0.,0.)) ;
#19283 = DIRECTION('ref_axis',(0.,0.,-1.)) ;
#19284 = DIRECTION('center_axis',(1.,0.,0.)) ;
#19285 = DIRECTION('ref_axis',(0.,0.,-1.)) ;
#19286 = DIRECTION('',(-1.,0.,0.)) ;
#19287 = DIRECTION('center_axis',(1.,0.,0.)) ;
#19288 = DIRECTION('ref_axis',(0.,0.,-1.)) ;
#19289 = DIRECTION('',(-1.,0.,0.)) ;
#19290 = DIRECTION('center_axis',(1.,0.,0.)) ;
#19291 = DIRECTION('ref_axis',(0.,0.,-1.)) ;
#19292 = DIRECTION('center_axis',(1.,0.,0.)) ;
#19293 = DIRECTION('ref_axis',(0.,0.,-1.)) ;
#19294 = DIRECTION('',(-1.,0.,0.)) ;
#19295 = DIRECTION('center_axis',(1.,0.,0.)) ;
#19296 = DIRECTION('ref_axis',(0.,0.,-1.)) ;
#19297 = DIRECTION('',(-1.,0.,0.)) ;
#19298 = DIRECTION('center_axis',(1.,0.,0.)) ;
#19299 = DIRECTION('ref_axis',(0.,0.,-1.)) ;
#19300 = DIRECTION('',(-1.,0.,0.)) ;
#19301 = DIRECTION('center_axis',(1.,0.,0.)) ;
#19302 = DIRECTION('ref_axis',(0.,0.,-1.)) ;
#19303 = DIRECTION('',(-1.,0.,0.)) ;
#19304 = DIRECTION('center_axis',(1.,0.,0.)) ;
#19305 = DIRECTION('ref_axis',(0.,0.,-1.)) ;
#19306 = DIRECTION('center_axis',(1.,0.,0.)) ;
#19307 = DIRECTION('ref_axis',(0.,0.,-1.)) ;
#19308 = DIRECTION('',(-1.,0.,0.)) ;
#19309 = DIRECTION('center_axis',(1.,0.,0.)) ;
#19310 = DIRECTION('ref_axis',(0.,0.,-1.)) ;
#19311 = DIRECTION('',(-1.,0.,0.)) ;
#19312 = DIRECTION('center_axis',(1.,0.,0.)) ;
#19313 = DIRECTION('ref_axis',(0.,0.,-1.)) ;
#19314 = DIRECTION('center_axis',(1.,0.,0.)) ;
#19315 = DIRECTION('ref_axis',(0.,0.,-1.)) ;
#19316 = DIRECTION('',(-1.,0.,0.)) ;
#19317 = DIRECTION('center_axis',(1.,0.,0.)) ;
#19318 = DIRECTION('ref_axis',(0.,0.,-1.)) ;
#19319 = DIRECTION('',(-1.,0.,0.)) ;
#19320 = DIRECTION('center_axis',(1.,0.,0.)) ;
#19321 = DIRECTION('ref_axis',(0.,0.,-1.)) ;
#19322 = DIRECTION('center_axis',(1.,0.,0.)) ;
#19323 = DIRECTION('ref_axis',(0.,0.,-1.)) ;
#19324 = DIRECTION('center_axis',(1.,0.,0.)) ;
#19325 = DIRECTION('ref_axis',(0.,0.,-1.)) ;
#19326 = DIRECTION('',(-1.,0.,0.)) ;
#19327 = DIRECTION('center_axis',(1.,0.,0.)) ;
#19328 = DIRECTION('ref_axis',(0.,0.,-1.)) ;
#19329 = DIRECTION('',(-1.,0.,0.)) ;
#19330 = DIRECTION('center_axis',(1.,0.,0.)) ;
#19331 = DIRECTION('ref_axis',(0.,0.,-1.)) ;
#19332 = DIRECTION('center_axis',(1.,0.,0.)) ;
#19333 = DIRECTION('ref_axis',(0.,0.,-1.)) ;
#19334 = DIRECTION('',(-1.,0.,0.)) ;
#19335 = DIRECTION('center_axis',(1.,0.,0.)) ;
#19336 = DIRECTION('ref_axis',(0.,0.,-1.)) ;
#19337 = DIRECTION('',(-1.,0.,0.)) ;
#19338 = DIRECTION('center_axis',(1.,0.,0.)) ;
#19339 = DIRECTION('ref_axis',(0.,0.,-1.)) ;
#19340 = DIRECTION('center_axis',(1.,0.,0.)) ;
#19341 = DIRECTION('ref_axis',(0.,0.,-1.)) ;
#19342 = DIRECTION('',(-1.,0.,0.)) ;
#19343 = DIRECTION('center_axis',(1.,0.,0.)) ;
#19344 = DIRECTION('ref_axis',(0.,0.,-1.)) ;
#19345 = DIRECTION('',(-1.,0.,0.)) ;
#19346 = DIRECTION('center_axis',(1.,0.,0.)) ;
#19347 = DIRECTION('ref_axis',(0.,0.,-1.)) ;
#19348 = DIRECTION('center_axis',(1.,0.,0.)) ;
#19349 = DIRECTION('ref_axis',(0.,0.,-1.)) ;
#19350 = DIRECTION('',(-1.,0.,0.)) ;
#19351 = DIRECTION('center_axis',(1.,0.,0.)) ;
#19352 = DIRECTION('ref_axis',(0.,0.,-1.)) ;
#19353 = DIRECTION('',(-1.,0.,0.)) ;
#19354 = DIRECTION('center_axis',(1.,0.,0.)) ;
#19355 = DIRECTION('ref_axis',(0.,0.,-1.)) ;
#19356 = DIRECTION('center_axis',(1.,0.,0.)) ;
#19357 = DIRECTION('ref_axis',(0.,0.,-1.)) ;
#19358 = DIRECTION('',(-1.,0.,0.)) ;
#19359 = DIRECTION('center_axis',(1.,0.,0.)) ;
#19360 = DIRECTION('ref_axis',(0.,0.,-1.)) ;
#19361 = DIRECTION('',(-1.,0.,0.)) ;
#19362 = DIRECTION('center_axis',(1.,0.,0.)) ;
#19363 = DIRECTION('ref_axis',(0.,0.,-1.)) ;
#19364 = DIRECTION('center_axis',(1.,0.,0.)) ;
#19365 = DIRECTION('ref_axis',(0.,0.,-1.)) ;
#19366 = DIRECTION('',(-1.,0.,0.)) ;
#19367 = DIRECTION('center_axis',(1.,0.,0.)) ;
#19368 = DIRECTION('ref_axis',(0.,0.,-1.)) ;
#19369 = DIRECTION('',(-1.,0.,0.)) ;
#19370 = DIRECTION('center_axis',(1.,0.,0.)) ;
#19371 = DIRECTION('ref_axis',(0.,0.,-1.)) ;
#19372 = DIRECTION('center_axis',(1.,0.,0.)) ;
#19373 = DIRECTION('ref_axis',(0.,0.,-1.)) ;
#19374 = DIRECTION('',(-1.,0.,0.)) ;
#19375 = DIRECTION('center_axis',(1.,0.,0.)) ;
#19376 = DIRECTION('ref_axis',(0.,0.,-1.)) ;
#19377 = DIRECTION('',(-1.,0.,0.)) ;
#19378 = DIRECTION('center_axis',(1.,0.,0.)) ;
#19379 = DIRECTION('ref_axis',(0.,0.,-1.)) ;
#19380 = DIRECTION('center_axis',(1.,0.,0.)) ;
#19381 = DIRECTION('ref_axis',(0.,0.,-1.)) ;
#19382 = DIRECTION('',(-1.,0.,0.)) ;
#19383 = DIRECTION('center_axis',(1.,0.,0.)) ;
#19384 = DIRECTION('ref_axis',(0.,0.,-1.)) ;
#19385 = DIRECTION('',(-1.,0.,0.)) ;
#19386 = DIRECTION('center_axis',(1.,0.,0.)) ;
#19387 = DIRECTION('ref_axis',(0.,0.,-1.)) ;
#19388 = DIRECTION('center_axis',(1.,0.,0.)) ;
#19389 = DIRECTION('ref_axis',(0.,0.,-1.)) ;
#19390 = DIRECTION('',(-1.,0.,0.)) ;
#19391 = DIRECTION('center_axis',(1.,0.,0.)) ;
#19392 = DIRECTION('ref_axis',(0.,0.,-1.)) ;
#19393 = DIRECTION('',(-1.,0.,0.)) ;
#19394 = DIRECTION('center_axis',(1.,0.,0.)) ;
#19395 = DIRECTION('ref_axis',(0.,0.,-1.)) ;
#19396 = DIRECTION('center_axis',(1.,0.,0.)) ;
#19397 = DIRECTION('ref_axis',(0.,0.,-1.)) ;
#19398 = DIRECTION('',(-1.,0.,0.)) ;
#19399 = DIRECTION('center_axis',(1.,0.,0.)) ;
#19400 = DIRECTION('ref_axis',(0.,0.,-1.)) ;
#19401 = DIRECTION('',(-1.,0.,0.)) ;
#19402 = DIRECTION('center_axis',(1.,0.,0.)) ;
#19403 = DIRECTION('ref_axis',(0.,0.,-1.)) ;
#19404 = DIRECTION('center_axis',(1.,0.,0.)) ;
#19405 = DIRECTION('ref_axis',(0.,0.,-1.)) ;
#19406 = DIRECTION('',(-1.,0.,0.)) ;
#19407 = DIRECTION('center_axis',(1.,0.,0.)) ;
#19408 = DIRECTION('ref_axis',(0.,0.,-1.)) ;
#19409 = DIRECTION('',(-1.,0.,0.)) ;
#19410 = DIRECTION('center_axis',(1.,0.,0.)) ;
#19411 = DIRECTION('ref_axis',(0.,0.,-1.)) ;
#19412 = DIRECTION('center_axis',(1.,0.,0.)) ;
#19413 = DIRECTION('ref_axis',(0.,0.,-1.)) ;
#19414 = DIRECTION('',(-1.,0.,0.)) ;
#19415 = DIRECTION('center_axis',(1.,0.,0.)) ;
#19416 = DIRECTION('ref_axis',(0.,0.,-1.)) ;
#19417 = DIRECTION('',(-1.,0.,0.)) ;
#19418 = DIRECTION('center_axis',(1.,0.,0.)) ;
#19419 = DIRECTION('ref_axis',(0.,0.,-1.)) ;
#19420 = DIRECTION('center_axis',(1.,0.,0.)) ;
#19421 = DIRECTION('ref_axis',(0.,0.,-1.)) ;
#19422 = DIRECTION('',(-1.,0.,0.)) ;
#19423 = DIRECTION('center_axis',(1.,0.,0.)) ;
#19424 = DIRECTION('ref_axis',(0.,0.,-1.)) ;
#19425 = DIRECTION('',(-1.,0.,0.)) ;
#19426 = DIRECTION('center_axis',(1.,0.,0.)) ;
#19427 = DIRECTION('ref_axis',(0.,0.,-1.)) ;
#19428 = DIRECTION('',(-1.,0.,0.)) ;
#19429 = DIRECTION('center_axis',(1.,0.,0.)) ;
#19430 = DIRECTION('ref_axis',(0.,0.,-1.)) ;
#19431 = DIRECTION('',(-1.,0.,0.)) ;
#19432 = DIRECTION('center_axis',(1.,0.,0.)) ;
#19433 = DIRECTION('ref_axis',(0.,0.,-1.)) ;
#19434 = DIRECTION('center_axis',(1.,0.,0.)) ;
#19435 = DIRECTION('ref_axis',(0.,0.,-1.)) ;
#19436 = DIRECTION('center_axis',(1.,0.,0.)) ;
#19437 = DIRECTION('ref_axis',(0.,0.,-1.)) ;
#19438 = DIRECTION('',(-1.,0.,0.)) ;
#19439 = DIRECTION('center_axis',(1.,0.,0.)) ;
#19440 = DIRECTION('ref_axis',(0.,0.,-1.)) ;
#19441 = DIRECTION('',(-1.,0.,0.)) ;
#19442 = DIRECTION('center_axis',(1.,0.,0.)) ;
#19443 = DIRECTION('ref_axis',(0.,0.,-1.)) ;
#19444 = DIRECTION('center_axis',(1.,0.,0.)) ;
#19445 = DIRECTION('ref_axis',(0.,0.,-1.)) ;
#19446 = DIRECTION('',(-1.,0.,0.)) ;
#19447 = DIRECTION('center_axis',(1.,0.,0.)) ;
#19448 = DIRECTION('ref_axis',(0.,0.,-1.)) ;
#19449 = DIRECTION('',(-1.,0.,0.)) ;
#19450 = DIRECTION('center_axis',(1.,0.,0.)) ;
#19451 = DIRECTION('ref_axis',(0.,0.,-1.)) ;
#19452 = DIRECTION('center_axis',(1.,0.,0.)) ;
#19453 = DIRECTION('ref_axis',(0.,0.,-1.)) ;
#19454 = DIRECTION('',(-1.,0.,0.)) ;
#19455 = DIRECTION('center_axis',(1.,0.,0.)) ;
#19456 = DIRECTION('ref_axis',(0.,0.,-1.)) ;
#19457 = DIRECTION('',(-1.,0.,0.)) ;
#19458 = DIRECTION('center_axis',(1.,0.,0.)) ;
#19459 = DIRECTION('ref_axis',(0.,0.,-1.)) ;
#19460 = DIRECTION('center_axis',(1.,0.,0.)) ;
#19461 = DIRECTION('ref_axis',(0.,0.,-1.)) ;
#19462 = DIRECTION('',(-1.,0.,0.)) ;
#19463 = DIRECTION('center_axis',(1.,0.,0.)) ;
#19464 = DIRECTION('ref_axis',(0.,0.,-1.)) ;
#19465 = DIRECTION('',(-1.,0.,0.)) ;
#19466 = DIRECTION('center_axis',(1.,0.,0.)) ;
#19467 = DIRECTION('ref_axis',(0.,0.,-1.)) ;
#19468 = DIRECTION('center_axis',(1.,0.,0.)) ;
#19469 = DIRECTION('ref_axis',(0.,0.,-1.)) ;
#19470 = DIRECTION('',(-1.,0.,0.)) ;
#19471 = DIRECTION('center_axis',(1.,0.,0.)) ;
#19472 = DIRECTION('ref_axis',(0.,0.,-1.)) ;
#19473 = DIRECTION('',(-1.,0.,0.)) ;
#19474 = DIRECTION('center_axis',(1.,0.,0.)) ;
#19475 = DIRECTION('ref_axis',(0.,0.,-1.)) ;
#19476 = DIRECTION('center_axis',(1.,0.,0.)) ;
#19477 = DIRECTION('ref_axis',(0.,0.,-1.)) ;
#19478 = DIRECTION('',(-1.,0.,0.)) ;
#19479 = DIRECTION('center_axis',(1.,0.,0.)) ;
#19480 = DIRECTION('ref_axis',(0.,0.,-1.)) ;
#19481 = DIRECTION('',(-1.,0.,0.)) ;
#19482 = DIRECTION('center_axis',(1.,0.,0.)) ;
#19483 = DIRECTION('ref_axis',(0.,0.,-1.)) ;
#19484 = DIRECTION('center_axis',(1.,0.,0.)) ;
#19485 = DIRECTION('ref_axis',(0.,0.,-1.)) ;
#19486 = DIRECTION('',(-1.,0.,0.)) ;
#19487 = DIRECTION('center_axis',(1.,0.,0.)) ;
#19488 = DIRECTION('ref_axis',(0.,0.,-1.)) ;
#19489 = DIRECTION('',(-1.,0.,0.)) ;
#19490 = DIRECTION('center_axis',(1.,0.,0.)) ;
#19491 = DIRECTION('ref_axis',(0.,0.,-1.)) ;
#19492 = DIRECTION('center_axis',(1.,0.,0.)) ;
#19493 = DIRECTION('ref_axis',(0.,0.,-1.)) ;
#19494 = DIRECTION('',(-1.,0.,0.)) ;
#19495 = DIRECTION('center_axis',(1.,0.,0.)) ;
#19496 = DIRECTION('ref_axis',(0.,0.,-1.)) ;
#19497 = DIRECTION('',(-1.,0.,0.)) ;
#19498 = DIRECTION('center_axis',(1.,0.,0.)) ;
#19499 = DIRECTION('ref_axis',(0.,0.,-1.)) ;
#19500 = DIRECTION('center_axis',(1.,0.,0.)) ;
#19501 = DIRECTION('ref_axis',(0.,0.,-1.)) ;
#19502 = DIRECTION('',(-1.,0.,0.)) ;
#19503 = DIRECTION('center_axis',(1.,0.,0.)) ;
#19504 = DIRECTION('ref_axis',(0.,0.,-1.)) ;
#19505 = DIRECTION('',(-1.,0.,0.)) ;
#19506 = DIRECTION('center_axis',(1.,0.,0.)) ;
#19507 = DIRECTION('ref_axis',(0.,0.,-1.)) ;
#19508 = DIRECTION('center_axis',(1.,0.,0.)) ;
#19509 = DIRECTION('ref_axis',(0.,0.,-1.)) ;
#19510 = DIRECTION('',(-1.,0.,0.)) ;
#19511 = DIRECTION('center_axis',(1.,0.,0.)) ;
#19512 = DIRECTION('ref_axis',(0.,0.,-1.)) ;
#19513 = DIRECTION('',(-1.,0.,0.)) ;
#19514 = DIRECTION('center_axis',(1.,0.,0.)) ;
#19515 = DIRECTION('ref_axis',(0.,0.,-1.)) ;
#19516 = DIRECTION('center_axis',(1.,0.,0.)) ;
#19517 = DIRECTION('ref_axis',(0.,0.,-1.)) ;
#19518 = DIRECTION('',(-1.,0.,0.)) ;
#19519 = DIRECTION('center_axis',(1.,0.,0.)) ;
#19520 = DIRECTION('ref_axis',(0.,0.,-1.)) ;
#19521 = DIRECTION('',(-1.,0.,0.)) ;
#19522 = DIRECTION('center_axis',(1.,0.,0.)) ;
#19523 = DIRECTION('ref_axis',(0.,0.,-1.)) ;
#19524 = DIRECTION('',(-1.,0.,0.)) ;
#19525 = DIRECTION('center_axis',(1.,0.,0.)) ;
#19526 = DIRECTION('ref_axis',(0.,0.,-1.)) ;
#19527 = DIRECTION('',(-1.,0.,0.)) ;
#19528 = DIRECTION('center_axis',(1.,0.,0.)) ;
#19529 = DIRECTION('ref_axis',(0.,0.,-1.)) ;
#19530 = DIRECTION('center_axis',(1.,0.,0.)) ;
#19531 = DIRECTION('ref_axis',(0.,0.,-1.)) ;
#19532 = DIRECTION('',(-1.,0.,0.)) ;
#19533 = DIRECTION('center_axis',(1.,0.,0.)) ;
#19534 = DIRECTION('ref_axis',(0.,0.,-1.)) ;
#19535 = DIRECTION('',(-1.,0.,0.)) ;
#19536 = DIRECTION('center_axis',(1.,0.,0.)) ;
#19537 = DIRECTION('ref_axis',(0.,0.,-1.)) ;
#19538 = DIRECTION('center_axis',(1.,0.,0.)) ;
#19539 = DIRECTION('ref_axis',(0.,0.,-1.)) ;
#19540 = DIRECTION('',(-1.,0.,0.)) ;
#19541 = DIRECTION('center_axis',(1.,0.,0.)) ;
#19542 = DIRECTION('ref_axis',(0.,0.,-1.)) ;
#19543 = DIRECTION('',(-1.,0.,0.)) ;
#19544 = DIRECTION('center_axis',(1.,0.,0.)) ;
#19545 = DIRECTION('ref_axis',(0.,0.,-1.)) ;
#19546 = DIRECTION('center_axis',(1.,0.,0.)) ;
#19547 = DIRECTION('ref_axis',(0.,0.,-1.)) ;
#19548 = DIRECTION('',(-1.,0.,0.)) ;
#19549 = DIRECTION('center_axis',(1.,0.,0.)) ;
#19550 = DIRECTION('ref_axis',(0.,0.,-1.)) ;
#19551 = DIRECTION('',(-1.,0.,0.)) ;
#19552 = DIRECTION('center_axis',(1.,0.,0.)) ;
#19553 = DIRECTION('ref_axis',(0.,0.,-1.)) ;
#19554 = DIRECTION('center_axis',(1.,0.,0.)) ;
#19555 = DIRECTION('ref_axis',(0.,0.,-1.)) ;
#19556 = DIRECTION('',(-1.,0.,0.)) ;
#19557 = DIRECTION('center_axis',(1.,0.,0.)) ;
#19558 = DIRECTION('ref_axis',(0.,0.,-1.)) ;
#19559 = DIRECTION('',(-1.,0.,0.)) ;
#19560 = DIRECTION('center_axis',(1.,0.,0.)) ;
#19561 = DIRECTION('ref_axis',(0.,0.,-1.)) ;
#19562 = DIRECTION('center_axis',(1.,0.,0.)) ;
#19563 = DIRECTION('ref_axis',(0.,0.,-1.)) ;
#19564 = DIRECTION('',(-1.,0.,0.)) ;
#19565 = DIRECTION('center_axis',(1.,0.,0.)) ;
#19566 = DIRECTION('ref_axis',(0.,0.,-1.)) ;
#19567 = DIRECTION('',(-1.,0.,0.)) ;
#19568 = DIRECTION('center_axis',(1.,0.,0.)) ;
#19569 = DIRECTION('ref_axis',(0.,0.,-1.)) ;
#19570 = DIRECTION('center_axis',(1.,0.,0.)) ;
#19571 = DIRECTION('ref_axis',(0.,0.,-1.)) ;
#19572 = DIRECTION('',(-1.,0.,0.)) ;
#19573 = DIRECTION('center_axis',(1.,0.,0.)) ;
#19574 = DIRECTION('ref_axis',(0.,0.,-1.)) ;
#19575 = DIRECTION('',(-1.,0.,0.)) ;
#19576 = DIRECTION('center_axis',(1.,0.,0.)) ;
#19577 = DIRECTION('ref_axis',(0.,0.,-1.)) ;
#19578 = DIRECTION('center_axis',(1.,0.,0.)) ;
#19579 = DIRECTION('ref_axis',(0.,0.,-1.)) ;
#19580 = DIRECTION('center_axis',(1.,0.,0.)) ;
#19581 = DIRECTION('ref_axis',(0.,0.,-1.)) ;
#19582 = DIRECTION('',(-1.,0.,0.)) ;
#19583 = DIRECTION('center_axis',(1.,0.,0.)) ;
#19584 = DIRECTION('ref_axis',(0.,0.,-1.)) ;
#19585 = DIRECTION('',(-1.,0.,0.)) ;
#19586 = DIRECTION('center_axis',(1.,0.,0.)) ;
#19587 = DIRECTION('ref_axis',(0.,0.,-1.)) ;
#19588 = DIRECTION('center_axis',(1.,0.,0.)) ;
#19589 = DIRECTION('ref_axis',(0.,0.,-1.)) ;
#19590 = DIRECTION('',(-1.,0.,0.)) ;
#19591 = DIRECTION('center_axis',(1.,0.,0.)) ;
#19592 = DIRECTION('ref_axis',(0.,0.,-1.)) ;
#19593 = DIRECTION('',(-1.,0.,0.)) ;
#19594 = DIRECTION('center_axis',(1.,0.,0.)) ;
#19595 = DIRECTION('ref_axis',(0.,0.,-1.)) ;
#19596 = DIRECTION('center_axis',(1.,0.,0.)) ;
#19597 = DIRECTION('ref_axis',(0.,0.,-1.)) ;
#19598 = DIRECTION('',(-1.,0.,0.)) ;
#19599 = DIRECTION('center_axis',(1.,0.,0.)) ;
#19600 = DIRECTION('ref_axis',(0.,0.,-1.)) ;
#19601 = DIRECTION('',(-1.,0.,0.)) ;
#19602 = DIRECTION('center_axis',(1.,0.,0.)) ;
#19603 = DIRECTION('ref_axis',(0.,0.,-1.)) ;
#19604 = DIRECTION('center_axis',(1.,0.,0.)) ;
#19605 = DIRECTION('ref_axis',(0.,0.,-1.)) ;
#19606 = DIRECTION('',(-1.,0.,0.)) ;
#19607 = DIRECTION('center_axis',(1.,0.,0.)) ;
#19608 = DIRECTION('ref_axis',(0.,0.,-1.)) ;
#19609 = DIRECTION('',(-1.,0.,0.)) ;
#19610 = DIRECTION('center_axis',(1.,0.,0.)) ;
#19611 = DIRECTION('ref_axis',(0.,0.,-1.)) ;
#19612 = DIRECTION('center_axis',(1.,0.,0.)) ;
#19613 = DIRECTION('ref_axis',(0.,0.,-1.)) ;
#19614 = DIRECTION('',(-1.,0.,0.)) ;
#19615 = DIRECTION('center_axis',(1.,0.,0.)) ;
#19616 = DIRECTION('ref_axis',(0.,0.,-1.)) ;
#19617 = DIRECTION('',(-1.,0.,0.)) ;
#19618 = DIRECTION('center_axis',(1.,0.,0.)) ;
#19619 = DIRECTION('ref_axis',(0.,0.,-1.)) ;
#19620 = DIRECTION('center_axis',(1.,0.,0.)) ;
#19621 = DIRECTION('ref_axis',(0.,0.,-1.)) ;
#19622 = DIRECTION('',(-1.,0.,0.)) ;
#19623 = DIRECTION('center_axis',(1.,0.,0.)) ;
#19624 = DIRECTION('ref_axis',(0.,0.,-1.)) ;
#19625 = DIRECTION('',(-1.,0.,0.)) ;
#19626 = DIRECTION('center_axis',(1.,0.,0.)) ;
#19627 = DIRECTION('ref_axis',(0.,0.,-1.)) ;
#19628 = DIRECTION('center_axis',(1.,0.,0.)) ;
#19629 = DIRECTION('ref_axis',(0.,0.,-1.)) ;
#19630 = DIRECTION('',(-1.,0.,0.)) ;
#19631 = DIRECTION('center_axis',(1.,0.,0.)) ;
#19632 = DIRECTION('ref_axis',(0.,0.,-1.)) ;
#19633 = DIRECTION('',(-1.,0.,0.)) ;
#19634 = DIRECTION('center_axis',(1.,0.,0.)) ;
#19635 = DIRECTION('ref_axis',(0.,0.,-1.)) ;
#19636 = DIRECTION('center_axis',(1.,0.,0.)) ;
#19637 = DIRECTION('ref_axis',(0.,0.,-1.)) ;
#19638 = DIRECTION('',(-1.,0.,0.)) ;
#19639 = DIRECTION('center_axis',(1.,0.,0.)) ;
#19640 = DIRECTION('ref_axis',(0.,0.,-1.)) ;
#19641 = DIRECTION('',(-1.,0.,0.)) ;
#19642 = DIRECTION('center_axis',(1.,0.,0.)) ;
#19643 = DIRECTION('ref_axis',(0.,0.,-1.)) ;
#19644 = DIRECTION('center_axis',(1.,0.,0.)) ;
#19645 = DIRECTION('ref_axis',(0.,0.,-1.)) ;
#19646 = DIRECTION('',(-1.,0.,0.)) ;
#19647 = DIRECTION('center_axis',(1.,0.,0.)) ;
#19648 = DIRECTION('ref_axis',(0.,0.,-1.)) ;
#19649 = DIRECTION('',(-1.,0.,0.)) ;
#19650 = DIRECTION('center_axis',(1.,0.,0.)) ;
#19651 = DIRECTION('ref_axis',(0.,0.,-1.)) ;
#19652 = DIRECTION('center_axis',(1.,0.,0.)) ;
#19653 = DIRECTION('ref_axis',(0.,0.,-1.)) ;
#19654 = DIRECTION('',(-1.,0.,0.)) ;
#19655 = DIRECTION('center_axis',(1.,0.,0.)) ;
#19656 = DIRECTION('ref_axis',(0.,0.,-1.)) ;
#19657 = DIRECTION('',(-1.,0.,0.)) ;
#19658 = DIRECTION('center_axis',(1.,0.,0.)) ;
#19659 = DIRECTION('ref_axis',(0.,0.,-1.)) ;
#19660 = DIRECTION('center_axis',(1.,0.,0.)) ;
#19661 = DIRECTION('ref_axis',(0.,0.,-1.)) ;
#19662 = DIRECTION('',(-1.,0.,0.)) ;
#19663 = DIRECTION('center_axis',(1.,0.,0.)) ;
#19664 = DIRECTION('ref_axis',(0.,0.,-1.)) ;
#19665 = DIRECTION('',(-1.,0.,0.)) ;
#19666 = DIRECTION('center_axis',(1.,0.,0.)) ;
#19667 = DIRECTION('ref_axis',(0.,0.,-1.)) ;
#19668 = DIRECTION('',(-1.,0.,0.)) ;
#19669 = DIRECTION('center_axis',(1.,0.,0.)) ;
#19670 = DIRECTION('ref_axis',(0.,0.,-1.)) ;
#19671 = DIRECTION('',(-1.,0.,0.)) ;
#19672 = DIRECTION('center_axis',(1.,0.,0.)) ;
#19673 = DIRECTION('ref_axis',(0.,0.,-1.)) ;
#19674 = DIRECTION('center_axis',(1.,0.,0.)) ;
#19675 = DIRECTION('ref_axis',(0.,0.,-1.)) ;
#19676 = DIRECTION('center_axis',(1.,0.,0.)) ;
#19677 = DIRECTION('ref_axis',(0.,0.,-1.)) ;
#19678 = DIRECTION('',(-1.,0.,0.)) ;
#19679 = DIRECTION('center_axis',(1.,0.,0.)) ;
#19680 = DIRECTION('ref_axis',(0.,0.,-1.)) ;
#19681 = DIRECTION('',(-1.,0.,0.)) ;
#19682 = DIRECTION('center_axis',(1.,0.,0.)) ;
#19683 = DIRECTION('ref_axis',(0.,0.,-1.)) ;
#19684 = DIRECTION('center_axis',(1.,0.,0.)) ;
#19685 = DIRECTION('ref_axis',(0.,0.,-1.)) ;
#19686 = DIRECTION('',(-1.,0.,0.)) ;
#19687 = DIRECTION('center_axis',(1.,0.,0.)) ;
#19688 = DIRECTION('ref_axis',(0.,0.,-1.)) ;
#19689 = DIRECTION('',(-1.,0.,0.)) ;
#19690 = DIRECTION('center_axis',(1.,0.,0.)) ;
#19691 = DIRECTION('ref_axis',(0.,0.,-1.)) ;
#19692 = DIRECTION('center_axis',(1.,0.,0.)) ;
#19693 = DIRECTION('ref_axis',(0.,0.,-1.)) ;
#19694 = DIRECTION('',(-1.,0.,0.)) ;
#19695 = DIRECTION('center_axis',(1.,0.,0.)) ;
#19696 = DIRECTION('ref_axis',(0.,0.,-1.)) ;
#19697 = DIRECTION('',(-1.,0.,0.)) ;
#19698 = DIRECTION('center_axis',(1.,0.,0.)) ;
#19699 = DIRECTION('ref_axis',(0.,0.,-1.)) ;
#19700 = DIRECTION('center_axis',(1.,0.,0.)) ;
#19701 = DIRECTION('ref_axis',(0.,0.,-1.)) ;
#19702 = DIRECTION('',(-1.,0.,0.)) ;
#19703 = DIRECTION('center_axis',(1.,0.,0.)) ;
#19704 = DIRECTION('ref_axis',(0.,0.,-1.)) ;
#19705 = DIRECTION('',(-1.,0.,0.)) ;
#19706 = DIRECTION('center_axis',(1.,0.,0.)) ;
#19707 = DIRECTION('ref_axis',(0.,0.,-1.)) ;
#19708 = DIRECTION('center_axis',(1.,0.,0.)) ;
#19709 = DIRECTION('ref_axis',(0.,0.,-1.)) ;
#19710 = DIRECTION('',(-1.,0.,0.)) ;
#19711 = DIRECTION('center_axis',(1.,0.,0.)) ;
#19712 = DIRECTION('ref_axis',(0.,0.,-1.)) ;
#19713 = DIRECTION('',(-1.,0.,0.)) ;
#19714 = DIRECTION('center_axis',(1.,0.,0.)) ;
#19715 = DIRECTION('ref_axis',(0.,0.,-1.)) ;
#19716 = DIRECTION('center_axis',(1.,0.,0.)) ;
#19717 = DIRECTION('ref_axis',(0.,0.,-1.)) ;
#19718 = DIRECTION('',(-1.,0.,0.)) ;
#19719 = DIRECTION('center_axis',(1.,0.,0.)) ;
#19720 = DIRECTION('ref_axis',(0.,0.,-1.)) ;
#19721 = DIRECTION('',(-1.,0.,0.)) ;
#19722 = DIRECTION('center_axis',(1.,0.,0.)) ;
#19723 = DIRECTION('ref_axis',(0.,0.,-1.)) ;
#19724 = DIRECTION('center_axis',(1.,0.,0.)) ;
#19725 = DIRECTION('ref_axis',(0.,0.,-1.)) ;
#19726 = DIRECTION('',(-1.,0.,0.)) ;
#19727 = DIRECTION('center_axis',(1.,0.,0.)) ;
#19728 = DIRECTION('ref_axis',(0.,0.,-1.)) ;
#19729 = DIRECTION('',(-1.,0.,0.)) ;
#19730 = DIRECTION('center_axis',(1.,0.,0.)) ;
#19731 = DIRECTION('ref_axis',(0.,0.,-1.)) ;
#19732 = DIRECTION('',(-1.,0.,0.)) ;
#19733 = DIRECTION('center_axis',(1.,0.,0.)) ;
#19734 = DIRECTION('ref_axis',(0.,0.,-1.)) ;
#19735 = DIRECTION('',(-1.,0.,0.)) ;
#19736 = DIRECTION('center_axis',(1.,0.,0.)) ;
#19737 = DIRECTION('ref_axis',(0.,0.,-1.)) ;
#19738 = DIRECTION('center_axis',(1.,0.,0.)) ;
#19739 = DIRECTION('ref_axis',(0.,0.,-1.)) ;
#19740 = DIRECTION('center_axis',(1.,0.,0.)) ;
#19741 = DIRECTION('ref_axis',(0.,0.,-1.)) ;
#19742 = DIRECTION('',(-1.,0.,0.)) ;
#19743 = DIRECTION('center_axis',(1.,0.,0.)) ;
#19744 = DIRECTION('ref_axis',(0.,0.,-1.)) ;
#19745 = DIRECTION('',(-1.,0.,0.)) ;
#19746 = DIRECTION('center_axis',(1.,0.,0.)) ;
#19747 = DIRECTION('ref_axis',(0.,0.,-1.)) ;
#19748 = DIRECTION('center_axis',(1.,0.,0.)) ;
#19749 = DIRECTION('ref_axis',(0.,0.,-1.)) ;
#19750 = DIRECTION('',(-1.,0.,0.)) ;
#19751 = DIRECTION('center_axis',(1.,0.,0.)) ;
#19752 = DIRECTION('ref_axis',(0.,0.,-1.)) ;
#19753 = DIRECTION('center_axis',(1.,0.,0.)) ;
#19754 = DIRECTION('ref_axis',(0.,0.,-1.)) ;
#19755 = DIRECTION('center_axis',(-1.,0.,0.)) ;
#19756 = DIRECTION('ref_axis',(0.,0.,1.)) ;
#19757 = DIRECTION('',(-0.258819045102518,-1.18291797137867E-16,-0.965925826289069)) ;
#19758 = DIRECTION('center_axis',(1.,0.,0.)) ;
#19759 = DIRECTION('ref_axis',(0.,0.,-1.)) ;
#19760 = DIRECTION('center_axis',(1.,0.,0.)) ;
#19761 = DIRECTION('ref_axis',(0.,0.,-1.)) ;
#19762 = DIRECTION('center_axis',(1.,0.,0.)) ;
#19763 = DIRECTION('ref_axis',(0.,0.,-1.)) ;
#19764 = DIRECTION('center_axis',(1.,0.,0.)) ;
#19765 = DIRECTION('ref_axis',(0.,0.,-1.)) ;
#19766 = DIRECTION('center_axis',(1.,0.,0.)) ;
#19767 = DIRECTION('ref_axis',(0.,0.,-1.)) ;
#19768 = DIRECTION('',(-0.965925826289059,3.16961915143221E-17,-0.258819045102557)) ;
#19769 = DIRECTION('center_axis',(-1.,0.,0.)) ;
#19770 = DIRECTION('ref_axis',(0.,0.,1.)) ;
#19771 = DIRECTION('',(0.258819045102518,1.18291797137867E-16,0.965925826289069)) ;
#19772 = DIRECTION('center_axis',(1.,0.,0.)) ;
#19773 = DIRECTION('ref_axis',(0.,0.,-1.)) ;
#19774 = DIRECTION('center_axis',(1.,0.,0.)) ;
#19775 = DIRECTION('ref_axis',(0.,0.,-1.)) ;
#19776 = DIRECTION('center_axis',(1.,0.,0.)) ;
#19777 = DIRECTION('ref_axis',(0.,0.,-1.)) ;
#19778 = DIRECTION('center_axis',(1.,0.,0.)) ;
#19779 = DIRECTION('ref_axis',(0.,0.,-1.)) ;
#19780 = DIRECTION('center_axis',(1.,0.,0.)) ;
#19781 = DIRECTION('ref_axis',(0.,0.,-1.)) ;
#19782 = DIRECTION('center_axis',(1.,0.,0.)) ;
#19783 = DIRECTION('ref_axis',(0.,0.,-1.)) ;
#19784 = DIRECTION('center_axis',(1.,0.,0.)) ;
#19785 = DIRECTION('ref_axis',(0.,0.,-1.)) ;
#19786 = DIRECTION('center_axis',(1.,0.,0.)) ;
#19787 = DIRECTION('ref_axis',(0.,0.,-1.)) ;
#19788 = DIRECTION('center_axis',(1.,0.,0.)) ;
#19789 = DIRECTION('ref_axis',(0.,0.,-1.)) ;
#19790 = DIRECTION('center_axis',(1.,0.,0.)) ;
#19791 = DIRECTION('ref_axis',(0.,0.,-1.)) ;
#19792 = DIRECTION('center_axis',(1.,0.,0.)) ;
#19793 = DIRECTION('ref_axis',(0.,0.,-1.)) ;
#19794 = DIRECTION('center_axis',(1.,0.,0.)) ;
#19795 = DIRECTION('ref_axis',(0.,0.,-1.)) ;
#19796 = DIRECTION('center_axis',(1.,0.,0.)) ;
#19797 = DIRECTION('ref_axis',(0.,0.,-1.)) ;
#19798 = DIRECTION('center_axis',(1.,0.,0.)) ;
#19799 = DIRECTION('ref_axis',(0.,0.,-1.)) ;
#19800 = DIRECTION('center_axis',(1.,0.,0.)) ;
#19801 = DIRECTION('ref_axis',(0.,0.,-1.)) ;
#19802 = DIRECTION('center_axis',(1.,0.,0.)) ;
#19803 = DIRECTION('ref_axis',(0.,0.,-1.)) ;
#19804 = DIRECTION('center_axis',(1.,0.,0.)) ;
#19805 = DIRECTION('ref_axis',(0.,0.,-1.)) ;
#19806 = DIRECTION('center_axis',(1.,0.,0.)) ;
#19807 = DIRECTION('ref_axis',(0.,0.,-1.)) ;
#19808 = DIRECTION('center_axis',(1.,0.,0.)) ;
#19809 = DIRECTION('ref_axis',(0.,0.,-1.)) ;
#19810 = DIRECTION('center_axis',(1.,0.,0.)) ;
#19811 = DIRECTION('ref_axis',(0.,0.,-1.)) ;
#19812 = DIRECTION('center_axis',(1.,0.,0.)) ;
#19813 = DIRECTION('ref_axis',(0.,0.,-1.)) ;
#19814 = DIRECTION('center_axis',(1.,0.,0.)) ;
#19815 = DIRECTION('ref_axis',(0.,0.,-1.)) ;
#19816 = DIRECTION('center_axis',(1.,0.,0.)) ;
#19817 = DIRECTION('ref_axis',(0.,0.,-1.)) ;
#19818 = DIRECTION('center_axis',(1.,0.,0.)) ;
#19819 = DIRECTION('ref_axis',(0.,0.,-1.)) ;
#19820 = DIRECTION('center_axis',(1.,0.,0.)) ;
#19821 = DIRECTION('ref_axis',(0.,0.,-1.)) ;
#19822 = DIRECTION('center_axis',(1.,0.,0.)) ;
#19823 = DIRECTION('ref_axis',(0.,0.,-1.)) ;
#19824 = DIRECTION('center_axis',(1.,0.,0.)) ;
#19825 = DIRECTION('ref_axis',(0.,0.,-1.)) ;
#19826 = DIRECTION('center_axis',(1.,0.,0.)) ;
#19827 = DIRECTION('ref_axis',(0.,0.,-1.)) ;
#19828 = DIRECTION('center_axis',(1.,0.,0.)) ;
#19829 = DIRECTION('ref_axis',(0.,0.,-1.)) ;
#19830 = DIRECTION('center_axis',(1.,0.,0.)) ;
#19831 = DIRECTION('ref_axis',(0.,0.,-1.)) ;
#19832 = DIRECTION('center_axis',(1.,0.,0.)) ;
#19833 = DIRECTION('ref_axis',(0.,0.,-1.)) ;
#19834 = DIRECTION('center_axis',(1.,0.,0.)) ;
#19835 = DIRECTION('ref_axis',(0.,0.,-1.)) ;
#19836 = DIRECTION('center_axis',(1.,0.,0.)) ;
#19837 = DIRECTION('ref_axis',(0.,0.,-1.)) ;
#19838 = DIRECTION('center_axis',(1.,0.,0.)) ;
#19839 = DIRECTION('ref_axis',(0.,0.,-1.)) ;
#19840 = DIRECTION('center_axis',(1.,0.,0.)) ;
#19841 = DIRECTION('ref_axis',(0.,0.,-1.)) ;
#19842 = DIRECTION('center_axis',(1.,0.,0.)) ;
#19843 = DIRECTION('ref_axis',(0.,0.,-1.)) ;
#19844 = DIRECTION('center_axis',(1.,0.,0.)) ;
#19845 = DIRECTION('ref_axis',(0.,0.,-1.)) ;
#19846 = DIRECTION('center_axis',(1.,0.,0.)) ;
#19847 = DIRECTION('ref_axis',(0.,0.,-1.)) ;
#19848 = DIRECTION('center_axis',(1.,0.,0.)) ;
#19849 = DIRECTION('ref_axis',(0.,0.,-1.)) ;
#19850 = DIRECTION('center_axis',(1.,0.,0.)) ;
#19851 = DIRECTION('ref_axis',(0.,0.,-1.)) ;
#19852 = DIRECTION('center_axis',(1.,0.,0.)) ;
#19853 = DIRECTION('ref_axis',(0.,0.,-1.)) ;
#19854 = DIRECTION('center_axis',(1.,0.,0.)) ;
#19855 = DIRECTION('ref_axis',(0.,0.,-1.)) ;
#19856 = DIRECTION('center_axis',(1.,0.,0.)) ;
#19857 = DIRECTION('ref_axis',(0.,0.,-1.)) ;
#19858 = DIRECTION('center_axis',(1.,0.,0.)) ;
#19859 = DIRECTION('ref_axis',(0.,0.,-1.)) ;
#19860 = DIRECTION('center_axis',(1.,0.,0.)) ;
#19861 = DIRECTION('ref_axis',(0.,0.,-1.)) ;
#19862 = DIRECTION('center_axis',(1.,0.,0.)) ;
#19863 = DIRECTION('ref_axis',(0.,0.,-1.)) ;
#19864 = DIRECTION('center_axis',(1.,0.,0.)) ;
#19865 = DIRECTION('ref_axis',(0.,0.,-1.)) ;
#19866 = DIRECTION('center_axis',(1.,0.,0.)) ;
#19867 = DIRECTION('ref_axis',(0.,0.,-1.)) ;
#19868 = DIRECTION('center_axis',(1.,0.,0.)) ;
#19869 = DIRECTION('ref_axis',(0.,0.,-1.)) ;
#19870 = DIRECTION('center_axis',(1.,0.,0.)) ;
#19871 = DIRECTION('ref_axis',(0.,0.,-1.)) ;
#19872 = DIRECTION('center_axis',(1.,0.,0.)) ;
#19873 = DIRECTION('ref_axis',(0.,0.,-1.)) ;
#19874 = DIRECTION('center_axis',(1.,0.,0.)) ;
#19875 = DIRECTION('ref_axis',(0.,0.,-1.)) ;
#19876 = DIRECTION('center_axis',(1.,0.,0.)) ;
#19877 = DIRECTION('ref_axis',(0.,0.,-1.)) ;
#19878 = DIRECTION('center_axis',(1.,0.,0.)) ;
#19879 = DIRECTION('ref_axis',(0.,0.,-1.)) ;
#19880 = DIRECTION('center_axis',(1.,0.,0.)) ;
#19881 = DIRECTION('ref_axis',(0.,0.,-1.)) ;
#19882 = DIRECTION('center_axis',(1.,0.,0.)) ;
#19883 = DIRECTION('ref_axis',(0.,0.,-1.)) ;
#19884 = DIRECTION('center_axis',(1.,0.,0.)) ;
#19885 = DIRECTION('ref_axis',(0.,0.,-1.)) ;
#19886 = DIRECTION('center_axis',(1.,0.,0.)) ;
#19887 = DIRECTION('ref_axis',(0.,0.,-1.)) ;
#19888 = DIRECTION('center_axis',(1.,0.,0.)) ;
#19889 = DIRECTION('ref_axis',(0.,0.,-1.)) ;
#19890 = DIRECTION('center_axis',(1.,0.,0.)) ;
#19891 = DIRECTION('ref_axis',(0.,0.,-1.)) ;
#19892 = DIRECTION('center_axis',(1.,0.,0.)) ;
#19893 = DIRECTION('ref_axis',(0.,0.,-1.)) ;
#19894 = DIRECTION('center_axis',(1.,0.,0.)) ;
#19895 = DIRECTION('ref_axis',(0.,0.,-1.)) ;
#19896 = DIRECTION('center_axis',(1.,0.,0.)) ;
#19897 = DIRECTION('ref_axis',(0.,0.,-1.)) ;
#19898 = DIRECTION('center_axis',(1.,0.,0.)) ;
#19899 = DIRECTION('ref_axis',(0.,0.,-1.)) ;
#19900 = DIRECTION('',(-0.258819045102518,1.18291797137867E-16,-0.965925826289069)) ;
#19901 = DIRECTION('center_axis',(1.,0.,0.)) ;
#19902 = DIRECTION('ref_axis',(0.,0.,-1.)) ;
#19903 = DIRECTION('center_axis',(1.,0.,0.)) ;
#19904 = DIRECTION('ref_axis',(0.,0.,-1.)) ;
#19905 = DIRECTION('center_axis',(1.,0.,0.)) ;
#19906 = DIRECTION('ref_axis',(0.,0.,-1.)) ;
#19907 = DIRECTION('center_axis',(1.,0.,0.)) ;
#19908 = DIRECTION('ref_axis',(0.,0.,-1.)) ;
#19909 = DIRECTION('center_axis',(1.,0.,0.)) ;
#19910 = DIRECTION('ref_axis',(0.,0.,-1.)) ;
#19911 = DIRECTION('center_axis',(1.,0.,0.)) ;
#19912 = DIRECTION('ref_axis',(0.,0.,-1.)) ;
#19913 = DIRECTION('center_axis',(1.,0.,0.)) ;
#19914 = DIRECTION('ref_axis',(0.,0.,-1.)) ;
#19915 = DIRECTION('center_axis',(1.,0.,0.)) ;
#19916 = DIRECTION('ref_axis',(0.,0.,-1.)) ;
#19917 = DIRECTION('center_axis',(1.,0.,0.)) ;
#19918 = DIRECTION('ref_axis',(0.,0.,-1.)) ;
#19919 = DIRECTION('center_axis',(1.,0.,0.)) ;
#19920 = DIRECTION('ref_axis',(0.,0.,-1.)) ;
#19921 = DIRECTION('center_axis',(1.,0.,0.)) ;
#19922 = DIRECTION('ref_axis',(0.,0.,-1.)) ;
#19923 = DIRECTION('center_axis',(1.,0.,0.)) ;
#19924 = DIRECTION('ref_axis',(0.,0.,-1.)) ;
#19925 = DIRECTION('center_axis',(1.,0.,0.)) ;
#19926 = DIRECTION('ref_axis',(0.,0.,-1.)) ;
#19927 = DIRECTION('center_axis',(1.,0.,0.)) ;
#19928 = DIRECTION('ref_axis',(0.,0.,-1.)) ;
#19929 = DIRECTION('center_axis',(1.,0.,0.)) ;
#19930 = DIRECTION('ref_axis',(0.,0.,-1.)) ;
#19931 = DIRECTION('center_axis',(1.,0.,0.)) ;
#19932 = DIRECTION('ref_axis',(0.,0.,-1.)) ;
#19933 = DIRECTION('center_axis',(1.,0.,0.)) ;
#19934 = DIRECTION('ref_axis',(0.,0.,-1.)) ;
#19935 = DIRECTION('center_axis',(1.,0.,0.)) ;
#19936 = DIRECTION('ref_axis',(0.,0.,-1.)) ;
#19937 = DIRECTION('center_axis',(1.,0.,0.)) ;
#19938 = DIRECTION('ref_axis',(0.,0.,-1.)) ;
#19939 = DIRECTION('center_axis',(1.,0.,0.)) ;
#19940 = DIRECTION('ref_axis',(0.,0.,-1.)) ;
#19941 = DIRECTION('center_axis',(1.,0.,0.)) ;
#19942 = DIRECTION('ref_axis',(0.,0.,-1.)) ;
#19943 = DIRECTION('center_axis',(1.,0.,0.)) ;
#19944 = DIRECTION('ref_axis',(0.,0.,-1.)) ;
#19945 = DIRECTION('center_axis',(1.,0.,0.)) ;
#19946 = DIRECTION('ref_axis',(0.,0.,-1.)) ;
#19947 = DIRECTION('center_axis',(1.,0.,0.)) ;
#19948 = DIRECTION('ref_axis',(0.,0.,-1.)) ;
#19949 = DIRECTION('center_axis',(1.,0.,0.)) ;
#19950 = DIRECTION('ref_axis',(0.,0.,-1.)) ;
#19951 = DIRECTION('center_axis',(1.,0.,0.)) ;
#19952 = DIRECTION('ref_axis',(0.,0.,-1.)) ;
#19953 = DIRECTION('center_axis',(1.,0.,0.)) ;
#19954 = DIRECTION('ref_axis',(0.,0.,-1.)) ;
#19955 = DIRECTION('center_axis',(1.,0.,0.)) ;
#19956 = DIRECTION('ref_axis',(0.,0.,-1.)) ;
#19957 = DIRECTION('center_axis',(1.,0.,0.)) ;
#19958 = DIRECTION('ref_axis',(0.,0.,-1.)) ;
#19959 = DIRECTION('center_axis',(1.,0.,0.)) ;
#19960 = DIRECTION('ref_axis',(0.,0.,-1.)) ;
#19961 = DIRECTION('center_axis',(1.,0.,0.)) ;
#19962 = DIRECTION('ref_axis',(0.,0.,-1.)) ;
#19963 = DIRECTION('center_axis',(1.,0.,0.)) ;
#19964 = DIRECTION('ref_axis',(0.,0.,-1.)) ;
#19965 = DIRECTION('center_axis',(1.,0.,0.)) ;
#19966 = DIRECTION('ref_axis',(0.,0.,-1.)) ;
#19967 = DIRECTION('center_axis',(1.,0.,0.)) ;
#19968 = DIRECTION('ref_axis',(0.,0.,-1.)) ;
#19969 = DIRECTION('center_axis',(1.,0.,0.)) ;
#19970 = DIRECTION('ref_axis',(0.,0.,-1.)) ;
#19971 = DIRECTION('center_axis',(1.,0.,0.)) ;
#19972 = DIRECTION('ref_axis',(0.,0.,-1.)) ;
#19973 = DIRECTION('center_axis',(1.,0.,0.)) ;
#19974 = DIRECTION('ref_axis',(0.,0.,-1.)) ;
#19975 = DIRECTION('center_axis',(1.,0.,0.)) ;
#19976 = DIRECTION('ref_axis',(0.,0.,-1.)) ;
#19977 = DIRECTION('center_axis',(1.,0.,0.)) ;
#19978 = DIRECTION('ref_axis',(0.,0.,-1.)) ;
#19979 = DIRECTION('center_axis',(1.,0.,0.)) ;
#19980 = DIRECTION('ref_axis',(0.,0.,-1.)) ;
#19981 = DIRECTION('center_axis',(1.,0.,0.)) ;
#19982 = DIRECTION('ref_axis',(0.,0.,-1.)) ;
#19983 = DIRECTION('center_axis',(1.,0.,0.)) ;
#19984 = DIRECTION('ref_axis',(0.,0.,-1.)) ;
#19985 = DIRECTION('center_axis',(1.,0.,0.)) ;
#19986 = DIRECTION('ref_axis',(0.,0.,-1.)) ;
#19987 = DIRECTION('center_axis',(1.,0.,0.)) ;
#19988 = DIRECTION('ref_axis',(0.,0.,-1.)) ;
#19989 = DIRECTION('center_axis',(1.,0.,0.)) ;
#19990 = DIRECTION('ref_axis',(0.,0.,-1.)) ;
#19991 = DIRECTION('center_axis',(1.,0.,0.)) ;
#19992 = DIRECTION('ref_axis',(0.,0.,-1.)) ;
#19993 = DIRECTION('center_axis',(1.,0.,0.)) ;
#19994 = DIRECTION('ref_axis',(0.,0.,-1.)) ;
#19995 = DIRECTION('center_axis',(1.,0.,0.)) ;
#19996 = DIRECTION('ref_axis',(0.,0.,-1.)) ;
#19997 = DIRECTION('center_axis',(1.,0.,0.)) ;
#19998 = DIRECTION('ref_axis',(0.,0.,-1.)) ;
#19999 = DIRECTION('center_axis',(1.,0.,0.)) ;
#20000 = DIRECTION('ref_axis',(0.,0.,-1.)) ;
#20001 = DIRECTION('center_axis',(1.,0.,0.)) ;
#20002 = DIRECTION('ref_axis',(0.,0.,-1.)) ;
#20003 = DIRECTION('center_axis',(1.,0.,0.)) ;
#20004 = DIRECTION('ref_axis',(0.,0.,-1.)) ;
#20005 = DIRECTION('center_axis',(1.,0.,0.)) ;
#20006 = DIRECTION('ref_axis',(0.,0.,-1.)) ;
#20007 = DIRECTION('center_axis',(1.,0.,0.)) ;
#20008 = DIRECTION('ref_axis',(0.,0.,-1.)) ;
#20009 = DIRECTION('center_axis',(1.,0.,0.)) ;
#20010 = DIRECTION('ref_axis',(0.,0.,-1.)) ;
#20011 = DIRECTION('center_axis',(1.,0.,0.)) ;
#20012 = DIRECTION('ref_axis',(0.,0.,-1.)) ;
#20013 = DIRECTION('center_axis',(1.,0.,0.)) ;
#20014 = DIRECTION('ref_axis',(0.,0.,-1.)) ;
#20015 = DIRECTION('center_axis',(1.,0.,0.)) ;
#20016 = DIRECTION('ref_axis',(0.,0.,-1.)) ;
#20017 = DIRECTION('center_axis',(1.,0.,0.)) ;
#20018 = DIRECTION('ref_axis',(0.,0.,-1.)) ;
#20019 = DIRECTION('center_axis',(1.,0.,0.)) ;
#20020 = DIRECTION('ref_axis',(0.,0.,-1.)) ;
#20021 = DIRECTION('center_axis',(1.,0.,0.)) ;
#20022 = DIRECTION('ref_axis',(0.,0.,-1.)) ;
#20023 = DIRECTION('center_axis',(-1.,0.,0.)) ;
#20024 = DIRECTION('ref_axis',(0.,0.,1.)) ;
#20025 = DIRECTION('',(0.965925826289069,3.16961915143174E-17,0.258819045102518)) ;
#20026 = DIRECTION('center_axis',(1.,0.,0.)) ;
#20027 = DIRECTION('ref_axis',(0.,0.,-1.)) ;
#20028 = DIRECTION('center_axis',(1.,0.,0.)) ;
#20029 = DIRECTION('ref_axis',(0.,0.,-1.)) ;
#20030 = DIRECTION('center_axis',(1.,0.,0.)) ;
#20031 = DIRECTION('ref_axis',(0.,0.,-1.)) ;
#20032 = DIRECTION('center_axis',(1.,0.,0.)) ;
#20033 = DIRECTION('ref_axis',(0.,0.,-1.)) ;
#20034 = DIRECTION('',(0.258819045102518,-1.18291797137867E-16,0.965925826289069)) ;
#20035 = DIRECTION('center_axis',(-1.,0.,0.)) ;
#20036 = DIRECTION('ref_axis',(0.,0.,1.)) ;
#20037 = DIRECTION('center_axis',(1.,0.,0.)) ;
#20038 = DIRECTION('ref_axis',(0.,0.,-1.)) ;
#20039 = DIRECTION('center_axis',(1.,0.,0.)) ;
#20040 = DIRECTION('ref_axis',(0.,0.,-1.)) ;
#20041 = DIRECTION('center_axis',(1.,0.,0.)) ;
#20042 = DIRECTION('ref_axis',(0.,0.,-1.)) ;
#20043 = DIRECTION('',(-1.,0.,0.)) ;
#20044 = DIRECTION('center_axis',(-1.,0.,0.)) ;
#20045 = DIRECTION('ref_axis',(0.,0.,1.)) ;
#20046 = DIRECTION('center_axis',(1.,0.,0.)) ;
#20047 = DIRECTION('ref_axis',(0.,0.,-1.)) ;
#20048 = DIRECTION('center_axis',(1.,0.,0.)) ;
#20049 = DIRECTION('ref_axis',(0.,0.,-1.)) ;
#20050 = DIRECTION('center_axis',(1.,0.,0.)) ;
#20051 = DIRECTION('ref_axis',(0.,0.,-1.)) ;
#20052 = DIRECTION('',(-1.,0.,0.)) ;
#20053 = DIRECTION('center_axis',(-1.,0.,0.)) ;
#20054 = DIRECTION('ref_axis',(0.,0.,1.)) ;
#20055 = DIRECTION('center_axis',(1.,0.,0.)) ;
#20056 = DIRECTION('ref_axis',(0.,0.,-1.)) ;
#20057 = DIRECTION('center_axis',(1.,0.,0.)) ;
#20058 = DIRECTION('ref_axis',(0.,0.,-1.)) ;
#20059 = DIRECTION('center_axis',(1.,0.,0.)) ;
#20060 = DIRECTION('ref_axis',(0.,0.,-1.)) ;
#20061 = DIRECTION('center_axis',(1.,0.,0.)) ;
#20062 = DIRECTION('ref_axis',(0.,0.,-1.)) ;
#20063 = DIRECTION('center_axis',(1.,0.,0.)) ;
#20064 = DIRECTION('ref_axis',(0.,0.,-1.)) ;
#20065 = DIRECTION('center_axis',(1.,0.,0.)) ;
#20066 = DIRECTION('ref_axis',(0.,0.,-1.)) ;
#20067 = DIRECTION('center_axis',(1.,0.,0.)) ;
#20068 = DIRECTION('ref_axis',(0.,0.,-1.)) ;
#20069 = DIRECTION('center_axis',(1.,0.,0.)) ;
#20070 = DIRECTION('ref_axis',(0.,0.,-1.)) ;
#20071 = DIRECTION('center_axis',(1.,0.,0.)) ;
#20072 = DIRECTION('ref_axis',(0.,0.,-1.)) ;
#20073 = DIRECTION('center_axis',(-1.,0.,0.)) ;
#20074 = DIRECTION('ref_axis',(0.,0.,1.)) ;
#20075 = DIRECTION('',(-1.,0.,0.)) ;
#20076 = DIRECTION('center_axis',(-1.,0.,0.)) ;
#20077 = DIRECTION('ref_axis',(0.,0.,1.)) ;
#20078 = DIRECTION('',(-1.,0.,0.)) ;
#20079 = DIRECTION('center_axis',(-1.,0.,0.)) ;
#20080 = DIRECTION('ref_axis',(0.,0.,1.)) ;
#20081 = DIRECTION('center_axis',(1.,0.,0.)) ;
#20082 = DIRECTION('ref_axis',(0.,0.104528463267653,-0.994521895368273)) ;
#20083 = DIRECTION('center_axis',(1.,0.,0.)) ;
#20084 = DIRECTION('ref_axis',(0.,0.104528463267653,-0.994521895368273)) ;
#20085 = DIRECTION('center_axis',(1.,0.,0.)) ;
#20086 = DIRECTION('ref_axis',(0.,0.104528463267653,-0.994521895368273)) ;
#20087 = DIRECTION('center_axis',(1.,0.,0.)) ;
#20088 = DIRECTION('ref_axis',(0.,0.104528463267653,-0.994521895368273)) ;
#20089 = DIRECTION('center_axis',(1.,0.,0.)) ;
#20090 = DIRECTION('ref_axis',(0.,0.104528463267653,-0.994521895368273)) ;
#20091 = DIRECTION('center_axis',(1.,0.,0.)) ;
#20092 = DIRECTION('ref_axis',(0.,0.104528463267653,-0.994521895368273)) ;
#20093 = DIRECTION('center_axis',(1.,0.,0.)) ;
#20094 = DIRECTION('ref_axis',(0.,0.104528463267653,-0.994521895368273)) ;
#20095 = DIRECTION('center_axis',(1.,0.,0.)) ;
#20096 = DIRECTION('ref_axis',(0.,0.104528463267653,-0.994521895368273)) ;
#20097 = DIRECTION('center_axis',(-1.,0.,0.)) ;
#20098 = DIRECTION('ref_axis',(0.,-0.104528463267653,0.994521895368273)) ;
#20099 = DIRECTION('',(-1.,0.,0.)) ;
#20100 = DIRECTION('center_axis',(-1.,0.,0.)) ;
#20101 = DIRECTION('ref_axis',(0.,-0.104528463267653,0.994521895368273)) ;
#20102 = DIRECTION('',(-1.,0.,0.)) ;
#20103 = DIRECTION('center_axis',(-1.,0.,0.)) ;
#20104 = DIRECTION('ref_axis',(0.,-0.104528463267653,0.994521895368273)) ;
#20105 = DIRECTION('center_axis',(1.,0.,0.)) ;
#20106 = DIRECTION('ref_axis',(0.,-0.104528463267653,-0.994521895368273)) ;
#20107 = DIRECTION('center_axis',(1.,0.,0.)) ;
#20108 = DIRECTION('ref_axis',(0.,-0.104528463267653,-0.994521895368273)) ;
#20109 = DIRECTION('center_axis',(1.,0.,0.)) ;
#20110 = DIRECTION('ref_axis',(0.,-0.104528463267653,-0.994521895368273)) ;
#20111 = DIRECTION('center_axis',(1.,0.,0.)) ;
#20112 = DIRECTION('ref_axis',(0.,-0.104528463267653,-0.994521895368273)) ;
#20113 = DIRECTION('center_axis',(1.,0.,0.)) ;
#20114 = DIRECTION('ref_axis',(0.,-0.104528463267653,-0.994521895368273)) ;
#20115 = DIRECTION('center_axis',(1.,0.,0.)) ;
#20116 = DIRECTION('ref_axis',(0.,-0.104528463267653,-0.994521895368273)) ;
#20117 = DIRECTION('center_axis',(1.,0.,0.)) ;
#20118 = DIRECTION('ref_axis',(0.,-0.104528463267653,-0.994521895368273)) ;
#20119 = DIRECTION('center_axis',(1.,0.,0.)) ;
#20120 = DIRECTION('ref_axis',(0.,-0.104528463267653,-0.994521895368273)) ;
#20121 = DIRECTION('center_axis',(-1.,0.,0.)) ;
#20122 = DIRECTION('ref_axis',(0.,0.104528463267653,0.994521895368273)) ;
#20123 = DIRECTION('',(-1.,0.,0.)) ;
#20124 = DIRECTION('center_axis',(-1.,0.,0.)) ;
#20125 = DIRECTION('ref_axis',(0.,0.104528463267653,0.994521895368273)) ;
#20126 = DIRECTION('',(-1.,0.,0.)) ;
#20127 = DIRECTION('center_axis',(-1.,0.,0.)) ;
#20128 = DIRECTION('ref_axis',(0.,0.104528463267653,0.994521895368273)) ;
#20129 = DIRECTION('center_axis',(1.,0.,0.)) ;
#20130 = DIRECTION('ref_axis',(0.,-0.207911690817759,-0.978147600733806)) ;
#20131 = DIRECTION('center_axis',(1.,0.,0.)) ;
#20132 = DIRECTION('ref_axis',(0.,-0.207911690817759,-0.978147600733806)) ;
#20133 = DIRECTION('center_axis',(1.,0.,0.)) ;
#20134 = DIRECTION('ref_axis',(0.,-0.207911690817759,-0.978147600733806)) ;
#20135 = DIRECTION('center_axis',(1.,0.,0.)) ;
#20136 = DIRECTION('ref_axis',(0.,-0.207911690817759,-0.978147600733806)) ;
#20137 = DIRECTION('center_axis',(1.,0.,0.)) ;
#20138 = DIRECTION('ref_axis',(0.,-0.207911690817759,-0.978147600733806)) ;
#20139 = DIRECTION('center_axis',(1.,0.,0.)) ;
#20140 = DIRECTION('ref_axis',(0.,-0.207911690817759,-0.978147600733806)) ;
#20141 = DIRECTION('center_axis',(1.,0.,0.)) ;
#20142 = DIRECTION('ref_axis',(0.,-0.207911690817759,-0.978147600733806)) ;
#20143 = DIRECTION('center_axis',(1.,0.,0.)) ;
#20144 = DIRECTION('ref_axis',(0.,-0.207911690817759,-0.978147600733806)) ;
#20145 = DIRECTION('center_axis',(-1.,0.,0.)) ;
#20146 = DIRECTION('ref_axis',(0.,0.207911690817759,0.978147600733806)) ;
#20147 = DIRECTION('',(-1.,0.,0.)) ;
#20148 = DIRECTION('center_axis',(-1.,0.,0.)) ;
#20149 = DIRECTION('ref_axis',(0.,0.207911690817759,0.978147600733806)) ;
#20150 = DIRECTION('',(-1.,0.,0.)) ;
#20151 = DIRECTION('center_axis',(-1.,0.,0.)) ;
#20152 = DIRECTION('ref_axis',(0.,0.207911690817759,0.978147600733806)) ;
#20153 = DIRECTION('center_axis',(1.,0.,0.)) ;
#20154 = DIRECTION('ref_axis',(0.,-0.309016994374947,-0.951056516295154)) ;
#20155 = DIRECTION('center_axis',(1.,0.,0.)) ;
#20156 = DIRECTION('ref_axis',(0.,-0.309016994374947,-0.951056516295154)) ;
#20157 = DIRECTION('center_axis',(1.,0.,0.)) ;
#20158 = DIRECTION('ref_axis',(0.,-0.309016994374947,-0.951056516295154)) ;
#20159 = DIRECTION('center_axis',(1.,0.,0.)) ;
#20160 = DIRECTION('ref_axis',(0.,-0.309016994374947,-0.951056516295154)) ;
#20161 = DIRECTION('center_axis',(1.,0.,0.)) ;
#20162 = DIRECTION('ref_axis',(0.,-0.309016994374947,-0.951056516295154)) ;
#20163 = DIRECTION('center_axis',(1.,0.,0.)) ;
#20164 = DIRECTION('ref_axis',(0.,-0.309016994374947,-0.951056516295154)) ;
#20165 = DIRECTION('center_axis',(1.,0.,0.)) ;
#20166 = DIRECTION('ref_axis',(0.,-0.309016994374947,-0.951056516295154)) ;
#20167 = DIRECTION('center_axis',(1.,0.,0.)) ;
#20168 = DIRECTION('ref_axis',(0.,-0.309016994374947,-0.951056516295154)) ;
#20169 = DIRECTION('center_axis',(-1.,0.,0.)) ;
#20170 = DIRECTION('ref_axis',(0.,0.309016994374947,0.951056516295154)) ;
#20171 = DIRECTION('',(-1.,0.,0.)) ;
#20172 = DIRECTION('center_axis',(-1.,0.,0.)) ;
#20173 = DIRECTION('ref_axis',(0.,0.309016994374947,0.951056516295154)) ;
#20174 = DIRECTION('',(-1.,0.,0.)) ;
#20175 = DIRECTION('center_axis',(-1.,0.,0.)) ;
#20176 = DIRECTION('ref_axis',(0.,0.309016994374947,0.951056516295154)) ;
#20177 = DIRECTION('center_axis',(1.,0.,0.)) ;
#20178 = DIRECTION('ref_axis',(0.,-0.4067366430758,-0.913545457642601)) ;
#20179 = DIRECTION('center_axis',(1.,0.,0.)) ;
#20180 = DIRECTION('ref_axis',(0.,-0.4067366430758,-0.913545457642601)) ;
#20181 = DIRECTION('center_axis',(1.,0.,0.)) ;
#20182 = DIRECTION('ref_axis',(0.,-0.4067366430758,-0.913545457642601)) ;
#20183 = DIRECTION('center_axis',(1.,0.,0.)) ;
#20184 = DIRECTION('ref_axis',(0.,-0.4067366430758,-0.913545457642601)) ;
#20185 = DIRECTION('center_axis',(1.,0.,0.)) ;
#20186 = DIRECTION('ref_axis',(0.,-0.4067366430758,-0.913545457642601)) ;
#20187 = DIRECTION('center_axis',(1.,0.,0.)) ;
#20188 = DIRECTION('ref_axis',(0.,-0.4067366430758,-0.913545457642601)) ;
#20189 = DIRECTION('center_axis',(1.,0.,0.)) ;
#20190 = DIRECTION('ref_axis',(0.,-0.4067366430758,-0.913545457642601)) ;
#20191 = DIRECTION('center_axis',(1.,0.,0.)) ;
#20192 = DIRECTION('ref_axis',(0.,-0.4067366430758,-0.913545457642601)) ;
#20193 = DIRECTION('center_axis',(-1.,0.,0.)) ;
#20194 = DIRECTION('ref_axis',(0.,0.4067366430758,0.913545457642601)) ;
#20195 = DIRECTION('',(-1.,0.,0.)) ;
#20196 = DIRECTION('center_axis',(-1.,0.,0.)) ;
#20197 = DIRECTION('ref_axis',(0.,0.4067366430758,0.913545457642601)) ;
#20198 = DIRECTION('',(-1.,0.,0.)) ;
#20199 = DIRECTION('center_axis',(-1.,0.,0.)) ;
#20200 = DIRECTION('ref_axis',(0.,0.4067366430758,0.913545457642601)) ;
#20201 = DIRECTION('center_axis',(1.,0.,0.)) ;
#20202 = DIRECTION('ref_axis',(0.,-0.5,-0.866025403784439)) ;
#20203 = DIRECTION('center_axis',(1.,0.,0.)) ;
#20204 = DIRECTION('ref_axis',(0.,-0.5,-0.866025403784439)) ;
#20205 = DIRECTION('center_axis',(1.,0.,0.)) ;
#20206 = DIRECTION('ref_axis',(0.,-0.5,-0.866025403784439)) ;
#20207 = DIRECTION('center_axis',(1.,0.,0.)) ;
#20208 = DIRECTION('ref_axis',(0.,-0.5,-0.866025403784439)) ;
#20209 = DIRECTION('center_axis',(1.,0.,0.)) ;
#20210 = DIRECTION('ref_axis',(0.,-0.5,-0.866025403784439)) ;
#20211 = DIRECTION('center_axis',(1.,0.,0.)) ;
#20212 = DIRECTION('ref_axis',(0.,-0.5,-0.866025403784439)) ;
#20213 = DIRECTION('center_axis',(1.,0.,0.)) ;
#20214 = DIRECTION('ref_axis',(0.,-0.5,-0.866025403784439)) ;
#20215 = DIRECTION('center_axis',(1.,0.,0.)) ;
#20216 = DIRECTION('ref_axis',(0.,-0.5,-0.866025403784439)) ;
#20217 = DIRECTION('center_axis',(-1.,0.,0.)) ;
#20218 = DIRECTION('ref_axis',(0.,0.5,0.866025403784439)) ;
#20219 = DIRECTION('',(-1.,0.,0.)) ;
#20220 = DIRECTION('center_axis',(-1.,0.,0.)) ;
#20221 = DIRECTION('ref_axis',(0.,0.5,0.866025403784439)) ;
#20222 = DIRECTION('',(-1.,0.,0.)) ;
#20223 = DIRECTION('center_axis',(-1.,0.,0.)) ;
#20224 = DIRECTION('ref_axis',(0.,0.5,0.866025403784439)) ;
#20225 = DIRECTION('center_axis',(1.,0.,0.)) ;
#20226 = DIRECTION('ref_axis',(0.,-0.587785252292473,-0.809016994374947)) ;
#20227 = DIRECTION('center_axis',(1.,0.,0.)) ;
#20228 = DIRECTION('ref_axis',(0.,-0.587785252292473,-0.809016994374947)) ;
#20229 = DIRECTION('center_axis',(1.,0.,0.)) ;
#20230 = DIRECTION('ref_axis',(0.,-0.587785252292473,-0.809016994374947)) ;
#20231 = DIRECTION('center_axis',(1.,0.,0.)) ;
#20232 = DIRECTION('ref_axis',(0.,-0.587785252292473,-0.809016994374947)) ;
#20233 = DIRECTION('center_axis',(1.,0.,0.)) ;
#20234 = DIRECTION('ref_axis',(0.,-0.587785252292473,-0.809016994374947)) ;
#20235 = DIRECTION('center_axis',(1.,0.,0.)) ;
#20236 = DIRECTION('ref_axis',(0.,-0.587785252292473,-0.809016994374947)) ;
#20237 = DIRECTION('center_axis',(1.,0.,0.)) ;
#20238 = DIRECTION('ref_axis',(0.,-0.587785252292473,-0.809016994374947)) ;
#20239 = DIRECTION('center_axis',(1.,0.,0.)) ;
#20240 = DIRECTION('ref_axis',(0.,-0.587785252292473,-0.809016994374947)) ;
#20241 = DIRECTION('center_axis',(-1.,0.,0.)) ;
#20242 = DIRECTION('ref_axis',(0.,0.587785252292473,0.809016994374947)) ;
#20243 = DIRECTION('',(-1.,0.,0.)) ;
#20244 = DIRECTION('center_axis',(-1.,0.,0.)) ;
#20245 = DIRECTION('ref_axis',(0.,0.587785252292473,0.809016994374947)) ;
#20246 = DIRECTION('',(-1.,0.,0.)) ;
#20247 = DIRECTION('center_axis',(-1.,0.,0.)) ;
#20248 = DIRECTION('ref_axis',(0.,0.587785252292473,0.809016994374947)) ;
#20249 = DIRECTION('center_axis',(1.,0.,0.)) ;
#20250 = DIRECTION('ref_axis',(0.,-0.743144825477394,-0.669130606358858)) ;
#20251 = DIRECTION('center_axis',(1.,0.,0.)) ;
#20252 = DIRECTION('ref_axis',(0.,-0.743144825477394,-0.669130606358858)) ;
#20253 = DIRECTION('center_axis',(1.,0.,0.)) ;
#20254 = DIRECTION('ref_axis',(0.,-0.743144825477394,-0.669130606358858)) ;
#20255 = DIRECTION('center_axis',(1.,0.,0.)) ;
#20256 = DIRECTION('ref_axis',(0.,-0.743144825477394,-0.669130606358858)) ;
#20257 = DIRECTION('center_axis',(1.,0.,0.)) ;
#20258 = DIRECTION('ref_axis',(0.,-0.743144825477394,-0.669130606358858)) ;
#20259 = DIRECTION('center_axis',(1.,0.,0.)) ;
#20260 = DIRECTION('ref_axis',(0.,-0.743144825477394,-0.669130606358858)) ;
#20261 = DIRECTION('center_axis',(1.,0.,0.)) ;
#20262 = DIRECTION('ref_axis',(0.,-0.743144825477394,-0.669130606358858)) ;
#20263 = DIRECTION('center_axis',(1.,0.,0.)) ;
#20264 = DIRECTION('ref_axis',(0.,-0.743144825477394,-0.669130606358858)) ;
#20265 = DIRECTION('center_axis',(-1.,0.,0.)) ;
#20266 = DIRECTION('ref_axis',(0.,0.743144825477394,0.669130606358858)) ;
#20267 = DIRECTION('',(-1.,0.,0.)) ;
#20268 = DIRECTION('center_axis',(-1.,0.,0.)) ;
#20269 = DIRECTION('ref_axis',(0.,0.743144825477394,0.669130606358858)) ;
#20270 = DIRECTION('',(-1.,0.,0.)) ;
#20271 = DIRECTION('center_axis',(-1.,0.,0.)) ;
#20272 = DIRECTION('ref_axis',(0.,0.743144825477394,0.669130606358858)) ;
#20273 = DIRECTION('center_axis',(1.,0.,0.)) ;
#20274 = DIRECTION('ref_axis',(0.,-0.669130606358858,-0.743144825477394)) ;
#20275 = DIRECTION('center_axis',(1.,0.,0.)) ;
#20276 = DIRECTION('ref_axis',(0.,-0.669130606358858,-0.743144825477394)) ;
#20277 = DIRECTION('center_axis',(1.,0.,0.)) ;
#20278 = DIRECTION('ref_axis',(0.,-0.669130606358858,-0.743144825477394)) ;
#20279 = DIRECTION('center_axis',(1.,0.,0.)) ;
#20280 = DIRECTION('ref_axis',(0.,-0.669130606358858,-0.743144825477394)) ;
#20281 = DIRECTION('center_axis',(1.,0.,0.)) ;
#20282 = DIRECTION('ref_axis',(0.,-0.669130606358858,-0.743144825477394)) ;
#20283 = DIRECTION('center_axis',(1.,0.,0.)) ;
#20284 = DIRECTION('ref_axis',(0.,-0.669130606358858,-0.743144825477394)) ;
#20285 = DIRECTION('center_axis',(1.,0.,0.)) ;
#20286 = DIRECTION('ref_axis',(0.,-0.669130606358858,-0.743144825477394)) ;
#20287 = DIRECTION('center_axis',(1.,0.,0.)) ;
#20288 = DIRECTION('ref_axis',(0.,-0.669130606358858,-0.743144825477394)) ;
#20289 = DIRECTION('center_axis',(-1.,0.,0.)) ;
#20290 = DIRECTION('ref_axis',(0.,0.669130606358858,0.743144825477394)) ;
#20291 = DIRECTION('',(-1.,0.,0.)) ;
#20292 = DIRECTION('center_axis',(-1.,0.,0.)) ;
#20293 = DIRECTION('ref_axis',(0.,0.669130606358858,0.743144825477394)) ;
#20294 = DIRECTION('',(-1.,0.,0.)) ;
#20295 = DIRECTION('center_axis',(-1.,0.,0.)) ;
#20296 = DIRECTION('ref_axis',(0.,0.669130606358858,0.743144825477394)) ;
#20297 = DIRECTION('center_axis',(1.,0.,0.)) ;
#20298 = DIRECTION('ref_axis',(0.,-0.809016994374947,-0.587785252292473)) ;
#20299 = DIRECTION('center_axis',(1.,0.,0.)) ;
#20300 = DIRECTION('ref_axis',(0.,-0.809016994374947,-0.587785252292473)) ;
#20301 = DIRECTION('center_axis',(1.,0.,0.)) ;
#20302 = DIRECTION('ref_axis',(0.,-0.809016994374947,-0.587785252292473)) ;
#20303 = DIRECTION('center_axis',(1.,0.,0.)) ;
#20304 = DIRECTION('ref_axis',(0.,-0.809016994374947,-0.587785252292473)) ;
#20305 = DIRECTION('center_axis',(1.,0.,0.)) ;
#20306 = DIRECTION('ref_axis',(0.,-0.809016994374947,-0.587785252292473)) ;
#20307 = DIRECTION('center_axis',(1.,0.,0.)) ;
#20308 = DIRECTION('ref_axis',(0.,-0.809016994374947,-0.587785252292473)) ;
#20309 = DIRECTION('center_axis',(1.,0.,0.)) ;
#20310 = DIRECTION('ref_axis',(0.,-0.809016994374947,-0.587785252292473)) ;
#20311 = DIRECTION('center_axis',(1.,0.,0.)) ;
#20312 = DIRECTION('ref_axis',(0.,-0.809016994374947,-0.587785252292473)) ;
#20313 = DIRECTION('center_axis',(-1.,0.,0.)) ;
#20314 = DIRECTION('ref_axis',(0.,0.809016994374947,0.587785252292473)) ;
#20315 = DIRECTION('',(-1.,0.,0.)) ;
#20316 = DIRECTION('center_axis',(-1.,0.,0.)) ;
#20317 = DIRECTION('ref_axis',(0.,0.809016994374947,0.587785252292473)) ;
#20318 = DIRECTION('',(-1.,0.,0.)) ;
#20319 = DIRECTION('center_axis',(-1.,0.,0.)) ;
#20320 = DIRECTION('ref_axis',(0.,0.809016994374947,0.587785252292473)) ;
#20321 = DIRECTION('center_axis',(1.,0.,0.)) ;
#20322 = DIRECTION('ref_axis',(0.,-0.866025403784439,-0.5)) ;
#20323 = DIRECTION('center_axis',(1.,0.,0.)) ;
#20324 = DIRECTION('ref_axis',(0.,-0.866025403784439,-0.5)) ;
#20325 = DIRECTION('center_axis',(1.,0.,0.)) ;
#20326 = DIRECTION('ref_axis',(0.,-0.866025403784439,-0.5)) ;
#20327 = DIRECTION('center_axis',(1.,0.,0.)) ;
#20328 = DIRECTION('ref_axis',(0.,-0.866025403784439,-0.5)) ;
#20329 = DIRECTION('center_axis',(1.,0.,0.)) ;
#20330 = DIRECTION('ref_axis',(0.,-0.866025403784439,-0.5)) ;
#20331 = DIRECTION('center_axis',(1.,0.,0.)) ;
#20332 = DIRECTION('ref_axis',(0.,-0.866025403784439,-0.5)) ;
#20333 = DIRECTION('center_axis',(1.,0.,0.)) ;
#20334 = DIRECTION('ref_axis',(0.,-0.866025403784439,-0.5)) ;
#20335 = DIRECTION('center_axis',(1.,0.,0.)) ;
#20336 = DIRECTION('ref_axis',(0.,-0.866025403784439,-0.5)) ;
#20337 = DIRECTION('center_axis',(-1.,0.,0.)) ;
#20338 = DIRECTION('ref_axis',(0.,0.866025403784439,0.5)) ;
#20339 = DIRECTION('',(-1.,0.,0.)) ;
#20340 = DIRECTION('center_axis',(-1.,0.,0.)) ;
#20341 = DIRECTION('ref_axis',(0.,0.866025403784439,0.5)) ;
#20342 = DIRECTION('',(-1.,0.,0.)) ;
#20343 = DIRECTION('center_axis',(-1.,0.,0.)) ;
#20344 = DIRECTION('ref_axis',(0.,0.866025403784439,0.5)) ;
#20345 = DIRECTION('center_axis',(1.,0.,0.)) ;
#20346 = DIRECTION('ref_axis',(0.,-0.913545457642601,-0.4067366430758)) ;
#20347 = DIRECTION('center_axis',(1.,0.,0.)) ;
#20348 = DIRECTION('ref_axis',(0.,-0.913545457642601,-0.4067366430758)) ;
#20349 = DIRECTION('center_axis',(1.,0.,0.)) ;
#20350 = DIRECTION('ref_axis',(0.,-0.913545457642601,-0.4067366430758)) ;
#20351 = DIRECTION('center_axis',(1.,0.,0.)) ;
#20352 = DIRECTION('ref_axis',(0.,-0.913545457642601,-0.4067366430758)) ;
#20353 = DIRECTION('center_axis',(1.,0.,0.)) ;
#20354 = DIRECTION('ref_axis',(0.,-0.913545457642601,-0.4067366430758)) ;
#20355 = DIRECTION('center_axis',(1.,0.,0.)) ;
#20356 = DIRECTION('ref_axis',(0.,-0.913545457642601,-0.4067366430758)) ;
#20357 = DIRECTION('center_axis',(1.,0.,0.)) ;
#20358 = DIRECTION('ref_axis',(0.,-0.913545457642601,-0.4067366430758)) ;
#20359 = DIRECTION('center_axis',(1.,0.,0.)) ;
#20360 = DIRECTION('ref_axis',(0.,-0.913545457642601,-0.4067366430758)) ;
#20361 = DIRECTION('center_axis',(-1.,0.,0.)) ;
#20362 = DIRECTION('ref_axis',(0.,0.913545457642601,0.4067366430758)) ;
#20363 = DIRECTION('',(-1.,0.,0.)) ;
#20364 = DIRECTION('center_axis',(-1.,0.,0.)) ;
#20365 = DIRECTION('ref_axis',(0.,0.913545457642601,0.4067366430758)) ;
#20366 = DIRECTION('',(-1.,0.,0.)) ;
#20367 = DIRECTION('center_axis',(-1.,0.,0.)) ;
#20368 = DIRECTION('ref_axis',(0.,0.913545457642601,0.4067366430758)) ;
#20369 = DIRECTION('center_axis',(1.,0.,0.)) ;
#20370 = DIRECTION('ref_axis',(0.,-0.951056516295154,-0.309016994374947)) ;
#20371 = DIRECTION('center_axis',(1.,0.,0.)) ;
#20372 = DIRECTION('ref_axis',(0.,-0.951056516295154,-0.309016994374947)) ;
#20373 = DIRECTION('center_axis',(1.,0.,0.)) ;
#20374 = DIRECTION('ref_axis',(0.,-0.951056516295154,-0.309016994374947)) ;
#20375 = DIRECTION('center_axis',(1.,0.,0.)) ;
#20376 = DIRECTION('ref_axis',(0.,-0.951056516295154,-0.309016994374947)) ;
#20377 = DIRECTION('center_axis',(1.,0.,0.)) ;
#20378 = DIRECTION('ref_axis',(0.,-0.951056516295154,-0.309016994374947)) ;
#20379 = DIRECTION('center_axis',(1.,0.,0.)) ;
#20380 = DIRECTION('ref_axis',(0.,-0.951056516295154,-0.309016994374947)) ;
#20381 = DIRECTION('center_axis',(1.,0.,0.)) ;
#20382 = DIRECTION('ref_axis',(0.,-0.951056516295154,-0.309016994374947)) ;
#20383 = DIRECTION('center_axis',(1.,0.,0.)) ;
#20384 = DIRECTION('ref_axis',(0.,-0.951056516295154,-0.309016994374947)) ;
#20385 = DIRECTION('center_axis',(-1.,0.,0.)) ;
#20386 = DIRECTION('ref_axis',(0.,0.951056516295154,0.309016994374947)) ;
#20387 = DIRECTION('',(-1.,0.,0.)) ;
#20388 = DIRECTION('center_axis',(-1.,0.,0.)) ;
#20389 = DIRECTION('ref_axis',(0.,0.951056516295154,0.309016994374947)) ;
#20390 = DIRECTION('',(-1.,0.,0.)) ;
#20391 = DIRECTION('center_axis',(-1.,0.,0.)) ;
#20392 = DIRECTION('ref_axis',(0.,0.951056516295154,0.309016994374947)) ;
#20393 = DIRECTION('center_axis',(1.,0.,0.)) ;
#20394 = DIRECTION('ref_axis',(0.,-0.978147600733806,-0.207911690817759)) ;
#20395 = DIRECTION('center_axis',(1.,0.,0.)) ;
#20396 = DIRECTION('ref_axis',(0.,-0.978147600733806,-0.207911690817759)) ;
#20397 = DIRECTION('center_axis',(1.,0.,0.)) ;
#20398 = DIRECTION('ref_axis',(0.,-0.978147600733806,-0.207911690817759)) ;
#20399 = DIRECTION('center_axis',(1.,0.,0.)) ;
#20400 = DIRECTION('ref_axis',(0.,-0.978147600733806,-0.207911690817759)) ;
#20401 = DIRECTION('center_axis',(1.,0.,0.)) ;
#20402 = DIRECTION('ref_axis',(0.,-0.978147600733806,-0.207911690817759)) ;
#20403 = DIRECTION('center_axis',(1.,0.,0.)) ;
#20404 = DIRECTION('ref_axis',(0.,-0.978147600733806,-0.207911690817759)) ;
#20405 = DIRECTION('center_axis',(1.,0.,0.)) ;
#20406 = DIRECTION('ref_axis',(0.,-0.978147600733806,-0.207911690817759)) ;
#20407 = DIRECTION('center_axis',(1.,0.,0.)) ;
#20408 = DIRECTION('ref_axis',(0.,-0.978147600733806,-0.207911690817759)) ;
#20409 = DIRECTION('center_axis',(-1.,0.,0.)) ;
#20410 = DIRECTION('ref_axis',(0.,0.978147600733806,0.207911690817759)) ;
#20411 = DIRECTION('',(-1.,0.,0.)) ;
#20412 = DIRECTION('center_axis',(-1.,0.,0.)) ;
#20413 = DIRECTION('ref_axis',(0.,0.978147600733806,0.207911690817759)) ;
#20414 = DIRECTION('',(-1.,0.,0.)) ;
#20415 = DIRECTION('center_axis',(-1.,0.,0.)) ;
#20416 = DIRECTION('ref_axis',(0.,0.978147600733806,0.207911690817759)) ;
#20417 = DIRECTION('center_axis',(1.,0.,0.)) ;
#20418 = DIRECTION('ref_axis',(0.,-0.994521895368273,-0.104528463267653)) ;
#20419 = DIRECTION('center_axis',(1.,0.,0.)) ;
#20420 = DIRECTION('ref_axis',(0.,-0.994521895368273,-0.104528463267653)) ;
#20421 = DIRECTION('center_axis',(1.,0.,0.)) ;
#20422 = DIRECTION('ref_axis',(0.,-0.994521895368273,-0.104528463267653)) ;
#20423 = DIRECTION('center_axis',(1.,0.,0.)) ;
#20424 = DIRECTION('ref_axis',(0.,-0.994521895368273,-0.104528463267653)) ;
#20425 = DIRECTION('center_axis',(1.,0.,0.)) ;
#20426 = DIRECTION('ref_axis',(0.,-0.994521895368273,-0.104528463267653)) ;
#20427 = DIRECTION('center_axis',(1.,0.,0.)) ;
#20428 = DIRECTION('ref_axis',(0.,-0.994521895368273,-0.104528463267653)) ;
#20429 = DIRECTION('center_axis',(1.,0.,0.)) ;
#20430 = DIRECTION('ref_axis',(0.,-0.994521895368273,-0.104528463267653)) ;
#20431 = DIRECTION('center_axis',(1.,0.,0.)) ;
#20432 = DIRECTION('ref_axis',(0.,-0.994521895368273,-0.104528463267653)) ;
#20433 = DIRECTION('center_axis',(-1.,0.,0.)) ;
#20434 = DIRECTION('ref_axis',(0.,0.994521895368273,0.104528463267653)) ;
#20435 = DIRECTION('',(-1.,0.,0.)) ;
#20436 = DIRECTION('center_axis',(-1.,0.,0.)) ;
#20437 = DIRECTION('ref_axis',(0.,0.994521895368273,0.104528463267653)) ;
#20438 = DIRECTION('',(-1.,0.,0.)) ;
#20439 = DIRECTION('center_axis',(-1.,0.,0.)) ;
#20440 = DIRECTION('ref_axis',(0.,0.994521895368273,0.104528463267653)) ;
#20441 = DIRECTION('center_axis',(1.,0.,0.)) ;
#20442 = DIRECTION('ref_axis',(0.,-1.,1.83697019872103E-16)) ;
#20443 = DIRECTION('center_axis',(1.,0.,0.)) ;
#20444 = DIRECTION('ref_axis',(0.,-1.,1.83697019872103E-16)) ;
#20445 = DIRECTION('center_axis',(1.,0.,0.)) ;
#20446 = DIRECTION('ref_axis',(0.,-1.,1.83697019872103E-16)) ;
#20447 = DIRECTION('center_axis',(1.,0.,0.)) ;
#20448 = DIRECTION('ref_axis',(0.,-1.,1.83697019872103E-16)) ;
#20449 = DIRECTION('center_axis',(1.,0.,0.)) ;
#20450 = DIRECTION('ref_axis',(0.,-1.,1.83697019872103E-16)) ;
#20451 = DIRECTION('center_axis',(1.,0.,0.)) ;
#20452 = DIRECTION('ref_axis',(0.,-1.,1.83697019872103E-16)) ;
#20453 = DIRECTION('center_axis',(1.,0.,0.)) ;
#20454 = DIRECTION('ref_axis',(0.,-1.,1.83697019872103E-16)) ;
#20455 = DIRECTION('center_axis',(1.,0.,0.)) ;
#20456 = DIRECTION('ref_axis',(0.,-1.,1.83697019872103E-16)) ;
#20457 = DIRECTION('center_axis',(-1.,0.,0.)) ;
#20458 = DIRECTION('ref_axis',(0.,1.,-1.83697019872103E-16)) ;
#20459 = DIRECTION('',(-1.,0.,0.)) ;
#20460 = DIRECTION('center_axis',(-1.,0.,0.)) ;
#20461 = DIRECTION('ref_axis',(0.,1.,-1.83697019872103E-16)) ;
#20462 = DIRECTION('',(-1.,0.,0.)) ;
#20463 = DIRECTION('center_axis',(-1.,0.,0.)) ;
#20464 = DIRECTION('ref_axis',(0.,1.,-1.83697019872103E-16)) ;
#20465 = DIRECTION('center_axis',(1.,0.,0.)) ;
#20466 = DIRECTION('ref_axis',(0.,-0.994521895368273,0.104528463267653)) ;
#20467 = DIRECTION('center_axis',(1.,0.,0.)) ;
#20468 = DIRECTION('ref_axis',(0.,-0.994521895368273,0.104528463267653)) ;
#20469 = DIRECTION('center_axis',(1.,0.,0.)) ;
#20470 = DIRECTION('ref_axis',(0.,-0.994521895368273,0.104528463267653)) ;
#20471 = DIRECTION('center_axis',(1.,0.,0.)) ;
#20472 = DIRECTION('ref_axis',(0.,-0.994521895368273,0.104528463267653)) ;
#20473 = DIRECTION('center_axis',(1.,0.,0.)) ;
#20474 = DIRECTION('ref_axis',(0.,-0.994521895368273,0.104528463267653)) ;
#20475 = DIRECTION('center_axis',(1.,0.,0.)) ;
#20476 = DIRECTION('ref_axis',(0.,-0.994521895368273,0.104528463267653)) ;
#20477 = DIRECTION('center_axis',(1.,0.,0.)) ;
#20478 = DIRECTION('ref_axis',(0.,-0.994521895368273,0.104528463267653)) ;
#20479 = DIRECTION('center_axis',(1.,0.,0.)) ;
#20480 = DIRECTION('ref_axis',(0.,-0.994521895368273,0.104528463267653)) ;
#20481 = DIRECTION('center_axis',(-1.,0.,0.)) ;
#20482 = DIRECTION('ref_axis',(0.,0.994521895368273,-0.104528463267653)) ;
#20483 = DIRECTION('',(-1.,0.,0.)) ;
#20484 = DIRECTION('center_axis',(-1.,0.,0.)) ;
#20485 = DIRECTION('ref_axis',(0.,0.994521895368273,-0.104528463267653)) ;
#20486 = DIRECTION('',(-1.,0.,0.)) ;
#20487 = DIRECTION('center_axis',(-1.,0.,0.)) ;
#20488 = DIRECTION('ref_axis',(0.,0.994521895368273,-0.104528463267653)) ;
#20489 = DIRECTION('center_axis',(1.,0.,0.)) ;
#20490 = DIRECTION('ref_axis',(0.,-0.978147600733805,0.20791169081776)) ;
#20491 = DIRECTION('center_axis',(1.,0.,0.)) ;
#20492 = DIRECTION('ref_axis',(0.,-0.978147600733805,0.20791169081776)) ;
#20493 = DIRECTION('center_axis',(1.,0.,0.)) ;
#20494 = DIRECTION('ref_axis',(0.,-0.978147600733805,0.20791169081776)) ;
#20495 = DIRECTION('center_axis',(1.,0.,0.)) ;
#20496 = DIRECTION('ref_axis',(0.,-0.978147600733805,0.20791169081776)) ;
#20497 = DIRECTION('center_axis',(1.,0.,0.)) ;
#20498 = DIRECTION('ref_axis',(0.,-0.978147600733805,0.20791169081776)) ;
#20499 = DIRECTION('center_axis',(1.,0.,0.)) ;
#20500 = DIRECTION('ref_axis',(0.,-0.978147600733805,0.20791169081776)) ;
#20501 = DIRECTION('center_axis',(1.,0.,0.)) ;
#20502 = DIRECTION('ref_axis',(0.,-0.978147600733805,0.20791169081776)) ;
#20503 = DIRECTION('center_axis',(1.,0.,0.)) ;
#20504 = DIRECTION('ref_axis',(0.,-0.978147600733805,0.20791169081776)) ;
#20505 = DIRECTION('center_axis',(-1.,0.,0.)) ;
#20506 = DIRECTION('ref_axis',(0.,0.978147600733805,-0.20791169081776)) ;
#20507 = DIRECTION('',(-1.,0.,0.)) ;
#20508 = DIRECTION('center_axis',(-1.,0.,0.)) ;
#20509 = DIRECTION('ref_axis',(0.,0.978147600733805,-0.20791169081776)) ;
#20510 = DIRECTION('',(-1.,0.,0.)) ;
#20511 = DIRECTION('center_axis',(-1.,0.,0.)) ;
#20512 = DIRECTION('ref_axis',(0.,0.978147600733805,-0.20791169081776)) ;
#20513 = DIRECTION('center_axis',(1.,0.,0.)) ;
#20514 = DIRECTION('ref_axis',(0.,-0.951056516295154,0.309016994374948)) ;
#20515 = DIRECTION('center_axis',(1.,0.,0.)) ;
#20516 = DIRECTION('ref_axis',(0.,-0.951056516295153,0.309016994374948)) ;
#20517 = DIRECTION('center_axis',(1.,0.,0.)) ;
#20518 = DIRECTION('ref_axis',(0.,-0.951056516295154,0.309016994374948)) ;
#20519 = DIRECTION('center_axis',(1.,0.,0.)) ;
#20520 = DIRECTION('ref_axis',(0.,-0.951056516295153,0.309016994374948)) ;
#20521 = DIRECTION('center_axis',(1.,0.,0.)) ;
#20522 = DIRECTION('ref_axis',(0.,-0.951056516295154,0.309016994374948)) ;
#20523 = DIRECTION('center_axis',(1.,0.,0.)) ;
#20524 = DIRECTION('ref_axis',(0.,-0.951056516295153,0.309016994374948)) ;
#20525 = DIRECTION('center_axis',(1.,0.,0.)) ;
#20526 = DIRECTION('ref_axis',(0.,-0.951056516295154,0.309016994374948)) ;
#20527 = DIRECTION('center_axis',(1.,0.,0.)) ;
#20528 = DIRECTION('ref_axis',(0.,-0.951056516295153,0.309016994374948)) ;
#20529 = DIRECTION('center_axis',(-1.,0.,0.)) ;
#20530 = DIRECTION('ref_axis',(0.,0.951056516295153,-0.309016994374948)) ;
#20531 = DIRECTION('',(-1.,0.,0.)) ;
#20532 = DIRECTION('center_axis',(-1.,0.,0.)) ;
#20533 = DIRECTION('ref_axis',(0.,0.951056516295154,-0.309016994374948)) ;
#20534 = DIRECTION('',(-1.,0.,0.)) ;
#20535 = DIRECTION('center_axis',(-1.,0.,0.)) ;
#20536 = DIRECTION('ref_axis',(0.,0.951056516295153,-0.309016994374948)) ;
#20537 = DIRECTION('center_axis',(1.,0.,0.)) ;
#20538 = DIRECTION('ref_axis',(0.,-0.4067366430758,0.913545457642601)) ;
#20539 = DIRECTION('center_axis',(1.,0.,0.)) ;
#20540 = DIRECTION('ref_axis',(0.,-0.4067366430758,0.913545457642601)) ;
#20541 = DIRECTION('center_axis',(1.,0.,0.)) ;
#20542 = DIRECTION('ref_axis',(0.,-0.4067366430758,0.913545457642601)) ;
#20543 = DIRECTION('center_axis',(1.,0.,0.)) ;
#20544 = DIRECTION('ref_axis',(0.,-0.4067366430758,0.913545457642601)) ;
#20545 = DIRECTION('center_axis',(1.,0.,0.)) ;
#20546 = DIRECTION('ref_axis',(0.,-0.4067366430758,0.913545457642601)) ;
#20547 = DIRECTION('center_axis',(1.,0.,0.)) ;
#20548 = DIRECTION('ref_axis',(0.,-0.4067366430758,0.913545457642601)) ;
#20549 = DIRECTION('center_axis',(1.,0.,0.)) ;
#20550 = DIRECTION('ref_axis',(0.,-0.4067366430758,0.913545457642601)) ;
#20551 = DIRECTION('center_axis',(1.,0.,0.)) ;
#20552 = DIRECTION('ref_axis',(0.,-0.4067366430758,0.913545457642601)) ;
#20553 = DIRECTION('center_axis',(-1.,0.,0.)) ;
#20554 = DIRECTION('ref_axis',(0.,0.4067366430758,-0.913545457642601)) ;
#20555 = DIRECTION('',(-1.,0.,0.)) ;
#20556 = DIRECTION('center_axis',(-1.,0.,0.)) ;
#20557 = DIRECTION('ref_axis',(0.,0.4067366430758,-0.913545457642601)) ;
#20558 = DIRECTION('',(-1.,0.,0.)) ;
#20559 = DIRECTION('center_axis',(-1.,0.,0.)) ;
#20560 = DIRECTION('ref_axis',(0.,0.4067366430758,-0.913545457642601)) ;
#20561 = DIRECTION('center_axis',(1.,0.,0.)) ;
#20562 = DIRECTION('ref_axis',(0.,-0.499999999999999,0.866025403784439)) ;
#20563 = DIRECTION('center_axis',(1.,0.,0.)) ;
#20564 = DIRECTION('ref_axis',(0.,-0.499999999999999,0.866025403784439)) ;
#20565 = DIRECTION('center_axis',(1.,0.,0.)) ;
#20566 = DIRECTION('ref_axis',(0.,-0.499999999999999,0.866025403784439)) ;
#20567 = DIRECTION('center_axis',(1.,0.,0.)) ;
#20568 = DIRECTION('ref_axis',(0.,-0.499999999999999,0.866025403784439)) ;
#20569 = DIRECTION('center_axis',(1.,0.,0.)) ;
#20570 = DIRECTION('ref_axis',(0.,-0.499999999999999,0.866025403784439)) ;
#20571 = DIRECTION('center_axis',(1.,0.,0.)) ;
#20572 = DIRECTION('ref_axis',(0.,-0.499999999999999,0.866025403784439)) ;
#20573 = DIRECTION('center_axis',(1.,0.,0.)) ;
#20574 = DIRECTION('ref_axis',(0.,-0.499999999999999,0.866025403784439)) ;
#20575 = DIRECTION('center_axis',(1.,0.,0.)) ;
#20576 = DIRECTION('ref_axis',(0.,-0.499999999999999,0.866025403784439)) ;
#20577 = DIRECTION('center_axis',(-1.,0.,0.)) ;
#20578 = DIRECTION('ref_axis',(0.,0.499999999999999,-0.866025403784439)) ;
#20579 = DIRECTION('',(-1.,0.,0.)) ;
#20580 = DIRECTION('center_axis',(-1.,0.,0.)) ;
#20581 = DIRECTION('ref_axis',(0.,0.499999999999999,-0.866025403784439)) ;
#20582 = DIRECTION('',(-1.,0.,0.)) ;
#20583 = DIRECTION('center_axis',(-1.,0.,0.)) ;
#20584 = DIRECTION('ref_axis',(0.,0.499999999999999,-0.866025403784439)) ;
#20585 = DIRECTION('center_axis',(1.,0.,0.)) ;
#20586 = DIRECTION('ref_axis',(0.,-0.587785252292473,0.809016994374947)) ;
#20587 = DIRECTION('center_axis',(1.,0.,0.)) ;
#20588 = DIRECTION('ref_axis',(0.,-0.587785252292473,0.809016994374947)) ;
#20589 = DIRECTION('center_axis',(1.,0.,0.)) ;
#20590 = DIRECTION('ref_axis',(0.,-0.587785252292473,0.809016994374947)) ;
#20591 = DIRECTION('center_axis',(1.,0.,0.)) ;
#20592 = DIRECTION('ref_axis',(0.,-0.587785252292473,0.809016994374947)) ;
#20593 = DIRECTION('center_axis',(1.,0.,0.)) ;
#20594 = DIRECTION('ref_axis',(0.,-0.587785252292473,0.809016994374947)) ;
#20595 = DIRECTION('center_axis',(1.,0.,0.)) ;
#20596 = DIRECTION('ref_axis',(0.,-0.587785252292473,0.809016994374947)) ;
#20597 = DIRECTION('center_axis',(1.,0.,0.)) ;
#20598 = DIRECTION('ref_axis',(0.,-0.587785252292473,0.809016994374947)) ;
#20599 = DIRECTION('center_axis',(1.,0.,0.)) ;
#20600 = DIRECTION('ref_axis',(0.,-0.587785252292473,0.809016994374947)) ;
#20601 = DIRECTION('center_axis',(-1.,0.,0.)) ;
#20602 = DIRECTION('ref_axis',(0.,0.587785252292473,-0.809016994374947)) ;
#20603 = DIRECTION('',(-1.,0.,0.)) ;
#20604 = DIRECTION('center_axis',(-1.,0.,0.)) ;
#20605 = DIRECTION('ref_axis',(0.,0.587785252292473,-0.809016994374947)) ;
#20606 = DIRECTION('',(-1.,0.,0.)) ;
#20607 = DIRECTION('center_axis',(-1.,0.,0.)) ;
#20608 = DIRECTION('ref_axis',(0.,0.587785252292473,-0.809016994374947)) ;
#20609 = DIRECTION('center_axis',(1.,0.,0.)) ;
#20610 = DIRECTION('ref_axis',(0.,-0.669130606358858,0.743144825477394)) ;
#20611 = DIRECTION('center_axis',(1.,0.,0.)) ;
#20612 = DIRECTION('ref_axis',(0.,-0.669130606358858,0.743144825477394)) ;
#20613 = DIRECTION('center_axis',(1.,0.,0.)) ;
#20614 = DIRECTION('ref_axis',(0.,-0.669130606358858,0.743144825477394)) ;
#20615 = DIRECTION('center_axis',(1.,0.,0.)) ;
#20616 = DIRECTION('ref_axis',(0.,-0.669130606358858,0.743144825477394)) ;
#20617 = DIRECTION('center_axis',(1.,0.,0.)) ;
#20618 = DIRECTION('ref_axis',(0.,-0.669130606358858,0.743144825477394)) ;
#20619 = DIRECTION('center_axis',(1.,0.,0.)) ;
#20620 = DIRECTION('ref_axis',(0.,-0.669130606358858,0.743144825477394)) ;
#20621 = DIRECTION('center_axis',(1.,0.,0.)) ;
#20622 = DIRECTION('ref_axis',(0.,-0.669130606358858,0.743144825477394)) ;
#20623 = DIRECTION('center_axis',(1.,0.,0.)) ;
#20624 = DIRECTION('ref_axis',(0.,-0.669130606358858,0.743144825477394)) ;
#20625 = DIRECTION('center_axis',(-1.,0.,0.)) ;
#20626 = DIRECTION('ref_axis',(0.,0.669130606358858,-0.743144825477394)) ;
#20627 = DIRECTION('',(-1.,0.,0.)) ;
#20628 = DIRECTION('center_axis',(-1.,0.,0.)) ;
#20629 = DIRECTION('ref_axis',(0.,0.669130606358858,-0.743144825477394)) ;
#20630 = DIRECTION('',(-1.,0.,0.)) ;
#20631 = DIRECTION('center_axis',(-1.,0.,0.)) ;
#20632 = DIRECTION('ref_axis',(0.,0.669130606358858,-0.743144825477394)) ;
#20633 = DIRECTION('center_axis',(1.,0.,0.)) ;
#20634 = DIRECTION('ref_axis',(0.,-0.743144825477394,0.669130606358858)) ;
#20635 = DIRECTION('center_axis',(1.,0.,0.)) ;
#20636 = DIRECTION('ref_axis',(0.,-0.743144825477394,0.669130606358858)) ;
#20637 = DIRECTION('center_axis',(1.,0.,0.)) ;
#20638 = DIRECTION('ref_axis',(0.,-0.743144825477394,0.669130606358858)) ;
#20639 = DIRECTION('center_axis',(1.,0.,0.)) ;
#20640 = DIRECTION('ref_axis',(0.,-0.743144825477394,0.669130606358858)) ;
#20641 = DIRECTION('center_axis',(1.,0.,0.)) ;
#20642 = DIRECTION('ref_axis',(0.,-0.743144825477394,0.669130606358858)) ;
#20643 = DIRECTION('center_axis',(1.,0.,0.)) ;
#20644 = DIRECTION('ref_axis',(0.,-0.743144825477394,0.669130606358858)) ;
#20645 = DIRECTION('center_axis',(1.,0.,0.)) ;
#20646 = DIRECTION('ref_axis',(0.,-0.743144825477394,0.669130606358858)) ;
#20647 = DIRECTION('center_axis',(1.,0.,0.)) ;
#20648 = DIRECTION('ref_axis',(0.,-0.743144825477394,0.669130606358858)) ;
#20649 = DIRECTION('center_axis',(-1.,0.,0.)) ;
#20650 = DIRECTION('ref_axis',(0.,0.743144825477394,-0.669130606358858)) ;
#20651 = DIRECTION('',(-1.,0.,0.)) ;
#20652 = DIRECTION('center_axis',(-1.,0.,0.)) ;
#20653 = DIRECTION('ref_axis',(0.,0.743144825477394,-0.669130606358858)) ;
#20654 = DIRECTION('',(-1.,0.,0.)) ;
#20655 = DIRECTION('center_axis',(-1.,0.,0.)) ;
#20656 = DIRECTION('ref_axis',(0.,0.743144825477394,-0.669130606358858)) ;
#20657 = DIRECTION('center_axis',(1.,0.,0.)) ;
#20658 = DIRECTION('ref_axis',(0.,-0.809016994374947,0.587785252292473)) ;
#20659 = DIRECTION('center_axis',(1.,0.,0.)) ;
#20660 = DIRECTION('ref_axis',(0.,-0.809016994374947,0.587785252292473)) ;
#20661 = DIRECTION('center_axis',(1.,0.,0.)) ;
#20662 = DIRECTION('ref_axis',(0.,-0.809016994374947,0.587785252292473)) ;
#20663 = DIRECTION('center_axis',(1.,0.,0.)) ;
#20664 = DIRECTION('ref_axis',(0.,-0.809016994374947,0.587785252292473)) ;
#20665 = DIRECTION('center_axis',(1.,0.,0.)) ;
#20666 = DIRECTION('ref_axis',(0.,-0.809016994374947,0.587785252292473)) ;
#20667 = DIRECTION('center_axis',(1.,0.,0.)) ;
#20668 = DIRECTION('ref_axis',(0.,-0.809016994374947,0.587785252292473)) ;
#20669 = DIRECTION('center_axis',(1.,0.,0.)) ;
#20670 = DIRECTION('ref_axis',(0.,-0.809016994374947,0.587785252292473)) ;
#20671 = DIRECTION('center_axis',(1.,0.,0.)) ;
#20672 = DIRECTION('ref_axis',(0.,-0.809016994374947,0.587785252292473)) ;
#20673 = DIRECTION('center_axis',(-1.,0.,0.)) ;
#20674 = DIRECTION('ref_axis',(0.,0.809016994374947,-0.587785252292473)) ;
#20675 = DIRECTION('',(-1.,0.,0.)) ;
#20676 = DIRECTION('center_axis',(-1.,0.,0.)) ;
#20677 = DIRECTION('ref_axis',(0.,0.809016994374947,-0.587785252292473)) ;
#20678 = DIRECTION('',(-1.,0.,0.)) ;
#20679 = DIRECTION('center_axis',(-1.,0.,0.)) ;
#20680 = DIRECTION('ref_axis',(0.,0.809016994374947,-0.587785252292473)) ;
#20681 = DIRECTION('center_axis',(1.,0.,0.)) ;
#20682 = DIRECTION('ref_axis',(0.,-0.866025403784438,0.5)) ;
#20683 = DIRECTION('center_axis',(1.,0.,0.)) ;
#20684 = DIRECTION('ref_axis',(0.,-0.866025403784438,0.5)) ;
#20685 = DIRECTION('center_axis',(1.,0.,0.)) ;
#20686 = DIRECTION('ref_axis',(0.,-0.866025403784438,0.5)) ;
#20687 = DIRECTION('center_axis',(1.,0.,0.)) ;
#20688 = DIRECTION('ref_axis',(0.,-0.866025403784438,0.5)) ;
#20689 = DIRECTION('center_axis',(1.,0.,0.)) ;
#20690 = DIRECTION('ref_axis',(0.,-0.866025403784438,0.5)) ;
#20691 = DIRECTION('center_axis',(1.,0.,0.)) ;
#20692 = DIRECTION('ref_axis',(0.,-0.866025403784438,0.5)) ;
#20693 = DIRECTION('center_axis',(1.,0.,0.)) ;
#20694 = DIRECTION('ref_axis',(0.,-0.866025403784438,0.5)) ;
#20695 = DIRECTION('center_axis',(1.,0.,0.)) ;
#20696 = DIRECTION('ref_axis',(0.,-0.866025403784438,0.5)) ;
#20697 = DIRECTION('center_axis',(-1.,0.,0.)) ;
#20698 = DIRECTION('ref_axis',(0.,0.866025403784438,-0.5)) ;
#20699 = DIRECTION('',(-1.,0.,0.)) ;
#20700 = DIRECTION('center_axis',(-1.,0.,0.)) ;
#20701 = DIRECTION('ref_axis',(0.,0.866025403784438,-0.5)) ;
#20702 = DIRECTION('',(-1.,0.,0.)) ;
#20703 = DIRECTION('center_axis',(-1.,0.,0.)) ;
#20704 = DIRECTION('ref_axis',(0.,0.866025403784438,-0.5)) ;
#20705 = DIRECTION('center_axis',(1.,0.,0.)) ;
#20706 = DIRECTION('ref_axis',(0.,-0.913545457642601,0.4067366430758)) ;
#20707 = DIRECTION('center_axis',(1.,0.,0.)) ;
#20708 = DIRECTION('ref_axis',(0.,-0.913545457642601,0.4067366430758)) ;
#20709 = DIRECTION('center_axis',(1.,0.,0.)) ;
#20710 = DIRECTION('ref_axis',(0.,-0.913545457642601,0.4067366430758)) ;
#20711 = DIRECTION('center_axis',(1.,0.,0.)) ;
#20712 = DIRECTION('ref_axis',(0.,-0.913545457642601,0.4067366430758)) ;
#20713 = DIRECTION('center_axis',(1.,0.,0.)) ;
#20714 = DIRECTION('ref_axis',(0.,-0.913545457642601,0.4067366430758)) ;
#20715 = DIRECTION('center_axis',(1.,0.,0.)) ;
#20716 = DIRECTION('ref_axis',(0.,-0.913545457642601,0.4067366430758)) ;
#20717 = DIRECTION('center_axis',(1.,0.,0.)) ;
#20718 = DIRECTION('ref_axis',(0.,-0.913545457642601,0.4067366430758)) ;
#20719 = DIRECTION('center_axis',(1.,0.,0.)) ;
#20720 = DIRECTION('ref_axis',(0.,-0.913545457642601,0.4067366430758)) ;
#20721 = DIRECTION('center_axis',(-1.,0.,0.)) ;
#20722 = DIRECTION('ref_axis',(0.,0.913545457642601,-0.4067366430758)) ;
#20723 = DIRECTION('',(-1.,0.,0.)) ;
#20724 = DIRECTION('center_axis',(-1.,0.,0.)) ;
#20725 = DIRECTION('ref_axis',(0.,0.913545457642601,-0.4067366430758)) ;
#20726 = DIRECTION('',(-1.,0.,0.)) ;
#20727 = DIRECTION('center_axis',(-1.,0.,0.)) ;
#20728 = DIRECTION('ref_axis',(0.,0.913545457642601,-0.4067366430758)) ;
#20729 = DIRECTION('center_axis',(1.,0.,0.)) ;
#20730 = DIRECTION('ref_axis',(0.,-0.309016994374948,0.951056516295154)) ;
#20731 = DIRECTION('center_axis',(1.,0.,0.)) ;
#20732 = DIRECTION('ref_axis',(0.,-0.309016994374948,0.951056516295153)) ;
#20733 = DIRECTION('center_axis',(1.,0.,0.)) ;
#20734 = DIRECTION('ref_axis',(0.,-0.309016994374948,0.951056516295154)) ;
#20735 = DIRECTION('center_axis',(1.,0.,0.)) ;
#20736 = DIRECTION('ref_axis',(0.,-0.309016994374948,0.951056516295153)) ;
#20737 = DIRECTION('center_axis',(1.,0.,0.)) ;
#20738 = DIRECTION('ref_axis',(0.,-0.309016994374948,0.951056516295154)) ;
#20739 = DIRECTION('center_axis',(1.,0.,0.)) ;
#20740 = DIRECTION('ref_axis',(0.,-0.309016994374948,0.951056516295153)) ;
#20741 = DIRECTION('center_axis',(1.,0.,0.)) ;
#20742 = DIRECTION('ref_axis',(0.,-0.309016994374948,0.951056516295154)) ;
#20743 = DIRECTION('center_axis',(1.,0.,0.)) ;
#20744 = DIRECTION('ref_axis',(0.,-0.309016994374948,0.951056516295153)) ;
#20745 = DIRECTION('center_axis',(-1.,0.,0.)) ;
#20746 = DIRECTION('ref_axis',(0.,0.309016994374948,-0.951056516295153)) ;
#20747 = DIRECTION('',(-1.,0.,0.)) ;
#20748 = DIRECTION('center_axis',(-1.,0.,0.)) ;
#20749 = DIRECTION('ref_axis',(0.,0.309016994374948,-0.951056516295154)) ;
#20750 = DIRECTION('',(-1.,0.,0.)) ;
#20751 = DIRECTION('center_axis',(-1.,0.,0.)) ;
#20752 = DIRECTION('ref_axis',(0.,0.309016994374948,-0.951056516295153)) ;
#20753 = DIRECTION('center_axis',(1.,0.,0.)) ;
#20754 = DIRECTION('ref_axis',(0.,-0.207911690817759,0.978147600733806)) ;
#20755 = DIRECTION('center_axis',(1.,0.,0.)) ;
#20756 = DIRECTION('ref_axis',(0.,-0.207911690817759,0.978147600733806)) ;
#20757 = DIRECTION('center_axis',(1.,0.,0.)) ;
#20758 = DIRECTION('ref_axis',(0.,-0.207911690817759,0.978147600733806)) ;
#20759 = DIRECTION('center_axis',(1.,0.,0.)) ;
#20760 = DIRECTION('ref_axis',(0.,-0.207911690817759,0.978147600733806)) ;
#20761 = DIRECTION('center_axis',(1.,0.,0.)) ;
#20762 = DIRECTION('ref_axis',(0.,-0.207911690817759,0.978147600733806)) ;
#20763 = DIRECTION('center_axis',(1.,0.,0.)) ;
#20764 = DIRECTION('ref_axis',(0.,-0.207911690817759,0.978147600733806)) ;
#20765 = DIRECTION('center_axis',(1.,0.,0.)) ;
#20766 = DIRECTION('ref_axis',(0.,-0.207911690817759,0.978147600733806)) ;
#20767 = DIRECTION('center_axis',(1.,0.,0.)) ;
#20768 = DIRECTION('ref_axis',(0.,-0.207911690817759,0.978147600733806)) ;
#20769 = DIRECTION('center_axis',(-1.,0.,0.)) ;
#20770 = DIRECTION('ref_axis',(0.,0.207911690817759,-0.978147600733806)) ;
#20771 = DIRECTION('',(-1.,0.,0.)) ;
#20772 = DIRECTION('center_axis',(-1.,0.,0.)) ;
#20773 = DIRECTION('ref_axis',(0.,0.207911690817759,-0.978147600733806)) ;
#20774 = DIRECTION('',(-1.,0.,0.)) ;
#20775 = DIRECTION('center_axis',(-1.,0.,0.)) ;
#20776 = DIRECTION('ref_axis',(0.,0.207911690817759,-0.978147600733806)) ;
#20777 = DIRECTION('center_axis',(1.,0.,0.)) ;
#20778 = DIRECTION('ref_axis',(0.,-0.104528463267653,0.994521895368273)) ;
#20779 = DIRECTION('center_axis',(1.,0.,0.)) ;
#20780 = DIRECTION('ref_axis',(0.,-0.104528463267653,0.994521895368273)) ;
#20781 = DIRECTION('center_axis',(1.,0.,0.)) ;
#20782 = DIRECTION('ref_axis',(0.,-0.104528463267653,0.994521895368273)) ;
#20783 = DIRECTION('center_axis',(1.,0.,0.)) ;
#20784 = DIRECTION('ref_axis',(0.,-0.104528463267653,0.994521895368273)) ;
#20785 = DIRECTION('center_axis',(1.,0.,0.)) ;
#20786 = DIRECTION('ref_axis',(0.,-0.104528463267653,0.994521895368273)) ;
#20787 = DIRECTION('center_axis',(1.,0.,0.)) ;
#20788 = DIRECTION('ref_axis',(0.,-0.104528463267653,0.994521895368273)) ;
#20789 = DIRECTION('center_axis',(1.,0.,0.)) ;
#20790 = DIRECTION('ref_axis',(0.,-0.104528463267653,0.994521895368273)) ;
#20791 = DIRECTION('center_axis',(1.,0.,0.)) ;
#20792 = DIRECTION('ref_axis',(0.,-0.104528463267653,0.994521895368273)) ;
#20793 = DIRECTION('center_axis',(-1.,0.,0.)) ;
#20794 = DIRECTION('ref_axis',(0.,0.104528463267653,-0.994521895368273)) ;
#20795 = DIRECTION('',(-1.,0.,0.)) ;
#20796 = DIRECTION('center_axis',(-1.,0.,0.)) ;
#20797 = DIRECTION('ref_axis',(0.,0.104528463267653,-0.994521895368273)) ;
#20798 = DIRECTION('',(-1.,0.,0.)) ;
#20799 = DIRECTION('center_axis',(-1.,0.,0.)) ;
#20800 = DIRECTION('ref_axis',(0.,0.104528463267653,-0.994521895368273)) ;
#20801 = DIRECTION('center_axis',(1.,0.,0.)) ;
#20802 = DIRECTION('ref_axis',(0.,1.22464679914735E-16,1.)) ;
#20803 = DIRECTION('center_axis',(1.,0.,0.)) ;
#20804 = DIRECTION('ref_axis',(0.,1.22464679914735E-16,1.)) ;
#20805 = DIRECTION('center_axis',(1.,0.,0.)) ;
#20806 = DIRECTION('ref_axis',(0.,1.22464679914735E-16,1.)) ;
#20807 = DIRECTION('center_axis',(1.,0.,0.)) ;
#20808 = DIRECTION('ref_axis',(0.,1.22464679914735E-16,1.)) ;
#20809 = DIRECTION('center_axis',(1.,0.,0.)) ;
#20810 = DIRECTION('ref_axis',(0.,1.22464679914735E-16,1.)) ;
#20811 = DIRECTION('center_axis',(1.,0.,0.)) ;
#20812 = DIRECTION('ref_axis',(0.,1.22464679914735E-16,1.)) ;
#20813 = DIRECTION('center_axis',(1.,0.,0.)) ;
#20814 = DIRECTION('ref_axis',(0.,1.22464679914735E-16,1.)) ;
#20815 = DIRECTION('center_axis',(1.,0.,0.)) ;
#20816 = DIRECTION('ref_axis',(0.,1.22464679914735E-16,1.)) ;
#20817 = DIRECTION('center_axis',(-1.,0.,0.)) ;
#20818 = DIRECTION('ref_axis',(0.,-1.22464679914735E-16,-1.)) ;
#20819 = DIRECTION('',(-1.,0.,0.)) ;
#20820 = DIRECTION('center_axis',(-1.,0.,0.)) ;
#20821 = DIRECTION('ref_axis',(0.,-1.22464679914735E-16,-1.)) ;
#20822 = DIRECTION('',(-1.,0.,0.)) ;
#20823 = DIRECTION('center_axis',(-1.,0.,0.)) ;
#20824 = DIRECTION('ref_axis',(0.,-1.22464679914735E-16,-1.)) ;
#20825 = DIRECTION('center_axis',(1.,0.,0.)) ;
#20826 = DIRECTION('ref_axis',(0.,0.104528463267654,0.994521895368273)) ;
#20827 = DIRECTION('center_axis',(1.,0.,0.)) ;
#20828 = DIRECTION('ref_axis',(0.,0.104528463267654,0.994521895368273)) ;
#20829 = DIRECTION('center_axis',(1.,0.,0.)) ;
#20830 = DIRECTION('ref_axis',(0.,0.104528463267654,0.994521895368273)) ;
#20831 = DIRECTION('center_axis',(1.,0.,0.)) ;
#20832 = DIRECTION('ref_axis',(0.,0.104528463267654,0.994521895368273)) ;
#20833 = DIRECTION('center_axis',(1.,0.,0.)) ;
#20834 = DIRECTION('ref_axis',(0.,0.104528463267654,0.994521895368273)) ;
#20835 = DIRECTION('center_axis',(1.,0.,0.)) ;
#20836 = DIRECTION('ref_axis',(0.,0.104528463267654,0.994521895368273)) ;
#20837 = DIRECTION('center_axis',(1.,0.,0.)) ;
#20838 = DIRECTION('ref_axis',(0.,0.104528463267654,0.994521895368273)) ;
#20839 = DIRECTION('center_axis',(1.,0.,0.)) ;
#20840 = DIRECTION('ref_axis',(0.,0.104528463267654,0.994521895368273)) ;
#20841 = DIRECTION('center_axis',(-1.,0.,0.)) ;
#20842 = DIRECTION('ref_axis',(0.,-0.104528463267654,-0.994521895368273)) ;
#20843 = DIRECTION('',(-1.,0.,0.)) ;
#20844 = DIRECTION('center_axis',(-1.,0.,0.)) ;
#20845 = DIRECTION('ref_axis',(0.,-0.104528463267654,-0.994521895368273)) ;
#20846 = DIRECTION('',(-1.,0.,0.)) ;
#20847 = DIRECTION('center_axis',(-1.,0.,0.)) ;
#20848 = DIRECTION('ref_axis',(0.,-0.104528463267654,-0.994521895368273)) ;
#20849 = DIRECTION('center_axis',(1.,0.,0.)) ;
#20850 = DIRECTION('ref_axis',(0.,0.207911690817759,0.978147600733806)) ;
#20851 = DIRECTION('center_axis',(1.,0.,0.)) ;
#20852 = DIRECTION('ref_axis',(0.,0.207911690817759,0.978147600733806)) ;
#20853 = DIRECTION('center_axis',(1.,0.,0.)) ;
#20854 = DIRECTION('ref_axis',(0.,0.207911690817759,0.978147600733806)) ;
#20855 = DIRECTION('center_axis',(1.,0.,0.)) ;
#20856 = DIRECTION('ref_axis',(0.,0.207911690817759,0.978147600733806)) ;
#20857 = DIRECTION('center_axis',(1.,0.,0.)) ;
#20858 = DIRECTION('ref_axis',(0.,0.207911690817759,0.978147600733806)) ;
#20859 = DIRECTION('center_axis',(1.,0.,0.)) ;
#20860 = DIRECTION('ref_axis',(0.,0.207911690817759,0.978147600733806)) ;
#20861 = DIRECTION('center_axis',(1.,0.,0.)) ;
#20862 = DIRECTION('ref_axis',(0.,0.207911690817759,0.978147600733806)) ;
#20863 = DIRECTION('center_axis',(1.,0.,0.)) ;
#20864 = DIRECTION('ref_axis',(0.,0.207911690817759,0.978147600733806)) ;
#20865 = DIRECTION('center_axis',(-1.,0.,0.)) ;
#20866 = DIRECTION('ref_axis',(0.,-0.207911690817759,-0.978147600733806)) ;
#20867 = DIRECTION('',(-1.,0.,0.)) ;
#20868 = DIRECTION('center_axis',(-1.,0.,0.)) ;
#20869 = DIRECTION('ref_axis',(0.,-0.207911690817759,-0.978147600733806)) ;
#20870 = DIRECTION('',(-1.,0.,0.)) ;
#20871 = DIRECTION('center_axis',(-1.,0.,0.)) ;
#20872 = DIRECTION('ref_axis',(0.,-0.207911690817759,-0.978147600733806)) ;
#20873 = DIRECTION('center_axis',(1.,0.,0.)) ;
#20874 = DIRECTION('ref_axis',(0.,0.309016994374948,0.951056516295154)) ;
#20875 = DIRECTION('center_axis',(1.,0.,0.)) ;
#20876 = DIRECTION('ref_axis',(0.,0.309016994374948,0.951056516295153)) ;
#20877 = DIRECTION('center_axis',(1.,0.,0.)) ;
#20878 = DIRECTION('ref_axis',(0.,0.309016994374948,0.951056516295154)) ;
#20879 = DIRECTION('center_axis',(1.,0.,0.)) ;
#20880 = DIRECTION('ref_axis',(0.,0.309016994374948,0.951056516295153)) ;
#20881 = DIRECTION('center_axis',(1.,0.,0.)) ;
#20882 = DIRECTION('ref_axis',(0.,0.309016994374948,0.951056516295154)) ;
#20883 = DIRECTION('center_axis',(1.,0.,0.)) ;
#20884 = DIRECTION('ref_axis',(0.,0.309016994374948,0.951056516295153)) ;
#20885 = DIRECTION('center_axis',(1.,0.,0.)) ;
#20886 = DIRECTION('ref_axis',(0.,0.309016994374948,0.951056516295154)) ;
#20887 = DIRECTION('center_axis',(1.,0.,0.)) ;
#20888 = DIRECTION('ref_axis',(0.,0.309016994374948,0.951056516295153)) ;
#20889 = DIRECTION('center_axis',(-1.,0.,0.)) ;
#20890 = DIRECTION('ref_axis',(0.,-0.309016994374948,-0.951056516295153)) ;
#20891 = DIRECTION('',(-1.,0.,0.)) ;
#20892 = DIRECTION('center_axis',(-1.,0.,0.)) ;
#20893 = DIRECTION('ref_axis',(0.,-0.309016994374948,-0.951056516295154)) ;
#20894 = DIRECTION('',(-1.,0.,0.)) ;
#20895 = DIRECTION('center_axis',(-1.,0.,0.)) ;
#20896 = DIRECTION('ref_axis',(0.,-0.309016994374948,-0.951056516295153)) ;
#20897 = DIRECTION('center_axis',(1.,0.,0.)) ;
#20898 = DIRECTION('ref_axis',(0.,0.4067366430758,0.913545457642601)) ;
#20899 = DIRECTION('center_axis',(1.,0.,0.)) ;
#20900 = DIRECTION('ref_axis',(0.,0.4067366430758,0.913545457642601)) ;
#20901 = DIRECTION('center_axis',(1.,0.,0.)) ;
#20902 = DIRECTION('ref_axis',(0.,0.4067366430758,0.913545457642601)) ;
#20903 = DIRECTION('center_axis',(1.,0.,0.)) ;
#20904 = DIRECTION('ref_axis',(0.,0.4067366430758,0.913545457642601)) ;
#20905 = DIRECTION('center_axis',(1.,0.,0.)) ;
#20906 = DIRECTION('ref_axis',(0.,0.4067366430758,0.913545457642601)) ;
#20907 = DIRECTION('center_axis',(1.,0.,0.)) ;
#20908 = DIRECTION('ref_axis',(0.,0.4067366430758,0.913545457642601)) ;
#20909 = DIRECTION('center_axis',(1.,0.,0.)) ;
#20910 = DIRECTION('ref_axis',(0.,0.4067366430758,0.913545457642601)) ;
#20911 = DIRECTION('center_axis',(1.,0.,0.)) ;
#20912 = DIRECTION('ref_axis',(0.,0.4067366430758,0.913545457642601)) ;
#20913 = DIRECTION('center_axis',(-1.,0.,0.)) ;
#20914 = DIRECTION('ref_axis',(0.,-0.4067366430758,-0.913545457642601)) ;
#20915 = DIRECTION('',(-1.,0.,0.)) ;
#20916 = DIRECTION('center_axis',(-1.,0.,0.)) ;
#20917 = DIRECTION('ref_axis',(0.,-0.4067366430758,-0.913545457642601)) ;
#20918 = DIRECTION('',(-1.,0.,0.)) ;
#20919 = DIRECTION('center_axis',(-1.,0.,0.)) ;
#20920 = DIRECTION('ref_axis',(0.,-0.4067366430758,-0.913545457642601)) ;
#20921 = DIRECTION('center_axis',(1.,0.,0.)) ;
#20922 = DIRECTION('ref_axis',(0.,0.5,0.866025403784439)) ;
#20923 = DIRECTION('center_axis',(1.,0.,0.)) ;
#20924 = DIRECTION('ref_axis',(0.,0.5,0.866025403784439)) ;
#20925 = DIRECTION('center_axis',(1.,0.,0.)) ;
#20926 = DIRECTION('ref_axis',(0.,0.5,0.866025403784439)) ;
#20927 = DIRECTION('center_axis',(1.,0.,0.)) ;
#20928 = DIRECTION('ref_axis',(0.,0.5,0.866025403784439)) ;
#20929 = DIRECTION('center_axis',(1.,0.,0.)) ;
#20930 = DIRECTION('ref_axis',(0.,0.5,0.866025403784439)) ;
#20931 = DIRECTION('center_axis',(1.,0.,0.)) ;
#20932 = DIRECTION('ref_axis',(0.,0.5,0.866025403784439)) ;
#20933 = DIRECTION('center_axis',(1.,0.,0.)) ;
#20934 = DIRECTION('ref_axis',(0.,0.5,0.866025403784439)) ;
#20935 = DIRECTION('center_axis',(1.,0.,0.)) ;
#20936 = DIRECTION('ref_axis',(0.,0.5,0.866025403784439)) ;
#20937 = DIRECTION('center_axis',(-1.,0.,0.)) ;
#20938 = DIRECTION('ref_axis',(0.,-0.5,-0.866025403784439)) ;
#20939 = DIRECTION('',(-1.,0.,0.)) ;
#20940 = DIRECTION('center_axis',(-1.,0.,0.)) ;
#20941 = DIRECTION('ref_axis',(0.,-0.5,-0.866025403784439)) ;
#20942 = DIRECTION('',(-1.,0.,0.)) ;
#20943 = DIRECTION('center_axis',(-1.,0.,0.)) ;
#20944 = DIRECTION('ref_axis',(0.,-0.5,-0.866025403784439)) ;
#20945 = DIRECTION('center_axis',(1.,0.,0.)) ;
#20946 = DIRECTION('ref_axis',(0.,0.587785252292474,0.809016994374947)) ;
#20947 = DIRECTION('center_axis',(1.,0.,0.)) ;
#20948 = DIRECTION('ref_axis',(0.,0.587785252292474,0.809016994374947)) ;
#20949 = DIRECTION('center_axis',(1.,0.,0.)) ;
#20950 = DIRECTION('ref_axis',(0.,0.587785252292474,0.809016994374947)) ;
#20951 = DIRECTION('center_axis',(1.,0.,0.)) ;
#20952 = DIRECTION('ref_axis',(0.,0.587785252292474,0.809016994374947)) ;
#20953 = DIRECTION('center_axis',(1.,0.,0.)) ;
#20954 = DIRECTION('ref_axis',(0.,0.587785252292474,0.809016994374947)) ;
#20955 = DIRECTION('center_axis',(1.,0.,0.)) ;
#20956 = DIRECTION('ref_axis',(0.,0.587785252292474,0.809016994374947)) ;
#20957 = DIRECTION('center_axis',(1.,0.,0.)) ;
#20958 = DIRECTION('ref_axis',(0.,0.587785252292474,0.809016994374947)) ;
#20959 = DIRECTION('center_axis',(1.,0.,0.)) ;
#20960 = DIRECTION('ref_axis',(0.,0.587785252292474,0.809016994374947)) ;
#20961 = DIRECTION('center_axis',(-1.,0.,0.)) ;
#20962 = DIRECTION('ref_axis',(0.,-0.587785252292474,-0.809016994374947)) ;
#20963 = DIRECTION('',(-1.,0.,0.)) ;
#20964 = DIRECTION('center_axis',(-1.,0.,0.)) ;
#20965 = DIRECTION('ref_axis',(0.,-0.587785252292474,-0.809016994374947)) ;
#20966 = DIRECTION('',(-1.,0.,0.)) ;
#20967 = DIRECTION('center_axis',(-1.,0.,0.)) ;
#20968 = DIRECTION('ref_axis',(0.,-0.587785252292474,-0.809016994374947)) ;
#20969 = DIRECTION('center_axis',(1.,0.,0.)) ;
#20970 = DIRECTION('ref_axis',(0.,0.743144825477395,0.669130606358858)) ;
#20971 = DIRECTION('center_axis',(1.,0.,0.)) ;
#20972 = DIRECTION('ref_axis',(0.,0.743144825477395,0.669130606358858)) ;
#20973 = DIRECTION('center_axis',(1.,0.,0.)) ;
#20974 = DIRECTION('ref_axis',(0.,0.743144825477395,0.669130606358858)) ;
#20975 = DIRECTION('center_axis',(1.,0.,0.)) ;
#20976 = DIRECTION('ref_axis',(0.,0.743144825477395,0.669130606358858)) ;
#20977 = DIRECTION('center_axis',(1.,0.,0.)) ;
#20978 = DIRECTION('ref_axis',(0.,0.743144825477395,0.669130606358858)) ;
#20979 = DIRECTION('center_axis',(1.,0.,0.)) ;
#20980 = DIRECTION('ref_axis',(0.,0.743144825477395,0.669130606358858)) ;
#20981 = DIRECTION('center_axis',(1.,0.,0.)) ;
#20982 = DIRECTION('ref_axis',(0.,0.743144825477395,0.669130606358858)) ;
#20983 = DIRECTION('center_axis',(1.,0.,0.)) ;
#20984 = DIRECTION('ref_axis',(0.,0.743144825477395,0.669130606358858)) ;
#20985 = DIRECTION('center_axis',(-1.,0.,0.)) ;
#20986 = DIRECTION('ref_axis',(0.,-0.743144825477395,-0.669130606358858)) ;
#20987 = DIRECTION('',(-1.,0.,0.)) ;
#20988 = DIRECTION('center_axis',(-1.,0.,0.)) ;
#20989 = DIRECTION('ref_axis',(0.,-0.743144825477395,-0.669130606358858)) ;
#20990 = DIRECTION('',(-1.,0.,0.)) ;
#20991 = DIRECTION('center_axis',(-1.,0.,0.)) ;
#20992 = DIRECTION('ref_axis',(0.,-0.743144825477395,-0.669130606358858)) ;
#20993 = DIRECTION('center_axis',(1.,0.,0.)) ;
#20994 = DIRECTION('ref_axis',(0.,0.669130606358858,0.743144825477394)) ;
#20995 = DIRECTION('center_axis',(1.,0.,0.)) ;
#20996 = DIRECTION('ref_axis',(0.,0.669130606358858,0.743144825477394)) ;
#20997 = DIRECTION('center_axis',(1.,0.,0.)) ;
#20998 = DIRECTION('ref_axis',(0.,0.669130606358858,0.743144825477394)) ;
#20999 = DIRECTION('center_axis',(1.,0.,0.)) ;
#21000 = DIRECTION('ref_axis',(0.,0.669130606358858,0.743144825477394)) ;
#21001 = DIRECTION('center_axis',(1.,0.,0.)) ;
#21002 = DIRECTION('ref_axis',(0.,0.669130606358858,0.743144825477394)) ;
#21003 = DIRECTION('center_axis',(1.,0.,0.)) ;
#21004 = DIRECTION('ref_axis',(0.,0.669130606358858,0.743144825477394)) ;
#21005 = DIRECTION('center_axis',(1.,0.,0.)) ;
#21006 = DIRECTION('ref_axis',(0.,0.669130606358858,0.743144825477394)) ;
#21007 = DIRECTION('center_axis',(1.,0.,0.)) ;
#21008 = DIRECTION('ref_axis',(0.,0.669130606358858,0.743144825477394)) ;
#21009 = DIRECTION('center_axis',(-1.,0.,0.)) ;
#21010 = DIRECTION('ref_axis',(0.,-0.669130606358858,-0.743144825477394)) ;
#21011 = DIRECTION('',(-1.,0.,0.)) ;
#21012 = DIRECTION('center_axis',(-1.,0.,0.)) ;
#21013 = DIRECTION('ref_axis',(0.,-0.669130606358858,-0.743144825477394)) ;
#21014 = DIRECTION('',(-1.,0.,0.)) ;
#21015 = DIRECTION('center_axis',(-1.,0.,0.)) ;
#21016 = DIRECTION('ref_axis',(0.,-0.669130606358858,-0.743144825477394)) ;
#21017 = DIRECTION('center_axis',(1.,0.,0.)) ;
#21018 = DIRECTION('ref_axis',(0.,0.809016994374948,0.587785252292473)) ;
#21019 = DIRECTION('center_axis',(1.,0.,0.)) ;
#21020 = DIRECTION('ref_axis',(0.,0.809016994374948,0.587785252292473)) ;
#21021 = DIRECTION('center_axis',(1.,0.,0.)) ;
#21022 = DIRECTION('ref_axis',(0.,0.809016994374948,0.587785252292473)) ;
#21023 = DIRECTION('center_axis',(1.,0.,0.)) ;
#21024 = DIRECTION('ref_axis',(0.,0.809016994374948,0.587785252292473)) ;
#21025 = DIRECTION('center_axis',(1.,0.,0.)) ;
#21026 = DIRECTION('ref_axis',(0.,0.809016994374948,0.587785252292473)) ;
#21027 = DIRECTION('center_axis',(1.,0.,0.)) ;
#21028 = DIRECTION('ref_axis',(0.,0.809016994374948,0.587785252292473)) ;
#21029 = DIRECTION('center_axis',(1.,0.,0.)) ;
#21030 = DIRECTION('ref_axis',(0.,0.809016994374948,0.587785252292473)) ;
#21031 = DIRECTION('center_axis',(1.,0.,0.)) ;
#21032 = DIRECTION('ref_axis',(0.,0.809016994374948,0.587785252292473)) ;
#21033 = DIRECTION('center_axis',(-1.,0.,0.)) ;
#21034 = DIRECTION('ref_axis',(0.,-0.809016994374948,-0.587785252292473)) ;
#21035 = DIRECTION('',(-1.,0.,0.)) ;
#21036 = DIRECTION('center_axis',(-1.,0.,0.)) ;
#21037 = DIRECTION('ref_axis',(0.,-0.809016994374948,-0.587785252292473)) ;
#21038 = DIRECTION('',(-1.,0.,0.)) ;
#21039 = DIRECTION('center_axis',(-1.,0.,0.)) ;
#21040 = DIRECTION('ref_axis',(0.,-0.809016994374948,-0.587785252292473)) ;
#21041 = DIRECTION('center_axis',(1.,0.,0.)) ;
#21042 = DIRECTION('ref_axis',(0.,0.866025403784439,0.499999999999999)) ;
#21043 = DIRECTION('center_axis',(1.,0.,0.)) ;
#21044 = DIRECTION('ref_axis',(0.,0.866025403784439,0.499999999999999)) ;
#21045 = DIRECTION('center_axis',(1.,0.,0.)) ;
#21046 = DIRECTION('ref_axis',(0.,0.866025403784439,0.499999999999999)) ;
#21047 = DIRECTION('center_axis',(1.,0.,0.)) ;
#21048 = DIRECTION('ref_axis',(0.,0.866025403784439,0.499999999999999)) ;
#21049 = DIRECTION('center_axis',(1.,0.,0.)) ;
#21050 = DIRECTION('ref_axis',(0.,0.866025403784439,0.499999999999999)) ;
#21051 = DIRECTION('center_axis',(1.,0.,0.)) ;
#21052 = DIRECTION('ref_axis',(0.,0.866025403784439,0.499999999999999)) ;
#21053 = DIRECTION('center_axis',(1.,0.,0.)) ;
#21054 = DIRECTION('ref_axis',(0.,0.866025403784439,0.499999999999999)) ;
#21055 = DIRECTION('center_axis',(1.,0.,0.)) ;
#21056 = DIRECTION('ref_axis',(0.,0.866025403784439,0.499999999999999)) ;
#21057 = DIRECTION('center_axis',(-1.,0.,0.)) ;
#21058 = DIRECTION('ref_axis',(0.,-0.866025403784439,-0.499999999999999)) ;
#21059 = DIRECTION('',(-1.,0.,0.)) ;
#21060 = DIRECTION('center_axis',(-1.,0.,0.)) ;
#21061 = DIRECTION('ref_axis',(0.,-0.866025403784439,-0.499999999999999)) ;
#21062 = DIRECTION('',(-1.,0.,0.)) ;
#21063 = DIRECTION('center_axis',(-1.,0.,0.)) ;
#21064 = DIRECTION('ref_axis',(0.,-0.866025403784439,-0.499999999999999)) ;
#21065 = DIRECTION('center_axis',(1.,0.,0.)) ;
#21066 = DIRECTION('ref_axis',(0.,0.913545457642601,0.4067366430758)) ;
#21067 = DIRECTION('center_axis',(1.,0.,0.)) ;
#21068 = DIRECTION('ref_axis',(0.,0.913545457642601,0.4067366430758)) ;
#21069 = DIRECTION('center_axis',(1.,0.,0.)) ;
#21070 = DIRECTION('ref_axis',(0.,0.913545457642601,0.4067366430758)) ;
#21071 = DIRECTION('center_axis',(1.,0.,0.)) ;
#21072 = DIRECTION('ref_axis',(0.,0.913545457642601,0.4067366430758)) ;
#21073 = DIRECTION('center_axis',(1.,0.,0.)) ;
#21074 = DIRECTION('ref_axis',(0.,0.913545457642601,0.4067366430758)) ;
#21075 = DIRECTION('center_axis',(1.,0.,0.)) ;
#21076 = DIRECTION('ref_axis',(0.,0.913545457642601,0.4067366430758)) ;
#21077 = DIRECTION('center_axis',(1.,0.,0.)) ;
#21078 = DIRECTION('ref_axis',(0.,0.913545457642601,0.4067366430758)) ;
#21079 = DIRECTION('center_axis',(1.,0.,0.)) ;
#21080 = DIRECTION('ref_axis',(0.,0.913545457642601,0.4067366430758)) ;
#21081 = DIRECTION('center_axis',(-1.,0.,0.)) ;
#21082 = DIRECTION('ref_axis',(0.,-0.913545457642601,-0.4067366430758)) ;
#21083 = DIRECTION('',(-1.,0.,0.)) ;
#21084 = DIRECTION('center_axis',(-1.,0.,0.)) ;
#21085 = DIRECTION('ref_axis',(0.,-0.913545457642601,-0.4067366430758)) ;
#21086 = DIRECTION('',(-1.,0.,0.)) ;
#21087 = DIRECTION('center_axis',(-1.,0.,0.)) ;
#21088 = DIRECTION('ref_axis',(0.,-0.913545457642601,-0.4067366430758)) ;
#21089 = DIRECTION('center_axis',(1.,0.,0.)) ;
#21090 = DIRECTION('ref_axis',(0.,0.951056516295154,0.309016994374947)) ;
#21091 = DIRECTION('center_axis',(1.,0.,0.)) ;
#21092 = DIRECTION('ref_axis',(0.,0.951056516295154,0.309016994374947)) ;
#21093 = DIRECTION('center_axis',(1.,0.,0.)) ;
#21094 = DIRECTION('ref_axis',(0.,0.951056516295154,0.309016994374947)) ;
#21095 = DIRECTION('center_axis',(1.,0.,0.)) ;
#21096 = DIRECTION('ref_axis',(0.,0.951056516295154,0.309016994374947)) ;
#21097 = DIRECTION('center_axis',(1.,0.,0.)) ;
#21098 = DIRECTION('ref_axis',(0.,0.951056516295154,0.309016994374947)) ;
#21099 = DIRECTION('center_axis',(1.,0.,0.)) ;
#21100 = DIRECTION('ref_axis',(0.,0.951056516295154,0.309016994374947)) ;
#21101 = DIRECTION('center_axis',(1.,0.,0.)) ;
#21102 = DIRECTION('ref_axis',(0.,0.951056516295154,0.309016994374947)) ;
#21103 = DIRECTION('center_axis',(1.,0.,0.)) ;
#21104 = DIRECTION('ref_axis',(0.,0.951056516295154,0.309016994374947)) ;
#21105 = DIRECTION('center_axis',(-1.,0.,0.)) ;
#21106 = DIRECTION('ref_axis',(0.,-0.951056516295154,-0.309016994374947)) ;
#21107 = DIRECTION('',(-1.,0.,0.)) ;
#21108 = DIRECTION('center_axis',(-1.,0.,0.)) ;
#21109 = DIRECTION('ref_axis',(0.,-0.951056516295154,-0.309016994374947)) ;
#21110 = DIRECTION('',(-1.,0.,0.)) ;
#21111 = DIRECTION('center_axis',(-1.,0.,0.)) ;
#21112 = DIRECTION('ref_axis',(0.,-0.951056516295154,-0.309016994374947)) ;
#21113 = DIRECTION('center_axis',(1.,0.,0.)) ;
#21114 = DIRECTION('ref_axis',(0.,0.978147600733806,0.207911690817759)) ;
#21115 = DIRECTION('center_axis',(1.,0.,0.)) ;
#21116 = DIRECTION('ref_axis',(0.,0.978147600733806,0.207911690817759)) ;
#21117 = DIRECTION('center_axis',(1.,0.,0.)) ;
#21118 = DIRECTION('ref_axis',(0.,0.978147600733806,0.207911690817759)) ;
#21119 = DIRECTION('center_axis',(1.,0.,0.)) ;
#21120 = DIRECTION('ref_axis',(0.,0.978147600733806,0.207911690817759)) ;
#21121 = DIRECTION('center_axis',(1.,0.,0.)) ;
#21122 = DIRECTION('ref_axis',(0.,0.978147600733806,0.207911690817759)) ;
#21123 = DIRECTION('center_axis',(1.,0.,0.)) ;
#21124 = DIRECTION('ref_axis',(0.,0.978147600733806,0.207911690817759)) ;
#21125 = DIRECTION('center_axis',(1.,0.,0.)) ;
#21126 = DIRECTION('ref_axis',(0.,0.978147600733806,0.207911690817759)) ;
#21127 = DIRECTION('center_axis',(1.,0.,0.)) ;
#21128 = DIRECTION('ref_axis',(0.,0.978147600733806,0.207911690817759)) ;
#21129 = DIRECTION('center_axis',(-1.,0.,0.)) ;
#21130 = DIRECTION('ref_axis',(0.,-0.978147600733806,-0.207911690817759)) ;
#21131 = DIRECTION('',(-1.,0.,0.)) ;
#21132 = DIRECTION('center_axis',(-1.,0.,0.)) ;
#21133 = DIRECTION('ref_axis',(0.,-0.978147600733806,-0.207911690817759)) ;
#21134 = DIRECTION('',(-1.,0.,0.)) ;
#21135 = DIRECTION('center_axis',(-1.,0.,0.)) ;
#21136 = DIRECTION('ref_axis',(0.,-0.978147600733806,-0.207911690817759)) ;
#21137 = DIRECTION('center_axis',(1.,0.,0.)) ;
#21138 = DIRECTION('ref_axis',(0.,0.994521895368273,0.104528463267653)) ;
#21139 = DIRECTION('center_axis',(1.,0.,0.)) ;
#21140 = DIRECTION('ref_axis',(0.,0.994521895368273,0.104528463267653)) ;
#21141 = DIRECTION('center_axis',(1.,0.,0.)) ;
#21142 = DIRECTION('ref_axis',(0.,0.994521895368273,0.104528463267653)) ;
#21143 = DIRECTION('center_axis',(1.,0.,0.)) ;
#21144 = DIRECTION('ref_axis',(0.,0.994521895368273,0.104528463267653)) ;
#21145 = DIRECTION('center_axis',(1.,0.,0.)) ;
#21146 = DIRECTION('ref_axis',(0.,0.994521895368273,0.104528463267653)) ;
#21147 = DIRECTION('center_axis',(1.,0.,0.)) ;
#21148 = DIRECTION('ref_axis',(0.,0.994521895368273,0.104528463267653)) ;
#21149 = DIRECTION('center_axis',(1.,0.,0.)) ;
#21150 = DIRECTION('ref_axis',(0.,0.994521895368273,0.104528463267653)) ;
#21151 = DIRECTION('center_axis',(1.,0.,0.)) ;
#21152 = DIRECTION('ref_axis',(0.,0.994521895368273,0.104528463267653)) ;
#21153 = DIRECTION('center_axis',(-1.,0.,0.)) ;
#21154 = DIRECTION('ref_axis',(0.,-0.994521895368273,-0.104528463267653)) ;
#21155 = DIRECTION('',(-1.,0.,0.)) ;
#21156 = DIRECTION('center_axis',(-1.,0.,0.)) ;
#21157 = DIRECTION('ref_axis',(0.,-0.994521895368273,-0.104528463267653)) ;
#21158 = DIRECTION('',(-1.,0.,0.)) ;
#21159 = DIRECTION('center_axis',(-1.,0.,0.)) ;
#21160 = DIRECTION('ref_axis',(0.,-0.994521895368273,-0.104528463267653)) ;
#21161 = DIRECTION('center_axis',(1.,0.,0.)) ;
#21162 = DIRECTION('ref_axis',(0.,1.,-6.12323399573677E-17)) ;
#21163 = DIRECTION('center_axis',(1.,0.,0.)) ;
#21164 = DIRECTION('ref_axis',(0.,1.,-6.12323399573677E-17)) ;
#21165 = DIRECTION('center_axis',(1.,0.,0.)) ;
#21166 = DIRECTION('ref_axis',(0.,1.,-6.12323399573677E-17)) ;
#21167 = DIRECTION('center_axis',(1.,0.,0.)) ;
#21168 = DIRECTION('ref_axis',(0.,1.,-6.12323399573677E-17)) ;
#21169 = DIRECTION('center_axis',(1.,0.,0.)) ;
#21170 = DIRECTION('ref_axis',(0.,1.,-6.12323399573677E-17)) ;
#21171 = DIRECTION('center_axis',(1.,0.,0.)) ;
#21172 = DIRECTION('ref_axis',(0.,1.,-6.12323399573677E-17)) ;
#21173 = DIRECTION('center_axis',(1.,0.,0.)) ;
#21174 = DIRECTION('ref_axis',(0.,1.,-6.12323399573677E-17)) ;
#21175 = DIRECTION('center_axis',(1.,0.,0.)) ;
#21176 = DIRECTION('ref_axis',(0.,1.,-6.12323399573677E-17)) ;
#21177 = DIRECTION('center_axis',(-1.,0.,0.)) ;
#21178 = DIRECTION('ref_axis',(0.,-1.,6.12323399573677E-17)) ;
#21179 = DIRECTION('',(-1.,0.,0.)) ;
#21180 = DIRECTION('center_axis',(-1.,0.,0.)) ;
#21181 = DIRECTION('ref_axis',(0.,-1.,6.12323399573677E-17)) ;
#21182 = DIRECTION('',(-1.,0.,0.)) ;
#21183 = DIRECTION('center_axis',(-1.,0.,0.)) ;
#21184 = DIRECTION('ref_axis',(0.,-1.,6.12323399573677E-17)) ;
#21185 = DIRECTION('center_axis',(1.,0.,0.)) ;
#21186 = DIRECTION('ref_axis',(0.,0.994521895368273,-0.104528463267653)) ;
#21187 = DIRECTION('center_axis',(1.,0.,0.)) ;
#21188 = DIRECTION('ref_axis',(0.,0.994521895368273,-0.104528463267653)) ;
#21189 = DIRECTION('center_axis',(1.,0.,0.)) ;
#21190 = DIRECTION('ref_axis',(0.,0.994521895368273,-0.104528463267653)) ;
#21191 = DIRECTION('center_axis',(1.,0.,0.)) ;
#21192 = DIRECTION('ref_axis',(0.,0.994521895368273,-0.104528463267653)) ;
#21193 = DIRECTION('center_axis',(1.,0.,0.)) ;
#21194 = DIRECTION('ref_axis',(0.,0.994521895368273,-0.104528463267653)) ;
#21195 = DIRECTION('center_axis',(1.,0.,0.)) ;
#21196 = DIRECTION('ref_axis',(0.,0.994521895368273,-0.104528463267653)) ;
#21197 = DIRECTION('center_axis',(1.,0.,0.)) ;
#21198 = DIRECTION('ref_axis',(0.,0.994521895368273,-0.104528463267653)) ;
#21199 = DIRECTION('center_axis',(1.,0.,0.)) ;
#21200 = DIRECTION('ref_axis',(0.,0.994521895368273,-0.104528463267653)) ;
#21201 = DIRECTION('center_axis',(-1.,0.,0.)) ;
#21202 = DIRECTION('ref_axis',(0.,-0.994521895368273,0.104528463267653)) ;
#21203 = DIRECTION('',(-1.,0.,0.)) ;
#21204 = DIRECTION('center_axis',(-1.,0.,0.)) ;
#21205 = DIRECTION('ref_axis',(0.,-0.994521895368273,0.104528463267653)) ;
#21206 = DIRECTION('',(-1.,0.,0.)) ;
#21207 = DIRECTION('center_axis',(-1.,0.,0.)) ;
#21208 = DIRECTION('ref_axis',(0.,-0.994521895368273,0.104528463267653)) ;
#21209 = DIRECTION('center_axis',(1.,0.,0.)) ;
#21210 = DIRECTION('ref_axis',(0.,0.978147600733806,-0.207911690817759)) ;
#21211 = DIRECTION('center_axis',(1.,0.,0.)) ;
#21212 = DIRECTION('ref_axis',(0.,0.978147600733806,-0.207911690817759)) ;
#21213 = DIRECTION('center_axis',(1.,0.,0.)) ;
#21214 = DIRECTION('ref_axis',(0.,0.978147600733806,-0.207911690817759)) ;
#21215 = DIRECTION('center_axis',(1.,0.,0.)) ;
#21216 = DIRECTION('ref_axis',(0.,0.978147600733806,-0.207911690817759)) ;
#21217 = DIRECTION('center_axis',(1.,0.,0.)) ;
#21218 = DIRECTION('ref_axis',(0.,0.978147600733806,-0.207911690817759)) ;
#21219 = DIRECTION('center_axis',(1.,0.,0.)) ;
#21220 = DIRECTION('ref_axis',(0.,0.978147600733806,-0.207911690817759)) ;
#21221 = DIRECTION('center_axis',(1.,0.,0.)) ;
#21222 = DIRECTION('ref_axis',(0.,0.978147600733806,-0.207911690817759)) ;
#21223 = DIRECTION('center_axis',(1.,0.,0.)) ;
#21224 = DIRECTION('ref_axis',(0.,0.978147600733806,-0.207911690817759)) ;
#21225 = DIRECTION('center_axis',(-1.,0.,0.)) ;
#21226 = DIRECTION('ref_axis',(0.,-0.978147600733806,0.207911690817759)) ;
#21227 = DIRECTION('',(-1.,0.,0.)) ;
#21228 = DIRECTION('center_axis',(-1.,0.,0.)) ;
#21229 = DIRECTION('ref_axis',(0.,-0.978147600733806,0.207911690817759)) ;
#21230 = DIRECTION('',(-1.,0.,0.)) ;
#21231 = DIRECTION('center_axis',(-1.,0.,0.)) ;
#21232 = DIRECTION('ref_axis',(0.,-0.978147600733806,0.207911690817759)) ;
#21233 = DIRECTION('center_axis',(1.,0.,0.)) ;
#21234 = DIRECTION('ref_axis',(0.,0.951056516295154,-0.309016994374947)) ;
#21235 = DIRECTION('center_axis',(1.,0.,0.)) ;
#21236 = DIRECTION('ref_axis',(0.,0.951056516295154,-0.309016994374947)) ;
#21237 = DIRECTION('center_axis',(1.,0.,0.)) ;
#21238 = DIRECTION('ref_axis',(0.,0.951056516295154,-0.309016994374947)) ;
#21239 = DIRECTION('center_axis',(1.,0.,0.)) ;
#21240 = DIRECTION('ref_axis',(0.,0.951056516295154,-0.309016994374947)) ;
#21241 = DIRECTION('center_axis',(1.,0.,0.)) ;
#21242 = DIRECTION('ref_axis',(0.,0.951056516295154,-0.309016994374947)) ;
#21243 = DIRECTION('center_axis',(1.,0.,0.)) ;
#21244 = DIRECTION('ref_axis',(0.,0.951056516295154,-0.309016994374947)) ;
#21245 = DIRECTION('center_axis',(1.,0.,0.)) ;
#21246 = DIRECTION('ref_axis',(0.,0.951056516295154,-0.309016994374947)) ;
#21247 = DIRECTION('center_axis',(1.,0.,0.)) ;
#21248 = DIRECTION('ref_axis',(0.,0.951056516295154,-0.309016994374947)) ;
#21249 = DIRECTION('center_axis',(-1.,0.,0.)) ;
#21250 = DIRECTION('ref_axis',(0.,-0.951056516295154,0.309016994374947)) ;
#21251 = DIRECTION('',(-1.,0.,0.)) ;
#21252 = DIRECTION('center_axis',(-1.,0.,0.)) ;
#21253 = DIRECTION('ref_axis',(0.,-0.951056516295154,0.309016994374947)) ;
#21254 = DIRECTION('',(-1.,0.,0.)) ;
#21255 = DIRECTION('center_axis',(-1.,0.,0.)) ;
#21256 = DIRECTION('ref_axis',(0.,-0.951056516295154,0.309016994374947)) ;
#21257 = DIRECTION('center_axis',(1.,0.,0.)) ;
#21258 = DIRECTION('ref_axis',(0.,0.913545457642601,-0.4067366430758)) ;
#21259 = DIRECTION('center_axis',(1.,0.,0.)) ;
#21260 = DIRECTION('ref_axis',(0.,0.913545457642601,-0.4067366430758)) ;
#21261 = DIRECTION('center_axis',(1.,0.,0.)) ;
#21262 = DIRECTION('ref_axis',(0.,0.913545457642601,-0.4067366430758)) ;
#21263 = DIRECTION('center_axis',(1.,0.,0.)) ;
#21264 = DIRECTION('ref_axis',(0.,0.913545457642601,-0.4067366430758)) ;
#21265 = DIRECTION('center_axis',(1.,0.,0.)) ;
#21266 = DIRECTION('ref_axis',(0.,0.913545457642601,-0.4067366430758)) ;
#21267 = DIRECTION('center_axis',(1.,0.,0.)) ;
#21268 = DIRECTION('ref_axis',(0.,0.913545457642601,-0.4067366430758)) ;
#21269 = DIRECTION('center_axis',(1.,0.,0.)) ;
#21270 = DIRECTION('ref_axis',(0.,0.913545457642601,-0.4067366430758)) ;
#21271 = DIRECTION('center_axis',(1.,0.,0.)) ;
#21272 = DIRECTION('ref_axis',(0.,0.913545457642601,-0.4067366430758)) ;
#21273 = DIRECTION('center_axis',(-1.,0.,0.)) ;
#21274 = DIRECTION('ref_axis',(0.,-0.913545457642601,0.4067366430758)) ;
#21275 = DIRECTION('',(-1.,0.,0.)) ;
#21276 = DIRECTION('center_axis',(-1.,0.,0.)) ;
#21277 = DIRECTION('ref_axis',(0.,-0.913545457642601,0.4067366430758)) ;
#21278 = DIRECTION('',(-1.,0.,0.)) ;
#21279 = DIRECTION('center_axis',(-1.,0.,0.)) ;
#21280 = DIRECTION('ref_axis',(0.,-0.913545457642601,0.4067366430758)) ;
#21281 = DIRECTION('center_axis',(1.,0.,0.)) ;
#21282 = DIRECTION('ref_axis',(0.,0.866025403784439,-0.5)) ;
#21283 = DIRECTION('center_axis',(1.,0.,0.)) ;
#21284 = DIRECTION('ref_axis',(0.,0.866025403784439,-0.5)) ;
#21285 = DIRECTION('center_axis',(1.,0.,0.)) ;
#21286 = DIRECTION('ref_axis',(0.,0.866025403784439,-0.5)) ;
#21287 = DIRECTION('center_axis',(1.,0.,0.)) ;
#21288 = DIRECTION('ref_axis',(0.,0.866025403784439,-0.5)) ;
#21289 = DIRECTION('center_axis',(1.,0.,0.)) ;
#21290 = DIRECTION('ref_axis',(0.,0.866025403784439,-0.5)) ;
#21291 = DIRECTION('center_axis',(1.,0.,0.)) ;
#21292 = DIRECTION('ref_axis',(0.,0.866025403784439,-0.5)) ;
#21293 = DIRECTION('center_axis',(1.,0.,0.)) ;
#21294 = DIRECTION('ref_axis',(0.,0.866025403784439,-0.5)) ;
#21295 = DIRECTION('center_axis',(1.,0.,0.)) ;
#21296 = DIRECTION('ref_axis',(0.,0.866025403784439,-0.5)) ;
#21297 = DIRECTION('center_axis',(-1.,0.,0.)) ;
#21298 = DIRECTION('ref_axis',(0.,-0.866025403784439,0.5)) ;
#21299 = DIRECTION('',(-1.,0.,0.)) ;
#21300 = DIRECTION('center_axis',(-1.,0.,0.)) ;
#21301 = DIRECTION('ref_axis',(0.,-0.866025403784439,0.5)) ;
#21302 = DIRECTION('',(-1.,0.,0.)) ;
#21303 = DIRECTION('center_axis',(-1.,0.,0.)) ;
#21304 = DIRECTION('ref_axis',(0.,-0.866025403784439,0.5)) ;
#21305 = DIRECTION('center_axis',(1.,0.,0.)) ;
#21306 = DIRECTION('ref_axis',(0.,0.587785252292473,-0.809016994374947)) ;
#21307 = DIRECTION('center_axis',(1.,0.,0.)) ;
#21308 = DIRECTION('ref_axis',(0.,0.587785252292473,-0.809016994374947)) ;
#21309 = DIRECTION('center_axis',(1.,0.,0.)) ;
#21310 = DIRECTION('ref_axis',(0.,0.587785252292473,-0.809016994374947)) ;
#21311 = DIRECTION('center_axis',(1.,0.,0.)) ;
#21312 = DIRECTION('ref_axis',(0.,0.587785252292473,-0.809016994374947)) ;
#21313 = DIRECTION('center_axis',(1.,0.,0.)) ;
#21314 = DIRECTION('ref_axis',(0.,0.587785252292473,-0.809016994374947)) ;
#21315 = DIRECTION('center_axis',(1.,0.,0.)) ;
#21316 = DIRECTION('ref_axis',(0.,0.587785252292473,-0.809016994374947)) ;
#21317 = DIRECTION('center_axis',(1.,0.,0.)) ;
#21318 = DIRECTION('ref_axis',(0.,0.587785252292473,-0.809016994374947)) ;
#21319 = DIRECTION('center_axis',(1.,0.,0.)) ;
#21320 = DIRECTION('ref_axis',(0.,0.587785252292473,-0.809016994374947)) ;
#21321 = DIRECTION('center_axis',(-1.,0.,0.)) ;
#21322 = DIRECTION('ref_axis',(0.,-0.587785252292473,0.809016994374947)) ;
#21323 = DIRECTION('',(-1.,0.,0.)) ;
#21324 = DIRECTION('center_axis',(-1.,0.,0.)) ;
#21325 = DIRECTION('ref_axis',(0.,-0.587785252292473,0.809016994374947)) ;
#21326 = DIRECTION('',(-1.,0.,0.)) ;
#21327 = DIRECTION('center_axis',(-1.,0.,0.)) ;
#21328 = DIRECTION('ref_axis',(0.,-0.587785252292473,0.809016994374947)) ;
#21329 = DIRECTION('center_axis',(1.,0.,0.)) ;
#21330 = DIRECTION('ref_axis',(0.,0.669130606358858,-0.743144825477394)) ;
#21331 = DIRECTION('center_axis',(1.,0.,0.)) ;
#21332 = DIRECTION('ref_axis',(0.,0.669130606358858,-0.743144825477394)) ;
#21333 = DIRECTION('center_axis',(1.,0.,0.)) ;
#21334 = DIRECTION('ref_axis',(0.,0.669130606358858,-0.743144825477394)) ;
#21335 = DIRECTION('center_axis',(1.,0.,0.)) ;
#21336 = DIRECTION('ref_axis',(0.,0.669130606358858,-0.743144825477394)) ;
#21337 = DIRECTION('center_axis',(1.,0.,0.)) ;
#21338 = DIRECTION('ref_axis',(0.,0.669130606358858,-0.743144825477394)) ;
#21339 = DIRECTION('center_axis',(1.,0.,0.)) ;
#21340 = DIRECTION('ref_axis',(0.,0.669130606358858,-0.743144825477394)) ;
#21341 = DIRECTION('center_axis',(1.,0.,0.)) ;
#21342 = DIRECTION('ref_axis',(0.,0.669130606358858,-0.743144825477394)) ;
#21343 = DIRECTION('center_axis',(1.,0.,0.)) ;
#21344 = DIRECTION('ref_axis',(0.,0.669130606358858,-0.743144825477394)) ;
#21345 = DIRECTION('center_axis',(-1.,0.,0.)) ;
#21346 = DIRECTION('ref_axis',(0.,-0.669130606358858,0.743144825477394)) ;
#21347 = DIRECTION('',(-1.,0.,0.)) ;
#21348 = DIRECTION('center_axis',(-1.,0.,0.)) ;
#21349 = DIRECTION('ref_axis',(0.,-0.669130606358858,0.743144825477394)) ;
#21350 = DIRECTION('',(-1.,0.,0.)) ;
#21351 = DIRECTION('center_axis',(-1.,0.,0.)) ;
#21352 = DIRECTION('ref_axis',(0.,-0.669130606358858,0.743144825477394)) ;
#21353 = DIRECTION('center_axis',(1.,0.,0.)) ;
#21354 = DIRECTION('ref_axis',(0.,0.743144825477394,-0.669130606358859)) ;
#21355 = DIRECTION('center_axis',(1.,0.,0.)) ;
#21356 = DIRECTION('ref_axis',(0.,0.743144825477394,-0.669130606358859)) ;
#21357 = DIRECTION('center_axis',(1.,0.,0.)) ;
#21358 = DIRECTION('ref_axis',(0.,0.743144825477394,-0.669130606358859)) ;
#21359 = DIRECTION('center_axis',(1.,0.,0.)) ;
#21360 = DIRECTION('ref_axis',(0.,0.743144825477394,-0.669130606358859)) ;
#21361 = DIRECTION('center_axis',(1.,0.,0.)) ;
#21362 = DIRECTION('ref_axis',(0.,0.743144825477394,-0.669130606358859)) ;
#21363 = DIRECTION('center_axis',(1.,0.,0.)) ;
#21364 = DIRECTION('ref_axis',(0.,0.743144825477394,-0.669130606358859)) ;
#21365 = DIRECTION('center_axis',(1.,0.,0.)) ;
#21366 = DIRECTION('ref_axis',(0.,0.743144825477394,-0.669130606358859)) ;
#21367 = DIRECTION('center_axis',(1.,0.,0.)) ;
#21368 = DIRECTION('ref_axis',(0.,0.743144825477394,-0.669130606358859)) ;
#21369 = DIRECTION('center_axis',(-1.,0.,0.)) ;
#21370 = DIRECTION('ref_axis',(0.,-0.743144825477394,0.669130606358859)) ;
#21371 = DIRECTION('',(-1.,0.,0.)) ;
#21372 = DIRECTION('center_axis',(-1.,0.,0.)) ;
#21373 = DIRECTION('ref_axis',(0.,-0.743144825477394,0.669130606358859)) ;
#21374 = DIRECTION('',(-1.,0.,0.)) ;
#21375 = DIRECTION('center_axis',(-1.,0.,0.)) ;
#21376 = DIRECTION('ref_axis',(0.,-0.743144825477394,0.669130606358859)) ;
#21377 = DIRECTION('center_axis',(1.,0.,0.)) ;
#21378 = DIRECTION('ref_axis',(0.,0.809016994374947,-0.587785252292473)) ;
#21379 = DIRECTION('center_axis',(1.,0.,0.)) ;
#21380 = DIRECTION('ref_axis',(0.,0.809016994374947,-0.587785252292473)) ;
#21381 = DIRECTION('center_axis',(1.,0.,0.)) ;
#21382 = DIRECTION('ref_axis',(0.,0.809016994374947,-0.587785252292473)) ;
#21383 = DIRECTION('center_axis',(1.,0.,0.)) ;
#21384 = DIRECTION('ref_axis',(0.,0.809016994374947,-0.587785252292473)) ;
#21385 = DIRECTION('center_axis',(1.,0.,0.)) ;
#21386 = DIRECTION('ref_axis',(0.,0.809016994374947,-0.587785252292473)) ;
#21387 = DIRECTION('center_axis',(1.,0.,0.)) ;
#21388 = DIRECTION('ref_axis',(0.,0.809016994374947,-0.587785252292473)) ;
#21389 = DIRECTION('center_axis',(1.,0.,0.)) ;
#21390 = DIRECTION('ref_axis',(0.,0.809016994374947,-0.587785252292473)) ;
#21391 = DIRECTION('center_axis',(1.,0.,0.)) ;
#21392 = DIRECTION('ref_axis',(0.,0.809016994374947,-0.587785252292473)) ;
#21393 = DIRECTION('center_axis',(-1.,0.,0.)) ;
#21394 = DIRECTION('ref_axis',(0.,-0.809016994374947,0.587785252292473)) ;
#21395 = DIRECTION('',(-1.,0.,0.)) ;
#21396 = DIRECTION('center_axis',(-1.,0.,0.)) ;
#21397 = DIRECTION('ref_axis',(0.,-0.809016994374947,0.587785252292473)) ;
#21398 = DIRECTION('',(-1.,0.,0.)) ;
#21399 = DIRECTION('center_axis',(-1.,0.,0.)) ;
#21400 = DIRECTION('ref_axis',(0.,-0.809016994374947,0.587785252292473)) ;
#21401 = DIRECTION('center_axis',(1.,0.,0.)) ;
#21402 = DIRECTION('ref_axis',(0.,0.5,-0.866025403784439)) ;
#21403 = DIRECTION('center_axis',(1.,0.,0.)) ;
#21404 = DIRECTION('ref_axis',(0.,0.5,-0.866025403784439)) ;
#21405 = DIRECTION('center_axis',(1.,0.,0.)) ;
#21406 = DIRECTION('ref_axis',(0.,0.5,-0.866025403784439)) ;
#21407 = DIRECTION('center_axis',(1.,0.,0.)) ;
#21408 = DIRECTION('ref_axis',(0.,0.5,-0.866025403784439)) ;
#21409 = DIRECTION('center_axis',(1.,0.,0.)) ;
#21410 = DIRECTION('ref_axis',(0.,0.5,-0.866025403784439)) ;
#21411 = DIRECTION('center_axis',(1.,0.,0.)) ;
#21412 = DIRECTION('ref_axis',(0.,0.5,-0.866025403784439)) ;
#21413 = DIRECTION('center_axis',(1.,0.,0.)) ;
#21414 = DIRECTION('ref_axis',(0.,0.5,-0.866025403784439)) ;
#21415 = DIRECTION('center_axis',(1.,0.,0.)) ;
#21416 = DIRECTION('ref_axis',(0.,0.5,-0.866025403784439)) ;
#21417 = DIRECTION('center_axis',(-1.,0.,0.)) ;
#21418 = DIRECTION('ref_axis',(0.,-0.5,0.866025403784439)) ;
#21419 = DIRECTION('',(-1.,0.,0.)) ;
#21420 = DIRECTION('center_axis',(-1.,0.,0.)) ;
#21421 = DIRECTION('ref_axis',(0.,-0.5,0.866025403784439)) ;
#21422 = DIRECTION('',(-1.,0.,0.)) ;
#21423 = DIRECTION('center_axis',(-1.,0.,0.)) ;
#21424 = DIRECTION('ref_axis',(0.,-0.5,0.866025403784439)) ;
#21425 = DIRECTION('center_axis',(1.,0.,0.)) ;
#21426 = DIRECTION('ref_axis',(0.,0.4067366430758,-0.913545457642601)) ;
#21427 = DIRECTION('center_axis',(1.,0.,0.)) ;
#21428 = DIRECTION('ref_axis',(0.,0.4067366430758,-0.913545457642601)) ;
#21429 = DIRECTION('center_axis',(1.,0.,0.)) ;
#21430 = DIRECTION('ref_axis',(0.,0.4067366430758,-0.913545457642601)) ;
#21431 = DIRECTION('center_axis',(1.,0.,0.)) ;
#21432 = DIRECTION('ref_axis',(0.,0.4067366430758,-0.913545457642601)) ;
#21433 = DIRECTION('center_axis',(1.,0.,0.)) ;
#21434 = DIRECTION('ref_axis',(0.,0.4067366430758,-0.913545457642601)) ;
#21435 = DIRECTION('center_axis',(1.,0.,0.)) ;
#21436 = DIRECTION('ref_axis',(0.,0.4067366430758,-0.913545457642601)) ;
#21437 = DIRECTION('center_axis',(1.,0.,0.)) ;
#21438 = DIRECTION('ref_axis',(0.,0.4067366430758,-0.913545457642601)) ;
#21439 = DIRECTION('center_axis',(1.,0.,0.)) ;
#21440 = DIRECTION('ref_axis',(0.,0.4067366430758,-0.913545457642601)) ;
#21441 = DIRECTION('center_axis',(-1.,0.,0.)) ;
#21442 = DIRECTION('ref_axis',(0.,-0.4067366430758,0.913545457642601)) ;
#21443 = DIRECTION('',(-1.,0.,0.)) ;
#21444 = DIRECTION('center_axis',(-1.,0.,0.)) ;
#21445 = DIRECTION('ref_axis',(0.,-0.4067366430758,0.913545457642601)) ;
#21446 = DIRECTION('',(-1.,0.,0.)) ;
#21447 = DIRECTION('center_axis',(-1.,0.,0.)) ;
#21448 = DIRECTION('ref_axis',(0.,-0.4067366430758,0.913545457642601)) ;
#21449 = DIRECTION('center_axis',(1.,0.,0.)) ;
#21450 = DIRECTION('ref_axis',(0.,0.309016994374947,-0.951056516295154)) ;
#21451 = DIRECTION('center_axis',(1.,0.,0.)) ;
#21452 = DIRECTION('ref_axis',(0.,0.309016994374947,-0.951056516295154)) ;
#21453 = DIRECTION('center_axis',(1.,0.,0.)) ;
#21454 = DIRECTION('ref_axis',(0.,0.309016994374947,-0.951056516295154)) ;
#21455 = DIRECTION('center_axis',(1.,0.,0.)) ;
#21456 = DIRECTION('ref_axis',(0.,0.309016994374947,-0.951056516295154)) ;
#21457 = DIRECTION('center_axis',(1.,0.,0.)) ;
#21458 = DIRECTION('ref_axis',(0.,0.309016994374947,-0.951056516295154)) ;
#21459 = DIRECTION('center_axis',(1.,0.,0.)) ;
#21460 = DIRECTION('ref_axis',(0.,0.309016994374947,-0.951056516295154)) ;
#21461 = DIRECTION('center_axis',(1.,0.,0.)) ;
#21462 = DIRECTION('ref_axis',(0.,0.309016994374947,-0.951056516295154)) ;
#21463 = DIRECTION('center_axis',(1.,0.,0.)) ;
#21464 = DIRECTION('ref_axis',(0.,0.309016994374947,-0.951056516295154)) ;
#21465 = DIRECTION('center_axis',(-1.,0.,0.)) ;
#21466 = DIRECTION('ref_axis',(0.,-0.309016994374947,0.951056516295154)) ;
#21467 = DIRECTION('',(-1.,0.,0.)) ;
#21468 = DIRECTION('center_axis',(-1.,0.,0.)) ;
#21469 = DIRECTION('ref_axis',(0.,-0.309016994374947,0.951056516295154)) ;
#21470 = DIRECTION('',(-1.,0.,0.)) ;
#21471 = DIRECTION('center_axis',(-1.,0.,0.)) ;
#21472 = DIRECTION('ref_axis',(0.,-0.309016994374947,0.951056516295154)) ;
#21473 = DIRECTION('center_axis',(1.,0.,0.)) ;
#21474 = DIRECTION('ref_axis',(0.,0.207911690817759,-0.978147600733806)) ;
#21475 = DIRECTION('center_axis',(1.,0.,0.)) ;
#21476 = DIRECTION('ref_axis',(0.,0.207911690817759,-0.978147600733806)) ;
#21477 = DIRECTION('center_axis',(1.,0.,0.)) ;
#21478 = DIRECTION('ref_axis',(0.,0.207911690817759,-0.978147600733806)) ;
#21479 = DIRECTION('center_axis',(1.,0.,0.)) ;
#21480 = DIRECTION('ref_axis',(0.,0.207911690817759,-0.978147600733806)) ;
#21481 = DIRECTION('center_axis',(1.,0.,0.)) ;
#21482 = DIRECTION('ref_axis',(0.,0.207911690817759,-0.978147600733806)) ;
#21483 = DIRECTION('center_axis',(1.,0.,0.)) ;
#21484 = DIRECTION('ref_axis',(0.,0.207911690817759,-0.978147600733806)) ;
#21485 = DIRECTION('center_axis',(1.,0.,0.)) ;
#21486 = DIRECTION('ref_axis',(0.,0.207911690817759,-0.978147600733806)) ;
#21487 = DIRECTION('center_axis',(1.,0.,0.)) ;
#21488 = DIRECTION('ref_axis',(0.,0.207911690817759,-0.978147600733806)) ;
#21489 = DIRECTION('center_axis',(-1.,0.,0.)) ;
#21490 = DIRECTION('ref_axis',(0.,-0.207911690817759,0.978147600733806)) ;
#21491 = DIRECTION('',(-1.,0.,0.)) ;
#21492 = DIRECTION('center_axis',(-1.,0.,0.)) ;
#21493 = DIRECTION('ref_axis',(0.,-0.207911690817759,0.978147600733806)) ;
#21494 = DIRECTION('',(-1.,0.,0.)) ;
#21495 = DIRECTION('center_axis',(-1.,0.,0.)) ;
#21496 = DIRECTION('ref_axis',(0.,-0.207911690817759,0.978147600733806)) ;
#21497 = DIRECTION('center_axis',(1.,0.,0.)) ;
#21498 = DIRECTION('ref_axis',(0.,-1.,-6.12323399573677E-17)) ;
#21499 = DIRECTION('axis',(0.,0.,1.)) ;
#21500 = DIRECTION('refdir',(1.,0.,0.)) ;
#21501 = DIRECTION('center_axis',(-1.,-6.12323399573677E-17,0.)) ;
#21502 = DIRECTION('ref_axis',(6.12323399573677E-17,-1.,0.)) ;
#21503 = DIRECTION('center_axis',(-1.,-6.12323399573677E-17,0.)) ;
#21504 = DIRECTION('ref_axis',(6.12323399573677E-17,-1.,0.)) ;
#21505 = DIRECTION('center_axis',(-1.,-6.12323399573677E-17,0.)) ;
#21506 = DIRECTION('ref_axis',(6.12323399573677E-17,-1.,0.)) ;
#21507 = DIRECTION('',(-1.,-6.12323399573677E-17,0.)) ;
#21508 = DIRECTION('center_axis',(-1.,-6.12323399573677E-17,0.)) ;
#21509 = DIRECTION('ref_axis',(6.12323399573677E-17,-1.,0.)) ;
#21510 = DIRECTION('center_axis',(-1.,-6.12323399573677E-17,0.)) ;
#21511 = DIRECTION('ref_axis',(6.12323399573677E-17,-1.,0.)) ;
#21512 = DIRECTION('',(-0.707106781186547,0.707106781186548,-8.65956056235494E-17)) ;
#21513 = DIRECTION('center_axis',(-1.,-6.12323399573677E-17,0.)) ;
#21514 = DIRECTION('ref_axis',(6.12323399573677E-17,-1.,0.)) ;
#21515 = DIRECTION('center_axis',(-1.,-6.12323399573677E-17,0.)) ;
#21516 = DIRECTION('ref_axis',(6.12323399573677E-17,-1.,0.)) ;
#21517 = DIRECTION('center_axis',(-1.,-6.12323399573677E-17,0.)) ;
#21518 = DIRECTION('ref_axis',(6.12323399573677E-17,-1.,0.)) ;
#21519 = DIRECTION('center_axis',(1.,6.12323399573677E-17,0.)) ;
#21520 = DIRECTION('ref_axis',(-6.12323399573677E-17,1.,0.)) ;
#21521 = DIRECTION('center_axis',(-1.,-6.12323399573677E-17,0.)) ;
#21522 = DIRECTION('ref_axis',(6.12323399573677E-17,-1.,0.)) ;
#21523 = DIRECTION('',(-0.707106781186547,0.707106781186548,8.65956056235494E-17)) ;
#21524 = DIRECTION('center_axis',(-1.,-6.12323399573677E-17,0.)) ;
#21525 = DIRECTION('ref_axis',(6.12323399573677E-17,-1.,0.)) ;
#21526 = DIRECTION('center_axis',(-1.,-6.12323399573677E-17,0.)) ;
#21527 = DIRECTION('ref_axis',(6.12323399573677E-17,-1.,0.)) ;
#21528 = DIRECTION('',(1.,6.12323399573677E-17,0.)) ;
#21529 = DIRECTION('center_axis',(-1.,-6.12323399573677E-17,0.)) ;
#21530 = DIRECTION('ref_axis',(6.12323399573677E-17,-1.,0.)) ;
#21531 = DIRECTION('center_axis',(-1.,-6.12323399573677E-17,0.)) ;
#21532 = DIRECTION('ref_axis',(6.12323399573677E-17,-1.,0.)) ;
#21533 = DIRECTION('',(0.707106781186548,-0.707106781186547,8.65956056235493E-17)) ;
#21534 = DIRECTION('center_axis',(-1.,-6.12323399573677E-17,0.)) ;
#21535 = DIRECTION('ref_axis',(6.12323399573677E-17,-1.,0.)) ;
#21536 = DIRECTION('center_axis',(1.,6.12323399573677E-17,0.)) ;
#21537 = DIRECTION('ref_axis',(-6.12323399573677E-17,1.,0.)) ;
#21538 = DIRECTION('center_axis',(-1.,-6.12323399573677E-17,0.)) ;
#21539 = DIRECTION('ref_axis',(6.12323399573677E-17,-1.,0.)) ;
#21540 = DIRECTION('center_axis',(1.,6.12323399573677E-17,0.)) ;
#21541 = DIRECTION('ref_axis',(-6.12323399573677E-17,1.,0.)) ;
#21542 = DIRECTION('',(0.707106781186548,-0.707106781186547,-8.65956056235493E-17)) ;
#21543 = DIRECTION('axis',(0.,0.,1.)) ;
#21544 = DIRECTION('refdir',(1.,0.,0.)) ;
#21545 = DIRECTION('center_axis',(-1.83697019872103E-16,-1.,0.)) ;
#21546 = DIRECTION('ref_axis',(-1.,1.83697019872103E-16,0.)) ;
#21547 = DIRECTION('',(0.,0.,1.)) ;
#21548 = DIRECTION('',(1.,-1.83697019872103E-16,0.)) ;
#21549 = DIRECTION('',(0.,0.,-1.)) ;
#21550 = DIRECTION('center_axis',(1.83697019872103E-16,1.,0.)) ;
#21551 = DIRECTION('ref_axis',(1.,-1.83697019872103E-16,0.)) ;
#21552 = DIRECTION('',(0.,0.,-1.)) ;
#21553 = DIRECTION('',(-1.,1.83697019872103E-16,0.)) ;
#21554 = DIRECTION('',(0.,0.,-1.)) ;
#21555 = DIRECTION('center_axis',(0.,0.,-1.)) ;
#21556 = DIRECTION('ref_axis',(-1.83697019872103E-16,-1.,0.)) ;
#21557 = DIRECTION('center_axis',(0.,0.,-1.)) ;
#21558 = DIRECTION('ref_axis',(1.,0.,0.)) ;
#21559 = DIRECTION('center_axis',(0.,0.,-1.)) ;
#21560 = DIRECTION('ref_axis',(-1.83697019872103E-16,-1.,0.)) ;
#21561 = DIRECTION('center_axis',(0.,0.,1.)) ;
#21562 = DIRECTION('ref_axis',(1.,0.,0.)) ;
#21563 = DIRECTION('center_axis',(0.,0.,1.)) ;
#21564 = DIRECTION('ref_axis',(1.,0.,0.)) ;
#21565 = DIRECTION('',(1.22464679914735E-16,1.,0.)) ;
#21566 = DIRECTION('center_axis',(0.,0.,-1.)) ;
#21567 = DIRECTION('ref_axis',(-1.,1.22464679914735E-16,0.)) ;
#21568 = DIRECTION('',(-1.22464679914735E-16,-1.,0.)) ;
#21569 = DIRECTION('center_axis',(0.,0.,1.)) ;
#21570 = DIRECTION('ref_axis',(1.,0.,0.)) ;
#21571 = DIRECTION('',(1.,-6.12323399573677E-17,0.)) ;
#21572 = DIRECTION('center_axis',(0.,0.,-1.)) ;
#21573 = DIRECTION('ref_axis',(6.12323399573677E-17,1.,0.)) ;
#21574 = DIRECTION('',(-1.,6.12323399573677E-17,0.)) ;
#21575 = DIRECTION('center_axis',(0.,0.,1.)) ;
#21576 = DIRECTION('ref_axis',(1.,0.,0.)) ;
#21577 = DIRECTION('',(0.,-1.,0.)) ;
#21578 = DIRECTION('center_axis',(0.,0.,-1.)) ;
#21579 = DIRECTION('ref_axis',(1.,0.,0.)) ;
#21580 = DIRECTION('',(0.,1.,0.)) ;
#21581 = DIRECTION('center_axis',(0.,0.,1.)) ;
#21582 = DIRECTION('ref_axis',(1.,0.,0.)) ;
#21583 = DIRECTION('center_axis',(0.,0.,1.)) ;
#21584 = DIRECTION('ref_axis',(1.,0.,0.)) ;
#21585 = DIRECTION('center_axis',(0.,0.,1.)) ;
#21586 = DIRECTION('ref_axis',(1.,0.,0.)) ;
#21587 = DIRECTION('center_axis',(0.,0.,1.)) ;
#21588 = DIRECTION('ref_axis',(1.,0.,0.)) ;
#21589 = DIRECTION('',(0.,0.,-1.)) ;
#21590 = DIRECTION('center_axis',(0.,0.,-1.)) ;
#21591 = DIRECTION('ref_axis',(1.,0.,0.)) ;
#21592 = DIRECTION('center_axis',(0.,0.,-1.)) ;
#21593 = DIRECTION('ref_axis',(1.,0.,0.)) ;
#21594 = DIRECTION('center_axis',(-1.,1.22464679914735E-16,0.)) ;
#21595 = DIRECTION('ref_axis',(1.22464679914735E-16,1.,0.)) ;
#21596 = DIRECTION('',(0.,0.,1.)) ;
#21597 = DIRECTION('',(0.,0.,-1.)) ;
#21598 = DIRECTION('center_axis',(1.,-1.22464679914735E-16,0.)) ;
#21599 = DIRECTION('ref_axis',(-1.22464679914735E-16,-1.,0.)) ;
#21600 = DIRECTION('',(0.,0.,-1.)) ;
#21601 = DIRECTION('center_axis',(0.,0.,-1.)) ;
#21602 = DIRECTION('ref_axis',(-1.,1.22464679914735E-16,0.)) ;
#21603 = DIRECTION('center_axis',(0.,0.,-1.)) ;
#21604 = DIRECTION('ref_axis',(1.,0.,0.)) ;
#21605 = DIRECTION('center_axis',(0.,0.,1.)) ;
#21606 = DIRECTION('ref_axis',(1.,0.,0.)) ;
#21607 = DIRECTION('center_axis',(0.,0.,1.)) ;
#21608 = DIRECTION('ref_axis',(1.,0.,0.)) ;
#21609 = DIRECTION('',(0.,0.,-1.)) ;
#21610 = DIRECTION('center_axis',(0.,0.,-1.)) ;
#21611 = DIRECTION('ref_axis',(1.,0.,0.)) ;
#21612 = DIRECTION('center_axis',(0.,0.,-1.)) ;
#21613 = DIRECTION('ref_axis',(1.,0.,0.)) ;
#21614 = DIRECTION('center_axis',(6.12323399573677E-17,1.,0.)) ;
#21615 = DIRECTION('ref_axis',(1.,-6.12323399573677E-17,0.)) ;
#21616 = DIRECTION('',(0.,0.,1.)) ;
#21617 = DIRECTION('',(0.,0.,-1.)) ;
#21618 = DIRECTION('center_axis',(-6.12323399573677E-17,-1.,0.)) ;
#21619 = DIRECTION('ref_axis',(-1.,6.12323399573677E-17,0.)) ;
#21620 = DIRECTION('',(0.,0.,-1.)) ;
#21621 = DIRECTION('center_axis',(0.,0.,-1.)) ;
#21622 = DIRECTION('ref_axis',(6.12323399573677E-17,1.,0.)) ;
#21623 = DIRECTION('center_axis',(0.,0.,-1.)) ;
#21624 = DIRECTION('ref_axis',(1.,0.,0.)) ;
#21625 = DIRECTION('center_axis',(0.,0.,1.)) ;
#21626 = DIRECTION('ref_axis',(1.,0.,0.)) ;
#21627 = DIRECTION('center_axis',(0.,0.,1.)) ;
#21628 = DIRECTION('ref_axis',(1.,0.,0.)) ;
#21629 = DIRECTION('',(0.,0.,-1.)) ;
#21630 = DIRECTION('center_axis',(0.,0.,-1.)) ;
#21631 = DIRECTION('ref_axis',(1.,0.,0.)) ;
#21632 = DIRECTION('center_axis',(0.,0.,-1.)) ;
#21633 = DIRECTION('ref_axis',(1.,0.,0.)) ;
#21634 = DIRECTION('center_axis',(1.,0.,0.)) ;
#21635 = DIRECTION('ref_axis',(0.,-1.,0.)) ;
#21636 = DIRECTION('',(0.,0.,1.)) ;
#21637 = DIRECTION('',(0.,0.,-1.)) ;
#21638 = DIRECTION('center_axis',(-1.,0.,0.)) ;
#21639 = DIRECTION('ref_axis',(0.,1.,0.)) ;
#21640 = DIRECTION('',(0.,0.,-1.)) ;
#21641 = DIRECTION('center_axis',(0.,0.,-1.)) ;
#21642 = DIRECTION('ref_axis',(1.,0.,0.)) ;
#21643 = DIRECTION('center_axis',(0.,0.,-1.)) ;
#21644 = DIRECTION('ref_axis',(1.,0.,0.)) ;
#21645 = DIRECTION('center_axis',(0.,0.,-1.)) ;
#21646 = DIRECTION('ref_axis',(1.,0.,0.)) ;
#21647 = DIRECTION('center_axis',(0.,0.,1.)) ;
#21648 = DIRECTION('ref_axis',(1.,0.,0.)) ;
#21649 = DIRECTION('center_axis',(0.,0.,-1.)) ;
#21650 = DIRECTION('ref_axis',(1.,0.,0.)) ;
#21651 = DIRECTION('center_axis',(0.,0.,1.)) ;
#21652 = DIRECTION('ref_axis',(1.,0.,0.)) ;
#21653 = DIRECTION('center_axis',(0.,0.,1.)) ;
#21654 = DIRECTION('ref_axis',(1.,0.,0.)) ;
#21655 = DIRECTION('center_axis',(0.,0.,1.)) ;
#21656 = DIRECTION('ref_axis',(1.,0.,0.)) ;
#21657 = DIRECTION('center_axis',(0.,0.,1.)) ;
#21658 = DIRECTION('ref_axis',(1.,0.,0.)) ;
#21659 = DIRECTION('',(0.,0.,1.)) ;
#21660 = DIRECTION('axis',(0.,0.,1.)) ;
#21661 = DIRECTION('refdir',(1.,0.,0.)) ;
#21662 = DIRECTION('center_axis',(1.83697019872103E-16,1.,0.)) ;
#21663 = DIRECTION('ref_axis',(6.12323399573677E-17,-1.12481983699639E-32,
1.)) ;
#21664 = DIRECTION('center_axis',(1.83697019872103E-16,1.,1.82109527525433E-48)) ;
#21665 = DIRECTION('ref_axis',(6.12323399573677E-17,-1.12481983699639E-32,
1.)) ;
#21666 = DIRECTION('',(-1.46793425709383E-16,0.183848416855218,-0.982954607100364)) ;
#21667 = DIRECTION('center_axis',(1.83697019872103E-16,1.,0.)) ;
#21668 = DIRECTION('ref_axis',(6.12323399573677E-17,-1.12481983699639E-32,
1.)) ;
#21669 = DIRECTION('center_axis',(1.83697019872103E-16,1.,0.)) ;
#21670 = DIRECTION('ref_axis',(6.12323399573677E-17,-1.12481983699639E-32,
1.)) ;
#21671 = DIRECTION('center_axis',(1.83697019872103E-16,1.,0.)) ;
#21672 = DIRECTION('ref_axis',(6.12323399573677E-17,-1.12481983699639E-32,
1.)) ;
#21673 = DIRECTION('center_axis',(1.83697019872103E-16,1.,0.)) ;
#21674 = DIRECTION('ref_axis',(6.12323399573677E-17,-1.12481983699639E-32,
1.)) ;
#21675 = DIRECTION('center_axis',(1.83697019872103E-16,1.,0.)) ;
#21676 = DIRECTION('ref_axis',(6.12323399573677E-17,-1.12481983699639E-32,
1.)) ;
#21677 = DIRECTION('center_axis',(1.83697019872103E-16,1.,0.)) ;
#21678 = DIRECTION('ref_axis',(6.12323399573677E-17,-1.12481983699639E-32,
1.)) ;
#21679 = DIRECTION('center_axis',(1.83697019872103E-16,1.,0.)) ;
#21680 = DIRECTION('ref_axis',(6.12323399573677E-17,-1.12481983699639E-32,
1.)) ;
#21681 = DIRECTION('center_axis',(1.83697019872103E-16,1.,0.)) ;
#21682 = DIRECTION('ref_axis',(6.12323399573677E-17,-1.12481983699639E-32,
1.)) ;
#21683 = DIRECTION('center_axis',(1.83697019872103E-16,1.,0.)) ;
#21684 = DIRECTION('ref_axis',(6.12323399573677E-17,-1.12481983699639E-32,
1.)) ;
#21685 = DIRECTION('center_axis',(1.83697019872103E-16,1.,0.)) ;
#21686 = DIRECTION('ref_axis',(6.12323399573677E-17,-1.12481983699639E-32,
1.)) ;
#21687 = DIRECTION('center_axis',(1.83697019872103E-16,1.,0.)) ;
#21688 = DIRECTION('ref_axis',(6.12323399573677E-17,-1.12481983699639E-32,
1.)) ;
#21689 = DIRECTION('center_axis',(1.83697019872103E-16,1.,0.)) ;
#21690 = DIRECTION('ref_axis',(6.12323399573677E-17,-1.12481983699639E-32,
1.)) ;
#21691 = DIRECTION('center_axis',(1.83697019872103E-16,1.,0.)) ;
#21692 = DIRECTION('ref_axis',(6.12323399573677E-17,-1.12481983699639E-32,
1.)) ;
#21693 = DIRECTION('center_axis',(1.83697019872103E-16,1.,0.)) ;
#21694 = DIRECTION('ref_axis',(6.12323399573677E-17,-1.12481983699639E-32,
1.)) ;
#21695 = DIRECTION('center_axis',(1.83697019872103E-16,1.,0.)) ;
#21696 = DIRECTION('ref_axis',(6.12323399573677E-17,-1.12481983699639E-32,
1.)) ;
#21697 = DIRECTION('center_axis',(1.83697019872103E-16,1.,0.)) ;
#21698 = DIRECTION('ref_axis',(6.12323399573677E-17,-1.12481983699639E-32,
1.)) ;
#21699 = DIRECTION('center_axis',(1.83697019872103E-16,1.,0.)) ;
#21700 = DIRECTION('ref_axis',(6.12323399573677E-17,-1.12481983699639E-32,
1.)) ;
#21701 = DIRECTION('center_axis',(1.83697019872103E-16,1.,0.)) ;
#21702 = DIRECTION('ref_axis',(6.12323399573677E-17,-1.12481983699639E-32,
1.)) ;
#21703 = DIRECTION('center_axis',(1.83697019872103E-16,1.,0.)) ;
#21704 = DIRECTION('ref_axis',(6.12323399573677E-17,-1.12481983699639E-32,
1.)) ;
#21705 = DIRECTION('center_axis',(1.83697019872103E-16,1.,0.)) ;
#21706 = DIRECTION('ref_axis',(6.12323399573677E-17,-1.12481983699639E-32,
1.)) ;
#21707 = DIRECTION('center_axis',(1.83697019872103E-16,1.,0.)) ;
#21708 = DIRECTION('ref_axis',(6.12323399573677E-17,-1.12481983699639E-32,
1.)) ;
#21709 = DIRECTION('center_axis',(1.83697019872103E-16,1.,0.)) ;
#21710 = DIRECTION('ref_axis',(6.12323399573677E-17,-1.12481983699639E-32,
1.)) ;
#21711 = DIRECTION('center_axis',(1.83697019872103E-16,1.,0.)) ;
#21712 = DIRECTION('ref_axis',(6.12323399573677E-17,-1.12481983699639E-32,
1.)) ;
#21713 = DIRECTION('center_axis',(1.83697019872103E-16,1.,0.)) ;
#21714 = DIRECTION('ref_axis',(6.12323399573677E-17,-1.12481983699639E-32,
1.)) ;
#21715 = DIRECTION('center_axis',(1.83697019872103E-16,1.,0.)) ;
#21716 = DIRECTION('ref_axis',(6.12323399573677E-17,-1.12481983699639E-32,
1.)) ;
#21717 = DIRECTION('center_axis',(1.83697019872103E-16,1.,0.)) ;
#21718 = DIRECTION('ref_axis',(6.12323399573677E-17,-1.12481983699639E-32,
1.)) ;
#21719 = DIRECTION('center_axis',(1.83697019872103E-16,1.,0.)) ;
#21720 = DIRECTION('ref_axis',(6.12323399573677E-17,-1.12481983699639E-32,
1.)) ;
#21721 = DIRECTION('center_axis',(1.83697019872103E-16,1.,0.)) ;
#21722 = DIRECTION('ref_axis',(6.12323399573677E-17,-1.12481983699639E-32,
1.)) ;
#21723 = DIRECTION('center_axis',(1.83697019872103E-16,1.,0.)) ;
#21724 = DIRECTION('ref_axis',(6.12323399573677E-17,-1.12481983699639E-32,
1.)) ;
#21725 = DIRECTION('center_axis',(1.83697019872103E-16,1.,0.)) ;
#21726 = DIRECTION('ref_axis',(6.12323399573677E-17,-1.12481983699639E-32,
1.)) ;
#21727 = DIRECTION('center_axis',(1.83697019872103E-16,1.,0.)) ;
#21728 = DIRECTION('ref_axis',(6.12323399573677E-17,-1.12481983699639E-32,
1.)) ;
#21729 = DIRECTION('center_axis',(1.83697019872103E-16,1.,0.)) ;
#21730 = DIRECTION('ref_axis',(6.12323399573677E-17,-1.12481983699639E-32,
1.)) ;
#21731 = DIRECTION('center_axis',(1.83697019872103E-16,1.,0.)) ;
#21732 = DIRECTION('ref_axis',(6.12323399573677E-17,-1.12481983699639E-32,
1.)) ;
#21733 = DIRECTION('center_axis',(1.83697019872103E-16,1.,0.)) ;
#21734 = DIRECTION('ref_axis',(6.12323399573677E-17,-1.12481983699639E-32,
1.)) ;
#21735 = DIRECTION('center_axis',(1.83697019872103E-16,1.,0.)) ;
#21736 = DIRECTION('ref_axis',(6.12323399573677E-17,-1.12481983699639E-32,
1.)) ;
#21737 = DIRECTION('center_axis',(1.83697019872103E-16,1.,0.)) ;
#21738 = DIRECTION('ref_axis',(6.12323399573677E-17,-1.12481983699639E-32,
1.)) ;
#21739 = DIRECTION('center_axis',(1.83697019872103E-16,1.,0.)) ;
#21740 = DIRECTION('ref_axis',(6.12323399573677E-17,-1.12481983699639E-32,
1.)) ;
#21741 = DIRECTION('center_axis',(1.83697019872103E-16,1.,0.)) ;
#21742 = DIRECTION('ref_axis',(6.12323399573677E-17,-1.12481983699639E-32,
1.)) ;
#21743 = DIRECTION('center_axis',(1.83697019872103E-16,1.,0.)) ;
#21744 = DIRECTION('ref_axis',(6.12323399573677E-17,-1.12481983699639E-32,
1.)) ;
#21745 = DIRECTION('center_axis',(1.83697019872103E-16,1.,0.)) ;
#21746 = DIRECTION('ref_axis',(6.12323399573677E-17,-1.12481983699639E-32,
1.)) ;
#21747 = DIRECTION('center_axis',(1.83697019872103E-16,1.,0.)) ;
#21748 = DIRECTION('ref_axis',(6.12323399573677E-17,-1.12481983699639E-32,
1.)) ;
#21749 = DIRECTION('center_axis',(1.83697019872103E-16,1.,0.)) ;
#21750 = DIRECTION('ref_axis',(6.12323399573677E-17,-1.12481983699639E-32,
1.)) ;
#21751 = DIRECTION('center_axis',(1.83697019872103E-16,1.,0.)) ;
#21752 = DIRECTION('ref_axis',(6.12323399573677E-17,-1.12481983699639E-32,
1.)) ;
#21753 = DIRECTION('center_axis',(1.83697019872103E-16,1.,0.)) ;
#21754 = DIRECTION('ref_axis',(6.12323399573677E-17,-1.12481983699639E-32,
1.)) ;
#21755 = DIRECTION('center_axis',(1.83697019872103E-16,1.,0.)) ;
#21756 = DIRECTION('ref_axis',(6.12323399573677E-17,-1.12481983699639E-32,
1.)) ;
#21757 = DIRECTION('center_axis',(1.83697019872103E-16,1.,0.)) ;
#21758 = DIRECTION('ref_axis',(6.12323399573677E-17,-1.12481983699639E-32,
1.)) ;
#21759 = DIRECTION('center_axis',(1.83697019872103E-16,1.,0.)) ;
#21760 = DIRECTION('ref_axis',(6.12323399573677E-17,-1.12481983699639E-32,
1.)) ;
#21761 = DIRECTION('center_axis',(1.83697019872103E-16,1.,0.)) ;
#21762 = DIRECTION('ref_axis',(6.12323399573677E-17,-1.12481983699639E-32,
1.)) ;
#21763 = DIRECTION('center_axis',(1.83697019872103E-16,1.,0.)) ;
#21764 = DIRECTION('ref_axis',(6.12323399573677E-17,-1.12481983699639E-32,
1.)) ;
#21765 = DIRECTION('center_axis',(1.83697019872103E-16,1.,0.)) ;
#21766 = DIRECTION('ref_axis',(6.12323399573677E-17,-1.12481983699639E-32,
1.)) ;
#21767 = DIRECTION('center_axis',(1.83697019872103E-16,1.,0.)) ;
#21768 = DIRECTION('ref_axis',(6.12323399573677E-17,-1.12481983699639E-32,
1.)) ;
#21769 = DIRECTION('center_axis',(1.83697019872103E-16,1.,0.)) ;
#21770 = DIRECTION('ref_axis',(6.12323399573677E-17,-1.12481983699639E-32,
1.)) ;
#21771 = DIRECTION('center_axis',(1.83697019872103E-16,1.,0.)) ;
#21772 = DIRECTION('ref_axis',(6.12323399573677E-17,-1.12481983699639E-32,
1.)) ;
#21773 = DIRECTION('center_axis',(1.83697019872103E-16,1.,0.)) ;
#21774 = DIRECTION('ref_axis',(6.12323399573677E-17,-1.12481983699639E-32,
1.)) ;
#21775 = DIRECTION('center_axis',(1.83697019872103E-16,1.,0.)) ;
#21776 = DIRECTION('ref_axis',(6.12323399573677E-17,-1.12481983699639E-32,
1.)) ;
#21777 = DIRECTION('center_axis',(1.83697019872103E-16,1.,0.)) ;
#21778 = DIRECTION('ref_axis',(6.12323399573677E-17,-1.12481983699639E-32,
1.)) ;
#21779 = DIRECTION('center_axis',(1.83697019872103E-16,1.,0.)) ;
#21780 = DIRECTION('ref_axis',(6.12323399573677E-17,-1.12481983699639E-32,
1.)) ;
#21781 = DIRECTION('center_axis',(1.83697019872103E-16,1.,0.)) ;
#21782 = DIRECTION('ref_axis',(6.12323399573677E-17,-1.12481983699639E-32,
1.)) ;
#21783 = DIRECTION('center_axis',(1.83697019872103E-16,1.,0.)) ;
#21784 = DIRECTION('ref_axis',(6.12323399573677E-17,-1.12481983699639E-32,
1.)) ;
#21785 = DIRECTION('center_axis',(-1.83697019872103E-16,-1.,0.)) ;
#21786 = DIRECTION('ref_axis',(6.12323399573677E-17,-1.12481983699639E-32,
1.)) ;
#21787 = DIRECTION('',(1.71053004918302E-16,0.986251982240049,0.165248381316047)) ;
#21788 = DIRECTION('center_axis',(1.83697019872103E-16,1.,0.)) ;
#21789 = DIRECTION('ref_axis',(6.12323399573677E-17,-1.12481983699639E-32,
1.)) ;
#21790 = DIRECTION('center_axis',(-0.0198775103691821,0.982954607100363,0.182770689558513)) ;
#21791 = DIRECTION('ref_axis',(0.106276087274991,0.183848416855221,-0.97719248507822)) ;
#21792 = DIRECTION('center_axis',(1.83697019872103E-16,1.,0.)) ;
#21793 = DIRECTION('ref_axis',(6.12323399573677E-17,-1.12481983699639E-32,
1.)) ;
#21794 = DIRECTION('center_axis',(-0.0587030808149488,0.982954607100363,0.174224535249788)) ;
#21795 = DIRECTION('ref_axis',(0.313858910101312,0.183848416855221,-0.93150005054742)) ;
#21796 = DIRECTION('center_axis',(1.83697019872103E-16,1.,0.)) ;
#21797 = DIRECTION('ref_axis',(6.12323399573677E-17,-1.12481983699639E-32,
1.)) ;
#21798 = DIRECTION('center_axis',(-0.0947837604455976,0.982954607100363,0.157531835309445)) ;
#21799 = DIRECTION('ref_axis',(0.506766039120339,0.183848416855219,-0.842251708941046)) ;
#21800 = DIRECTION('center_axis',(1.83697019872103E-16,1.,0.)) ;
#21801 = DIRECTION('ref_axis',(6.12323399573677E-17,-1.12481983699639E-32,
1.)) ;
#21802 = DIRECTION('center_axis',(-0.126432456782393,0.982954607100363,0.133473121834093)) ;
#21803 = DIRECTION('ref_axis',(0.675977351380336,0.183848416855219,-0.713620613519996)) ;
#21804 = DIRECTION('center_axis',(1.83697019872103E-16,1.,0.)) ;
#21805 = DIRECTION('ref_axis',(6.12323399573677E-17,-1.12481983699639E-32,
1.)) ;
#21806 = DIRECTION('center_axis',(-0.152169311959628,0.982954607100363,0.1031733535265)) ;
#21807 = DIRECTION('ref_axis',(-0.813580713984576,-0.18384841685522,0.55162141134312)) ;
#21808 = DIRECTION('center_axis',(1.83697019872103E-16,1.,0.)) ;
#21809 = DIRECTION('ref_axis',(6.12323399573677E-17,-1.12481983699639E-32,
1.)) ;
#21810 = DIRECTION('center_axis',(-0.170790899233672,0.982954607100363,0.0680493138769549)) ;
#21811 = DIRECTION('ref_axis',(-0.913141946632867,-0.18384841685522,0.363829005055077)) ;
#21812 = DIRECTION('center_axis',(1.83697019872103E-16,1.,0.)) ;
#21813 = DIRECTION('ref_axis',(6.12323399573677E-17,-1.12481983699639E-32,
1.)) ;
#21814 = DIRECTION('center_axis',(-0.181426493880004,0.982954607100363,0.0297433639419022)) ;
#21815 = DIRECTION('ref_axis',(-0.970005676741035,-0.183848416855222,0.159024358857364)) ;
#21816 = DIRECTION('center_axis',(1.83697019872103E-16,1.,0.)) ;
#21817 = DIRECTION('ref_axis',(6.12323399573677E-17,-1.12481983699639E-32,
1.)) ;
#21818 = DIRECTION('center_axis',(-0.183578787313568,0.982954607100363,-0.00995335263369878)) ;
#21819 = DIRECTION('ref_axis',(-0.981513019488615,-0.183848416855221,-0.0532160896174334)) ;
#21820 = DIRECTION('center_axis',(1.83697019872103E-16,1.,0.)) ;
#21821 = DIRECTION('ref_axis',(6.12323399573677E-17,-1.12481983699639E-32,
1.)) ;
#21822 = DIRECTION('center_axis',(1.83697019872103E-16,1.,0.)) ;
#21823 = DIRECTION('ref_axis',(6.12323399573677E-17,-1.12481983699639E-32,
1.)) ;
#21824 = DIRECTION('center_axis',(-0.16243229064392,0.982954607100363,-0.0861161502642797)) ;
#21825 = DIRECTION('ref_axis',(-0.868452234516904,-0.18384841685522,-0.460424234790508)) ;
#21826 = DIRECTION('center_axis',(1.83697019872103E-16,1.,0.)) ;
#21827 = DIRECTION('ref_axis',(6.12323399573677E-17,-1.12481983699639E-32,
1.)) ;
#21828 = DIRECTION('center_axis',(-0.140122287222336,0.982954607100363,-0.119020943550922)) ;
#21829 = DIRECTION('ref_axis',(-0.749170703444705,-0.18384841685522,-0.636351331199986)) ;
#21830 = DIRECTION('center_axis',(1.83697019872103E-16,1.,0.)) ;
#21831 = DIRECTION('ref_axis',(6.12323399573677E-17,-1.12481983699639E-32,
1.)) ;
#21832 = DIRECTION('center_axis',(-0.111260321384975,0.982954607100363,-0.146360449799402)) ;
#21833 = DIRECTION('ref_axis',(-0.594858782923343,-0.183848416855221,-0.782523346615798)) ;
#21834 = DIRECTION('center_axis',(1.83697019872103E-16,1.,0.)) ;
#21835 = DIRECTION('ref_axis',(6.12323399573677E-17,-1.12481983699639E-32,
1.)) ;
#21836 = DIRECTION('center_axis',(-0.0771959465766158,0.982954607100363,-0.166856304083218)) ;
#21837 = DIRECTION('ref_axis',(-0.412731926849916,-0.183848416855221,-0.892105440056603)) ;
#21838 = DIRECTION('center_axis',(1.83697019872103E-16,1.,0.)) ;
#21839 = DIRECTION('ref_axis',(6.12323399573677E-17,-1.12481983699639E-32,
1.)) ;
#21840 = DIRECTION('center_axis',(1.83697019872103E-16,1.,0.)) ;
#21841 = DIRECTION('ref_axis',(6.12323399573677E-17,-1.12481983699639E-32,
1.)) ;
#21842 = DIRECTION('center_axis',(1.80565831993891E-16,0.982954607100363,
-0.18384841685522)) ;
#21843 = DIRECTION('ref_axis',(4.87486550750718E-15,-0.18384841685522,-0.982954607100363)) ;
#21844 = DIRECTION('center_axis',(1.83697019872103E-16,1.,0.)) ;
#21845 = DIRECTION('ref_axis',(6.12323399573677E-17,-1.12481983699639E-32,
1.)) ;
#21846 = DIRECTION('center_axis',(0.039521975103467,0.982954607100363,-0.179550143035566)) ;
#21847 = DIRECTION('ref_axis',(0.211306184595842,-0.183848416855221,-0.959973674624141)) ;
#21848 = DIRECTION('center_axis',(1.83697019872103E-16,1.,0.)) ;
#21849 = DIRECTION('ref_axis',(6.12323399573677E-17,-1.12481983699639E-32,
1.)) ;
#21850 = DIRECTION('center_axis',(0.0771959465766158,0.982954607100363,-0.166856304083218)) ;
#21851 = DIRECTION('ref_axis',(0.412731926849801,-0.183848416855221,-0.892105440056656)) ;
#21852 = DIRECTION('center_axis',(1.83697019872103E-16,1.,0.)) ;
#21853 = DIRECTION('ref_axis',(6.12323399573677E-17,-1.12481983699639E-32,
1.)) ;
#21854 = DIRECTION('center_axis',(0.111260321384975,0.982954607100363,-0.146360449799403)) ;
#21855 = DIRECTION('ref_axis',(0.594858782923056,-0.183848416855222,-0.782523346616016)) ;
#21856 = DIRECTION('center_axis',(1.83697019872103E-16,1.,0.)) ;
#21857 = DIRECTION('ref_axis',(6.12323399573677E-17,-1.12481983699639E-32,
1.)) ;
#21858 = DIRECTION('center_axis',(0.140122287222336,0.982954607100363,-0.119020943550922)) ;
#21859 = DIRECTION('ref_axis',(-0.749170703444731,0.18384841685522,0.636351331199956)) ;
#21860 = DIRECTION('center_axis',(1.83697019872103E-16,1.,0.)) ;
#21861 = DIRECTION('ref_axis',(6.12323399573677E-17,-1.12481983699639E-32,
1.)) ;
#21862 = DIRECTION('center_axis',(0.16243229064392,0.982954607100363,-0.0861161502642797)) ;
#21863 = DIRECTION('ref_axis',(-0.868452234516886,0.18384841685522,0.460424234790542)) ;
#21864 = DIRECTION('center_axis',(1.83697019872103E-16,1.,0.)) ;
#21865 = DIRECTION('ref_axis',(6.12323399573677E-17,-1.12481983699639E-32,
1.)) ;
#21866 = DIRECTION('center_axis',(0.17714714068552,0.982954607100363,-0.0491846615025046)) ;
#21867 = DIRECTION('ref_axis',(-0.947125904318293,0.183848416855222,0.262968212887193)) ;
#21868 = DIRECTION('center_axis',(1.83697019872103E-16,1.,0.)) ;
#21869 = DIRECTION('ref_axis',(6.12323399573677E-17,-1.12481983699639E-32,
1.)) ;
#21870 = DIRECTION('center_axis',(0.183578787313568,0.982954607100363,-0.00995335263369856)) ;
#21871 = DIRECTION('ref_axis',(-0.981513019488616,0.183848416855221,0.0532160896174185)) ;
#21872 = DIRECTION('center_axis',(1.83697019872103E-16,1.,0.)) ;
#21873 = DIRECTION('ref_axis',(6.12323399573677E-17,-1.12481983699639E-32,
1.)) ;
#21874 = DIRECTION('center_axis',(0.181426493880004,0.982954607100363,0.0297433639419022)) ;
#21875 = DIRECTION('ref_axis',(-0.97000567674103,0.183848416855222,-0.159024358857395)) ;
#21876 = DIRECTION('center_axis',(1.83697019872103E-16,1.,0.)) ;
#21877 = DIRECTION('ref_axis',(6.12323399573677E-17,-1.12481983699639E-32,
1.)) ;
#21878 = DIRECTION('center_axis',(0.170790899233673,0.982954607100363,0.0680493138769549)) ;
#21879 = DIRECTION('ref_axis',(-0.913141946632915,0.183848416855221,-0.363829005054957)) ;
#21880 = DIRECTION('center_axis',(1.83697019872103E-16,1.,0.)) ;
#21881 = DIRECTION('ref_axis',(6.12323399573677E-17,-1.12481983699639E-32,
1.)) ;
#21882 = DIRECTION('center_axis',(0.152169311959628,0.982954607100363,0.1031733535265)) ;
#21883 = DIRECTION('ref_axis',(-0.813580713984593,0.18384841685522,-0.551621411343096)) ;
#21884 = DIRECTION('center_axis',(1.83697019872103E-16,1.,0.)) ;
#21885 = DIRECTION('ref_axis',(6.12323399573677E-17,-1.12481983699639E-32,
1.)) ;
#21886 = DIRECTION('center_axis',(0.126432456782393,0.982954607100363,0.133473121834093)) ;
#21887 = DIRECTION('ref_axis',(-0.675977351380349,0.183848416855219,-0.713620613519984)) ;
#21888 = DIRECTION('center_axis',(1.83697019872103E-16,1.,0.)) ;
#21889 = DIRECTION('ref_axis',(6.12323399573677E-17,-1.12481983699639E-32,
1.)) ;
#21890 = DIRECTION('center_axis',(0.0947837604455976,0.982954607100363,0.157531835309445)) ;
#21891 = DIRECTION('ref_axis',(-0.506766039120492,0.18384841685522,-0.842251708940954)) ;
#21892 = DIRECTION('center_axis',(1.83697019872103E-16,1.,0.)) ;
#21893 = DIRECTION('ref_axis',(6.12323399573677E-17,-1.12481983699639E-32,
1.)) ;
#21894 = DIRECTION('center_axis',(0.0587030808149488,0.982954607100363,0.174224535249788)) ;
#21895 = DIRECTION('ref_axis',(-0.313858910101348,0.183848416855221,-0.931500050547408)) ;
#21896 = DIRECTION('center_axis',(1.83697019872103E-16,1.,0.)) ;
#21897 = DIRECTION('ref_axis',(6.12323399573677E-17,-1.12481983699639E-32,
1.)) ;
#21898 = DIRECTION('center_axis',(0.0198775103691822,0.982954607100363,0.182770689558513)) ;
#21899 = DIRECTION('ref_axis',(-0.10627608727498,0.183848416855221,-0.977192485078221)) ;
#21900 = DIRECTION('center_axis',(1.83697019872103E-16,1.,0.)) ;
#21901 = DIRECTION('ref_axis',(6.12323399573677E-17,-1.12481983699639E-32,
1.)) ;
#21902 = DIRECTION('center_axis',(-0.17714714068552,0.982954607100363,-0.0491846615025055)) ;
#21903 = DIRECTION('ref_axis',(-0.947125904318291,-0.183848416855222,-0.262968212887199)) ;
#21904 = DIRECTION('center_axis',(-0.0395219751034661,0.982954607100363,-0.179550143035566)) ;
#21905 = DIRECTION('ref_axis',(-0.211306184595852,-0.183848416855221,-0.959973674624139)) ;
#21906 = DIRECTION('center_axis',(1.83697019872103E-16,1.,0.)) ;
#21907 = DIRECTION('ref_axis',(6.12323399573677E-17,-1.12481983699639E-32,
1.)) ;
#21908 = DIRECTION('',(0.0894326665084245,-0.995991732165632,0.00150586151291223)) ;
#21909 = DIRECTION('center_axis',(-0.0198775103691822,0.982954607100363,0.182770689558513)) ;
#21910 = DIRECTION('ref_axis',(-0.106276087274983,-0.183848416855221,0.977192485078221)) ;
#21911 = DIRECTION('center_axis',(-0.0198775103691822,0.982954607100363,0.182770689558513)) ;
#21912 = DIRECTION('ref_axis',(-0.106276087274983,-0.183848416855221,0.977192485078221)) ;
#21913 = DIRECTION('',(0.0876654961771864,0.9959917321656,0.0177547243790319)) ;
#21914 = DIRECTION('',(0.0870195460927401,-0.995991472747943,0.0207022899988359)) ;
#21915 = DIRECTION('center_axis',(-0.0587030808149488,0.982954607100363,0.174224535249788)) ;
#21916 = DIRECTION('ref_axis',(-0.313858910101354,-0.183848416855221,0.931500050547405)) ;
#21917 = DIRECTION('center_axis',(-0.0587030808149488,0.982954607100363,0.174224535249788)) ;
#21918 = DIRECTION('ref_axis',(-0.313858910101354,-0.183848416855221,0.931500050547405)) ;
#21919 = DIRECTION('',(0.0818041493280548,0.995991472747942,0.0361810360009097)) ;
#21920 = DIRECTION('',(0.0805345699739786,-0.995991874626499,0.0389148906859529)) ;
#21921 = DIRECTION('center_axis',(-0.0947837604455976,0.982954607100363,0.157531835309445)) ;
#21922 = DIRECTION('ref_axis',(-0.506766039120519,-0.183848416855219,0.842251708940938)) ;
#21923 = DIRECTION('center_axis',(-0.0947837604455976,0.982954607100363,0.157531835309445)) ;
#21924 = DIRECTION('ref_axis',(-0.506766039120519,-0.183848416855219,0.842251708940938)) ;
#21925 = DIRECTION('',(0.0721048469731237,0.995991874626519,0.0529251992999018)) ;
#21926 = DIRECTION('',(0.070286008728264,-0.995991843748342,0.055318389020542)) ;
#21927 = DIRECTION('center_axis',(-0.126432456782393,0.982954607100363,0.133473121834093)) ;
#21928 = DIRECTION('ref_axis',(-0.675977351380399,-0.183848416855219,0.713620613519936)) ;
#21929 = DIRECTION('center_axis',(-0.126432456782393,0.982954607100363,0.133473121834093)) ;
#21930 = DIRECTION('ref_axis',(-0.675977351380399,-0.183848416855219,0.713620613519936)) ;
#21931 = DIRECTION('',(0.0590424676389299,0.995991843748325,0.0671880510352708)) ;
#21932 = DIRECTION('',(0.0567510610610272,-0.995991855108921,0.0691342290413218)) ;
#21933 = DIRECTION('center_axis',(-0.152169311959628,0.982954607100363,0.1031733535265)) ;
#21934 = DIRECTION('ref_axis',(-0.813580713984602,-0.18384841685522,0.551621411343083)) ;
#21935 = DIRECTION('center_axis',(-0.152169311959628,0.982954607100363,0.1031733535265)) ;
#21936 = DIRECTION('ref_axis',(-0.813580713984602,-0.18384841685522,0.551621411343083)) ;
#21937 = DIRECTION('',(0.0432183562672333,0.995991855108916,0.0783096305588247)) ;
#21938 = DIRECTION('',(0.0405615702551079,-0.995991800293961,0.0797188357017008)) ;
#21939 = DIRECTION('center_axis',(-0.170790899233673,0.982954607100363,0.0680493138769549)) ;
#21940 = DIRECTION('ref_axis',(-0.913141946632898,-0.183848416855221,0.363829005054999)) ;
#21941 = DIRECTION('center_axis',(-0.170790899233673,0.982954607100363,0.0680493138769549)) ;
#21942 = DIRECTION('ref_axis',(-0.913141946632898,-0.183848416855221,0.363829005054999)) ;
#21943 = DIRECTION('',(0.0253750830217403,0.99599180029395,0.0857696852556677)) ;
#21944 = DIRECTION('',(0.0224747998305547,-0.995991732165588,0.0865757057745833)) ;
#21945 = DIRECTION('center_axis',(-0.181426493880003,0.982954607100363,0.0297433639419022)) ;
#21946 = DIRECTION('ref_axis',(-0.970005676741024,-0.183848416855221,0.159024358857432)) ;
#21947 = DIRECTION('center_axis',(-0.181426493880003,0.982954607100363,0.0297433639419022)) ;
#21948 = DIRECTION('ref_axis',(-0.970005676741024,-0.183848416855221,0.159024358857432)) ;
#21949 = DIRECTION('',(0.00634543999453282,0.995991732165633,0.0892199800996225)) ;
#21950 = DIRECTION('',(0.00333813391881096,-0.995991732165608,0.0893830314975548)) ;
#21951 = DIRECTION('center_axis',(-0.183578787313568,0.982954607100363,-0.00995335263369877)) ;
#21952 = DIRECTION('ref_axis',(0.981513019488616,0.183848416855221,0.0532160896174231)) ;
#21953 = DIRECTION('center_axis',(-0.183578787313568,0.982954607100363,-0.00995335263369877)) ;
#21954 = DIRECTION('ref_axis',(0.981513019488616,0.183848416855221,0.0532160896174231)) ;
#21955 = DIRECTION('',(-0.0129825712619722,0.995991732165591,0.0884981485750611)) ;
#21956 = DIRECTION('',(-0.0159729881663253,-0.995990956174831,0.0880163556788385)) ;
#21957 = DIRECTION('center_axis',(-0.17714714068552,0.982954607100363,-0.0491846615025055)) ;
#21958 = DIRECTION('ref_axis',(0.947125904318289,0.183848416855222,0.262968212887207)) ;
#21959 = DIRECTION('center_axis',(-0.17714714068552,0.982954607100363,-0.0491846615025055)) ;
#21960 = DIRECTION('ref_axis',(0.947125904318289,0.183848416855222,0.262968212887207)) ;
#21961 = DIRECTION('',(-0.0316906021296052,0.995990956174818,0.0836523816435276)) ;
#21962 = DIRECTION('',(-0.0344972257280317,-0.995991897161699,0.0825232222184031)) ;
#21963 = DIRECTION('center_axis',(-0.16243229064392,0.982954607100363,-0.0861161502642797)) ;
#21964 = DIRECTION('ref_axis',(0.868452234516877,0.18384841685522,0.460424234790559)) ;
#21965 = DIRECTION('center_axis',(-0.16243229064392,0.982954607100363,-0.0861161502642797)) ;
#21966 = DIRECTION('ref_axis',(0.868452234516877,0.18384841685522,0.460424234790559)) ;
#21967 = DIRECTION('',(-0.0489441662534316,0.995991897161676,0.0748639391031554)) ;
#21968 = DIRECTION('',(-0.0514320044770238,-0.995991845655882,0.0731778129111852)) ;
#21969 = DIRECTION('center_axis',(-0.140122287222336,0.982954607100363,-0.119020943550922)) ;
#21970 = DIRECTION('ref_axis',(0.749170703444789,0.18384841685522,0.636351331199888)) ;
#21971 = DIRECTION('center_axis',(-0.140122287222336,0.982954607100363,-0.119020943550922)) ;
#21972 = DIRECTION('ref_axis',(0.749170703444789,0.18384841685522,0.636351331199888)) ;
#21973 = DIRECTION('',(-0.0638930342713704,0.995991845655898,0.06259331880126)) ;
#21974 = DIRECTION('',(-0.0659605301635769,-0.995991849453985,0.0604106305361067)) ;
#21975 = DIRECTION('center_axis',(-0.111260321384975,0.982954607100363,-0.146360449799403)) ;
#21976 = DIRECTION('ref_axis',(0.594858782923059,0.183848416855222,0.782523346616013)) ;
#21977 = DIRECTION('center_axis',(-0.111260321384975,0.982954607100363,-0.146360449799403)) ;
#21978 = DIRECTION('ref_axis',(0.594858782923059,0.183848416855222,0.782523346616013)) ;
#21979 = DIRECTION('',(-0.0758549736440145,0.995991849454008,0.0473947127288519)) ;
#21980 = DIRECTION('',(-0.0774044203990348,-0.995991874113701,0.044818995996865)) ;
#21981 = DIRECTION('center_axis',(-0.0771959465766158,0.982954607100363,-0.166856304083218)) ;
#21982 = DIRECTION('ref_axis',(0.412731926849895,0.183848416855221,0.892105440056612)) ;
#21983 = DIRECTION('center_axis',(-0.0771959465766158,0.982954607100363,-0.166856304083218)) ;
#21984 = DIRECTION('ref_axis',(0.412731926849895,0.183848416855221,0.892105440056612)) ;
#21985 = DIRECTION('',(-0.0842698982455389,0.995991874113698,0.0299795088213562)) ;
#21986 = DIRECTION('',(-0.085251590350561,-0.995990596094747,0.0271090175685372)) ;
#21987 = DIRECTION('center_axis',(-0.0395219751034661,0.982954607100363,-0.179550143035566)) ;
#21988 = DIRECTION('ref_axis',(0.211306184595816,0.183848416855221,0.959973674624147)) ;
#21989 = DIRECTION('center_axis',(-0.0395219751034661,0.982954607100363,-0.179550143035566)) ;
#21990 = DIRECTION('ref_axis',(0.211306184595816,0.183848416855221,0.959973674624147)) ;
#21991 = DIRECTION('',(-0.0887550289210553,0.995990596094745,0.0111927356824723)) ;
#21992 = DIRECTION('',(-0.0890712206546686,-0.995991732165598,0.00817233802896422)) ;
#21993 = DIRECTION('center_axis',(1.80565831993891E-16,0.982954607100363,
-0.18384841685522)) ;
#21994 = DIRECTION('ref_axis',(9.39610169491382E-17,0.18384841685522,0.982954607100363)) ;
#21995 = DIRECTION('center_axis',(1.80565831993891E-16,0.982954607100363,
-0.18384841685522)) ;
#21996 = DIRECTION('ref_axis',(9.39610169491382E-17,0.18384841685522,0.982954607100363)) ;
#21997 = DIRECTION('',(-0.0890712206546686,0.995991732165598,-0.00817233802896422)) ;
#21998 = DIRECTION('',(-0.0887550289209964,-0.995990596094752,-0.0111927356822663)) ;
#21999 = DIRECTION('center_axis',(0.039521975103467,0.982954607100363,-0.179550143035566)) ;
#22000 = DIRECTION('ref_axis',(-0.211306184595819,0.183848416855221,0.959973674624146)) ;
#22001 = DIRECTION('center_axis',(0.039521975103467,0.982954607100363,-0.179550143035566)) ;
#22002 = DIRECTION('ref_axis',(-0.211306184595819,0.183848416855221,0.959973674624146)) ;
#22003 = DIRECTION('',(-0.0852515903504576,0.995990596094755,-0.0271090175685374)) ;
#22004 = DIRECTION('',(-0.0842698982454947,-0.995991874113696,-0.0299795088215489)) ;
#22005 = DIRECTION('center_axis',(0.0771959465766158,0.982954607100363,-0.166856304083218)) ;
#22006 = DIRECTION('ref_axis',(-0.412731926849894,0.183848416855221,0.892105440056613)) ;
#22007 = DIRECTION('center_axis',(0.0771959465766158,0.982954607100363,-0.166856304083218)) ;
#22008 = DIRECTION('ref_axis',(-0.412731926849894,0.183848416855221,0.892105440056613)) ;
#22009 = DIRECTION('',(-0.0774044203992267,0.995991874113696,-0.0448189959966469)) ;
#22010 = DIRECTION('',(-0.0758549736442256,-0.995991849454001,-0.0473947127286581)) ;
#22011 = DIRECTION('center_axis',(0.111260321384975,0.982954607100363,-0.146360449799403)) ;
#22012 = DIRECTION('ref_axis',(-0.594858782923059,0.183848416855222,0.782523346616014)) ;
#22013 = DIRECTION('center_axis',(0.111260321384975,0.982954607100363,-0.146360449799403)) ;
#22014 = DIRECTION('ref_axis',(-0.594858782923059,0.183848416855222,0.782523346616014)) ;
#22015 = DIRECTION('',(-0.0659605301634746,0.995991849453984,-0.060410630536239)) ;
#22016 = DIRECTION('',(-0.0638930342712978,-0.995991845655893,-0.0625933188014015)) ;
#22017 = DIRECTION('center_axis',(0.140122287222336,0.982954607100363,-0.119020943550922)) ;
#22018 = DIRECTION('ref_axis',(-0.74917070344479,0.18384841685522,0.636351331199887)) ;
#22019 = DIRECTION('center_axis',(0.140122287222336,0.982954607100363,-0.119020943550922)) ;
#22020 = DIRECTION('ref_axis',(-0.74917070344479,0.18384841685522,0.636351331199887)) ;
#22021 = DIRECTION('',(-0.0514320044769895,0.995991845655871,-0.073177812911361)) ;
#22022 = DIRECTION('',(-0.0489441662532377,-0.995991897161693,-0.0748639391030673)) ;
#22023 = DIRECTION('center_axis',(0.16243229064392,0.982954607100363,-0.0861161502642797)) ;
#22024 = DIRECTION('ref_axis',(-0.868452234516877,0.18384841685522,0.460424234790559)) ;
#22025 = DIRECTION('center_axis',(0.16243229064392,0.982954607100363,-0.0861161502642797)) ;
#22026 = DIRECTION('ref_axis',(-0.868452234516877,0.18384841685522,0.460424234790559)) ;
#22027 = DIRECTION('',(-0.0344972257278522,0.9959918971617,-0.0825232222184722)) ;
#22028 = DIRECTION('',(-0.0316906021296349,-0.995990956174831,-0.0836523816433686)) ;
#22029 = DIRECTION('center_axis',(0.17714714068552,0.982954607100363,-0.0491846615025046)) ;
#22030 = DIRECTION('ref_axis',(-0.947125904318291,0.183848416855222,0.262968212887201)) ;
#22031 = DIRECTION('center_axis',(0.17714714068552,0.982954607100363,-0.0491846615025046)) ;
#22032 = DIRECTION('ref_axis',(-0.947125904318291,0.183848416855222,0.262968212887201)) ;
#22033 = DIRECTION('',(-0.0159729881664467,0.995990956174826,-0.0880163556788801)) ;
#22034 = DIRECTION('',(-0.0129825712619121,-0.99599173216567,-0.0884981485741822)) ;
#22035 = DIRECTION('center_axis',(0.183578787313568,0.982954607100363,-0.00995335263369855)) ;
#22036 = DIRECTION('ref_axis',(-0.981513019488616,0.183848416855221,0.0532160896174219)) ;
#22037 = DIRECTION('center_axis',(0.183578787313568,0.982954607100363,-0.00995335263369855)) ;
#22038 = DIRECTION('ref_axis',(-0.981513019488616,0.183848416855221,0.0532160896174219)) ;
#22039 = DIRECTION('',(0.00333813391881109,0.995991732165649,-0.0893830314970895)) ;
#22040 = DIRECTION('',(0.00634543999453281,-0.995991732165632,-0.0892199800996354)) ;
#22041 = DIRECTION('center_axis',(0.181426493880003,0.982954607100363,0.0297433639419022)) ;
#22042 = DIRECTION('ref_axis',(0.970005676741024,-0.183848416855221,0.159024358857432)) ;
#22043 = DIRECTION('center_axis',(0.181426493880003,0.982954607100363,0.0297433639419022)) ;
#22044 = DIRECTION('ref_axis',(0.970005676741024,-0.183848416855221,0.159024358857432)) ;
#22045 = DIRECTION('',(0.0224747998304496,0.995991732165622,-0.0865757057742305)) ;
#22046 = DIRECTION('',(0.0253750830216289,-0.995991800293954,-0.0857696852556559)) ;
#22047 = DIRECTION('center_axis',(0.170790899233672,0.982954607100363,0.0680493138769549)) ;
#22048 = DIRECTION('ref_axis',(0.913141946632898,-0.18384841685522,0.363829005054999)) ;
#22049 = DIRECTION('center_axis',(0.170790899233672,0.982954607100363,0.0680493138769549)) ;
#22050 = DIRECTION('ref_axis',(0.913141946632898,-0.18384841685522,0.363829005054999)) ;
#22051 = DIRECTION('',(0.0405615702551252,0.995991800293957,-0.0797188357017419)) ;
#22052 = DIRECTION('',(0.0432183562674327,-0.995991855108905,-0.0783096305588474)) ;
#22053 = DIRECTION('center_axis',(0.152169311959628,0.982954607100363,0.1031733535265)) ;
#22054 = DIRECTION('ref_axis',(0.813580713984602,-0.18384841685522,0.551621411343082)) ;
#22055 = DIRECTION('center_axis',(0.152169311959628,0.982954607100363,0.1031733535265)) ;
#22056 = DIRECTION('ref_axis',(0.813580713984602,-0.18384841685522,0.551621411343082)) ;
#22057 = DIRECTION('',(0.0567510610609564,0.99599185510892,-0.0691342290413986)) ;
#22058 = DIRECTION('',(0.0590424676390377,-0.995991843748321,-0.0671880510352316)) ;
#22059 = DIRECTION('center_axis',(0.126432456782393,0.982954607100363,0.133473121834093)) ;
#22060 = DIRECTION('ref_axis',(0.675977351380399,-0.183848416855219,0.713620613519936)) ;
#22061 = DIRECTION('center_axis',(0.126432456782393,0.982954607100363,0.133473121834093)) ;
#22062 = DIRECTION('ref_axis',(0.675977351380399,-0.183848416855219,0.713620613519936)) ;
#22063 = DIRECTION('',(0.0702860087283124,0.995991843748332,-0.0553183890206689)) ;
#22064 = DIRECTION('',(0.0721048469732812,-0.9959918746265,-0.0529251993000518)) ;
#22065 = DIRECTION('center_axis',(0.0947837604455977,0.982954607100363,0.157531835309445)) ;
#22066 = DIRECTION('ref_axis',(0.506766039120516,-0.18384841685522,0.842251708940939)) ;
#22067 = DIRECTION('center_axis',(0.0947837604455977,0.982954607100363,0.157531835309445)) ;
#22068 = DIRECTION('ref_axis',(0.506766039120516,-0.18384841685522,0.842251708940939)) ;
#22069 = DIRECTION('',(0.0805345699739992,0.995991874626496,-0.0389148906859699)) ;
#22070 = DIRECTION('',(0.0818041493280427,-0.995991472747948,-0.036181036000766)) ;
#22071 = DIRECTION('center_axis',(0.0587030808149488,0.982954607100363,0.174224535249788)) ;
#22072 = DIRECTION('ref_axis',(0.313858910101352,-0.183848416855221,0.931500050547406)) ;
#22073 = DIRECTION('center_axis',(0.0587030808149488,0.982954607100363,0.174224535249788)) ;
#22074 = DIRECTION('ref_axis',(0.313858910101352,-0.183848416855221,0.931500050547406)) ;
#22075 = DIRECTION('',(0.087019546092724,0.99599147274794,-0.0207022899990529)) ;
#22076 = DIRECTION('',(0.0876654961766692,-0.995991732165646,-0.0177547243790327)) ;
#22077 = DIRECTION('center_axis',(0.0198775103691822,0.982954607100363,0.182770689558513)) ;
#22078 = DIRECTION('ref_axis',(0.106276087274981,-0.183848416855221,0.977192485078221)) ;
#22079 = DIRECTION('center_axis',(0.0198775103691822,0.982954607100363,0.182770689558513)) ;
#22080 = DIRECTION('ref_axis',(0.106276087274981,-0.183848416855221,0.977192485078221)) ;
#22081 = DIRECTION('',(0.089432666508431,0.995991732165632,-0.00150586151291223)) ;
#22082 = DIRECTION('',(-1.83697019872103E-16,-1.,0.)) ;
#22083 = DIRECTION('center_axis',(1.83697019872103E-16,1.,0.)) ;
#22084 = DIRECTION('ref_axis',(6.12323399573677E-17,-1.12481983699639E-32,
1.)) ;
#22085 = DIRECTION('center_axis',(-1.83697019872103E-16,-1.,0.)) ;
#22086 = DIRECTION('ref_axis',(6.12323399573676E-17,-1.12481983699639E-32,
1.)) ;
#22087 = DIRECTION('center_axis',(1.83697019872103E-16,1.,0.)) ;
#22088 = DIRECTION('ref_axis',(6.12323399573676E-17,-1.12481983699639E-32,
1.)) ;
#22089 = DIRECTION('',(-1.67503306565163E-16,-0.979306480331619,-0.202382849027518)) ;
#22090 = DIRECTION('center_axis',(1.83697019872103E-16,1.,0.)) ;
#22091 = DIRECTION('ref_axis',(6.12323399573676E-17,-1.12481983699639E-32,
1.)) ;
#22092 = DIRECTION('center_axis',(-1.80565831993891E-16,-0.982954607100363,
0.18384841685522)) ;
#22093 = DIRECTION('ref_axis',(3.97603040674231E-15,-0.18384841685522,-0.982954607100363)) ;
#22094 = DIRECTION('center_axis',(0.0771959465766158,-0.982954607100363,0.166856304083218)) ;
#22095 = DIRECTION('ref_axis',(-0.412731926849851,-0.183848416855221,-0.892105440056633)) ;
#22096 = DIRECTION('center_axis',(0.140122287222336,-0.982954607100363,0.119020943550922)) ;
#22097 = DIRECTION('ref_axis',(-0.749170703444893,-0.18384841685522,-0.636351331199766)) ;
#22098 = DIRECTION('center_axis',(0.17714714068552,-0.982954607100363,0.0491846615025055)) ;
#22099 = DIRECTION('ref_axis',(-0.947125904318309,-0.183848416855222,-0.262968212887135)) ;
#22100 = DIRECTION('center_axis',(0.181426493880003,-0.982954607100363,-0.0297433639419022)) ;
#22101 = DIRECTION('ref_axis',(-0.970005676741017,-0.183848416855221,0.159024358857473)) ;
#22102 = DIRECTION('center_axis',(0.152169311959628,-0.982954607100363,-0.1031733535265)) ;
#22103 = DIRECTION('ref_axis',(-0.813580713984591,-0.18384841685522,0.551621411343099)) ;
#22104 = DIRECTION('center_axis',(0.0947837604455976,-0.982954607100363,-0.157531835309445)) ;
#22105 = DIRECTION('ref_axis',(0.506766039120523,0.183848416855219,-0.842251708940935)) ;
#22106 = DIRECTION('center_axis',(0.0198775103691822,-0.982954607100363,-0.182770689558513)) ;
#22107 = DIRECTION('ref_axis',(0.106276087274989,0.183848416855221,-0.97719248507822)) ;
#22108 = DIRECTION('center_axis',(0.0587030808149489,-0.982954607100363,-0.174224535249788)) ;
#22109 = DIRECTION('ref_axis',(0.31385891010127,0.183848416855221,-0.931500050547434)) ;
#22110 = DIRECTION('center_axis',(0.126432456782393,-0.982954607100363,-0.133473121834093)) ;
#22111 = DIRECTION('ref_axis',(-0.675977351380272,-0.183848416855219,0.713620613520057)) ;
#22112 = DIRECTION('center_axis',(0.170790899233672,-0.982954607100363,-0.0680493138769549)) ;
#22113 = DIRECTION('ref_axis',(-0.913141946632923,-0.18384841685522,0.363829005054938)) ;
#22114 = DIRECTION('center_axis',(0.183578787313568,-0.982954607100363,0.00995335263369878)) ;
#22115 = DIRECTION('ref_axis',(-0.981513019488616,-0.183848416855221,-0.0532160896174178)) ;
#22116 = DIRECTION('center_axis',(0.16243229064392,-0.982954607100363,0.0861161502642797)) ;
#22117 = DIRECTION('ref_axis',(-0.868452234516837,-0.183848416855221,-0.460424234790635)) ;
#22118 = DIRECTION('center_axis',(0.111260321384975,-0.982954607100363,0.146360449799402)) ;
#22119 = DIRECTION('ref_axis',(-0.594858782922928,-0.183848416855221,-0.782523346616113)) ;
#22120 = DIRECTION('center_axis',(0.0395219751034661,-0.982954607100363,0.179550143035566)) ;
#22121 = DIRECTION('ref_axis',(-0.211306184595861,-0.183848416855221,-0.959973674624137)) ;
#22122 = DIRECTION('center_axis',(-0.0771959465766158,-0.982954607100363,
0.166856304083218)) ;
#22123 = DIRECTION('ref_axis',(0.412731926849952,-0.183848416855221,-0.892105440056586)) ;
#22124 = DIRECTION('center_axis',(-0.140122287222336,-0.982954607100363,0.119020943550922)) ;
#22125 = DIRECTION('ref_axis',(-0.749170703444845,0.18384841685522,0.636351331199822)) ;
#22126 = DIRECTION('center_axis',(-0.17714714068552,-0.982954607100363,0.0491846615025046)) ;
#22127 = DIRECTION('ref_axis',(-0.947125904318295,0.183848416855222,0.262968212887186)) ;
#22128 = DIRECTION('center_axis',(-0.181426493880003,-0.982954607100363,-0.0297433639419022)) ;
#22129 = DIRECTION('ref_axis',(-0.97000567674102,0.183848416855221,-0.159024358857453)) ;
#22130 = DIRECTION('center_axis',(-0.152169311959628,-0.982954607100363,-0.1031733535265)) ;
#22131 = DIRECTION('ref_axis',(-0.813580713984562,0.18384841685522,-0.551621411343141)) ;
#22132 = DIRECTION('center_axis',(-0.0947837604455976,-0.982954607100363,
-0.157531835309445)) ;
#22133 = DIRECTION('ref_axis',(-0.506766039120481,0.183848416855219,-0.842251708940961)) ;
#22134 = DIRECTION('center_axis',(-0.0198775103691822,-0.982954607100363,
-0.182770689558513)) ;
#22135 = DIRECTION('ref_axis',(-0.106276087274979,0.183848416855221,-0.977192485078221)) ;
#22136 = DIRECTION('center_axis',(-0.0587030808149489,-0.982954607100363,
-0.174224535249788)) ;
#22137 = DIRECTION('ref_axis',(-0.313858910101256,0.183848416855221,-0.931500050547439)) ;
#22138 = DIRECTION('center_axis',(-0.126432456782393,-0.982954607100363,-0.133473121834093)) ;
#22139 = DIRECTION('ref_axis',(-0.675977351380318,0.183848416855219,-0.713620613520013)) ;
#22140 = DIRECTION('center_axis',(-0.170790899233673,-0.982954607100363,-0.0680493138769549)) ;
#22141 = DIRECTION('ref_axis',(-0.913141946632883,0.183848416855221,-0.363829005055038)) ;
#22142 = DIRECTION('center_axis',(-0.183578787313568,-0.982954607100363,0.00995335263369855)) ;
#22143 = DIRECTION('ref_axis',(-0.981513019488616,0.183848416855221,0.0532160896174153)) ;
#22144 = DIRECTION('center_axis',(-0.16243229064392,-0.982954607100363,0.0861161502642797)) ;
#22145 = DIRECTION('ref_axis',(-0.868452234516967,0.18384841685522,0.460424234790391)) ;
#22146 = DIRECTION('center_axis',(-0.111260321384975,-0.982954607100363,0.146360449799403)) ;
#22147 = DIRECTION('ref_axis',(0.594858782923022,-0.183848416855222,-0.782523346616042)) ;
#22148 = DIRECTION('center_axis',(-0.039521975103467,-0.982954607100363,0.179550143035566)) ;
#22149 = DIRECTION('ref_axis',(0.211306184595843,-0.183848416855221,-0.959973674624141)) ;
#22150 = DIRECTION('center_axis',(1.83697019872103E-16,1.,1.91045767932109E-48)) ;
#22151 = DIRECTION('ref_axis',(6.12323399573677E-17,-1.12481983699639E-32,
1.)) ;
#22152 = DIRECTION('center_axis',(1.83697019872103E-16,1.,1.91045767932109E-48)) ;
#22153 = DIRECTION('ref_axis',(6.12323399573677E-17,-1.12481983699639E-32,
1.)) ;
#22154 = DIRECTION('',(-1.83697019872103E-16,-1.,-1.91045767932109E-48)) ;
#22155 = DIRECTION('center_axis',(1.83697019872103E-16,1.,1.91045767932109E-48)) ;
#22156 = DIRECTION('ref_axis',(6.12323399573677E-17,-1.12481983699639E-32,
1.)) ;
#22157 = DIRECTION('center_axis',(1.83697019872103E-16,1.,0.)) ;
#22158 = DIRECTION('ref_axis',(0.,0.,1.)) ;
#22159 = DIRECTION('center_axis',(1.83697019872103E-16,1.,0.)) ;
#22160 = DIRECTION('ref_axis',(6.12323399573677E-17,-1.12481983699639E-32,
1.)) ;
#22161 = DIRECTION('center_axis',(-1.,1.83697019872103E-16,1.22464679914735E-16)) ;
#22162 = DIRECTION('ref_axis',(-1.22464679914735E-16,0.,-1.)) ;
#22163 = DIRECTION('center_axis',(1.83697019872103E-16,1.,0.)) ;
#22164 = DIRECTION('ref_axis',(6.12323399573677E-17,-1.12481983699639E-32,
1.)) ;
#22165 = DIRECTION('center_axis',(1.83697019872103E-16,1.,0.)) ;
#22166 = DIRECTION('ref_axis',(0.,0.,1.)) ;
#22167 = DIRECTION('center_axis',(1.83697019872103E-16,1.,2.10365691773288E-48)) ;
#22168 = DIRECTION('ref_axis',(6.12323399573676E-17,-1.12481983699639E-32,
1.)) ;
#22169 = DIRECTION('center_axis',(-1.,1.83697019872103E-16,1.22464679914735E-16)) ;
#22170 = DIRECTION('ref_axis',(-1.22464679914735E-16,0.,-1.)) ;
#22171 = DIRECTION('center_axis',(1.83697019872103E-16,1.,-1.99295781592863E-48)) ;
#22172 = DIRECTION('ref_axis',(6.12323399573676E-17,-1.12481983699639E-32,
1.)) ;
#22173 = DIRECTION('center_axis',(1.83697019872103E-16,1.,0.)) ;
#22174 = DIRECTION('ref_axis',(0.,0.,1.)) ;
#22175 = DIRECTION('center_axis',(1.83697019872103E-16,1.,-1.99295781592863E-48)) ;
#22176 = DIRECTION('ref_axis',(6.12323399573676E-17,-1.12481983699639E-32,
1.)) ;
#22177 = DIRECTION('center_axis',(-1.,1.83697019872103E-16,1.22464679914735E-16)) ;
#22178 = DIRECTION('ref_axis',(-1.22464679914735E-16,0.,-1.)) ;
#22179 = DIRECTION('center_axis',(1.83697019872103E-16,1.,-2.01979869638278E-48)) ;
#22180 = DIRECTION('ref_axis',(6.12323399573676E-17,-1.12481983699639E-32,
1.)) ;
#22181 = DIRECTION('center_axis',(1.83697019872103E-16,1.,0.)) ;
#22182 = DIRECTION('ref_axis',(6.12323399573677E-17,-1.12481983699639E-32,
1.)) ;
#22183 = DIRECTION('',(1.83697019872103E-16,1.,0.)) ;
#22184 = DIRECTION('center_axis',(1.83697019872103E-16,1.,0.)) ;
#22185 = DIRECTION('ref_axis',(6.12323399573677E-17,-1.12481983699639E-32,
1.)) ;
#22186 = DIRECTION('center_axis',(1.83697019872103E-16,1.,0.)) ;
#22187 = DIRECTION('ref_axis',(0.,0.,1.)) ;
#22188 = DIRECTION('center_axis',(-1.,1.83697019872103E-16,1.22464679914735E-16)) ;
#22189 = DIRECTION('ref_axis',(-1.22464679914735E-16,0.,-1.)) ;
#22190 = DIRECTION('center_axis',(1.83697019872103E-16,1.,0.)) ;
#22191 = DIRECTION('ref_axis',(6.12323399573677E-17,-1.12481983699639E-32,
1.)) ;
#22192 = DIRECTION('center_axis',(1.83697019872103E-16,1.,-1.99295781592863E-48)) ;
#22193 = DIRECTION('ref_axis',(6.12323399573676E-17,-1.12481983699639E-32,
1.)) ;
#22194 = DIRECTION('',(-1.83697019872103E-16,-1.,1.99295781592863E-48)) ;
#22195 = DIRECTION('center_axis',(1.83697019872103E-16,1.,1.83697019872103E-16)) ;
#22196 = DIRECTION('ref_axis',(6.12323399573676E-17,-1.83697019872103E-16,
1.)) ;
#22197 = DIRECTION('center_axis',(-1.83697019872103E-16,-1.,-5.58347057653491E-16)) ;
#22198 = DIRECTION('ref_axis',(-6.12323399573676E-17,5.58347057653491E-16,
-1.)) ;
#22199 = DIRECTION('center_axis',(1.83697019872103E-16,1.,6.12323399573677E-17)) ;
#22200 = DIRECTION('ref_axis',(6.12323399573676E-17,-6.12323399573677E-17,
1.)) ;
#22201 = DIRECTION('center_axis',(1.80565831993891E-16,0.982954607100363,
-0.18384841685522)) ;
#22202 = DIRECTION('ref_axis',(6.12323399573677E-17,0.18384841685522,0.982954607100363)) ;
#22203 = DIRECTION('center_axis',(1.80565831993891E-16,0.982954607100363,
-0.18384841685522)) ;
#22204 = DIRECTION('ref_axis',(6.12323399573677E-17,0.18384841685522,0.982954607100363)) ;
#22205 = DIRECTION('center_axis',(1.80565831993891E-16,0.982954607100363,
-0.18384841685522)) ;
#22206 = DIRECTION('ref_axis',(6.12323399573677E-17,0.18384841685522,0.982954607100363)) ;
#22207 = DIRECTION('center_axis',(0.039521975103467,0.982954607100363,-0.179550143035566)) ;
#22208 = DIRECTION('ref_axis',(-0.211306184595818,0.183848416855221,0.959973674624147)) ;
#22209 = DIRECTION('center_axis',(0.039521975103467,0.982954607100363,-0.179550143035567)) ;
#22210 = DIRECTION('ref_axis',(-0.211306184595818,0.183848416855222,0.959973674624146)) ;
#22211 = DIRECTION('center_axis',(0.039521975103467,0.982954607100363,-0.179550143035567)) ;
#22212 = DIRECTION('ref_axis',(-0.211306184595818,0.183848416855222,0.959973674624146)) ;
#22213 = DIRECTION('center_axis',(0.0771959465766159,0.982954607100363,-0.166856304083218)) ;
#22214 = DIRECTION('ref_axis',(-0.412731926849895,0.183848416855221,0.892105440056612)) ;
#22215 = DIRECTION('center_axis',(0.0771959465766159,0.982954607100363,-0.166856304083218)) ;
#22216 = DIRECTION('ref_axis',(-0.412731926849895,0.183848416855221,0.892105440056612)) ;
#22217 = DIRECTION('center_axis',(0.0771959465766159,0.982954607100363,-0.166856304083218)) ;
#22218 = DIRECTION('ref_axis',(-0.412731926849895,0.183848416855221,0.892105440056612)) ;
#22219 = DIRECTION('center_axis',(0.111260321384975,0.982954607100363,-0.146360449799403)) ;
#22220 = DIRECTION('ref_axis',(-0.594858782923058,0.183848416855222,0.782523346616014)) ;
#22221 = DIRECTION('center_axis',(0.111260321384975,0.982954607100363,-0.146360449799403)) ;
#22222 = DIRECTION('ref_axis',(-0.594858782923058,0.183848416855222,0.782523346616014)) ;
#22223 = DIRECTION('center_axis',(0.111260321384975,0.982954607100363,-0.146360449799403)) ;
#22224 = DIRECTION('ref_axis',(-0.594858782923058,0.183848416855222,0.782523346616014)) ;
#22225 = DIRECTION('center_axis',(0.140122287222337,0.982954607100363,-0.119020943550922)) ;
#22226 = DIRECTION('ref_axis',(-0.749170703444791,0.18384841685522,0.636351331199885)) ;
#22227 = DIRECTION('center_axis',(0.140122287222337,0.982954607100363,-0.119020943550922)) ;
#22228 = DIRECTION('ref_axis',(-0.749170703444791,0.18384841685522,0.636351331199885)) ;
#22229 = DIRECTION('center_axis',(0.140122287222337,0.982954607100363,-0.119020943550922)) ;
#22230 = DIRECTION('ref_axis',(-0.749170703444791,0.18384841685522,0.636351331199885)) ;
#22231 = DIRECTION('center_axis',(0.162432290643921,0.982954607100363,-0.0861161502642798)) ;
#22232 = DIRECTION('ref_axis',(-0.868452234516879,0.183848416855221,0.460424234790555)) ;
#22233 = DIRECTION('center_axis',(0.162432290643921,0.982954607100363,-0.0861161502642798)) ;
#22234 = DIRECTION('ref_axis',(-0.868452234516879,0.183848416855221,0.460424234790555)) ;
#22235 = DIRECTION('center_axis',(0.162432290643921,0.982954607100363,-0.0861161502642798)) ;
#22236 = DIRECTION('ref_axis',(-0.868452234516879,0.183848416855221,0.460424234790555)) ;
#22237 = DIRECTION('center_axis',(0.17714714068552,0.982954607100363,-0.0491846615025047)) ;
#22238 = DIRECTION('ref_axis',(-0.94712590431829,0.183848416855222,0.262968212887203)) ;
#22239 = DIRECTION('center_axis',(0.17714714068552,0.982954607100363,-0.0491846615025047)) ;
#22240 = DIRECTION('ref_axis',(-0.94712590431829,0.183848416855222,0.262968212887203)) ;
#22241 = DIRECTION('center_axis',(0.17714714068552,0.982954607100363,-0.0491846615025047)) ;
#22242 = DIRECTION('ref_axis',(-0.94712590431829,0.183848416855222,0.262968212887203)) ;
#22243 = DIRECTION('center_axis',(0.183578787313568,0.982954607100363,-0.00995335263369857)) ;
#22244 = DIRECTION('ref_axis',(-0.981513019488616,0.183848416855221,0.0532160896174226)) ;
#22245 = DIRECTION('center_axis',(0.183578787313568,0.982954607100363,-0.00995335263369857)) ;
#22246 = DIRECTION('ref_axis',(-0.981513019488616,0.183848416855221,0.0532160896174225)) ;
#22247 = DIRECTION('center_axis',(0.183578787313568,0.982954607100363,-0.00995335263369857)) ;
#22248 = DIRECTION('ref_axis',(-0.981513019488616,0.183848416855221,0.0532160896174225)) ;
#22249 = DIRECTION('center_axis',(0.181426493880004,0.982954607100363,0.0297433639419023)) ;
#22250 = DIRECTION('ref_axis',(-0.970005676741023,0.183848416855222,-0.159024358857435)) ;
#22251 = DIRECTION('center_axis',(0.181426493880004,0.982954607100363,0.0297433639419023)) ;
#22252 = DIRECTION('ref_axis',(-0.970005676741023,0.183848416855222,-0.159024358857435)) ;
#22253 = DIRECTION('center_axis',(0.181426493880004,0.982954607100363,0.0297433639419023)) ;
#22254 = DIRECTION('ref_axis',(-0.970005676741023,0.183848416855222,-0.159024358857435)) ;
#22255 = DIRECTION('center_axis',(0.170790899233673,0.982954607100363,0.068049313876955)) ;
#22256 = DIRECTION('ref_axis',(-0.913141946632898,0.183848416855221,-0.363829005055)) ;
#22257 = DIRECTION('center_axis',(0.170790899233673,0.982954607100363,0.0680493138769549)) ;
#22258 = DIRECTION('ref_axis',(-0.913141946632898,0.183848416855221,-0.363829005055)) ;
#22259 = DIRECTION('center_axis',(0.170790899233673,0.982954607100363,0.0680493138769549)) ;
#22260 = DIRECTION('ref_axis',(-0.913141946632898,0.183848416855221,-0.363829005055)) ;
#22261 = DIRECTION('center_axis',(0.152169311959629,0.982954607100363,0.103173353526501)) ;
#22262 = DIRECTION('ref_axis',(-0.813580713984599,0.183848416855221,-0.551621411343086)) ;
#22263 = DIRECTION('center_axis',(0.152169311959629,0.982954607100363,0.103173353526501)) ;
#22264 = DIRECTION('ref_axis',(-0.813580713984599,0.183848416855221,-0.551621411343086)) ;
#22265 = DIRECTION('center_axis',(0.152169311959629,0.982954607100363,0.103173353526501)) ;
#22266 = DIRECTION('ref_axis',(-0.813580713984599,0.183848416855221,-0.551621411343086)) ;
#22267 = DIRECTION('center_axis',(0.126432456782393,0.982954607100363,0.133473121834094)) ;
#22268 = DIRECTION('ref_axis',(-0.675977351380398,0.18384841685522,-0.713620613519937)) ;
#22269 = DIRECTION('center_axis',(0.126432456782393,0.982954607100363,0.133473121834094)) ;
#22270 = DIRECTION('ref_axis',(-0.675977351380398,0.18384841685522,-0.713620613519937)) ;
#22271 = DIRECTION('center_axis',(0.126432456782393,0.982954607100363,0.133473121834094)) ;
#22272 = DIRECTION('ref_axis',(-0.675977351380398,0.18384841685522,-0.713620613519937)) ;
#22273 = DIRECTION('center_axis',(0.0947837604455978,0.982954607100363,0.157531835309445)) ;
#22274 = DIRECTION('ref_axis',(-0.506766039120516,0.18384841685522,-0.84225170894094)) ;
#22275 = DIRECTION('center_axis',(0.0947837604455977,0.982954607100363,0.157531835309445)) ;
#22276 = DIRECTION('ref_axis',(-0.506766039120516,0.18384841685522,-0.84225170894094)) ;
#22277 = DIRECTION('center_axis',(0.0947837604455977,0.982954607100363,0.157531835309445)) ;
#22278 = DIRECTION('ref_axis',(-0.506766039120516,0.18384841685522,-0.84225170894094)) ;
#22279 = DIRECTION('center_axis',(0.0587030808149489,0.982954607100363,0.174224535249788)) ;
#22280 = DIRECTION('ref_axis',(-0.313858910101358,0.183848416855221,-0.931500050547404)) ;
#22281 = DIRECTION('center_axis',(0.0587030808149489,0.982954607100363,0.174224535249788)) ;
#22282 = DIRECTION('ref_axis',(-0.313858910101358,0.183848416855221,-0.931500050547404)) ;
#22283 = DIRECTION('center_axis',(0.0587030808149489,0.982954607100363,0.174224535249788)) ;
#22284 = DIRECTION('ref_axis',(-0.313858910101358,0.183848416855221,-0.931500050547404)) ;
#22285 = DIRECTION('center_axis',(0.0198775103691822,0.982954607100363,0.182770689558513)) ;
#22286 = DIRECTION('ref_axis',(-0.106276087274983,0.183848416855221,-0.977192485078221)) ;
#22287 = DIRECTION('center_axis',(0.0198775103691822,0.982954607100363,0.182770689558513)) ;
#22288 = DIRECTION('ref_axis',(-0.106276087274983,0.183848416855221,-0.977192485078221)) ;
#22289 = DIRECTION('center_axis',(0.0198775103691822,0.982954607100363,0.182770689558513)) ;
#22290 = DIRECTION('ref_axis',(-0.106276087274983,0.183848416855221,-0.977192485078221)) ;
#22291 = DIRECTION('center_axis',(-0.0198775103691822,0.982954607100363,0.182770689558513)) ;
#22292 = DIRECTION('ref_axis',(0.106276087274983,0.183848416855221,-0.977192485078221)) ;
#22293 = DIRECTION('center_axis',(-0.0198775103691822,0.982954607100363,0.182770689558513)) ;
#22294 = DIRECTION('ref_axis',(0.106276087274983,0.183848416855221,-0.977192485078221)) ;
#22295 = DIRECTION('center_axis',(-0.0198775103691822,0.982954607100363,0.182770689558513)) ;
#22296 = DIRECTION('ref_axis',(0.106276087274983,0.183848416855221,-0.977192485078221)) ;
#22297 = DIRECTION('center_axis',(-0.0587030808149489,0.982954607100363,0.174224535249788)) ;
#22298 = DIRECTION('ref_axis',(0.313858910101358,0.183848416855221,-0.931500050547404)) ;
#22299 = DIRECTION('center_axis',(-0.0587030808149489,0.982954607100363,0.174224535249788)) ;
#22300 = DIRECTION('ref_axis',(0.313858910101358,0.183848416855221,-0.931500050547404)) ;
#22301 = DIRECTION('center_axis',(-0.0587030808149489,0.982954607100363,0.174224535249788)) ;
#22302 = DIRECTION('ref_axis',(0.313858910101358,0.183848416855221,-0.931500050547404)) ;
#22303 = DIRECTION('center_axis',(-0.0947837604455977,0.982954607100363,0.157531835309445)) ;
#22304 = DIRECTION('ref_axis',(0.506766039120516,0.18384841685522,-0.842251708940939)) ;
#22305 = DIRECTION('center_axis',(-0.0947837604455978,0.982954607100363,0.157531835309445)) ;
#22306 = DIRECTION('ref_axis',(0.506766039120516,0.18384841685522,-0.842251708940939)) ;
#22307 = DIRECTION('center_axis',(-0.0947837604455978,0.982954607100363,0.157531835309445)) ;
#22308 = DIRECTION('ref_axis',(0.506766039120516,0.18384841685522,-0.842251708940939)) ;
#22309 = DIRECTION('center_axis',(-0.126432456782393,0.982954607100363,0.133473121834094)) ;
#22310 = DIRECTION('ref_axis',(0.6759773513804,0.18384841685522,-0.713620613519935)) ;
#22311 = DIRECTION('center_axis',(-0.126432456782393,0.982954607100363,0.133473121834094)) ;
#22312 = DIRECTION('ref_axis',(0.6759773513804,0.18384841685522,-0.713620613519935)) ;
#22313 = DIRECTION('center_axis',(-0.126432456782393,0.982954607100363,0.133473121834094)) ;
#22314 = DIRECTION('ref_axis',(0.6759773513804,0.18384841685522,-0.713620613519935)) ;
#22315 = DIRECTION('center_axis',(-0.152169311959629,0.982954607100363,0.103173353526501)) ;
#22316 = DIRECTION('ref_axis',(0.813580713984599,0.183848416855221,-0.551621411343086)) ;
#22317 = DIRECTION('center_axis',(-0.152169311959629,0.982954607100363,0.103173353526501)) ;
#22318 = DIRECTION('ref_axis',(0.813580713984599,0.183848416855221,-0.551621411343086)) ;
#22319 = DIRECTION('center_axis',(-0.152169311959629,0.982954607100363,0.103173353526501)) ;
#22320 = DIRECTION('ref_axis',(0.813580713984599,0.183848416855221,-0.551621411343086)) ;
#22321 = DIRECTION('center_axis',(-0.170790899233673,0.982954607100363,0.068049313876955)) ;
#22322 = DIRECTION('ref_axis',(0.913141946632899,0.183848416855221,-0.363829005054997)) ;
#22323 = DIRECTION('center_axis',(-0.170790899233673,0.982954607100363,0.0680493138769549)) ;
#22324 = DIRECTION('ref_axis',(0.913141946632899,0.183848416855221,-0.363829005054997)) ;
#22325 = DIRECTION('center_axis',(-0.170790899233673,0.982954607100363,0.0680493138769549)) ;
#22326 = DIRECTION('ref_axis',(0.913141946632899,0.183848416855221,-0.363829005054997)) ;
#22327 = DIRECTION('center_axis',(-0.181426493880004,0.982954607100363,0.0297433639419023)) ;
#22328 = DIRECTION('ref_axis',(0.970005676741023,0.183848416855222,-0.159024358857436)) ;
#22329 = DIRECTION('center_axis',(-0.181426493880004,0.982954607100363,0.0297433639419023)) ;
#22330 = DIRECTION('ref_axis',(0.970005676741023,0.183848416855222,-0.159024358857436)) ;
#22331 = DIRECTION('center_axis',(-0.181426493880004,0.982954607100363,0.0297433639419023)) ;
#22332 = DIRECTION('ref_axis',(0.970005676741023,0.183848416855222,-0.159024358857436)) ;
#22333 = DIRECTION('center_axis',(-0.183578787313568,0.982954607100363,-0.00995335263369879)) ;
#22334 = DIRECTION('ref_axis',(0.981513019488616,0.183848416855221,0.0532160896174224)) ;
#22335 = DIRECTION('center_axis',(-0.183578787313568,0.982954607100363,-0.0099533526336988)) ;
#22336 = DIRECTION('ref_axis',(0.981513019488616,0.183848416855221,0.0532160896174224)) ;
#22337 = DIRECTION('center_axis',(-0.183578787313568,0.982954607100363,-0.0099533526336988)) ;
#22338 = DIRECTION('ref_axis',(0.981513019488616,0.183848416855221,0.0532160896174224)) ;
#22339 = DIRECTION('center_axis',(-0.17714714068552,0.982954607100363,-0.0491846615025056)) ;
#22340 = DIRECTION('ref_axis',(0.94712590431829,0.183848416855222,0.262968212887203)) ;
#22341 = DIRECTION('center_axis',(-0.17714714068552,0.982954607100363,-0.0491846615025056)) ;
#22342 = DIRECTION('ref_axis',(0.94712590431829,0.183848416855222,0.262968212887203)) ;
#22343 = DIRECTION('center_axis',(-0.17714714068552,0.982954607100363,-0.0491846615025056)) ;
#22344 = DIRECTION('ref_axis',(0.94712590431829,0.183848416855222,0.262968212887203)) ;
#22345 = DIRECTION('center_axis',(-0.162432290643921,0.982954607100363,-0.0861161502642798)) ;
#22346 = DIRECTION('ref_axis',(0.868452234516879,0.183848416855221,0.460424234790556)) ;
#22347 = DIRECTION('center_axis',(-0.16243229064392,0.982954607100363,-0.0861161502642798)) ;
#22348 = DIRECTION('ref_axis',(0.868452234516879,0.183848416855221,0.460424234790556)) ;
#22349 = DIRECTION('center_axis',(-0.16243229064392,0.982954607100363,-0.0861161502642798)) ;
#22350 = DIRECTION('ref_axis',(0.868452234516879,0.183848416855221,0.460424234790556)) ;
#22351 = DIRECTION('center_axis',(-0.140122287222337,0.982954607100363,-0.119020943550922)) ;
#22352 = DIRECTION('ref_axis',(0.749170703444791,0.18384841685522,0.636351331199885)) ;
#22353 = DIRECTION('center_axis',(-0.140122287222337,0.982954607100363,-0.119020943550922)) ;
#22354 = DIRECTION('ref_axis',(0.749170703444791,0.18384841685522,0.636351331199885)) ;
#22355 = DIRECTION('center_axis',(-0.140122287222337,0.982954607100363,-0.119020943550922)) ;
#22356 = DIRECTION('ref_axis',(0.749170703444791,0.18384841685522,0.636351331199885)) ;
#22357 = DIRECTION('center_axis',(-0.111260321384975,0.982954607100363,-0.146360449799403)) ;
#22358 = DIRECTION('ref_axis',(0.594858782923056,0.183848416855222,0.782523346616016)) ;
#22359 = DIRECTION('center_axis',(-0.111260321384975,0.982954607100363,-0.146360449799403)) ;
#22360 = DIRECTION('ref_axis',(0.594858782923056,0.183848416855222,0.782523346616015)) ;
#22361 = DIRECTION('center_axis',(-0.111260321384975,0.982954607100363,-0.146360449799403)) ;
#22362 = DIRECTION('ref_axis',(0.594858782923056,0.183848416855222,0.782523346616015)) ;
#22363 = DIRECTION('center_axis',(-0.077195946576616,0.982954607100363,-0.166856304083218)) ;
#22364 = DIRECTION('ref_axis',(0.412731926849892,0.183848416855221,0.892105440056614)) ;
#22365 = DIRECTION('center_axis',(-0.0771959465766159,0.982954607100363,-0.166856304083218)) ;
#22366 = DIRECTION('ref_axis',(0.412731926849892,0.183848416855221,0.892105440056614)) ;
#22367 = DIRECTION('center_axis',(-0.0771959465766159,0.982954607100363,-0.166856304083218)) ;
#22368 = DIRECTION('ref_axis',(0.412731926849892,0.183848416855221,0.892105440056614)) ;
#22369 = DIRECTION('center_axis',(-1.83697019872103E-16,-1.,0.)) ;
#22370 = DIRECTION('ref_axis',(-6.12323399573677E-17,1.12481983699639E-32,
-1.)) ;
#22371 = DIRECTION('center_axis',(-0.0395219751034661,0.982954607100363,-0.179550143035566)) ;
#22372 = DIRECTION('ref_axis',(0.211306184595818,0.183848416855221,0.959973674624147)) ;
#22373 = DIRECTION('center_axis',(-0.0395219751034661,0.982954607100363,-0.179550143035566)) ;
#22374 = DIRECTION('ref_axis',(0.211306184595818,0.183848416855221,0.959973674624147)) ;
#22375 = DIRECTION('center_axis',(-0.0395219751034661,0.982954607100363,-0.179550143035566)) ;
#22376 = DIRECTION('ref_axis',(0.211306184595818,0.183848416855221,0.959973674624147)) ;
#22377 = DIRECTION('center_axis',(1.83697019872103E-16,1.,2.02545731253837E-48)) ;
#22378 = DIRECTION('ref_axis',(6.12323399573677E-17,-1.12481983699639E-32,
1.)) ;
#22379 = DIRECTION('',(1.46793425709383E-16,-0.183848416855218,0.982954607100364)) ;
#22380 = DIRECTION('center_axis',(-1.80565831993891E-16,-0.982954607100363,
0.18384841685522)) ;
#22381 = DIRECTION('ref_axis',(1.,-1.84419353919637E-10,-9.8600616806345E-10)) ;
#22382 = DIRECTION('center_axis',(1.80565831993891E-16,0.982954607100363,
-0.18384841685522)) ;
#22383 = DIRECTION('ref_axis',(6.12323399573677E-17,0.18384841685522,0.982954607100363)) ;
#22384 = DIRECTION('center_axis',(1.80565831993891E-16,0.982954607100363,
-0.18384841685522)) ;
#22385 = DIRECTION('ref_axis',(6.12323399573677E-17,0.18384841685522,0.982954607100363)) ;
#22386 = DIRECTION('center_axis',(-1.80565831993891E-16,-0.982954607100363,
0.18384841685522)) ;
#22387 = DIRECTION('ref_axis',(-6.12323399573676E-17,-0.18384841685522,-0.982954607100363)) ;
#22388 = DIRECTION('center_axis',(1.80565831993891E-16,0.982954607100363,
-0.18384841685522)) ;
#22389 = DIRECTION('ref_axis',(6.12323399573677E-17,0.18384841685522,0.982954607100363)) ;
#22390 = DIRECTION('center_axis',(1.80565831993891E-16,0.982954607100363,
-0.18384841685522)) ;
#22391 = DIRECTION('ref_axis',(6.12323399573677E-17,0.18384841685522,0.982954607100363)) ;
#22392 = DIRECTION('center_axis',(-1.80565831993891E-16,-0.982954607100363,
0.18384841685522)) ;
#22393 = DIRECTION('ref_axis',(6.12323399573676E-17,0.18384841685522,0.982954607100363)) ;
#22394 = DIRECTION('center_axis',(-0.039521975103467,-0.982954607100363,0.179550143035567)) ;
#22395 = DIRECTION('ref_axis',(0.97662278989035,-1.9439115888104E-6,0.21496028996773)) ;
#22396 = DIRECTION('center_axis',(0.039521975103467,0.982954607100363,-0.179550143035566)) ;
#22397 = DIRECTION('ref_axis',(-0.211306184595818,0.183848416855221,0.959973674624147)) ;
#22398 = DIRECTION('center_axis',(0.039521975103467,0.982954607100363,-0.179550143035566)) ;
#22399 = DIRECTION('ref_axis',(-0.211306184595818,0.183848416855221,0.959973674624147)) ;
#22400 = DIRECTION('center_axis',(-0.039521975103467,-0.982954607100363,0.179550143035566)) ;
#22401 = DIRECTION('ref_axis',(0.211306184595818,-0.183848416855221,-0.959973674624147)) ;
#22402 = DIRECTION('center_axis',(0.039521975103467,0.982954607100363,-0.179550143035566)) ;
#22403 = DIRECTION('ref_axis',(-0.211306184595818,0.183848416855221,0.959973674624147)) ;
#22404 = DIRECTION('center_axis',(0.039521975103467,0.982954607100363,-0.179550143035566)) ;
#22405 = DIRECTION('ref_axis',(-0.211306184595818,0.183848416855221,0.959973674624147)) ;
#22406 = DIRECTION('center_axis',(-0.039521975103467,-0.982954607100363,0.179550143035567)) ;
#22407 = DIRECTION('ref_axis',(-0.211306184595818,0.183848416855222,0.959973674624146)) ;
#22408 = DIRECTION('center_axis',(-0.0771959465766159,-0.982954607100363,
0.166856304083218)) ;
#22409 = DIRECTION('ref_axis',(0.907575420122405,-2.010944117565E-10,0.419889100584476)) ;
#22410 = DIRECTION('center_axis',(0.077195946576616,0.982954607100363,-0.166856304083218)) ;
#22411 = DIRECTION('ref_axis',(-0.412731926849895,0.183848416855221,0.892105440056612)) ;
#22412 = DIRECTION('center_axis',(0.077195946576616,0.982954607100363,-0.166856304083218)) ;
#22413 = DIRECTION('ref_axis',(-0.412731926849895,0.183848416855221,0.892105440056612)) ;
#22414 = DIRECTION('center_axis',(-0.0771959465766158,-0.982954607100363,
0.166856304083218)) ;
#22415 = DIRECTION('ref_axis',(0.412731926849895,-0.183848416855221,-0.892105440056612)) ;
#22416 = DIRECTION('center_axis',(0.077195946576616,0.982954607100363,-0.166856304083218)) ;
#22417 = DIRECTION('ref_axis',(-0.412731926849895,0.183848416855221,0.892105440056612)) ;
#22418 = DIRECTION('center_axis',(0.077195946576616,0.982954607100363,-0.166856304083218)) ;
#22419 = DIRECTION('ref_axis',(-0.412731926849895,0.183848416855221,0.892105440056612)) ;
#22420 = DIRECTION('center_axis',(-0.0771959465766159,-0.982954607100363,
0.166856304083218)) ;
#22421 = DIRECTION('ref_axis',(-0.412731926849895,0.183848416855221,0.892105440056612)) ;
#22422 = DIRECTION('center_axis',(-0.111260321384975,-0.982954607100363,0.146360449799403)) ;
#22423 = DIRECTION('ref_axis',(0.796093066345906,-1.9788077417699E-10,0.605174214351514)) ;
#22424 = DIRECTION('center_axis',(0.111260321384975,0.982954607100363,-0.146360449799403)) ;
#22425 = DIRECTION('ref_axis',(-0.594858782923058,0.183848416855222,0.782523346616014)) ;
#22426 = DIRECTION('center_axis',(0.111260321384975,0.982954607100363,-0.146360449799403)) ;
#22427 = DIRECTION('ref_axis',(-0.594858782923058,0.183848416855222,0.782523346616014)) ;
#22428 = DIRECTION('center_axis',(-0.111260321384975,-0.982954607100363,0.146360449799403)) ;
#22429 = DIRECTION('ref_axis',(0.594858782923058,-0.183848416855222,-0.782523346616014)) ;
#22430 = DIRECTION('center_axis',(0.111260321384975,0.982954607100363,-0.146360449799403)) ;
#22431 = DIRECTION('ref_axis',(-0.594858782923058,0.183848416855222,0.782523346616014)) ;
#22432 = DIRECTION('center_axis',(0.111260321384975,0.982954607100363,-0.146360449799403)) ;
#22433 = DIRECTION('ref_axis',(-0.594858782923058,0.183848416855222,0.782523346616014)) ;
#22434 = DIRECTION('center_axis',(-0.111260321384975,-0.982954607100363,0.146360449799403)) ;
#22435 = DIRECTION('ref_axis',(-0.594858782923058,0.183848416855222,0.782523346616014)) ;
#22436 = DIRECTION('center_axis',(-0.140122287222336,-0.982954607100363,0.119020943550922)) ;
#22437 = DIRECTION('ref_axis',(0.647386285486055,-1.72818379975615E-10,0.76216205452946)) ;
#22438 = DIRECTION('center_axis',(0.140122287222336,0.982954607100363,-0.119020943550922)) ;
#22439 = DIRECTION('ref_axis',(-0.749170703444791,0.18384841685522,0.636351331199885)) ;
#22440 = DIRECTION('center_axis',(0.140122287222336,0.982954607100363,-0.119020943550922)) ;
#22441 = DIRECTION('ref_axis',(-0.749170703444791,0.18384841685522,0.636351331199885)) ;
#22442 = DIRECTION('center_axis',(-0.140122287222336,-0.982954607100363,0.119020943550922)) ;
#22443 = DIRECTION('ref_axis',(0.749170703444791,-0.18384841685522,-0.636351331199886)) ;
#22444 = DIRECTION('center_axis',(0.140122287222336,0.982954607100363,-0.119020943550922)) ;
#22445 = DIRECTION('ref_axis',(-0.749170703444791,0.18384841685522,0.636351331199885)) ;
#22446 = DIRECTION('center_axis',(0.140122287222336,0.982954607100363,-0.119020943550922)) ;
#22447 = DIRECTION('ref_axis',(-0.749170703444791,0.18384841685522,0.636351331199885)) ;
#22448 = DIRECTION('center_axis',(-0.140122287222336,-0.982954607100363,0.119020943550922)) ;
#22449 = DIRECTION('ref_axis',(-0.647386285943796,2.8514919837155E-10,-0.762162054140651)) ;
#22450 = DIRECTION('center_axis',(-0.162432290643921,-0.982954607100363,0.0861161502642798)) ;
#22451 = DIRECTION('ref_axis',(0.468408900302222,-9.72963020982897E-8,0.883511800780077)) ;
#22452 = DIRECTION('center_axis',(0.162432290643921,0.982954607100363,-0.0861161502642798)) ;
#22453 = DIRECTION('ref_axis',(-0.868452234516879,0.183848416855221,0.460424234790555)) ;
#22454 = DIRECTION('center_axis',(0.162432290643921,0.982954607100363,-0.0861161502642798)) ;
#22455 = DIRECTION('ref_axis',(-0.868452234516879,0.183848416855221,0.460424234790555)) ;
#22456 = DIRECTION('center_axis',(-0.16243229064392,-0.982954607100363,0.0861161502642797)) ;
#22457 = DIRECTION('ref_axis',(0.868452234516879,-0.18384841685522,-0.460424234790555)) ;
#22458 = DIRECTION('center_axis',(0.162432290643921,0.982954607100363,-0.0861161502642798)) ;
#22459 = DIRECTION('ref_axis',(-0.868452234516879,0.183848416855221,0.460424234790555)) ;
#22460 = DIRECTION('center_axis',(0.162432290643921,0.982954607100363,-0.0861161502642798)) ;
#22461 = DIRECTION('ref_axis',(-0.868452234516879,0.183848416855221,0.460424234790555)) ;
#22462 = DIRECTION('center_axis',(-0.162432290643921,-0.982954607100363,0.0861161502642798)) ;
#22463 = DIRECTION('ref_axis',(-0.868452234516879,0.183848416855221,0.460424234790555)) ;
#22464 = DIRECTION('center_axis',(-0.17714714068552,-0.982954607100363,0.0491846615025047)) ;
#22465 = DIRECTION('ref_axis',(0.267536309373971,-1.54723772605301E-6,0.963547779388319)) ;
#22466 = DIRECTION('center_axis',(0.17714714068552,0.982954607100363,-0.0491846615025047)) ;
#22467 = DIRECTION('ref_axis',(-0.94712590431829,0.183848416855222,0.262968212887203)) ;
#22468 = DIRECTION('center_axis',(0.17714714068552,0.982954607100363,-0.0491846615025047)) ;
#22469 = DIRECTION('ref_axis',(-0.94712590431829,0.183848416855222,0.262968212887203)) ;
#22470 = DIRECTION('center_axis',(-0.17714714068552,-0.982954607100363,0.0491846615025046)) ;
#22471 = DIRECTION('ref_axis',(0.94712590431829,-0.183848416855222,-0.262968212887203)) ;
#22472 = DIRECTION('center_axis',(0.17714714068552,0.982954607100363,-0.0491846615025047)) ;
#22473 = DIRECTION('ref_axis',(-0.94712590431829,0.183848416855222,0.262968212887203)) ;
#22474 = DIRECTION('center_axis',(0.17714714068552,0.982954607100363,-0.0491846615025047)) ;
#22475 = DIRECTION('ref_axis',(-0.94712590431829,0.183848416855222,0.262968212887203)) ;
#22476 = DIRECTION('center_axis',(-0.17714714068552,-0.982954607100363,0.0491846615025047)) ;
#22477 = DIRECTION('ref_axis',(-0.94712590431829,0.183848416855222,0.262968212887203)) ;
#22478 = DIRECTION('center_axis',(-0.183578787313568,-0.982954607100363,0.00995335263369857)) ;
#22479 = DIRECTION('ref_axis',(0.0541389096098241,-1.91882817342339E-10,0.998533413795582)) ;
#22480 = DIRECTION('center_axis',(0.183578787313568,0.982954607100363,-0.00995335263369857)) ;
#22481 = DIRECTION('ref_axis',(-0.981513019488616,0.183848416855221,0.0532160896174226)) ;
#22482 = DIRECTION('center_axis',(0.183578787313568,0.982954607100363,-0.00995335263369857)) ;
#22483 = DIRECTION('ref_axis',(-0.981513019488616,0.183848416855221,0.0532160896174226)) ;
#22484 = DIRECTION('center_axis',(-0.183578787313568,-0.982954607100363,0.00995335263369856)) ;
#22485 = DIRECTION('ref_axis',(0.981513019488616,-0.183848416855221,-0.0532160896174226)) ;
#22486 = DIRECTION('center_axis',(0.183578787313568,0.982954607100363,-0.00995335263369857)) ;
#22487 = DIRECTION('ref_axis',(-0.981513019488616,0.183848416855221,0.0532160896174226)) ;
#22488 = DIRECTION('center_axis',(0.183578787313568,0.982954607100363,-0.00995335263369857)) ;
#22489 = DIRECTION('ref_axis',(-0.981513019488616,0.183848416855221,0.0532160896174226)) ;
#22490 = DIRECTION('center_axis',(-0.183578787313568,-0.982954607100363,0.00995335263369857)) ;
#22491 = DIRECTION('ref_axis',(-0.981513019488616,0.183848416855221,0.0532160896174226)) ;
#22492 = DIRECTION('center_axis',(-0.181426493880004,-0.982954607100363,-0.0297433639419023)) ;
#22493 = DIRECTION('ref_axis',(-0.161781995558069,-1.88527458823811E-10,0.986826522704598)) ;
#22494 = DIRECTION('center_axis',(0.181426493880004,0.982954607100363,0.0297433639419023)) ;
#22495 = DIRECTION('ref_axis',(-0.970005676741023,0.183848416855222,-0.159024358857435)) ;
#22496 = DIRECTION('center_axis',(0.181426493880004,0.982954607100363,0.0297433639419023)) ;
#22497 = DIRECTION('ref_axis',(-0.970005676741023,0.183848416855222,-0.159024358857435)) ;
#22498 = DIRECTION('center_axis',(-0.181426493880003,-0.982954607100363,-0.0297433639419022)) ;
#22499 = DIRECTION('ref_axis',(0.970005676741023,-0.183848416855221,0.159024358857435)) ;
#22500 = DIRECTION('center_axis',(0.181426493880004,0.982954607100363,0.0297433639419023)) ;
#22501 = DIRECTION('ref_axis',(-0.970005676741023,0.183848416855222,-0.159024358857435)) ;
#22502 = DIRECTION('center_axis',(0.181426493880004,0.982954607100363,0.0297433639419023)) ;
#22503 = DIRECTION('ref_axis',(-0.970005676741023,0.183848416855222,-0.159024358857435)) ;
#22504 = DIRECTION('center_axis',(-0.181426493880004,-0.982954607100363,-0.0297433639419023)) ;
#22505 = DIRECTION('ref_axis',(0.161781994932387,3.07115069039933E-10,-0.986826522807174)) ;
#22506 = DIRECTION('center_axis',(-0.170790899233673,-0.982954607100363,-0.0680493138769549)) ;
#22507 = DIRECTION('ref_axis',(-0.370138154397863,-1.89668830078089E-10,0.928976720192139)) ;
#22508 = DIRECTION('center_axis',(0.170790899233673,0.982954607100363,0.0680493138769549)) ;
#22509 = DIRECTION('ref_axis',(-0.913141946632898,0.183848416855221,-0.363829005055)) ;
#22510 = DIRECTION('center_axis',(0.170790899233673,0.982954607100363,0.0680493138769549)) ;
#22511 = DIRECTION('ref_axis',(-0.913141946632898,0.183848416855221,-0.363829005055)) ;
#22512 = DIRECTION('center_axis',(-0.170790899233673,-0.982954607100363,-0.0680493138769549)) ;
#22513 = DIRECTION('ref_axis',(0.913141946632898,-0.183848416855221,0.363829005055)) ;
#22514 = DIRECTION('center_axis',(0.170790899233673,0.982954607100363,0.0680493138769549)) ;
#22515 = DIRECTION('ref_axis',(-0.913141946632898,0.183848416855221,-0.363829005055)) ;
#22516 = DIRECTION('center_axis',(0.170790899233673,0.982954607100363,0.0680493138769549)) ;
#22517 = DIRECTION('ref_axis',(-0.913141946632898,0.183848416855221,-0.363829005055)) ;
#22518 = DIRECTION('center_axis',(-0.170790899233673,-0.982954607100363,-0.0680493138769549)) ;
#22519 = DIRECTION('ref_axis',(-0.913141946632898,0.183848416855221,-0.363829005055)) ;
#22520 = DIRECTION('center_axis',(-0.152169311959629,-0.982954607100363,-0.103173353526501)) ;
#22521 = DIRECTION('ref_axis',(-0.561187064344022,-2.30122606296928E-10,0.827688998847356)) ;
#22522 = DIRECTION('center_axis',(0.152169311959629,0.982954607100363,0.103173353526501)) ;
#22523 = DIRECTION('ref_axis',(-0.8135807139846,0.183848416855221,-0.551621411343086)) ;
#22524 = DIRECTION('center_axis',(0.152169311959629,0.982954607100363,0.103173353526501)) ;
#22525 = DIRECTION('ref_axis',(-0.8135807139846,0.183848416855221,-0.551621411343086)) ;
#22526 = DIRECTION('center_axis',(-0.152169311959628,-0.982954607100363,-0.1031733535265)) ;
#22527 = DIRECTION('ref_axis',(0.8135807139846,-0.18384841685522,0.551621411343086)) ;
#22528 = DIRECTION('center_axis',(0.152169311959629,0.982954607100363,0.103173353526501)) ;
#22529 = DIRECTION('ref_axis',(-0.8135807139846,0.183848416855221,-0.551621411343086)) ;
#22530 = DIRECTION('center_axis',(0.152169311959629,0.982954607100363,0.103173353526501)) ;
#22531 = DIRECTION('ref_axis',(-0.8135807139846,0.183848416855221,-0.551621411343086)) ;
#22532 = DIRECTION('center_axis',(-0.152169311959629,-0.982954607100363,-0.103173353526501)) ;
#22533 = DIRECTION('ref_axis',(-0.813580713984599,0.183848416855221,-0.551621411343086)) ;
#22534 = DIRECTION('center_axis',(-0.126432456782393,-0.982954607100363,-0.133473121834094)) ;
#22535 = DIRECTION('ref_axis',(-0.725995491248325,-1.83529846792861E-10,0.687699459565807)) ;
#22536 = DIRECTION('center_axis',(0.126432456782393,0.982954607100363,0.133473121834094)) ;
#22537 = DIRECTION('ref_axis',(-0.675977351380398,0.18384841685522,-0.713620613519937)) ;
#22538 = DIRECTION('center_axis',(0.126432456782393,0.982954607100363,0.133473121834094)) ;
#22539 = DIRECTION('ref_axis',(-0.675977351380398,0.18384841685522,-0.713620613519937)) ;
#22540 = DIRECTION('center_axis',(-0.126432456782393,-0.982954607100363,-0.133473121834093)) ;
#22541 = DIRECTION('ref_axis',(0.675977351380398,-0.183848416855219,0.713620613519937)) ;
#22542 = DIRECTION('center_axis',(0.126432456782393,0.982954607100363,0.133473121834094)) ;
#22543 = DIRECTION('ref_axis',(-0.675977351380398,0.18384841685522,-0.713620613519937)) ;
#22544 = DIRECTION('center_axis',(0.126432456782393,0.982954607100363,0.133473121834094)) ;
#22545 = DIRECTION('ref_axis',(-0.675977351380398,0.18384841685522,-0.713620613519937)) ;
#22546 = DIRECTION('center_axis',(-0.126432456782393,-0.982954607100363,-0.133473121834094)) ;
#22547 = DIRECTION('ref_axis',(-0.675977351380398,0.18384841685522,-0.713620613519937)) ;
#22548 = DIRECTION('center_axis',(-0.0947837604455977,-0.982954607100363,
-0.157531835309445)) ;
#22549 = DIRECTION('ref_axis',(-0.856857175641539,-1.90844127298985E-10,0.515553858051324)) ;
#22550 = DIRECTION('center_axis',(0.0947837604455977,0.982954607100363,0.157531835309445)) ;
#22551 = DIRECTION('ref_axis',(-0.506766039120516,0.18384841685522,-0.84225170894094)) ;
#22552 = DIRECTION('center_axis',(0.0947837604455977,0.982954607100363,0.157531835309445)) ;
#22553 = DIRECTION('ref_axis',(-0.506766039120516,0.18384841685522,-0.84225170894094)) ;
#22554 = DIRECTION('center_axis',(-0.0947837604455976,-0.982954607100363,
-0.157531835309445)) ;
#22555 = DIRECTION('ref_axis',(0.506766039120516,-0.18384841685522,0.84225170894094)) ;
#22556 = DIRECTION('center_axis',(0.0947837604455977,0.982954607100363,0.157531835309445)) ;
#22557 = DIRECTION('ref_axis',(-0.506766039120516,0.18384841685522,-0.84225170894094)) ;
#22558 = DIRECTION('center_axis',(0.0947837604455977,0.982954607100363,0.157531835309445)) ;
#22559 = DIRECTION('ref_axis',(-0.506766039120516,0.18384841685522,-0.84225170894094)) ;
#22560 = DIRECTION('center_axis',(-0.0947837604455977,-0.982954607100363,
-0.157531835309445)) ;
#22561 = DIRECTION('ref_axis',(-0.506766039120516,0.18384841685522,-0.84225170894094)) ;
#22562 = DIRECTION('center_axis',(-0.0587030808149489,-0.982954607100363,
-0.174224535249788)) ;
#22563 = DIRECTION('ref_axis',(-0.94765317085513,-1.91940387467248E-10,0.319301531108476)) ;
#22564 = DIRECTION('center_axis',(0.058703080814949,0.982954607100363,0.174224535249788)) ;
#22565 = DIRECTION('ref_axis',(-0.313858910101358,0.183848416855221,-0.931500050547404)) ;
#22566 = DIRECTION('center_axis',(0.058703080814949,0.982954607100363,0.174224535249788)) ;
#22567 = DIRECTION('ref_axis',(-0.313858910101358,0.183848416855221,-0.931500050547404)) ;
#22568 = DIRECTION('center_axis',(-0.0587030808149489,-0.982954607100363,
-0.174224535249788)) ;
#22569 = DIRECTION('ref_axis',(0.313858910101358,-0.183848416855221,0.931500050547404)) ;
#22570 = DIRECTION('center_axis',(0.058703080814949,0.982954607100363,0.174224535249788)) ;
#22571 = DIRECTION('ref_axis',(-0.313858910101358,0.183848416855221,-0.931500050547404)) ;
#22572 = DIRECTION('center_axis',(0.058703080814949,0.982954607100363,0.174224535249788)) ;
#22573 = DIRECTION('ref_axis',(-0.313858910101358,0.183848416855221,-0.931500050547404)) ;
#22574 = DIRECTION('center_axis',(-0.0587030808149489,-0.982954607100363,
-0.174224535249788)) ;
#22575 = DIRECTION('ref_axis',(-0.313858910101358,0.183848416855221,-0.931500050547404)) ;
#22576 = DIRECTION('center_axis',(-0.0198775103691822,-0.982954607100363,
-0.182770689558513)) ;
#22577 = DIRECTION('ref_axis',(-0.994137957045046,-1.89103119640252E-10,0.108119019429064)) ;
#22578 = DIRECTION('center_axis',(0.0198775103691822,0.982954607100363,0.182770689558513)) ;
#22579 = DIRECTION('ref_axis',(-0.106276087274983,0.183848416855221,-0.977192485078221)) ;
#22580 = DIRECTION('center_axis',(0.0198775103691822,0.982954607100363,0.182770689558513)) ;
#22581 = DIRECTION('ref_axis',(-0.106276087274983,0.183848416855221,-0.977192485078221)) ;
#22582 = DIRECTION('center_axis',(-0.0198775103691822,-0.982954607100363,
-0.182770689558513)) ;
#22583 = DIRECTION('ref_axis',(0.106276087274983,-0.183848416855221,0.977192485078221)) ;
#22584 = DIRECTION('center_axis',(0.0198775103691822,0.982954607100363,0.182770689558513)) ;
#22585 = DIRECTION('ref_axis',(-0.106276087274983,0.183848416855221,-0.977192485078221)) ;
#22586 = DIRECTION('center_axis',(0.0198775103691822,0.982954607100363,0.182770689558513)) ;
#22587 = DIRECTION('ref_axis',(-0.106276087274983,0.183848416855221,-0.977192485078221)) ;
#22588 = DIRECTION('center_axis',(-0.0198775103691822,-0.982954607100363,
-0.182770689558513)) ;
#22589 = DIRECTION('ref_axis',(-0.106276087274983,0.183848416855221,-0.977192485078221)) ;
#22590 = DIRECTION('center_axis',(0.0198775103691822,-0.982954607100363,-0.182770689558513)) ;
#22591 = DIRECTION('ref_axis',(-0.994137957268381,-1.97246615825675E-10,-0.108119017375535)) ;
#22592 = DIRECTION('center_axis',(-0.0198775103691822,0.982954607100363,0.182770689558513)) ;
#22593 = DIRECTION('ref_axis',(0.106276087274983,0.183848416855221,-0.977192485078221)) ;
#22594 = DIRECTION('center_axis',(-0.0198775103691822,0.982954607100363,0.182770689558513)) ;
#22595 = DIRECTION('ref_axis',(0.106276087274983,0.183848416855221,-0.977192485078221)) ;
#22596 = DIRECTION('center_axis',(0.0198775103691822,-0.982954607100363,-0.182770689558513)) ;
#22597 = DIRECTION('ref_axis',(-0.106276087274983,-0.183848416855221,0.977192485078221)) ;
#22598 = DIRECTION('center_axis',(-0.0198775103691822,0.982954607100363,0.182770689558513)) ;
#22599 = DIRECTION('ref_axis',(0.106276087274983,0.183848416855221,-0.977192485078221)) ;
#22600 = DIRECTION('center_axis',(-0.0198775103691822,0.982954607100363,0.182770689558513)) ;
#22601 = DIRECTION('ref_axis',(0.106276087274983,0.183848416855221,-0.977192485078221)) ;
#22602 = DIRECTION('center_axis',(0.0198775103691822,-0.982954607100363,-0.182770689558513)) ;
#22603 = DIRECTION('ref_axis',(0.106276087274983,0.183848416855221,-0.977192485078221)) ;
#22604 = DIRECTION('center_axis',(0.0587030808149489,-0.982954607100363,-0.174224535249788)) ;
#22605 = DIRECTION('ref_axis',(-0.947653171526354,-2.01240630102731E-10,-0.319301529116356)) ;
#22606 = DIRECTION('center_axis',(-0.058703080814949,0.982954607100363,0.174224535249788)) ;
#22607 = DIRECTION('ref_axis',(0.313858910101358,0.183848416855221,-0.931500050547404)) ;
#22608 = DIRECTION('center_axis',(-0.058703080814949,0.982954607100363,0.174224535249788)) ;
#22609 = DIRECTION('ref_axis',(0.313858910101358,0.183848416855221,-0.931500050547404)) ;
#22610 = DIRECTION('center_axis',(0.0587030808149489,-0.982954607100363,-0.174224535249788)) ;
#22611 = DIRECTION('ref_axis',(-0.313858910101358,-0.183848416855221,0.931500050547404)) ;
#22612 = DIRECTION('center_axis',(-0.058703080814949,0.982954607100363,0.174224535249788)) ;
#22613 = DIRECTION('ref_axis',(0.313858910101358,0.183848416855221,-0.931500050547404)) ;
#22614 = DIRECTION('center_axis',(-0.058703080814949,0.982954607100363,0.174224535249788)) ;
#22615 = DIRECTION('ref_axis',(0.313858910101358,0.183848416855221,-0.931500050547404)) ;
#22616 = DIRECTION('center_axis',(0.0587030808149489,-0.982954607100363,-0.174224535249788)) ;
#22617 = DIRECTION('ref_axis',(0.313858910101358,0.183848416855221,-0.931500050547404)) ;
#22618 = DIRECTION('center_axis',(0.0947837604455977,-0.982954607100363,-0.157531835309445)) ;
#22619 = DIRECTION('ref_axis',(-0.856857176687482,-1.88611019607742E-10,-0.515553856312953)) ;
#22620 = DIRECTION('center_axis',(-0.0947837604455977,0.982954607100363,0.157531835309445)) ;
#22621 = DIRECTION('ref_axis',(0.506766039120516,0.18384841685522,-0.842251708940939)) ;
#22622 = DIRECTION('center_axis',(-0.0947837604455977,0.982954607100363,0.157531835309445)) ;
#22623 = DIRECTION('ref_axis',(0.506766039120516,0.18384841685522,-0.842251708940939)) ;
#22624 = DIRECTION('center_axis',(0.0947837604455976,-0.982954607100363,-0.157531835309445)) ;
#22625 = DIRECTION('ref_axis',(-0.506766039120516,-0.18384841685522,0.84225170894094)) ;
#22626 = DIRECTION('center_axis',(-0.0947837604455977,0.982954607100363,0.157531835309445)) ;
#22627 = DIRECTION('ref_axis',(0.506766039120516,0.18384841685522,-0.842251708940939)) ;
#22628 = DIRECTION('center_axis',(-0.0947837604455977,0.982954607100363,0.157531835309445)) ;
#22629 = DIRECTION('ref_axis',(0.506766039120516,0.18384841685522,-0.842251708940939)) ;
#22630 = DIRECTION('center_axis',(0.0947837604455977,-0.982954607100363,-0.157531835309445)) ;
#22631 = DIRECTION('ref_axis',(0.506766039120516,0.18384841685522,-0.842251708940939)) ;
#22632 = DIRECTION('center_axis',(0.126432456782393,-0.982954607100363,-0.133473121834094)) ;
#22633 = DIRECTION('ref_axis',(-0.725995492549092,-1.70245240902753E-10,-0.687699458192604)) ;
#22634 = DIRECTION('center_axis',(-0.126432456782393,0.982954607100363,0.133473121834094)) ;
#22635 = DIRECTION('ref_axis',(0.6759773513804,0.18384841685522,-0.713620613519935)) ;
#22636 = DIRECTION('center_axis',(-0.126432456782393,0.982954607100363,0.133473121834094)) ;
#22637 = DIRECTION('ref_axis',(0.6759773513804,0.18384841685522,-0.713620613519935)) ;
#22638 = DIRECTION('center_axis',(0.126432456782393,-0.982954607100363,-0.133473121834093)) ;
#22639 = DIRECTION('ref_axis',(-0.6759773513804,-0.183848416855219,0.713620613519935)) ;
#22640 = DIRECTION('center_axis',(-0.126432456782393,0.982954607100363,0.133473121834094)) ;
#22641 = DIRECTION('ref_axis',(0.6759773513804,0.18384841685522,-0.713620613519935)) ;
#22642 = DIRECTION('center_axis',(-0.126432456782393,0.982954607100363,0.133473121834094)) ;
#22643 = DIRECTION('ref_axis',(0.6759773513804,0.18384841685522,-0.713620613519935)) ;
#22644 = DIRECTION('center_axis',(0.126432456782393,-0.982954607100363,-0.133473121834094)) ;
#22645 = DIRECTION('ref_axis',(0.725995492955948,2.80899485909582E-10,0.687699457763092)) ;
#22646 = DIRECTION('center_axis',(0.152169311959629,-0.982954607100363,-0.103173353526501)) ;
#22647 = DIRECTION('ref_axis',(-0.561187066188927,-1.86778640161647E-10,-0.82768899759648)) ;
#22648 = DIRECTION('center_axis',(-0.152169311959629,0.982954607100363,0.103173353526501)) ;
#22649 = DIRECTION('ref_axis',(0.813580713984599,0.183848416855221,-0.551621411343086)) ;
#22650 = DIRECTION('center_axis',(-0.152169311959629,0.982954607100363,0.103173353526501)) ;
#22651 = DIRECTION('ref_axis',(0.813580713984599,0.183848416855221,-0.551621411343086)) ;
#22652 = DIRECTION('center_axis',(0.152169311959628,-0.982954607100363,-0.1031733535265)) ;
#22653 = DIRECTION('ref_axis',(-0.813580713984599,-0.18384841685522,0.551621411343087)) ;
#22654 = DIRECTION('center_axis',(-0.152169311959629,0.982954607100363,0.103173353526501)) ;
#22655 = DIRECTION('ref_axis',(0.813580713984599,0.183848416855221,-0.551621411343086)) ;
#22656 = DIRECTION('center_axis',(-0.152169311959629,0.982954607100363,0.103173353526501)) ;
#22657 = DIRECTION('ref_axis',(0.813580713984599,0.183848416855221,-0.551621411343086)) ;
#22658 = DIRECTION('center_axis',(0.152169311959629,-0.982954607100363,-0.103173353526501)) ;
#22659 = DIRECTION('ref_axis',(0.561187066725594,3.0805171850785E-10,0.82768899723261)) ;
#22660 = DIRECTION('center_axis',(0.170790899233673,-0.982954607100363,-0.068049313876955)) ;
#22661 = DIRECTION('ref_axis',(-0.370138156273929,-1.88050831664856E-10,-0.928976719444646)) ;
#22662 = DIRECTION('center_axis',(-0.170790899233673,0.982954607100363,0.0680493138769549)) ;
#22663 = DIRECTION('ref_axis',(0.913141946632899,0.183848416855221,-0.363829005054997)) ;
#22664 = DIRECTION('center_axis',(-0.170790899233673,0.982954607100363,0.0680493138769549)) ;
#22665 = DIRECTION('ref_axis',(0.913141946632899,0.183848416855221,-0.363829005054997)) ;
#22666 = DIRECTION('center_axis',(0.170790899233673,-0.982954607100363,-0.0680493138769549)) ;
#22667 = DIRECTION('ref_axis',(-0.913141946632899,-0.183848416855221,0.363829005054997)) ;
#22668 = DIRECTION('center_axis',(-0.170790899233673,0.982954607100363,0.0680493138769549)) ;
#22669 = DIRECTION('ref_axis',(0.913141946632899,0.183848416855221,-0.363829005054997)) ;
#22670 = DIRECTION('center_axis',(-0.170790899233673,0.982954607100363,0.0680493138769549)) ;
#22671 = DIRECTION('ref_axis',(0.913141946632899,0.183848416855221,-0.363829005054997)) ;
#22672 = DIRECTION('center_axis',(0.170790899233673,-0.982954607100363,-0.068049313876955)) ;
#22673 = DIRECTION('ref_axis',(0.913141946632899,0.183848416855221,-0.363829005054997)) ;
#22674 = DIRECTION('center_axis',(0.181426493880004,-0.982954607100363,-0.0297433639419023)) ;
#22675 = DIRECTION('ref_axis',(-0.161781997642536,-2.06548540774157E-10,-0.986826522362867)) ;
#22676 = DIRECTION('center_axis',(-0.181426493880004,0.982954607100363,0.0297433639419023)) ;
#22677 = DIRECTION('ref_axis',(0.970005676741023,0.183848416855222,-0.159024358857436)) ;
#22678 = DIRECTION('center_axis',(-0.181426493880004,0.982954607100363,0.0297433639419023)) ;
#22679 = DIRECTION('ref_axis',(0.970005676741023,0.183848416855222,-0.159024358857436)) ;
#22680 = DIRECTION('center_axis',(0.181426493880003,-0.982954607100363,-0.0297433639419022)) ;
#22681 = DIRECTION('ref_axis',(-0.970005676741023,-0.183848416855221,0.159024358857436)) ;
#22682 = DIRECTION('center_axis',(-0.181426493880004,0.982954607100363,0.0297433639419023)) ;
#22683 = DIRECTION('ref_axis',(0.970005676741023,0.183848416855222,-0.159024358857436)) ;
#22684 = DIRECTION('center_axis',(-0.181426493880004,0.982954607100363,0.0297433639419023)) ;
#22685 = DIRECTION('ref_axis',(0.970005676741023,0.183848416855222,-0.159024358857436)) ;
#22686 = DIRECTION('center_axis',(0.181426493880004,-0.982954607100363,-0.0297433639419023)) ;
#22687 = DIRECTION('ref_axis',(0.970005676741023,0.183848416855222,-0.159024358857436)) ;
#22688 = DIRECTION('center_axis',(0.183578787313568,-0.982954607100363,0.0099533526336988)) ;
#22689 = DIRECTION('ref_axis',(0.0541389075565303,-1.92722421117335E-10,-0.998533413906909)) ;
#22690 = DIRECTION('center_axis',(-0.183578787313568,0.982954607100363,-0.00995335263369879)) ;
#22691 = DIRECTION('ref_axis',(0.981513019488616,0.183848416855221,0.0532160896174224)) ;
#22692 = DIRECTION('center_axis',(-0.183578787313568,0.982954607100363,-0.00995335263369879)) ;
#22693 = DIRECTION('ref_axis',(0.981513019488616,0.183848416855221,0.0532160896174224)) ;
#22694 = DIRECTION('center_axis',(0.183578787313568,-0.982954607100363,0.00995335263369878)) ;
#22695 = DIRECTION('ref_axis',(-0.981513019488616,-0.183848416855221,-0.0532160896174224)) ;
#22696 = DIRECTION('center_axis',(-0.183578787313568,0.982954607100363,-0.00995335263369879)) ;
#22697 = DIRECTION('ref_axis',(0.981513019488616,0.183848416855221,0.0532160896174224)) ;
#22698 = DIRECTION('center_axis',(-0.183578787313568,0.982954607100363,-0.00995335263369879)) ;
#22699 = DIRECTION('ref_axis',(0.981513019488616,0.183848416855221,0.0532160896174224)) ;
#22700 = DIRECTION('center_axis',(0.183578787313568,-0.982954607100363,0.0099533526336988)) ;
#22701 = DIRECTION('ref_axis',(0.981513019488616,0.183848416855221,0.0532160896174224)) ;
#22702 = DIRECTION('center_axis',(0.17714714068552,-0.982954607100363,0.0491846615025056)) ;
#22703 = DIRECTION('ref_axis',(0.267536928724841,1.66746140147225E-6,-0.963547607420463)) ;
#22704 = DIRECTION('center_axis',(-0.17714714068552,0.982954607100363,-0.0491846615025056)) ;
#22705 = DIRECTION('ref_axis',(0.94712590431829,0.183848416855222,0.262968212887203)) ;
#22706 = DIRECTION('center_axis',(-0.17714714068552,0.982954607100363,-0.0491846615025056)) ;
#22707 = DIRECTION('ref_axis',(0.94712590431829,0.183848416855222,0.262968212887203)) ;
#22708 = DIRECTION('center_axis',(0.17714714068552,-0.982954607100363,0.0491846615025055)) ;
#22709 = DIRECTION('ref_axis',(-0.94712590431829,-0.183848416855222,-0.262968212887203)) ;
#22710 = DIRECTION('center_axis',(-0.17714714068552,0.982954607100363,-0.0491846615025056)) ;
#22711 = DIRECTION('ref_axis',(0.94712590431829,0.183848416855222,0.262968212887203)) ;
#22712 = DIRECTION('center_axis',(-0.17714714068552,0.982954607100363,-0.0491846615025056)) ;
#22713 = DIRECTION('ref_axis',(0.94712590431829,0.183848416855222,0.262968212887203)) ;
#22714 = DIRECTION('center_axis',(0.17714714068552,-0.982954607100363,0.0491846615025056)) ;
#22715 = DIRECTION('ref_axis',(-0.267536930966008,-1.66789643976773E-6,0.963547606798184)) ;
#22716 = DIRECTION('center_axis',(0.16243229064392,-0.982954607100363,0.0861161502642798)) ;
#22717 = DIRECTION('ref_axis',(0.468408439795022,-1.91537394307718E-10,-0.8835120449257)) ;
#22718 = DIRECTION('center_axis',(-0.16243229064392,0.982954607100363,-0.0861161502642798)) ;
#22719 = DIRECTION('ref_axis',(0.868452234516879,0.18384841685522,0.460424234790556)) ;
#22720 = DIRECTION('center_axis',(-0.16243229064392,0.982954607100363,-0.0861161502642798)) ;
#22721 = DIRECTION('ref_axis',(0.868452234516879,0.18384841685522,0.460424234790556)) ;
#22722 = DIRECTION('center_axis',(0.16243229064392,-0.982954607100363,0.0861161502642797)) ;
#22723 = DIRECTION('ref_axis',(-0.868452234516879,-0.183848416855221,-0.460424234790556)) ;
#22724 = DIRECTION('center_axis',(-0.16243229064392,0.982954607100363,-0.0861161502642798)) ;
#22725 = DIRECTION('ref_axis',(0.868452234516879,0.18384841685522,0.460424234790556)) ;
#22726 = DIRECTION('center_axis',(-0.16243229064392,0.982954607100363,-0.0861161502642798)) ;
#22727 = DIRECTION('ref_axis',(0.868452234516879,0.18384841685522,0.460424234790556)) ;
#22728 = DIRECTION('center_axis',(0.16243229064392,-0.982954607100363,0.0861161502642798)) ;
#22729 = DIRECTION('ref_axis',(0.868452234516879,0.183848416855221,0.460424234790556)) ;
#22730 = DIRECTION('center_axis',(0.140122287222337,-0.982954607100363,0.119020943550922)) ;
#22731 = DIRECTION('ref_axis',(0.647386284015078,-1.88162500161902E-10,-0.762162055778919)) ;
#22732 = DIRECTION('center_axis',(-0.140122287222336,0.982954607100363,-0.119020943550922)) ;
#22733 = DIRECTION('ref_axis',(0.749170703444791,0.18384841685522,0.636351331199885)) ;
#22734 = DIRECTION('center_axis',(-0.140122287222336,0.982954607100363,-0.119020943550922)) ;
#22735 = DIRECTION('ref_axis',(0.749170703444791,0.18384841685522,0.636351331199885)) ;
#22736 = DIRECTION('center_axis',(0.140122287222336,-0.982954607100363,0.119020943550922)) ;
#22737 = DIRECTION('ref_axis',(-0.749170703444791,-0.18384841685522,-0.636351331199885)) ;
#22738 = DIRECTION('center_axis',(-0.140122287222336,0.982954607100363,-0.119020943550922)) ;
#22739 = DIRECTION('ref_axis',(0.749170703444791,0.18384841685522,0.636351331199885)) ;
#22740 = DIRECTION('center_axis',(-0.140122287222336,0.982954607100363,-0.119020943550922)) ;
#22741 = DIRECTION('ref_axis',(0.749170703444791,0.18384841685522,0.636351331199885)) ;
#22742 = DIRECTION('center_axis',(0.140122287222337,-0.982954607100363,0.119020943550922)) ;
#22743 = DIRECTION('ref_axis',(0.749170703444791,0.18384841685522,0.636351331199885)) ;
#22744 = DIRECTION('center_axis',(0.111260321384975,-0.982954607100363,0.146360449799403)) ;
#22745 = DIRECTION('ref_axis',(0.796093065116338,-1.82132464471827E-10,-0.605174215968984)) ;
#22746 = DIRECTION('center_axis',(-0.111260321384975,0.982954607100363,-0.146360449799403)) ;
#22747 = DIRECTION('ref_axis',(0.594858782923056,0.183848416855222,0.782523346616016)) ;
#22748 = DIRECTION('center_axis',(-0.111260321384975,0.982954607100363,-0.146360449799403)) ;
#22749 = DIRECTION('ref_axis',(0.594858782923056,0.183848416855222,0.782523346616016)) ;
#22750 = DIRECTION('center_axis',(0.111260321384975,-0.982954607100363,0.146360449799402)) ;
#22751 = DIRECTION('ref_axis',(-0.594858782923056,-0.183848416855221,-0.782523346616016)) ;
#22752 = DIRECTION('center_axis',(-0.111260321384975,0.982954607100363,-0.146360449799403)) ;
#22753 = DIRECTION('ref_axis',(0.594858782923056,0.183848416855222,0.782523346616016)) ;
#22754 = DIRECTION('center_axis',(-0.111260321384975,0.982954607100363,-0.146360449799403)) ;
#22755 = DIRECTION('ref_axis',(0.594858782923056,0.183848416855222,0.782523346616016)) ;
#22756 = DIRECTION('center_axis',(0.111260321384975,-0.982954607100363,0.146360449799403)) ;
#22757 = DIRECTION('ref_axis',(-0.796093064783972,2.84854260519924E-10,0.605174216406204)) ;
#22758 = DIRECTION('center_axis',(0.0771959465766159,-0.982954607100363,0.166856304083218)) ;
#22759 = DIRECTION('ref_axis',(0.907575419211193,-2.04798413077975E-10,-0.419889102554029)) ;
#22760 = DIRECTION('center_axis',(-0.0771959465766159,0.982954607100363,-0.166856304083218)) ;
#22761 = DIRECTION('ref_axis',(0.412731926849892,0.183848416855221,0.892105440056614)) ;
#22762 = DIRECTION('center_axis',(-0.0771959465766159,0.982954607100363,-0.166856304083218)) ;
#22763 = DIRECTION('ref_axis',(0.412731926849892,0.183848416855221,0.892105440056614)) ;
#22764 = DIRECTION('center_axis',(0.0771959465766158,-0.982954607100363,0.166856304083218)) ;
#22765 = DIRECTION('ref_axis',(-0.412731926849892,-0.183848416855221,-0.892105440056614)) ;
#22766 = DIRECTION('center_axis',(-0.0771959465766159,0.982954607100363,-0.166856304083218)) ;
#22767 = DIRECTION('ref_axis',(0.412731926849892,0.183848416855221,0.892105440056614)) ;
#22768 = DIRECTION('center_axis',(-0.0771959465766159,0.982954607100363,-0.166856304083218)) ;
#22769 = DIRECTION('ref_axis',(0.412731926849892,0.183848416855221,0.892105440056614)) ;
#22770 = DIRECTION('center_axis',(0.0771959465766159,-0.982954607100363,0.166856304083218)) ;
#22771 = DIRECTION('ref_axis',(0.412731926849892,0.183848416855221,0.892105440056614)) ;
#22772 = DIRECTION('center_axis',(0.0395219751034661,-0.982954607100363,0.179550143035567)) ;
#22773 = DIRECTION('ref_axis',(0.976622826934841,1.97614399321564E-6,-0.214960121664217)) ;
#22774 = DIRECTION('center_axis',(-0.0395219751034661,0.982954607100363,-0.179550143035566)) ;
#22775 = DIRECTION('ref_axis',(0.211306184595818,0.183848416855221,0.959973674624147)) ;
#22776 = DIRECTION('center_axis',(-0.0395219751034661,0.982954607100363,-0.179550143035566)) ;
#22777 = DIRECTION('ref_axis',(0.211306184595818,0.183848416855221,0.959973674624147)) ;
#22778 = DIRECTION('center_axis',(0.0395219751034661,-0.982954607100363,0.179550143035566)) ;
#22779 = DIRECTION('ref_axis',(-0.211306184595818,-0.183848416855221,-0.959973674624147)) ;
#22780 = DIRECTION('center_axis',(-0.0395219751034661,0.982954607100363,-0.179550143035566)) ;
#22781 = DIRECTION('ref_axis',(0.211306184595818,0.183848416855221,0.959973674624147)) ;
#22782 = DIRECTION('center_axis',(-0.0395219751034661,0.982954607100363,-0.179550143035566)) ;
#22783 = DIRECTION('ref_axis',(0.211306184595818,0.183848416855221,0.959973674624147)) ;
#22784 = DIRECTION('center_axis',(0.0395219751034661,-0.982954607100363,0.179550143035567)) ;
#22785 = DIRECTION('ref_axis',(-0.976622827558554,-1.97668668594579E-6,0.214960118830513)) ;
#22786 = DIRECTION('axis',(0.,0.,1.)) ;
#22787 = DIRECTION('refdir',(1.,0.,0.)) ;
#22788 = DIRECTION('center_axis',(0.,0.,1.)) ;
#22789 = DIRECTION('ref_axis',(1.,0.,0.)) ;
#22790 = DIRECTION('center_axis',(0.,0.,-1.)) ;
#22791 = DIRECTION('ref_axis',(1.,0.,0.)) ;
#22792 = DIRECTION('',(0.707106781186548,8.65956056235494E-17,-0.707106781186547)) ;
#22793 = DIRECTION('center_axis',(0.,0.,1.)) ;
#22794 = DIRECTION('ref_axis',(1.,0.,0.)) ;
#22795 = DIRECTION('center_axis',(0.,0.,1.)) ;
#22796 = DIRECTION('ref_axis',(1.,0.,0.)) ;
#22797 = DIRECTION('center_axis',(0.,0.,-1.)) ;
#22798 = DIRECTION('ref_axis',(1.,0.,0.)) ;
#22799 = DIRECTION('center_axis',(0.,0.,1.)) ;
#22800 = DIRECTION('ref_axis',(1.,0.,0.)) ;
#22801 = DIRECTION('center_axis',(0.,0.,1.)) ;
#22802 = DIRECTION('ref_axis',(1.,0.,0.)) ;
#22803 = DIRECTION('',(0.,0.,-1.)) ;
#22804 = DIRECTION('center_axis',(0.,0.,-1.)) ;
#22805 = DIRECTION('ref_axis',(1.,0.,0.)) ;
#22806 = DIRECTION('center_axis',(0.,0.,1.)) ;
#22807 = DIRECTION('ref_axis',(1.,0.,0.)) ;
#22808 = DIRECTION('',(-0.707106781186548,8.65956056235494E-17,-0.707106781186547)) ;
#22809 = DIRECTION('center_axis',(0.,0.,1.)) ;
#22810 = DIRECTION('ref_axis',(1.,0.,0.)) ;
#22811 = DIRECTION('',(0.,0.,1.)) ;
#22812 = DIRECTION('center_axis',(0.,0.,-1.)) ;
#22813 = DIRECTION('ref_axis',(1.,0.,0.)) ;
#22814 = DIRECTION('center_axis',(0.,0.,-1.)) ;
#22815 = DIRECTION('ref_axis',(1.,0.,0.)) ;
#22816 = DIRECTION('',(0.707106781186547,-8.65956056235493E-17,0.707106781186548)) ;
#22817 = DIRECTION('center_axis',(0.,0.,-1.)) ;
#22818 = DIRECTION('ref_axis',(1.,0.,0.)) ;
#22819 = DIRECTION('center_axis',(0.,0.,1.)) ;
#22820 = DIRECTION('ref_axis',(1.,0.,0.)) ;
#22821 = DIRECTION('center_axis',(0.,0.,1.)) ;
#22822 = DIRECTION('ref_axis',(1.,0.,0.)) ;
#22823 = DIRECTION('center_axis',(0.,0.,1.)) ;
#22824 = DIRECTION('ref_axis',(1.,0.,0.)) ;
#22825 = DIRECTION('',(-0.707106781186547,-8.65956056235493E-17,0.707106781186548)) ;
#22826 = DIRECTION('axis',(0.,0.,1.)) ;
#22827 = DIRECTION('refdir',(1.,0.,0.)) ;
#22828 = DIRECTION('center_axis',(0.,0.,1.)) ;
#22829 = DIRECTION('ref_axis',(-1.,0.,0.)) ;
#22830 = DIRECTION('center_axis',(0.,0.,1.)) ;
#22831 = DIRECTION('ref_axis',(-1.,0.,0.)) ;
#22832 = DIRECTION('',(0.,0.,1.)) ;
#22833 = DIRECTION('center_axis',(0.,0.,-1.)) ;
#22834 = DIRECTION('ref_axis',(-1.,0.,0.)) ;
#22835 = DIRECTION('center_axis',(0.,0.,1.)) ;
#22836 = DIRECTION('ref_axis',(-1.,0.,0.)) ;
#22837 = DIRECTION('center_axis',(0.,0.,1.)) ;
#22838 = DIRECTION('ref_axis',(-1.,0.,0.)) ;
#22839 = DIRECTION('',(0.,0.,1.)) ;
#22840 = DIRECTION('center_axis',(0.,0.,-1.)) ;
#22841 = DIRECTION('ref_axis',(-1.,0.,0.)) ;
#22842 = DIRECTION('center_axis',(0.,0.,1.)) ;
#22843 = DIRECTION('ref_axis',(-1.,0.,0.)) ;
#22844 = DIRECTION('center_axis',(0.,0.,1.)) ;
#22845 = DIRECTION('ref_axis',(-1.,0.,0.)) ;
#22846 = DIRECTION('',(0.,0.,1.)) ;
#22847 = DIRECTION('center_axis',(0.,0.,-1.)) ;
#22848 = DIRECTION('ref_axis',(-1.,0.,0.)) ;
#22849 = DIRECTION('center_axis',(0.,0.,1.)) ;
#22850 = DIRECTION('ref_axis',(-1.,0.,0.)) ;
#22851 = DIRECTION('center_axis',(0.,0.,1.)) ;
#22852 = DIRECTION('ref_axis',(-1.,0.,0.)) ;
#22853 = DIRECTION('',(0.,0.,1.)) ;
#22854 = DIRECTION('center_axis',(0.,0.,-1.)) ;
#22855 = DIRECTION('ref_axis',(-1.,0.,0.)) ;
#22856 = DIRECTION('center_axis',(0.,0.,1.)) ;
#22857 = DIRECTION('ref_axis',(-1.,0.,0.)) ;
#22858 = DIRECTION('center_axis',(0.,0.,1.)) ;
#22859 = DIRECTION('ref_axis',(-1.,0.,0.)) ;
#22860 = DIRECTION('',(0.,0.,1.)) ;
#22861 = DIRECTION('center_axis',(0.,0.,-1.)) ;
#22862 = DIRECTION('ref_axis',(-1.,0.,0.)) ;
#22863 = DIRECTION('center_axis',(0.,0.,1.)) ;
#22864 = DIRECTION('ref_axis',(-1.,0.,0.)) ;
#22865 = DIRECTION('center_axis',(0.,0.,1.)) ;
#22866 = DIRECTION('ref_axis',(-1.,0.,0.)) ;
#22867 = DIRECTION('',(0.,0.,1.)) ;
#22868 = DIRECTION('center_axis',(0.,0.,-1.)) ;
#22869 = DIRECTION('ref_axis',(-1.,0.,0.)) ;
#22870 = DIRECTION('center_axis',(0.,0.,1.)) ;
#22871 = DIRECTION('ref_axis',(-1.,0.,0.)) ;
#22872 = DIRECTION('center_axis',(0.,0.,1.)) ;
#22873 = DIRECTION('ref_axis',(-1.,0.,0.)) ;
#22874 = DIRECTION('',(0.,0.,1.)) ;
#22875 = DIRECTION('center_axis',(0.,0.,-1.)) ;
#22876 = DIRECTION('ref_axis',(-1.,0.,0.)) ;
#22877 = DIRECTION('center_axis',(0.,0.,1.)) ;
#22878 = DIRECTION('ref_axis',(-1.,0.,0.)) ;
#22879 = DIRECTION('center_axis',(0.,0.,1.)) ;
#22880 = DIRECTION('ref_axis',(-1.,0.,0.)) ;
#22881 = DIRECTION('',(0.,0.,1.)) ;
#22882 = DIRECTION('center_axis',(0.,0.,-1.)) ;
#22883 = DIRECTION('ref_axis',(-1.,0.,0.)) ;
#22884 = DIRECTION('center_axis',(0.,0.,-1.)) ;
#22885 = DIRECTION('ref_axis',(1.,0.,0.)) ;
#22886 = DIRECTION('center_axis',(0.,0.,-1.)) ;
#22887 = DIRECTION('ref_axis',(1.,0.,0.)) ;
#22888 = DIRECTION('',(0.,0.,-1.)) ;
#22889 = DIRECTION('center_axis',(0.,0.,1.)) ;
#22890 = DIRECTION('ref_axis',(1.,0.,0.)) ;
#22891 = DIRECTION('center_axis',(0.,0.,-1.)) ;
#22892 = DIRECTION('ref_axis',(1.,0.,0.)) ;
#22893 = DIRECTION('center_axis',(0.,0.,-1.)) ;
#22894 = DIRECTION('ref_axis',(1.,0.,0.)) ;
#22895 = DIRECTION('',(0.,0.,1.)) ;
#22896 = DIRECTION('center_axis',(0.,0.,1.)) ;
#22897 = DIRECTION('ref_axis',(1.,0.,0.)) ;
#22898 = DIRECTION('center_axis',(0.,0.,-1.)) ;
#22899 = DIRECTION('ref_axis',(-1.,0.,0.)) ;
#22900 = DIRECTION('center_axis',(0.,0.,-1.)) ;
#22901 = DIRECTION('ref_axis',(-1.,0.,0.)) ;
#22902 = DIRECTION('axis',(0.,0.,1.)) ;
#22903 = DIRECTION('refdir',(1.,0.,0.)) ;
#22904 = DIRECTION('center_axis',(2.46519032881566E-32,-1.97215226305253E-31,
1.)) ;
#22905 = DIRECTION('ref_axis',(-1.,1.15088063745374E-32,2.46519032881566E-32)) ;
#22906 = DIRECTION('center_axis',(-2.46519032881566E-32,1.97215226305253E-31,
-1.)) ;
#22907 = DIRECTION('ref_axis',(-1.,1.15088063745374E-32,2.46519032881566E-32)) ;
#22908 = DIRECTION('',(2.46519032881566E-32,-1.97215226305253E-31,1.)) ;
#22909 = DIRECTION('center_axis',(2.46519032881566E-32,-1.97215226305253E-31,
1.)) ;
#22910 = DIRECTION('ref_axis',(-1.,1.15088063745374E-32,2.46519032881566E-32)) ;
#22911 = DIRECTION('center_axis',(2.46519032881566E-32,-1.97215226305253E-31,
1.)) ;
#22912 = DIRECTION('ref_axis',(-1.,1.15088063745374E-32,2.46519032881566E-32)) ;
#22913 = DIRECTION('center_axis',(-2.46519032881566E-32,1.97215226305253E-31,
-1.)) ;
#22914 = DIRECTION('ref_axis',(-1.,1.15088063745374E-32,2.46519032881566E-32)) ;
#22915 = DIRECTION('',(2.46519032881566E-32,-1.97215226305253E-31,1.)) ;
#22916 = DIRECTION('center_axis',(2.46519032881566E-32,-1.97215226305253E-31,
1.)) ;
#22917 = DIRECTION('ref_axis',(-1.,1.15088063745374E-32,2.46519032881566E-32)) ;
#22918 = DIRECTION('center_axis',(2.46519032881566E-32,-1.97215226305253E-31,
1.)) ;
#22919 = DIRECTION('ref_axis',(-1.,1.15088063745374E-32,2.46519032881566E-32)) ;
#22920 = DIRECTION('center_axis',(-2.46519032881566E-32,1.97215226305253E-31,
-1.)) ;
#22921 = DIRECTION('ref_axis',(-1.,1.15088063745374E-32,2.46519032881566E-32)) ;
#22922 = DIRECTION('',(2.46519032881566E-32,-1.97215226305253E-31,1.)) ;
#22923 = DIRECTION('center_axis',(2.46519032881566E-32,-1.97215226305253E-31,
1.)) ;
#22924 = DIRECTION('ref_axis',(-1.,1.15088063745374E-32,2.46519032881566E-32)) ;
#22925 = DIRECTION('center_axis',(2.46519032881566E-32,-1.97215226305253E-31,
1.)) ;
#22926 = DIRECTION('ref_axis',(-1.,1.15088063745374E-32,2.46519032881566E-32)) ;
#22927 = DIRECTION('center_axis',(-2.46519032881566E-32,1.97215226305253E-31,
-1.)) ;
#22928 = DIRECTION('ref_axis',(-1.,1.15088063745374E-32,2.46519032881566E-32)) ;
#22929 = DIRECTION('',(2.46519032881566E-32,-1.97215226305253E-31,1.)) ;
#22930 = DIRECTION('center_axis',(2.46519032881566E-32,-1.97215226305253E-31,
1.)) ;
#22931 = DIRECTION('ref_axis',(-1.,1.15088063745374E-32,2.46519032881566E-32)) ;
#22932 = DIRECTION('center_axis',(2.46519032881566E-32,-1.97215226305253E-31,
1.)) ;
#22933 = DIRECTION('ref_axis',(-1.,1.15088063745374E-32,2.46519032881566E-32)) ;
#22934 = DIRECTION('center_axis',(-2.46519032881566E-32,1.97215226305253E-31,
-1.)) ;
#22935 = DIRECTION('ref_axis',(-1.,1.15088063745374E-32,2.46519032881566E-32)) ;
#22936 = DIRECTION('',(2.46519032881566E-32,-1.97215226305253E-31,1.)) ;
#22937 = DIRECTION('center_axis',(2.46519032881566E-32,-1.97215226305253E-31,
1.)) ;
#22938 = DIRECTION('ref_axis',(-1.,1.15088063745374E-32,2.46519032881566E-32)) ;
#22939 = DIRECTION('center_axis',(2.46519032881566E-32,-1.97215226305253E-31,
1.)) ;
#22940 = DIRECTION('ref_axis',(-1.,1.15088063745374E-32,2.46519032881566E-32)) ;
#22941 = DIRECTION('center_axis',(-2.46519032881566E-32,1.97215226305253E-31,
-1.)) ;
#22942 = DIRECTION('ref_axis',(-1.,1.15088063745374E-32,2.46519032881566E-32)) ;
#22943 = DIRECTION('',(2.46519032881566E-32,-1.97215226305253E-31,1.)) ;
#22944 = DIRECTION('center_axis',(2.46519032881566E-32,-1.97215226305253E-31,
1.)) ;
#22945 = DIRECTION('ref_axis',(-1.,1.15088063745374E-32,2.46519032881566E-32)) ;
#22946 = DIRECTION('center_axis',(2.46519032881566E-32,-1.97215226305253E-31,
1.)) ;
#22947 = DIRECTION('ref_axis',(-1.,1.15088063745374E-32,2.46519032881566E-32)) ;
#22948 = DIRECTION('center_axis',(-2.46519032881566E-32,1.97215226305253E-31,
-1.)) ;
#22949 = DIRECTION('ref_axis',(-1.,1.15088063745374E-32,2.46519032881566E-32)) ;
#22950 = DIRECTION('',(2.46519032881566E-32,-1.97215226305253E-31,1.)) ;
#22951 = DIRECTION('center_axis',(2.46519032881566E-32,-1.97215226305253E-31,
1.)) ;
#22952 = DIRECTION('ref_axis',(-1.,1.15088063745374E-32,2.46519032881566E-32)) ;
#22953 = DIRECTION('center_axis',(2.46519032881566E-32,-1.97215226305253E-31,
1.)) ;
#22954 = DIRECTION('ref_axis',(-1.,1.15088063745374E-32,2.46519032881566E-32)) ;
#22955 = DIRECTION('center_axis',(-2.46519032881566E-32,1.97215226305253E-31,
-1.)) ;
#22956 = DIRECTION('ref_axis',(-1.,1.15088063745374E-32,2.46519032881566E-32)) ;
#22957 = DIRECTION('',(2.46519032881566E-32,-1.97215226305253E-31,1.)) ;
#22958 = DIRECTION('center_axis',(2.46519032881566E-32,-1.97215226305253E-31,
1.)) ;
#22959 = DIRECTION('ref_axis',(-1.,1.15088063745374E-32,2.46519032881566E-32)) ;
#22960 = DIRECTION('center_axis',(-2.46519032881566E-32,1.97215226305253E-31,
-1.)) ;
#22961 = DIRECTION('ref_axis',(1.,-1.15088063745374E-32,-2.46519032881566E-32)) ;
#22962 = DIRECTION('center_axis',(2.46519032881566E-32,-1.97215226305253E-31,
1.)) ;
#22963 = DIRECTION('ref_axis',(1.,-1.15088063745374E-32,-2.46519032881566E-32)) ;
#22964 = DIRECTION('',(-2.46519032881566E-32,1.97215226305253E-31,-1.)) ;
#22965 = DIRECTION('center_axis',(-2.46519032881566E-32,1.97215226305253E-31,
-1.)) ;
#22966 = DIRECTION('ref_axis',(1.,-1.15088063745374E-32,-2.46519032881566E-32)) ;
#22967 = DIRECTION('center_axis',(-2.46519032881566E-32,1.97215226305253E-31,
-1.)) ;
#22968 = DIRECTION('ref_axis',(1.,-1.15088063745374E-32,-2.46519032881566E-32)) ;
#22969 = DIRECTION('center_axis',(2.46519032881566E-32,-1.97215226305253E-31,
1.)) ;
#22970 = DIRECTION('ref_axis',(1.,-1.15088063745374E-32,-2.46519032881566E-32)) ;
#22971 = DIRECTION('',(2.46519032881566E-32,-1.97215226305253E-31,1.)) ;
#22972 = DIRECTION('center_axis',(-2.46519032881566E-32,1.97215226305253E-31,
-1.)) ;
#22973 = DIRECTION('ref_axis',(1.,-1.15088063745374E-32,-2.46519032881566E-32)) ;
#22974 = DIRECTION('center_axis',(-2.46519032881566E-32,1.97215226305253E-31,
-1.)) ;
#22975 = DIRECTION('ref_axis',(-1.,1.15088063745374E-32,2.46519032881566E-32)) ;
#22976 = DIRECTION('center_axis',(-2.46519032881566E-32,1.97215226305253E-31,
-1.)) ;
#22977 = DIRECTION('ref_axis',(-1.,1.15088063745374E-32,2.46519032881566E-32)) ;
#22978 = DIRECTION('',(0.,0.,1.)) ;
#22979 = DIRECTION('',(1.,0.,0.)) ;
#22980 = DIRECTION('',(0.,0.,1.)) ;
#22981 = DIRECTION('',(1.,0.,0.)) ;
#22982 = DIRECTION('',(0.,0.,1.)) ;
#22983 = DIRECTION('',(1.,0.,0.)) ;
#22984 = DIRECTION('',(1.59141291454589E-32,-1.,0.)) ;
#22985 = DIRECTION('',(1.,1.59141291454589E-32,3.08148791101958E-33)) ;
#22986 = DIRECTION('',(2.46519032881566E-32,-1.97215226305253E-31,1.)) ;
#22987 = DIRECTION('',(1.,-1.15088063745374E-32,-2.46519032881566E-32)) ;
#22988 = DIRECTION('',(-2.46519032881566E-32,1.97215226305253E-31,-1.)) ;
#22989 = DIRECTION('',(-1.,1.15088063745374E-32,2.46519032881566E-32)) ;
#22990 = DIRECTION('',(-2.46519032881566E-32,1.97215226305253E-31,-1.)) ;
#22991 = DIRECTION('',(-1.,1.22464679914735E-16,2.46519032881566E-32)) ;
#22992 = DIRECTION('',(-2.46519032881566E-32,1.97215226305253E-31,-1.)) ;
#22993 = DIRECTION('',(1.,-1.15088063745374E-32,-2.46519032881566E-32)) ;
#22994 = DIRECTION('',(-1.22464679914735E-16,-1.,6.292741183835E-49)) ;
#22995 = DIRECTION('',(-6.12323399573675E-17,7.49879891330925E-33,1.)) ;
#22996 = DIRECTION('',(-2.46519032881566E-32,1.97215226305253E-31,-1.)) ;
#22997 = DIRECTION('',(1.,-1.15088063745374E-32,-2.46519032881566E-32)) ;
#22998 = DIRECTION('',(1.,-1.15088063745374E-32,3.08148791101958E-33)) ;
#22999 = DIRECTION('',(3.08148791101958E-33,1.97215226305253E-31,-1.)) ;
#23000 = DIRECTION('',(1.,-1.15088063745374E-32,3.08148791101958E-33)) ;
#23001 = DIRECTION('',(-3.08148791101958E-33,-1.97215226305253E-31,1.)) ;
#23002 = DIRECTION('',(2.46519032881566E-32,-1.97215226305253E-31,1.)) ;
#23003 = DIRECTION('',(1.,-2.33486982377251E-16,-2.46519032881566E-32)) ;
#23004 = DIRECTION('',(-1.59141291454589E-32,1.,0.)) ;
#23005 = DIRECTION('',(1.,1.59141291454589E-32,3.08148791101958E-33)) ;
#23006 = DIRECTION('',(-2.46519032881566E-32,1.97215226305253E-31,-1.)) ;
#23007 = DIRECTION('',(1.,-1.15088063745374E-32,-2.46519032881566E-32)) ;
#23008 = DIRECTION('',(0.,0.,1.)) ;
#23009 = DIRECTION('',(1.,0.,0.)) ;
#23010 = DIRECTION('',(0.,0.,1.)) ;
#23011 = DIRECTION('',(1.,0.,0.)) ;
#23012 = CARTESIAN_POINT('',(0.,0.,0.)) ;
#23013 = CARTESIAN_POINT('',(0.,0.,0.)) ;
#23014 = CARTESIAN_POINT('Origin',(-45.0000000000005,385.343736383858,-12.)) ;
#23015 = CARTESIAN_POINT('',(-45.0000000000005,383.888531181086,-12.)) ;
#23016 = CARTESIAN_POINT('',(-45.0000000000005,386.45,-16.263)) ;
#23017 = CARTESIAN_POINT('',(-45.0000000000005,385.343736383858,-14.4218681615831)) ;
#23018 = CARTESIAN_POINT('Origin',(-45.0000000000005,386.45,-12.)) ;
#23019 = CARTESIAN_POINT('Origin',(-45.0000000000005,405.45,-12.)) ;
#23020 = CARTESIAN_POINT('',(-45.0000000000005,409.45,-16.263)) ;
#23021 = CARTESIAN_POINT('Origin',(-45.0000000000005,409.45,-12.)) ;
#23022 = CARTESIAN_POINT('',(-45.0000000000005,405.45,-16.263)) ;
#23023 = CARTESIAN_POINT('Origin',(44.9999999999989,385.343736383858,-12.)) ;
#23024 = CARTESIAN_POINT('',(44.9999999999989,383.888531181086,-12.)) ;
#23025 = CARTESIAN_POINT('',(44.9999999999989,386.45,-16.263)) ;
#23026 = CARTESIAN_POINT('',(44.9999999999989,385.343736383858,-14.4218681615831)) ;
#23027 = CARTESIAN_POINT('Origin',(44.9999999999989,386.45,-12.)) ;
#23028 = CARTESIAN_POINT('Origin',(44.9999999999989,405.45,-12.)) ;
#23029 = CARTESIAN_POINT('',(44.9999999999989,409.45,-16.263)) ;
#23030 = CARTESIAN_POINT('Origin',(44.9999999999989,409.45,-12.)) ;
#23031 = CARTESIAN_POINT('',(44.9999999999989,405.45,-16.263)) ;
#23032 = CARTESIAN_POINT('Origin',(-44.9999999999999,228.556263616143,-12.)) ;
#23033 = CARTESIAN_POINT('',(-44.9999999999999,230.011468818915,-12.)) ;
#23034 = CARTESIAN_POINT('',(-44.9999999999999,227.45,-7.737)) ;
#23035 = CARTESIAN_POINT('',(-44.9999999999999,228.556263616143,-9.57813183841693)) ;
#23036 = CARTESIAN_POINT('Origin',(-44.9999999999999,227.45,-12.)) ;
#23037 = CARTESIAN_POINT('Origin',(-44.9999999999999,208.45,-12.)) ;
#23038 = CARTESIAN_POINT('',(-44.9999999999999,209.449999999999,-7.737)) ;
#23039 = CARTESIAN_POINT('Origin',(-44.9999999999999,209.449999999999,-12.)) ;
#23040 = CARTESIAN_POINT('',(-44.9999999999999,208.45,-7.737)) ;
#23041 = CARTESIAN_POINT('Origin',(44.9999999999995,228.556263616143,-12.)) ;
#23042 = CARTESIAN_POINT('',(44.9999999999995,230.011468818915,-12.)) ;
#23043 = CARTESIAN_POINT('',(44.9999999999995,227.45,-7.737)) ;
#23044 = CARTESIAN_POINT('',(44.9999999999995,228.556263616143,-9.57813183841693)) ;
#23045 = CARTESIAN_POINT('Origin',(44.9999999999995,227.45,-12.)) ;
#23046 = CARTESIAN_POINT('Origin',(44.9999999999995,208.45,-12.)) ;
#23047 = CARTESIAN_POINT('',(44.9999999999995,209.449999999999,-7.737)) ;
#23048 = CARTESIAN_POINT('Origin',(44.9999999999995,209.449999999999,-12.)) ;
#23049 = CARTESIAN_POINT('',(44.9999999999995,208.45,-7.737)) ;
#23050 = CARTESIAN_POINT('Origin',(-62.9999999999999,239.45,-10.)) ;
#23051 = CARTESIAN_POINT('',(-71.9999999999999,239.45,-10.)) ;
#23052 = CARTESIAN_POINT('Origin',(-62.9999999999999,239.45,-10.)) ;
#23053 = CARTESIAN_POINT('',(-68.4999999999999,239.45,-10.)) ;
#23054 = CARTESIAN_POINT('Origin',(-62.9999999999999,239.45,-10.)) ;
#23055 = CARTESIAN_POINT('Origin',(-62.9999999999999,239.45,-5.)) ;
#23056 = CARTESIAN_POINT('',(-71.9999999999999,239.45,0.)) ;
#23057 = CARTESIAN_POINT('Origin',(-62.9999999999999,239.45,0.)) ;
#23058 = CARTESIAN_POINT('',(-71.9999999999999,239.45,-5.)) ;
#23059 = CARTESIAN_POINT('Origin',(-62.9999999999999,239.45,-19.)) ;
#23060 = CARTESIAN_POINT('',(-68.4999999999999,239.45,-24.)) ;
#23061 = CARTESIAN_POINT('',(-68.4999999999999,239.45,-19.)) ;
#23062 = CARTESIAN_POINT('Origin',(-62.9999999999999,239.45,-24.)) ;
#23063 = CARTESIAN_POINT('Origin',(63.,379.45,-10.)) ;
#23064 = CARTESIAN_POINT('',(54.,379.45,-10.)) ;
#23065 = CARTESIAN_POINT('Origin',(63.,379.45,-10.)) ;
#23066 = CARTESIAN_POINT('',(57.5,379.45,-10.)) ;
#23067 = CARTESIAN_POINT('Origin',(63.,379.45,-10.)) ;
#23068 = CARTESIAN_POINT('Origin',(63.,379.45,-5.)) ;
#23069 = CARTESIAN_POINT('',(54.,379.45,0.)) ;
#23070 = CARTESIAN_POINT('Origin',(63.,379.45,0.)) ;
#23071 = CARTESIAN_POINT('',(54.,379.45,-5.)) ;
#23072 = CARTESIAN_POINT('Origin',(63.,379.45,-19.)) ;
#23073 = CARTESIAN_POINT('',(57.5,379.45,-24.)) ;
#23074 = CARTESIAN_POINT('',(57.5,379.45,-19.)) ;
#23075 = CARTESIAN_POINT('Origin',(63.,379.45,-24.)) ;
#23076 = CARTESIAN_POINT('Origin',(63.,239.45,-10.)) ;
#23077 = CARTESIAN_POINT('',(54.,239.45,-10.)) ;
#23078 = CARTESIAN_POINT('Origin',(63.,239.45,-10.)) ;
#23079 = CARTESIAN_POINT('',(57.5,239.45,-10.)) ;
#23080 = CARTESIAN_POINT('Origin',(63.,239.45,-10.)) ;
#23081 = CARTESIAN_POINT('Origin',(63.,239.45,-5.)) ;
#23082 = CARTESIAN_POINT('',(54.,239.45,0.)) ;
#23083 = CARTESIAN_POINT('Origin',(63.,239.45,0.)) ;
#23084 = CARTESIAN_POINT('',(54.,239.45,-5.)) ;
#23085 = CARTESIAN_POINT('Origin',(63.,239.45,-19.)) ;
#23086 = CARTESIAN_POINT('',(57.5,239.45,-24.)) ;
#23087 = CARTESIAN_POINT('',(57.5,239.45,-19.)) ;
#23088 = CARTESIAN_POINT('Origin',(63.,239.45,-24.)) ;
#23089 = CARTESIAN_POINT('Origin',(-62.9999999999999,379.45,-10.)) ;
#23090 = CARTESIAN_POINT('',(-71.9999999999999,379.45,-10.)) ;
#23091 = CARTESIAN_POINT('Origin',(-62.9999999999999,379.45,-10.)) ;
#23092 = CARTESIAN_POINT('',(-68.4999999999999,379.45,-10.)) ;
#23093 = CARTESIAN_POINT('Origin',(-62.9999999999999,379.45,-10.)) ;
#23094 = CARTESIAN_POINT('Origin',(-62.9999999999999,379.45,-5.)) ;
#23095 = CARTESIAN_POINT('',(-71.9999999999999,379.45,0.)) ;
#23096 = CARTESIAN_POINT('Origin',(-62.9999999999999,379.45,0.)) ;
#23097 = CARTESIAN_POINT('',(-71.9999999999999,379.45,-5.)) ;
#23098 = CARTESIAN_POINT('Origin',(-62.9999999999999,379.45,-19.)) ;
#23099 = CARTESIAN_POINT('',(-68.4999999999999,379.45,-24.)) ;
#23100 = CARTESIAN_POINT('',(-68.4999999999999,379.45,-19.)) ;
#23101 = CARTESIAN_POINT('Origin',(-62.9999999999999,379.45,-24.)) ;
#23102 = CARTESIAN_POINT('Origin',(45.,354.45,-13.0085799786045)) ;
#23103 = CARTESIAN_POINT('',(45.,354.45,-12.0171599572091)) ;
#23104 = CARTESIAN_POINT('',(48.3,354.45,-14.)) ;
#23105 = CARTESIAN_POINT('',(46.65,354.45,-13.0085799786045)) ;
#23106 = CARTESIAN_POINT('Origin',(45.,354.45,-14.)) ;
#23107 = CARTESIAN_POINT('Origin',(45.,354.45,-22.)) ;
#23108 = CARTESIAN_POINT('',(48.3,354.45,-24.)) ;
#23109 = CARTESIAN_POINT('Origin',(45.,354.45,-24.)) ;
#23110 = CARTESIAN_POINT('',(48.3,354.45,-22.)) ;
#23111 = CARTESIAN_POINT('Origin',(-5.51091059616309E-15,399.45,-13.3540332243106)) ;
#23112 = CARTESIAN_POINT('',(-5.67105257905314E-15,399.45,-12.4873333915981)) ;
#23113 = CARTESIAN_POINT('',(2.51749999999999,399.45,-14.)) ;
#23114 = CARTESIAN_POINT('',(1.44243074893997,399.45,-13.3540332243106)) ;
#23115 = CARTESIAN_POINT('Origin',(-5.51091059616309E-15,399.45,-14.)) ;
#23116 = CARTESIAN_POINT('Origin',(-5.51091059616309E-15,399.45,-22.)) ;
#23117 = CARTESIAN_POINT('',(2.51749999999999,399.45,-24.)) ;
#23118 = CARTESIAN_POINT('Origin',(-5.51091059616309E-15,399.45,-24.)) ;
#23119 = CARTESIAN_POINT('',(2.51749999999999,399.45,-22.)) ;
#23120 = CARTESIAN_POINT('Origin',(-45.,354.45,-13.3540332243106)) ;
#23121 = CARTESIAN_POINT('',(-45.,354.45,-12.4873333915981)) ;
#23122 = CARTESIAN_POINT('',(-42.4825,354.45,-14.)) ;
#23123 = CARTESIAN_POINT('',(-43.55756925106,354.45,-13.3540332243106)) ;
#23124 = CARTESIAN_POINT('Origin',(-45.,354.45,-14.)) ;
#23125 = CARTESIAN_POINT('Origin',(-45.,354.45,-22.)) ;
#23126 = CARTESIAN_POINT('',(-42.4825,354.45,-24.)) ;
#23127 = CARTESIAN_POINT('Origin',(-45.,354.45,-24.)) ;
#23128 = CARTESIAN_POINT('',(-42.4825,354.45,-22.)) ;
#23129 = CARTESIAN_POINT('Origin',(0.,309.45,-13.3540332243106)) ;
#23130 = CARTESIAN_POINT('',(-1.60141982890047E-16,309.45,-12.4873333915981)) ;
#23131 = CARTESIAN_POINT('',(2.5175,309.45,-14.)) ;
#23132 = CARTESIAN_POINT('',(1.44243074893998,309.45,-13.3540332243106)) ;
#23133 = CARTESIAN_POINT('Origin',(0.,309.45,-14.)) ;
#23134 = CARTESIAN_POINT('Origin',(0.,309.45,-22.)) ;
#23135 = CARTESIAN_POINT('',(2.5175,309.45,-24.)) ;
#23136 = CARTESIAN_POINT('Origin',(0.,309.45,-24.)) ;
#23137 = CARTESIAN_POINT('',(2.5175,309.45,-22.)) ;
#23138 = CARTESIAN_POINT('Origin',(-31.8198051533946,322.630194846605,-13.3540332243106)) ;
#23139 = CARTESIAN_POINT('',(-31.8198051533946,322.630194846605,-12.4873333915981)) ;
#23140 = CARTESIAN_POINT('',(-29.3023051533946,322.630194846605,-14.)) ;
#23141 = CARTESIAN_POINT('',(-30.3773744044546,322.630194846605,-13.3540332243106)) ;
#23142 = CARTESIAN_POINT('Origin',(-31.8198051533946,322.630194846605,-14.)) ;
#23143 = CARTESIAN_POINT('Origin',(-31.8198051533946,322.630194846605,-22.)) ;
#23144 = CARTESIAN_POINT('',(-29.3023051533946,322.630194846605,-24.)) ;
#23145 = CARTESIAN_POINT('Origin',(-31.8198051533946,322.630194846605,-24.)) ;
#23146 = CARTESIAN_POINT('',(-29.3023051533946,322.630194846605,-22.)) ;
#23147 = CARTESIAN_POINT('Origin',(-31.8198051533946,386.269805153395,-13.3540332243106)) ;
#23148 = CARTESIAN_POINT('',(-31.8198051533946,386.269805153395,-12.4873333915981)) ;
#23149 = CARTESIAN_POINT('',(-29.3023051533946,386.269805153395,-14.)) ;
#23150 = CARTESIAN_POINT('',(-30.3773744044546,386.269805153395,-13.3540332243106)) ;
#23151 = CARTESIAN_POINT('Origin',(-31.8198051533946,386.269805153395,-14.)) ;
#23152 = CARTESIAN_POINT('Origin',(-31.8198051533946,386.269805153395,-22.)) ;
#23153 = CARTESIAN_POINT('',(-29.3023051533946,386.269805153395,-24.)) ;
#23154 = CARTESIAN_POINT('Origin',(-31.8198051533946,386.269805153395,-24.)) ;
#23155 = CARTESIAN_POINT('',(-29.3023051533946,386.269805153395,-22.)) ;
#23156 = CARTESIAN_POINT('Origin',(31.8198051533946,386.269805153395,-13.3540332243106)) ;
#23157 = CARTESIAN_POINT('',(31.8198051533946,386.269805153395,-12.4873333915981)) ;
#23158 = CARTESIAN_POINT('',(34.3373051533946,386.269805153395,-14.)) ;
#23159 = CARTESIAN_POINT('',(33.2622359023346,386.269805153395,-13.3540332243106)) ;
#23160 = CARTESIAN_POINT('Origin',(31.8198051533946,386.269805153395,-14.)) ;
#23161 = CARTESIAN_POINT('Origin',(31.8198051533946,386.269805153395,-22.)) ;
#23162 = CARTESIAN_POINT('',(34.3373051533946,386.269805153395,-24.)) ;
#23163 = CARTESIAN_POINT('Origin',(31.8198051533946,386.269805153395,-24.)) ;
#23164 = CARTESIAN_POINT('',(34.3373051533946,386.269805153395,-22.)) ;
#23165 = CARTESIAN_POINT('Origin',(31.8198051533946,322.630194846605,-13.0085799786045)) ;
#23166 = CARTESIAN_POINT('',(31.8198051533946,322.630194846605,-12.0171599572091)) ;
#23167 = CARTESIAN_POINT('',(35.1198051533946,322.630194846605,-14.)) ;
#23168 = CARTESIAN_POINT('',(33.4698051533946,322.630194846605,-13.0085799786045)) ;
#23169 = CARTESIAN_POINT('Origin',(31.8198051533946,322.630194846605,-14.)) ;
#23170 = CARTESIAN_POINT('Origin',(31.8198051533946,322.630194846605,-22.)) ;
#23171 = CARTESIAN_POINT('',(35.1198051533946,322.630194846605,-24.)) ;
#23172 = CARTESIAN_POINT('Origin',(31.8198051533946,322.630194846605,-24.)) ;
#23173 = CARTESIAN_POINT('',(35.1198051533946,322.630194846605,-22.)) ;
#23174 = CARTESIAN_POINT('Origin',(0.,354.45,0.)) ;
#23175 = CARTESIAN_POINT('',(-37.5,354.45,0.)) ;
#23176 = CARTESIAN_POINT('Origin',(0.,354.45,0.)) ;
#23177 = CARTESIAN_POINT('',(-37.5,354.45,-24.)) ;
#23178 = CARTESIAN_POINT('',(-37.5,354.45,0.)) ;
#23179 = CARTESIAN_POINT('Origin',(0.,354.45,-24.)) ;
#23180 = CARTESIAN_POINT('Origin',(75.,209.449999999999,0.)) ;
#23181 = CARTESIAN_POINT('',(-75.0000000000002,209.45,0.)) ;
#23182 = CARTESIAN_POINT('',(75.,209.449999999999,0.)) ;
#23183 = CARTESIAN_POINT('',(-100.,209.45,0.)) ;
#23184 = CARTESIAN_POINT('',(-75.0000000000002,209.45,-24.)) ;
#23185 = CARTESIAN_POINT('',(-75.0000000000002,209.45,0.)) ;
#23186 = CARTESIAN_POINT('',(75.,209.449999999999,-24.)) ;
#23187 = CARTESIAN_POINT('',(-100.,209.45,-24.)) ;
#23188 = CARTESIAN_POINT('',(75.,209.449999999999,0.)) ;
#23189 = CARTESIAN_POINT('Origin',(75.0000000000001,409.45,0.)) ;
#23190 = CARTESIAN_POINT('',(75.0000000000001,409.45,0.)) ;
#23191 = CARTESIAN_POINT('',(75.,209.449999999999,0.)) ;
#23192 = CARTESIAN_POINT('',(75.0000000000001,409.45,-24.)) ;
#23193 = CARTESIAN_POINT('',(75.,209.449999999999,-24.)) ;
#23194 = CARTESIAN_POINT('',(75.0000000000001,409.45,0.)) ;
#23195 = CARTESIAN_POINT('Origin',(-74.9999999999999,409.45,0.)) ;
#23196 = CARTESIAN_POINT('',(-74.9999999999999,409.45,0.)) ;
#23197 = CARTESIAN_POINT('',(-74.9999999999999,409.45,0.)) ;
#23198 = CARTESIAN_POINT('',(-74.9999999999999,409.45,-24.)) ;
#23199 = CARTESIAN_POINT('',(-74.9999999999999,409.45,-24.)) ;
#23200 = CARTESIAN_POINT('',(-74.9999999999999,409.45,0.)) ;
#23201 = CARTESIAN_POINT('Origin',(-75.0000000000002,209.45,0.)) ;
#23202 = CARTESIAN_POINT('',(-74.9999999999999,409.45,0.)) ;
#23203 = CARTESIAN_POINT('',(-74.9999999999999,409.45,-24.)) ;
#23204 = CARTESIAN_POINT('Origin',(-6.21724893790088E-14,309.45,0.)) ;
#23205 = CARTESIAN_POINT('Origin',(-6.21724893790088E-14,309.45,-24.)) ;
#23206 = CARTESIAN_POINT('',(0.,0.,0.)) ;
#23207 = CARTESIAN_POINT('Origin',(-63.0000000000005,199.45,-124.)) ;
#23208 = CARTESIAN_POINT('',(-63.0000000000005,199.45,-115.)) ;
#23209 = CARTESIAN_POINT('Origin',(-63.0000000000005,199.45,-124.)) ;
#23210 = CARTESIAN_POINT('',(-63.0000000000005,199.45,-118.5)) ;
#23211 = CARTESIAN_POINT('Origin',(-63.0000000000005,199.45,-124.)) ;
#23212 = CARTESIAN_POINT('Origin',(-63.0000000000005,194.45,-124.)) ;
#23213 = CARTESIAN_POINT('',(-63.0000000000005,189.45,-115.)) ;
#23214 = CARTESIAN_POINT('Origin',(-63.0000000000005,189.45,-124.)) ;
#23215 = CARTESIAN_POINT('',(-63.0000000000005,194.45,-115.)) ;
#23216 = CARTESIAN_POINT('Origin',(-63.0000000000005,208.45,-124.)) ;
#23217 = CARTESIAN_POINT('',(-63.0000000000005,209.45,-118.5)) ;
#23218 = CARTESIAN_POINT('',(-63.0000000000005,208.45,-118.5)) ;
#23219 = CARTESIAN_POINT('Origin',(-63.0000000000005,209.45,-124.)) ;
#23220 = CARTESIAN_POINT('Origin',(-44.9999999999999,199.45,-12.)) ;
#23221 = CARTESIAN_POINT('',(-44.9999999999999,199.45,-3.)) ;
#23222 = CARTESIAN_POINT('Origin',(-44.9999999999999,199.45,-12.)) ;
#23223 = CARTESIAN_POINT('',(-44.9999999999999,199.45,-6.5)) ;
#23224 = CARTESIAN_POINT('Origin',(-44.9999999999999,199.45,-12.)) ;
#23225 = CARTESIAN_POINT('Origin',(-44.9999999999999,194.45,-12.)) ;
#23226 = CARTESIAN_POINT('',(-44.9999999999999,189.45,-3.)) ;
#23227 = CARTESIAN_POINT('Origin',(-44.9999999999999,189.45,-12.)) ;
#23228 = CARTESIAN_POINT('',(-44.9999999999999,194.45,-3.)) ;
#23229 = CARTESIAN_POINT('Origin',(-44.9999999999999,208.45,-12.)) ;
#23230 = CARTESIAN_POINT('',(-44.9999999999999,209.45,-6.5)) ;
#23231 = CARTESIAN_POINT('',(-44.9999999999999,208.45,-6.5)) ;
#23232 = CARTESIAN_POINT('Origin',(-44.9999999999999,209.45,-12.)) ;
#23233 = CARTESIAN_POINT('Origin',(62.9999999999994,199.45,-124.)) ;
#23234 = CARTESIAN_POINT('',(62.9999999999994,199.45,-115.)) ;
#23235 = CARTESIAN_POINT('Origin',(62.9999999999994,199.45,-124.)) ;
#23236 = CARTESIAN_POINT('',(62.9999999999994,199.45,-118.5)) ;
#23237 = CARTESIAN_POINT('Origin',(62.9999999999994,199.45,-124.)) ;
#23238 = CARTESIAN_POINT('Origin',(62.9999999999994,194.45,-124.)) ;
#23239 = CARTESIAN_POINT('',(62.9999999999994,189.45,-115.)) ;
#23240 = CARTESIAN_POINT('Origin',(62.9999999999994,189.45,-124.)) ;
#23241 = CARTESIAN_POINT('',(62.9999999999994,194.45,-115.)) ;
#23242 = CARTESIAN_POINT('Origin',(62.9999999999994,208.45,-124.)) ;
#23243 = CARTESIAN_POINT('',(62.9999999999994,209.45,-118.5)) ;
#23244 = CARTESIAN_POINT('',(62.9999999999994,208.45,-118.5)) ;
#23245 = CARTESIAN_POINT('Origin',(62.9999999999994,209.45,-124.)) ;
#23246 = CARTESIAN_POINT('Origin',(44.9999999999995,199.45,-12.)) ;
#23247 = CARTESIAN_POINT('',(44.9999999999995,199.45,-3.)) ;
#23248 = CARTESIAN_POINT('Origin',(44.9999999999995,199.45,-12.)) ;
#23249 = CARTESIAN_POINT('',(44.9999999999995,199.45,-6.5)) ;
#23250 = CARTESIAN_POINT('Origin',(44.9999999999995,199.45,-12.)) ;
#23251 = CARTESIAN_POINT('Origin',(44.9999999999995,194.45,-12.)) ;
#23252 = CARTESIAN_POINT('',(44.9999999999995,189.45,-3.)) ;
#23253 = CARTESIAN_POINT('Origin',(44.9999999999995,189.45,-12.)) ;
#23254 = CARTESIAN_POINT('',(44.9999999999995,194.45,-3.)) ;
#23255 = CARTESIAN_POINT('Origin',(44.9999999999995,208.45,-12.)) ;
#23256 = CARTESIAN_POINT('',(44.9999999999995,209.45,-6.5)) ;
#23257 = CARTESIAN_POINT('',(44.9999999999995,208.45,-6.5)) ;
#23258 = CARTESIAN_POINT('Origin',(44.9999999999995,209.45,-12.)) ;
#23259 = CARTESIAN_POINT('Origin',(62.9999999999994,199.45,-54.)) ;
#23260 = CARTESIAN_POINT('',(62.9999999999994,199.45,-45.)) ;
#23261 = CARTESIAN_POINT('Origin',(62.9999999999994,199.45,-54.)) ;
#23262 = CARTESIAN_POINT('',(62.9999999999994,199.45,-48.5)) ;
#23263 = CARTESIAN_POINT('Origin',(62.9999999999994,199.45,-54.)) ;
#23264 = CARTESIAN_POINT('Origin',(62.9999999999994,194.45,-54.)) ;
#23265 = CARTESIAN_POINT('',(62.9999999999994,189.45,-45.)) ;
#23266 = CARTESIAN_POINT('Origin',(62.9999999999994,189.45,-54.)) ;
#23267 = CARTESIAN_POINT('',(62.9999999999994,194.45,-45.)) ;
#23268 = CARTESIAN_POINT('Origin',(62.9999999999994,208.45,-54.)) ;
#23269 = CARTESIAN_POINT('',(62.9999999999994,209.45,-48.5)) ;
#23270 = CARTESIAN_POINT('',(62.9999999999994,208.45,-48.5)) ;
#23271 = CARTESIAN_POINT('Origin',(62.9999999999994,209.45,-54.)) ;
#23272 = CARTESIAN_POINT('Origin',(44.9999999999995,199.45,-166.)) ;
#23273 = CARTESIAN_POINT('',(44.9999999999995,199.45,-157.)) ;
#23274 = CARTESIAN_POINT('Origin',(44.9999999999995,199.45,-166.)) ;
#23275 = CARTESIAN_POINT('',(44.9999999999995,199.45,-160.5)) ;
#23276 = CARTESIAN_POINT('Origin',(44.9999999999995,199.45,-166.)) ;
#23277 = CARTESIAN_POINT('Origin',(44.9999999999995,194.45,-166.)) ;
#23278 = CARTESIAN_POINT('',(44.9999999999995,189.45,-157.)) ;
#23279 = CARTESIAN_POINT('Origin',(44.9999999999995,189.45,-166.)) ;
#23280 = CARTESIAN_POINT('',(44.9999999999995,194.45,-157.)) ;
#23281 = CARTESIAN_POINT('Origin',(44.9999999999995,208.45,-166.)) ;
#23282 = CARTESIAN_POINT('',(44.9999999999995,209.45,-160.5)) ;
#23283 = CARTESIAN_POINT('',(44.9999999999995,208.45,-160.5)) ;
#23284 = CARTESIAN_POINT('Origin',(44.9999999999995,209.45,-166.)) ;
#23285 = CARTESIAN_POINT('Origin',(-63.0000000000005,199.45,-54.)) ;
#23286 = CARTESIAN_POINT('',(-63.0000000000005,199.45,-45.)) ;
#23287 = CARTESIAN_POINT('Origin',(-63.0000000000005,199.45,-54.)) ;
#23288 = CARTESIAN_POINT('',(-63.0000000000005,199.45,-48.5)) ;
#23289 = CARTESIAN_POINT('Origin',(-63.0000000000005,199.45,-54.)) ;
#23290 = CARTESIAN_POINT('Origin',(-63.0000000000005,194.45,-54.)) ;
#23291 = CARTESIAN_POINT('',(-63.0000000000005,189.45,-45.)) ;
#23292 = CARTESIAN_POINT('Origin',(-63.0000000000005,189.45,-54.)) ;
#23293 = CARTESIAN_POINT('',(-63.0000000000005,194.45,-45.)) ;
#23294 = CARTESIAN_POINT('Origin',(-63.0000000000005,208.45,-54.)) ;
#23295 = CARTESIAN_POINT('',(-63.0000000000005,209.45,-48.5)) ;
#23296 = CARTESIAN_POINT('',(-63.0000000000005,208.45,-48.5)) ;
#23297 = CARTESIAN_POINT('Origin',(-63.0000000000005,209.45,-54.)) ;
#23298 = CARTESIAN_POINT('Origin',(-44.9999999999999,199.45,-166.)) ;
#23299 = CARTESIAN_POINT('',(-44.9999999999999,199.45,-157.)) ;
#23300 = CARTESIAN_POINT('Origin',(-44.9999999999999,199.45,-166.)) ;
#23301 = CARTESIAN_POINT('',(-44.9999999999999,199.45,-160.5)) ;
#23302 = CARTESIAN_POINT('Origin',(-44.9999999999999,199.45,-166.)) ;
#23303 = CARTESIAN_POINT('Origin',(-44.9999999999999,194.45,-166.)) ;
#23304 = CARTESIAN_POINT('',(-44.9999999999999,189.45,-157.)) ;
#23305 = CARTESIAN_POINT('Origin',(-44.9999999999999,189.45,-166.)) ;
#23306 = CARTESIAN_POINT('',(-44.9999999999999,194.45,-157.)) ;
#23307 = CARTESIAN_POINT('Origin',(-44.9999999999999,208.45,-166.)) ;
#23308 = CARTESIAN_POINT('',(-44.9999999999999,209.45,-160.5)) ;
#23309 = CARTESIAN_POINT('',(-44.9999999999999,208.45,-160.5)) ;
#23310 = CARTESIAN_POINT('Origin',(-44.9999999999999,209.45,-166.)) ;
#23311 = CARTESIAN_POINT('Origin',(-87.4999999999996,199.449999999999,-158.)) ;
#23312 = CARTESIAN_POINT('',(-87.4999999999996,199.449999999999,-167.)) ;
#23313 = CARTESIAN_POINT('Origin',(-87.4999999999996,199.449999999999,-158.)) ;
#23314 = CARTESIAN_POINT('',(-87.4999999999996,199.449999999999,-163.5)) ;
#23315 = CARTESIAN_POINT('Origin',(-87.4999999999996,199.449999999999,-158.)) ;
#23316 = CARTESIAN_POINT('Origin',(-87.4999999999996,204.449999999999,-158.)) ;
#23317 = CARTESIAN_POINT('',(-87.4999999999996,209.45,-167.)) ;
#23318 = CARTESIAN_POINT('Origin',(-87.4999999999996,209.45,-158.)) ;
#23319 = CARTESIAN_POINT('',(-87.4999999999996,204.449999999999,-167.)) ;
#23320 = CARTESIAN_POINT('Origin',(-87.4999999999996,189.449999999999,-158.)) ;
#23321 = CARTESIAN_POINT('',(-87.4999999999996,189.45,-163.5)) ;
#23322 = CARTESIAN_POINT('',(-87.4999999999996,189.449999999999,-163.5)) ;
#23323 = CARTESIAN_POINT('Origin',(-87.4999999999996,189.45,-158.)) ;
#23324 = CARTESIAN_POINT('Origin',(87.5000000000001,199.45,-20.)) ;
#23325 = CARTESIAN_POINT('',(87.5000000000001,199.45,-29.)) ;
#23326 = CARTESIAN_POINT('Origin',(87.5000000000001,199.45,-20.)) ;
#23327 = CARTESIAN_POINT('',(87.5000000000001,199.45,-25.5)) ;
#23328 = CARTESIAN_POINT('Origin',(87.5000000000001,199.45,-20.)) ;
#23329 = CARTESIAN_POINT('Origin',(87.5000000000001,204.45,-20.)) ;
#23330 = CARTESIAN_POINT('',(87.5000000000001,209.45,-29.)) ;
#23331 = CARTESIAN_POINT('Origin',(87.5000000000001,209.45,-20.)) ;
#23332 = CARTESIAN_POINT('',(87.5000000000001,204.45,-29.)) ;
#23333 = CARTESIAN_POINT('Origin',(87.5000000000001,189.45,-20.)) ;
#23334 = CARTESIAN_POINT('',(87.5000000000001,189.45,-25.5)) ;
#23335 = CARTESIAN_POINT('',(87.5000000000001,189.45,-25.5)) ;
#23336 = CARTESIAN_POINT('Origin',(87.5000000000001,189.45,-20.)) ;
#23337 = CARTESIAN_POINT('Origin',(87.5000000000001,199.45,-158.)) ;
#23338 = CARTESIAN_POINT('',(87.5000000000001,199.45,-167.)) ;
#23339 = CARTESIAN_POINT('Origin',(87.5000000000001,199.45,-158.)) ;
#23340 = CARTESIAN_POINT('',(87.5000000000001,199.45,-163.5)) ;
#23341 = CARTESIAN_POINT('Origin',(87.5000000000001,199.45,-158.)) ;
#23342 = CARTESIAN_POINT('Origin',(87.5000000000001,204.45,-158.)) ;
#23343 = CARTESIAN_POINT('',(87.5,209.45,-167.)) ;
#23344 = CARTESIAN_POINT('Origin',(87.5,209.45,-158.)) ;
#23345 = CARTESIAN_POINT('',(87.5000000000001,204.45,-167.)) ;
#23346 = CARTESIAN_POINT('Origin',(87.5000000000001,189.45,-158.)) ;
#23347 = CARTESIAN_POINT('',(87.5000000000001,189.45,-163.5)) ;
#23348 = CARTESIAN_POINT('',(87.5000000000001,189.45,-163.5)) ;
#23349 = CARTESIAN_POINT('Origin',(87.5000000000001,189.45,-158.)) ;
#23350 = CARTESIAN_POINT('Origin',(-87.4999999999996,199.449999999999,-20.)) ;
#23351 = CARTESIAN_POINT('',(-87.4999999999996,199.449999999999,-29.)) ;
#23352 = CARTESIAN_POINT('Origin',(-87.4999999999996,199.449999999999,-20.)) ;
#23353 = CARTESIAN_POINT('',(-87.4999999999996,199.449999999999,-25.5)) ;
#23354 = CARTESIAN_POINT('Origin',(-87.4999999999996,199.449999999999,-20.)) ;
#23355 = CARTESIAN_POINT('Origin',(-87.4999999999996,204.449999999999,-20.)) ;
#23356 = CARTESIAN_POINT('',(-87.4999999999996,209.45,-29.)) ;
#23357 = CARTESIAN_POINT('Origin',(-87.4999999999996,209.45,-20.)) ;
#23358 = CARTESIAN_POINT('',(-87.4999999999996,204.449999999999,-29.)) ;
#23359 = CARTESIAN_POINT('Origin',(-87.4999999999995,189.449999999999,-20.)) ;
#23360 = CARTESIAN_POINT('',(-87.4999999999995,189.45,-25.5)) ;
#23361 = CARTESIAN_POINT('',(-87.4999999999995,189.449999999999,-25.5)) ;
#23362 = CARTESIAN_POINT('Origin',(-87.4999999999995,189.45,-20.)) ;
#23363 = CARTESIAN_POINT('Origin',(-100.,209.45,0.)) ;
#23364 = CARTESIAN_POINT('',(100.,209.449999999999,-178.)) ;
#23365 = CARTESIAN_POINT('',(-100.,209.45,-178.)) ;
#23366 = CARTESIAN_POINT('',(-50.0000000000001,209.45,-178.)) ;
#23367 = CARTESIAN_POINT('',(-100.,209.45,0.)) ;
#23368 = CARTESIAN_POINT('',(-100.,209.45,0.)) ;
#23369 = CARTESIAN_POINT('',(100.,209.449999999999,0.)) ;
#23370 = CARTESIAN_POINT('',(-100.,209.45,0.)) ;
#23371 = CARTESIAN_POINT('',(100.,209.449999999999,0.)) ;
#23372 = CARTESIAN_POINT('Origin',(-100.,189.45,0.)) ;
#23373 = CARTESIAN_POINT('',(-100.,189.45,-178.)) ;
#23374 = CARTESIAN_POINT('',(-100.,194.45,-178.)) ;
#23375 = CARTESIAN_POINT('',(-100.,189.45,0.)) ;
#23376 = CARTESIAN_POINT('',(-100.,189.45,0.)) ;
#23377 = CARTESIAN_POINT('',(-100.,189.45,0.)) ;
#23378 = CARTESIAN_POINT('Origin',(100.,189.45,0.)) ;
#23379 = CARTESIAN_POINT('',(100.,189.45,-178.)) ;
#23380 = CARTESIAN_POINT('',(50.,189.45,-178.)) ;
#23381 = CARTESIAN_POINT('',(100.,189.45,0.)) ;
#23382 = CARTESIAN_POINT('',(100.,189.45,0.)) ;
#23383 = CARTESIAN_POINT('',(100.,189.45,0.)) ;
#23384 = CARTESIAN_POINT('Origin',(100.,209.449999999999,0.)) ;
#23385 = CARTESIAN_POINT('',(100.,204.45,-178.)) ;
#23386 = CARTESIAN_POINT('',(100.,209.449999999999,0.)) ;
#23387 = CARTESIAN_POINT('Origin',(-3.5527136788005E-14,199.45,0.)) ;
#23388 = CARTESIAN_POINT('Origin',(-4.44089209850063E-14,199.45,-178.)) ;
#23389 = CARTESIAN_POINT('',(0.,0.,0.)) ;
#23390 = CARTESIAN_POINT('Origin',(62.9999999999988,385.343736383858,-54.)) ;
#23391 = CARTESIAN_POINT('',(62.9999999999988,383.888531181086,-54.)) ;
#23392 = CARTESIAN_POINT('',(62.9999999999988,386.45,-58.263)) ;
#23393 = CARTESIAN_POINT('',(62.9999999999988,385.343736383858,-56.4218681615831)) ;
#23394 = CARTESIAN_POINT('Origin',(62.9999999999988,386.45,-54.)) ;
#23395 = CARTESIAN_POINT('Origin',(62.9999999999988,405.45,-54.)) ;
#23396 = CARTESIAN_POINT('',(62.9999999999988,409.45,-58.263)) ;
#23397 = CARTESIAN_POINT('Origin',(62.9999999999988,409.45,-54.)) ;
#23398 = CARTESIAN_POINT('',(62.9999999999988,405.45,-58.263)) ;
#23399 = CARTESIAN_POINT('Origin',(62.9999999999988,385.343736383858,-124.)) ;
#23400 = CARTESIAN_POINT('',(62.9999999999988,383.888531181086,-124.)) ;
#23401 = CARTESIAN_POINT('',(62.9999999999988,386.45,-128.263)) ;
#23402 = CARTESIAN_POINT('',(62.9999999999988,385.343736383858,-126.421868161583)) ;
#23403 = CARTESIAN_POINT('Origin',(62.9999999999988,386.45,-124.)) ;
#23404 = CARTESIAN_POINT('Origin',(62.9999999999988,405.45,-124.)) ;
#23405 = CARTESIAN_POINT('',(62.9999999999988,409.45,-128.263)) ;
#23406 = CARTESIAN_POINT('Origin',(62.9999999999988,409.45,-124.)) ;
#23407 = CARTESIAN_POINT('',(62.9999999999988,405.45,-128.263)) ;
#23408 = CARTESIAN_POINT('Origin',(62.9999999999994,228.556263616143,-124.)) ;
#23409 = CARTESIAN_POINT('',(62.9999999999994,230.011468818914,-124.)) ;
#23410 = CARTESIAN_POINT('',(62.9999999999994,227.45,-119.737)) ;
#23411 = CARTESIAN_POINT('',(62.9999999999994,228.556263616143,-121.578131838417)) ;
#23412 = CARTESIAN_POINT('Origin',(62.9999999999994,227.45,-124.)) ;
#23413 = CARTESIAN_POINT('Origin',(62.9999999999994,208.45,-124.)) ;
#23414 = CARTESIAN_POINT('',(62.9999999999994,209.449999999999,-119.737)) ;
#23415 = CARTESIAN_POINT('Origin',(62.9999999999994,209.449999999999,-124.)) ;
#23416 = CARTESIAN_POINT('',(62.9999999999994,208.45,-119.737)) ;
#23417 = CARTESIAN_POINT('Origin',(62.9999999999994,228.556263616143,-54.)) ;
#23418 = CARTESIAN_POINT('',(62.9999999999994,230.011468818914,-54.)) ;
#23419 = CARTESIAN_POINT('',(62.9999999999994,227.45,-49.737)) ;
#23420 = CARTESIAN_POINT('',(62.9999999999994,228.556263616143,-51.5781318384169)) ;
#23421 = CARTESIAN_POINT('Origin',(62.9999999999994,227.45,-54.)) ;
#23422 = CARTESIAN_POINT('Origin',(62.9999999999994,208.45,-54.)) ;
#23423 = CARTESIAN_POINT('',(62.9999999999994,209.449999999999,-49.737)) ;
#23424 = CARTESIAN_POINT('Origin',(62.9999999999994,209.449999999999,-54.)) ;
#23425 = CARTESIAN_POINT('',(62.9999999999994,208.45,-49.737)) ;
#23426 = CARTESIAN_POINT('Origin',(63.,379.45,-138.893736383857)) ;
#23427 = CARTESIAN_POINT('',(63.,379.45,-137.438531181086)) ;
#23428 = CARTESIAN_POINT('',(58.737,379.45,-140.)) ;
#23429 = CARTESIAN_POINT('',(60.5781318384169,379.45,-138.893736383857)) ;
#23430 = CARTESIAN_POINT('Origin',(63.,379.45,-140.)) ;
#23431 = CARTESIAN_POINT('Origin',(63.,379.45,-159.)) ;
#23432 = CARTESIAN_POINT('',(58.737,379.45,-154.)) ;
#23433 = CARTESIAN_POINT('',(58.737,379.45,-159.)) ;
#23434 = CARTESIAN_POINT('Origin',(63.,379.45,-154.)) ;
#23435 = CARTESIAN_POINT('Origin',(63.,239.45,-138.893736383857)) ;
#23436 = CARTESIAN_POINT('',(63.,239.45,-137.438531181086)) ;
#23437 = CARTESIAN_POINT('',(58.737,239.45,-140.)) ;
#23438 = CARTESIAN_POINT('',(60.5781318384169,239.45,-138.893736383857)) ;
#23439 = CARTESIAN_POINT('Origin',(63.,239.45,-140.)) ;
#23440 = CARTESIAN_POINT('Origin',(63.,239.45,-159.)) ;
#23441 = CARTESIAN_POINT('',(58.737,239.45,-154.)) ;
#23442 = CARTESIAN_POINT('',(58.737,239.45,-159.)) ;
#23443 = CARTESIAN_POINT('Origin',(63.,239.45,-154.)) ;
#23444 = CARTESIAN_POINT('Origin',(63.,309.45,-154.)) ;
#23445 = CARTESIAN_POINT('',(51.0000000000001,209.449999999999,-154.)) ;
#23446 = CARTESIAN_POINT('',(75.,209.449999999999,-154.)) ;
#23447 = CARTESIAN_POINT('',(68.9999999999998,209.449999999999,-154.)) ;
#23448 = CARTESIAN_POINT('',(50.9999999999999,409.45,-154.)) ;
#23449 = CARTESIAN_POINT('',(51.0000000000001,259.449999999999,-154.)) ;
#23450 = CARTESIAN_POINT('',(75.0000000000001,409.45,-154.)) ;
#23451 = CARTESIAN_POINT('',(56.9999999999999,409.45,-154.)) ;
#23452 = CARTESIAN_POINT('',(75.0000000000001,359.45,-154.)) ;
#23453 = CARTESIAN_POINT('Origin',(63.,379.45,-39.1062636161425)) ;
#23454 = CARTESIAN_POINT('',(63.,379.45,-40.5614688189145)) ;
#23455 = CARTESIAN_POINT('',(58.737,379.45,-38.)) ;
#23456 = CARTESIAN_POINT('',(60.5781318384169,379.45,-39.1062636161425)) ;
#23457 = CARTESIAN_POINT('Origin',(63.,379.45,-38.)) ;
#23458 = CARTESIAN_POINT('Origin',(63.,379.45,-19.)) ;
#23459 = CARTESIAN_POINT('',(58.737,379.45,-24.)) ;
#23460 = CARTESIAN_POINT('Origin',(63.,379.45,-24.)) ;
#23461 = CARTESIAN_POINT('',(58.737,379.45,-19.)) ;
#23462 = CARTESIAN_POINT('Origin',(63.,239.45,-39.1062636161425)) ;
#23463 = CARTESIAN_POINT('',(63.,239.45,-40.5614688189145)) ;
#23464 = CARTESIAN_POINT('',(58.737,239.45,-38.)) ;
#23465 = CARTESIAN_POINT('',(60.5781318384169,239.45,-39.1062636161425)) ;
#23466 = CARTESIAN_POINT('Origin',(63.,239.45,-38.)) ;
#23467 = CARTESIAN_POINT('Origin',(63.,239.45,-19.)) ;
#23468 = CARTESIAN_POINT('',(58.737,239.45,-24.)) ;
#23469 = CARTESIAN_POINT('Origin',(63.,239.45,-24.)) ;
#23470 = CARTESIAN_POINT('',(58.737,239.45,-19.)) ;
#23471 = CARTESIAN_POINT('Origin',(75.0000000000001,409.45,-24.)) ;
#23472 = CARTESIAN_POINT('',(75.,209.449999999999,-24.)) ;
#23473 = CARTESIAN_POINT('',(75.0000000000001,409.45,-24.)) ;
#23474 = CARTESIAN_POINT('',(75.0000000000001,359.45,-24.)) ;
#23475 = CARTESIAN_POINT('',(75.,209.449999999999,-24.)) ;
#23476 = CARTESIAN_POINT('',(75.0000000000001,409.45,-24.)) ;
#23477 = CARTESIAN_POINT('Origin',(50.9999999999999,409.45,-24.)) ;
#23478 = CARTESIAN_POINT('',(50.9999999999999,409.45,-24.)) ;
#23479 = CARTESIAN_POINT('',(56.9999999999999,409.45,-24.)) ;
#23480 = CARTESIAN_POINT('',(50.9999999999999,409.45,-24.)) ;
#23481 = CARTESIAN_POINT('Origin',(51.0000000000001,209.449999999999,-24.)) ;
#23482 = CARTESIAN_POINT('',(51.0000000000001,209.449999999999,-24.)) ;
#23483 = CARTESIAN_POINT('',(51.0000000000001,259.449999999999,-24.)) ;
#23484 = CARTESIAN_POINT('',(51.0000000000001,209.449999999999,-24.)) ;
#23485 = CARTESIAN_POINT('Origin',(75.,209.449999999999,-24.)) ;
#23486 = CARTESIAN_POINT('',(68.9999999999998,209.449999999999,-24.)) ;
#23487 = CARTESIAN_POINT('Origin',(63.,309.45,-24.)) ;
#23488 = CARTESIAN_POINT('',(0.,0.,0.)) ;
#23489 = CARTESIAN_POINT('Origin',(63.,219.45,9.78673043802305)) ;
#23490 = CARTESIAN_POINT('',(63.,219.45,10.5120219304813)) ;
#23491 = CARTESIAN_POINT('',(65.117,219.45,9.24)) ;
#23492 = CARTESIAN_POINT('',(64.2070877496217,219.45,9.78673043802305)) ;
#23493 = CARTESIAN_POINT('Origin',(63.,219.45,9.24)) ;
#23494 = CARTESIAN_POINT('Origin',(63.,219.45,4.23999999999999)) ;
#23495 = CARTESIAN_POINT('',(65.117,219.45,0.)) ;
#23496 = CARTESIAN_POINT('Origin',(63.,219.45,0.)) ;
#23497 = CARTESIAN_POINT('',(65.117,219.45,4.23999999999999)) ;
#23498 = CARTESIAN_POINT('Origin',(-62.9999999999999,219.45,9.78673043802305)) ;
#23499 = CARTESIAN_POINT('',(-62.9999999999999,219.45,10.5120219304813)) ;
#23500 = CARTESIAN_POINT('',(-60.8829999999999,219.45,9.24)) ;
#23501 = CARTESIAN_POINT('',(-61.7929122503782,219.45,9.78673043802305)) ;
#23502 = CARTESIAN_POINT('Origin',(-62.9999999999999,219.45,9.24)) ;
#23503 = CARTESIAN_POINT('Origin',(-62.9999999999999,219.45,4.23999999999999)) ;
#23504 = CARTESIAN_POINT('',(-60.8829999999999,219.45,0.)) ;
#23505 = CARTESIAN_POINT('Origin',(-62.9999999999999,219.45,0.)) ;
#23506 = CARTESIAN_POINT('',(-60.8829999999999,219.45,4.23999999999999)) ;
#23507 = CARTESIAN_POINT('Origin',(44.9999999999989,385.343736383858,12.)) ;
#23508 = CARTESIAN_POINT('',(44.9999999999989,383.888531181086,12.)) ;
#23509 = CARTESIAN_POINT('',(44.9999999999989,386.45,7.73699999999999)) ;
#23510 = CARTESIAN_POINT('',(44.9999999999989,385.343736383858,9.57813183841693)) ;
#23511 = CARTESIAN_POINT('Origin',(44.9999999999989,386.45,12.)) ;
#23512 = CARTESIAN_POINT('Origin',(44.9999999999989,405.45,12.)) ;
#23513 = CARTESIAN_POINT('',(44.9999999999989,409.45,7.73699999999999)) ;
#23514 = CARTESIAN_POINT('Origin',(44.9999999999989,409.45,12.)) ;
#23515 = CARTESIAN_POINT('',(44.9999999999989,405.45,7.737)) ;
#23516 = CARTESIAN_POINT('Origin',(-45.0000000000005,385.343736383858,12.)) ;
#23517 = CARTESIAN_POINT('',(-45.0000000000005,383.888531181086,12.)) ;
#23518 = CARTESIAN_POINT('',(-45.0000000000005,386.45,7.73699999999999)) ;
#23519 = CARTESIAN_POINT('',(-45.0000000000005,385.343736383858,9.57813183841693)) ;
#23520 = CARTESIAN_POINT('Origin',(-45.0000000000005,386.45,12.)) ;
#23521 = CARTESIAN_POINT('Origin',(-45.0000000000005,405.45,12.)) ;
#23522 = CARTESIAN_POINT('',(-45.0000000000005,409.45,7.73699999999999)) ;
#23523 = CARTESIAN_POINT('Origin',(-45.0000000000005,409.45,12.)) ;
#23524 = CARTESIAN_POINT('',(-45.0000000000005,405.45,7.737)) ;
#23525 = CARTESIAN_POINT('Origin',(44.9999999999995,228.556263616143,12.)) ;
#23526 = CARTESIAN_POINT('',(44.9999999999995,230.011468818915,12.)) ;
#23527 = CARTESIAN_POINT('',(44.9999999999995,227.45,16.263)) ;
#23528 = CARTESIAN_POINT('',(44.9999999999995,228.556263616143,14.4218681615831)) ;
#23529 = CARTESIAN_POINT('Origin',(44.9999999999995,227.45,12.)) ;
#23530 = CARTESIAN_POINT('Origin',(44.9999999999995,208.45,12.)) ;
#23531 = CARTESIAN_POINT('',(44.9999999999995,209.449999999999,16.263)) ;
#23532 = CARTESIAN_POINT('Origin',(44.9999999999995,209.449999999999,12.)) ;
#23533 = CARTESIAN_POINT('',(44.9999999999995,208.45,16.263)) ;
#23534 = CARTESIAN_POINT('Origin',(-44.9999999999999,228.556263616143,12.)) ;
#23535 = CARTESIAN_POINT('',(-44.9999999999999,230.011468818915,12.)) ;
#23536 = CARTESIAN_POINT('',(-44.9999999999999,227.45,16.263)) ;
#23537 = CARTESIAN_POINT('',(-44.9999999999999,228.556263616143,14.4218681615831)) ;
#23538 = CARTESIAN_POINT('Origin',(-44.9999999999999,227.45,12.)) ;
#23539 = CARTESIAN_POINT('Origin',(-44.9999999999999,208.45,12.)) ;
#23540 = CARTESIAN_POINT('',(-44.9999999999999,209.449999999999,16.263)) ;
#23541 = CARTESIAN_POINT('Origin',(-44.9999999999999,209.449999999999,12.)) ;
#23542 = CARTESIAN_POINT('',(-44.9999999999999,208.45,16.263)) ;
#23543 = CARTESIAN_POINT('Origin',(-62.9999999999999,239.45,10.)) ;
#23544 = CARTESIAN_POINT('',(-71.9999999999999,239.45,10.)) ;
#23545 = CARTESIAN_POINT('Origin',(-62.9999999999999,239.45,10.)) ;
#23546 = CARTESIAN_POINT('',(-68.4999999999999,239.45,10.)) ;
#23547 = CARTESIAN_POINT('Origin',(-62.9999999999999,239.45,10.)) ;
#23548 = CARTESIAN_POINT('Origin',(-62.9999999999999,239.45,5.)) ;
#23549 = CARTESIAN_POINT('',(-71.9999999999999,239.45,0.)) ;
#23550 = CARTESIAN_POINT('',(-71.9999999999999,239.45,5.)) ;
#23551 = CARTESIAN_POINT('Origin',(-62.9999999999999,239.45,0.)) ;
#23552 = CARTESIAN_POINT('Origin',(-62.9999999999999,239.45,19.)) ;
#23553 = CARTESIAN_POINT('',(-68.4999999999999,239.45,24.)) ;
#23554 = CARTESIAN_POINT('Origin',(-62.9999999999999,239.45,24.)) ;
#23555 = CARTESIAN_POINT('',(-68.4999999999999,239.45,19.)) ;
#23556 = CARTESIAN_POINT('Origin',(63.,379.45,10.)) ;
#23557 = CARTESIAN_POINT('',(54.,379.45,10.)) ;
#23558 = CARTESIAN_POINT('Origin',(63.,379.45,10.)) ;
#23559 = CARTESIAN_POINT('',(57.5,379.45,10.)) ;
#23560 = CARTESIAN_POINT('Origin',(63.,379.45,10.)) ;
#23561 = CARTESIAN_POINT('Origin',(63.,379.45,5.)) ;
#23562 = CARTESIAN_POINT('',(54.,379.45,0.)) ;
#23563 = CARTESIAN_POINT('',(54.,379.45,5.)) ;
#23564 = CARTESIAN_POINT('Origin',(63.,379.45,0.)) ;
#23565 = CARTESIAN_POINT('Origin',(63.,379.45,19.)) ;
#23566 = CARTESIAN_POINT('',(57.5,379.45,24.)) ;
#23567 = CARTESIAN_POINT('Origin',(63.,379.45,24.)) ;
#23568 = CARTESIAN_POINT('',(57.5,379.45,19.)) ;
#23569 = CARTESIAN_POINT('Origin',(63.,239.45,10.)) ;
#23570 = CARTESIAN_POINT('',(54.,239.45,10.)) ;
#23571 = CARTESIAN_POINT('Origin',(63.,239.45,10.)) ;
#23572 = CARTESIAN_POINT('',(57.5,239.45,10.)) ;
#23573 = CARTESIAN_POINT('Origin',(63.,239.45,10.)) ;
#23574 = CARTESIAN_POINT('Origin',(63.,239.45,5.)) ;
#23575 = CARTESIAN_POINT('',(54.,239.45,0.)) ;
#23576 = CARTESIAN_POINT('',(54.,239.45,5.)) ;
#23577 = CARTESIAN_POINT('Origin',(63.,239.45,0.)) ;
#23578 = CARTESIAN_POINT('Origin',(63.,239.45,19.)) ;
#23579 = CARTESIAN_POINT('',(57.5,239.45,24.)) ;
#23580 = CARTESIAN_POINT('Origin',(63.,239.45,24.)) ;
#23581 = CARTESIAN_POINT('',(57.5,239.45,19.)) ;
#23582 = CARTESIAN_POINT('Origin',(-62.9999999999999,379.45,10.)) ;
#23583 = CARTESIAN_POINT('',(-71.9999999999999,379.45,10.)) ;
#23584 = CARTESIAN_POINT('Origin',(-62.9999999999999,379.45,10.)) ;
#23585 = CARTESIAN_POINT('',(-68.4999999999999,379.45,10.)) ;
#23586 = CARTESIAN_POINT('Origin',(-62.9999999999999,379.45,10.)) ;
#23587 = CARTESIAN_POINT('Origin',(-62.9999999999999,379.45,5.)) ;
#23588 = CARTESIAN_POINT('',(-71.9999999999999,379.45,0.)) ;
#23589 = CARTESIAN_POINT('',(-71.9999999999999,379.45,5.)) ;
#23590 = CARTESIAN_POINT('Origin',(-62.9999999999999,379.45,0.)) ;
#23591 = CARTESIAN_POINT('Origin',(-62.9999999999999,379.45,19.)) ;
#23592 = CARTESIAN_POINT('',(-68.4999999999999,379.45,24.)) ;
#23593 = CARTESIAN_POINT('Origin',(-62.9999999999999,379.45,24.)) ;
#23594 = CARTESIAN_POINT('',(-68.4999999999999,379.45,19.)) ;
#23595 = CARTESIAN_POINT('Origin',(45.,354.45,13.0085799786045)) ;
#23596 = CARTESIAN_POINT('',(45.,354.45,12.0171599572091)) ;
#23597 = CARTESIAN_POINT('',(48.3,354.45,14.)) ;
#23598 = CARTESIAN_POINT('',(46.65,354.45,13.0085799786045)) ;
#23599 = CARTESIAN_POINT('Origin',(45.,354.45,14.)) ;
#23600 = CARTESIAN_POINT('Origin',(45.,354.45,22.)) ;
#23601 = CARTESIAN_POINT('',(48.3,354.45,24.)) ;
#23602 = CARTESIAN_POINT('',(48.3,354.45,22.)) ;
#23603 = CARTESIAN_POINT('Origin',(45.,354.45,24.)) ;
#23604 = CARTESIAN_POINT('Origin',(-5.51091059616309E-15,399.45,13.3540332243106)) ;
#23605 = CARTESIAN_POINT('',(-5.67105257905314E-15,399.45,12.4873333915981)) ;
#23606 = CARTESIAN_POINT('',(2.51749999999999,399.45,14.)) ;
#23607 = CARTESIAN_POINT('',(1.44243074893997,399.45,13.3540332243106)) ;
#23608 = CARTESIAN_POINT('Origin',(-5.51091059616309E-15,399.45,14.)) ;
#23609 = CARTESIAN_POINT('Origin',(-5.51091059616309E-15,399.45,22.)) ;
#23610 = CARTESIAN_POINT('',(2.51749999999999,399.45,24.)) ;
#23611 = CARTESIAN_POINT('',(2.51749999999999,399.45,22.)) ;
#23612 = CARTESIAN_POINT('Origin',(-5.51091059616309E-15,399.45,24.)) ;
#23613 = CARTESIAN_POINT('Origin',(-45.,354.45,13.3540332243106)) ;
#23614 = CARTESIAN_POINT('',(-45.,354.45,12.4873333915981)) ;
#23615 = CARTESIAN_POINT('',(-42.4825,354.45,14.)) ;
#23616 = CARTESIAN_POINT('',(-43.55756925106,354.45,13.3540332243106)) ;
#23617 = CARTESIAN_POINT('Origin',(-45.,354.45,14.)) ;
#23618 = CARTESIAN_POINT('Origin',(-45.,354.45,22.)) ;
#23619 = CARTESIAN_POINT('',(-42.4825,354.45,24.)) ;
#23620 = CARTESIAN_POINT('',(-42.4825,354.45,22.)) ;
#23621 = CARTESIAN_POINT('Origin',(-45.,354.45,24.)) ;
#23622 = CARTESIAN_POINT('Origin',(0.,309.45,13.3540332243106)) ;
#23623 = CARTESIAN_POINT('',(-1.60141982890047E-16,309.45,12.4873333915981)) ;
#23624 = CARTESIAN_POINT('',(2.5175,309.45,14.)) ;
#23625 = CARTESIAN_POINT('',(1.44243074893998,309.45,13.3540332243106)) ;
#23626 = CARTESIAN_POINT('Origin',(0.,309.45,14.)) ;
#23627 = CARTESIAN_POINT('Origin',(0.,309.45,22.)) ;
#23628 = CARTESIAN_POINT('',(2.5175,309.45,24.)) ;
#23629 = CARTESIAN_POINT('',(2.5175,309.45,22.)) ;
#23630 = CARTESIAN_POINT('Origin',(0.,309.45,24.)) ;
#23631 = CARTESIAN_POINT('Origin',(-31.8198051533946,322.630194846605,13.3540332243106)) ;
#23632 = CARTESIAN_POINT('',(-31.8198051533946,322.630194846605,12.4873333915981)) ;
#23633 = CARTESIAN_POINT('',(-29.3023051533946,322.630194846605,14.)) ;
#23634 = CARTESIAN_POINT('',(-30.3773744044546,322.630194846605,13.3540332243106)) ;
#23635 = CARTESIAN_POINT('Origin',(-31.8198051533946,322.630194846605,14.)) ;
#23636 = CARTESIAN_POINT('Origin',(-31.8198051533946,322.630194846605,22.)) ;
#23637 = CARTESIAN_POINT('',(-29.3023051533946,322.630194846605,24.)) ;
#23638 = CARTESIAN_POINT('',(-29.3023051533946,322.630194846605,22.)) ;
#23639 = CARTESIAN_POINT('Origin',(-31.8198051533946,322.630194846605,24.)) ;
#23640 = CARTESIAN_POINT('Origin',(-31.8198051533946,386.269805153395,13.3540332243106)) ;
#23641 = CARTESIAN_POINT('',(-31.8198051533946,386.269805153395,12.4873333915981)) ;
#23642 = CARTESIAN_POINT('',(-29.3023051533946,386.269805153395,14.)) ;
#23643 = CARTESIAN_POINT('',(-30.3773744044546,386.269805153395,13.3540332243106)) ;
#23644 = CARTESIAN_POINT('Origin',(-31.8198051533946,386.269805153395,14.)) ;
#23645 = CARTESIAN_POINT('Origin',(-31.8198051533946,386.269805153395,22.)) ;
#23646 = CARTESIAN_POINT('',(-29.3023051533946,386.269805153395,24.)) ;
#23647 = CARTESIAN_POINT('',(-29.3023051533946,386.269805153395,22.)) ;
#23648 = CARTESIAN_POINT('Origin',(-31.8198051533946,386.269805153395,24.)) ;
#23649 = CARTESIAN_POINT('Origin',(31.8198051533946,386.269805153395,13.3540332243106)) ;
#23650 = CARTESIAN_POINT('',(31.8198051533946,386.269805153395,12.4873333915981)) ;
#23651 = CARTESIAN_POINT('',(34.3373051533946,386.269805153395,14.)) ;
#23652 = CARTESIAN_POINT('',(33.2622359023346,386.269805153395,13.3540332243106)) ;
#23653 = CARTESIAN_POINT('Origin',(31.8198051533946,386.269805153395,14.)) ;
#23654 = CARTESIAN_POINT('Origin',(31.8198051533946,386.269805153395,22.)) ;
#23655 = CARTESIAN_POINT('',(34.3373051533946,386.269805153395,24.)) ;
#23656 = CARTESIAN_POINT('',(34.3373051533946,386.269805153395,22.)) ;
#23657 = CARTESIAN_POINT('Origin',(31.8198051533946,386.269805153395,24.)) ;
#23658 = CARTESIAN_POINT('Origin',(31.8198051533946,322.630194846605,13.0085799786045)) ;
#23659 = CARTESIAN_POINT('',(31.8198051533946,322.630194846605,12.0171599572091)) ;
#23660 = CARTESIAN_POINT('',(35.1198051533946,322.630194846605,14.)) ;
#23661 = CARTESIAN_POINT('',(33.4698051533946,322.630194846605,13.0085799786045)) ;
#23662 = CARTESIAN_POINT('Origin',(31.8198051533946,322.630194846605,14.)) ;
#23663 = CARTESIAN_POINT('Origin',(31.8198051533946,322.630194846605,22.)) ;
#23664 = CARTESIAN_POINT('',(35.1198051533946,322.630194846605,24.)) ;
#23665 = CARTESIAN_POINT('',(35.1198051533946,322.630194846605,22.)) ;
#23666 = CARTESIAN_POINT('Origin',(31.8198051533946,322.630194846605,24.)) ;
#23667 = CARTESIAN_POINT('Origin',(0.,354.45,0.)) ;
#23668 = CARTESIAN_POINT('',(-37.5,354.45,24.)) ;
#23669 = CARTESIAN_POINT('Origin',(0.,354.45,24.)) ;
#23670 = CARTESIAN_POINT('',(-37.5,354.45,0.)) ;
#23671 = CARTESIAN_POINT('',(-37.5,354.45,0.)) ;
#23672 = CARTESIAN_POINT('Origin',(0.,354.45,0.)) ;
#23673 = CARTESIAN_POINT('Origin',(75.,209.449999999999,0.)) ;
#23674 = CARTESIAN_POINT('',(-75.0000000000002,209.45,0.)) ;
#23675 = CARTESIAN_POINT('',(75.,209.449999999999,0.)) ;
#23676 = CARTESIAN_POINT('',(-100.,209.45,0.)) ;
#23677 = CARTESIAN_POINT('',(75.,209.449999999999,24.)) ;
#23678 = CARTESIAN_POINT('',(75.,209.449999999999,0.)) ;
#23679 = CARTESIAN_POINT('',(-75.0000000000002,209.45,24.)) ;
#23680 = CARTESIAN_POINT('',(-100.,209.45,24.)) ;
#23681 = CARTESIAN_POINT('',(-75.0000000000002,209.45,0.)) ;
#23682 = CARTESIAN_POINT('Origin',(75.0000000000001,409.45,0.)) ;
#23683 = CARTESIAN_POINT('',(75.0000000000001,409.45,0.)) ;
#23684 = CARTESIAN_POINT('',(75.,209.449999999999,0.)) ;
#23685 = CARTESIAN_POINT('',(75.0000000000001,409.45,24.)) ;
#23686 = CARTESIAN_POINT('',(75.0000000000001,409.45,0.)) ;
#23687 = CARTESIAN_POINT('',(75.,209.449999999999,24.)) ;
#23688 = CARTESIAN_POINT('Origin',(-74.9999999999999,409.45,0.)) ;
#23689 = CARTESIAN_POINT('',(-74.9999999999999,409.45,0.)) ;
#23690 = CARTESIAN_POINT('',(-74.9999999999999,409.45,0.)) ;
#23691 = CARTESIAN_POINT('',(-74.9999999999999,409.45,24.)) ;
#23692 = CARTESIAN_POINT('',(-74.9999999999999,409.45,0.)) ;
#23693 = CARTESIAN_POINT('',(-74.9999999999999,409.45,24.)) ;
#23694 = CARTESIAN_POINT('Origin',(-75.0000000000002,209.45,0.)) ;
#23695 = CARTESIAN_POINT('',(-74.9999999999999,409.45,0.)) ;
#23696 = CARTESIAN_POINT('',(-74.9999999999999,409.45,24.)) ;
#23697 = CARTESIAN_POINT('Origin',(-6.21724893790088E-14,309.45,0.)) ;
#23698 = CARTESIAN_POINT('Origin',(-6.21724893790088E-14,309.45,24.)) ;
#23699 = CARTESIAN_POINT('',(0.,0.,0.)) ;
#23700 = CARTESIAN_POINT('Origin',(63.0000000000011,385.343736383857,54.)) ;
#23701 = CARTESIAN_POINT('',(63.0000000000011,383.888531181086,54.)) ;
#23702 = CARTESIAN_POINT('',(63.0000000000011,386.45,58.263)) ;
#23703 = CARTESIAN_POINT('',(63.0000000000011,385.343736383857,56.4218681615831)) ;
#23704 = CARTESIAN_POINT('Origin',(63.0000000000011,386.45,54.)) ;
#23705 = CARTESIAN_POINT('Origin',(63.0000000000011,405.45,54.)) ;
#23706 = CARTESIAN_POINT('',(63.0000000000011,409.45,58.263)) ;
#23707 = CARTESIAN_POINT('Origin',(63.0000000000011,409.45,54.)) ;
#23708 = CARTESIAN_POINT('',(63.0000000000011,405.45,58.263)) ;
#23709 = CARTESIAN_POINT('Origin',(63.0000000000011,385.343736383857,124.)) ;
#23710 = CARTESIAN_POINT('',(63.0000000000011,383.888531181086,124.)) ;
#23711 = CARTESIAN_POINT('',(63.0000000000011,386.45,128.263)) ;
#23712 = CARTESIAN_POINT('',(63.0000000000011,385.343736383857,126.421868161583)) ;
#23713 = CARTESIAN_POINT('Origin',(63.0000000000011,386.45,124.)) ;
#23714 = CARTESIAN_POINT('Origin',(63.0000000000011,405.45,124.)) ;
#23715 = CARTESIAN_POINT('',(63.0000000000011,409.45,128.263)) ;
#23716 = CARTESIAN_POINT('Origin',(63.0000000000011,409.45,124.)) ;
#23717 = CARTESIAN_POINT('',(63.0000000000011,405.45,128.263)) ;
#23718 = CARTESIAN_POINT('Origin',(63.0000000000005,228.556263616143,124.)) ;
#23719 = CARTESIAN_POINT('',(63.0000000000005,230.011468818915,124.)) ;
#23720 = CARTESIAN_POINT('',(63.0000000000005,227.45,119.737)) ;
#23721 = CARTESIAN_POINT('',(63.0000000000005,228.556263616143,121.578131838417)) ;
#23722 = CARTESIAN_POINT('Origin',(63.0000000000005,227.45,124.)) ;
#23723 = CARTESIAN_POINT('Origin',(63.0000000000005,208.45,124.)) ;
#23724 = CARTESIAN_POINT('',(63.0000000000005,209.449999999999,119.737)) ;
#23725 = CARTESIAN_POINT('Origin',(63.0000000000005,209.449999999999,124.)) ;
#23726 = CARTESIAN_POINT('',(63.0000000000005,208.45,119.737)) ;
#23727 = CARTESIAN_POINT('Origin',(63.0000000000005,228.556263616143,54.)) ;
#23728 = CARTESIAN_POINT('',(63.0000000000005,230.011468818915,54.)) ;
#23729 = CARTESIAN_POINT('',(63.0000000000005,227.45,49.737)) ;
#23730 = CARTESIAN_POINT('',(63.0000000000005,228.556263616143,51.5781318384169)) ;
#23731 = CARTESIAN_POINT('Origin',(63.0000000000005,227.45,54.)) ;
#23732 = CARTESIAN_POINT('Origin',(63.0000000000005,208.45,54.)) ;
#23733 = CARTESIAN_POINT('',(63.0000000000005,209.449999999999,49.737)) ;
#23734 = CARTESIAN_POINT('Origin',(63.0000000000005,209.449999999999,54.)) ;
#23735 = CARTESIAN_POINT('',(63.0000000000005,208.45,49.737)) ;
#23736 = CARTESIAN_POINT('Origin',(63.,379.45,138.893736383857)) ;
#23737 = CARTESIAN_POINT('',(63.,379.45,137.438531181086)) ;
#23738 = CARTESIAN_POINT('',(58.737,379.45,140.)) ;
#23739 = CARTESIAN_POINT('',(60.5781318384169,379.45,138.893736383857)) ;
#23740 = CARTESIAN_POINT('Origin',(63.,379.45,140.)) ;
#23741 = CARTESIAN_POINT('Origin',(63.,379.45,159.)) ;
#23742 = CARTESIAN_POINT('',(58.737,379.45,154.)) ;
#23743 = CARTESIAN_POINT('Origin',(63.,379.45,154.)) ;
#23744 = CARTESIAN_POINT('',(58.737,379.45,159.)) ;
#23745 = CARTESIAN_POINT('Origin',(63.,239.45,138.893736383857)) ;
#23746 = CARTESIAN_POINT('',(63.,239.45,137.438531181086)) ;
#23747 = CARTESIAN_POINT('',(58.737,239.45,140.)) ;
#23748 = CARTESIAN_POINT('',(60.5781318384169,239.45,138.893736383857)) ;
#23749 = CARTESIAN_POINT('Origin',(63.,239.45,140.)) ;
#23750 = CARTESIAN_POINT('Origin',(63.,239.45,159.)) ;
#23751 = CARTESIAN_POINT('',(58.737,239.45,154.)) ;
#23752 = CARTESIAN_POINT('Origin',(63.,239.45,154.)) ;
#23753 = CARTESIAN_POINT('',(58.737,239.45,159.)) ;
#23754 = CARTESIAN_POINT('Origin',(63.,309.45,154.)) ;
#23755 = CARTESIAN_POINT('',(51.0000000000001,209.449999999999,154.)) ;
#23756 = CARTESIAN_POINT('',(75.,209.449999999999,154.)) ;
#23757 = CARTESIAN_POINT('',(68.9999999999998,209.449999999999,154.)) ;
#23758 = CARTESIAN_POINT('',(75.0000000000001,409.45,154.)) ;
#23759 = CARTESIAN_POINT('',(75.0000000000001,359.45,154.)) ;
#23760 = CARTESIAN_POINT('',(50.9999999999999,409.45,154.)) ;
#23761 = CARTESIAN_POINT('',(56.9999999999999,409.45,154.)) ;
#23762 = CARTESIAN_POINT('',(51.0000000000001,259.449999999999,154.)) ;
#23763 = CARTESIAN_POINT('Origin',(63.,379.45,39.1062636161425)) ;
#23764 = CARTESIAN_POINT('',(63.,379.45,40.5614688189145)) ;
#23765 = CARTESIAN_POINT('',(58.737,379.45,38.)) ;
#23766 = CARTESIAN_POINT('',(60.5781318384169,379.45,39.1062636161425)) ;
#23767 = CARTESIAN_POINT('Origin',(63.,379.45,38.)) ;
#23768 = CARTESIAN_POINT('Origin',(63.,379.45,19.)) ;
#23769 = CARTESIAN_POINT('',(58.737,379.45,24.)) ;
#23770 = CARTESIAN_POINT('',(58.737,379.45,19.)) ;
#23771 = CARTESIAN_POINT('Origin',(63.,379.45,24.)) ;
#23772 = CARTESIAN_POINT('Origin',(63.,239.45,39.1062636161425)) ;
#23773 = CARTESIAN_POINT('',(63.,239.45,40.5614688189145)) ;
#23774 = CARTESIAN_POINT('',(58.737,239.45,38.)) ;
#23775 = CARTESIAN_POINT('',(60.5781318384169,239.45,39.1062636161425)) ;
#23776 = CARTESIAN_POINT('Origin',(63.,239.45,38.)) ;
#23777 = CARTESIAN_POINT('Origin',(63.,239.45,19.)) ;
#23778 = CARTESIAN_POINT('',(58.737,239.45,24.)) ;
#23779 = CARTESIAN_POINT('',(58.737,239.45,19.)) ;
#23780 = CARTESIAN_POINT('Origin',(63.,239.45,24.)) ;
#23781 = CARTESIAN_POINT('Origin',(75.0000000000001,409.45,24.)) ;
#23782 = CARTESIAN_POINT('',(75.,209.449999999999,24.)) ;
#23783 = CARTESIAN_POINT('',(75.0000000000001,409.45,24.)) ;
#23784 = CARTESIAN_POINT('',(75.0000000000001,359.45,24.)) ;
#23785 = CARTESIAN_POINT('',(75.0000000000001,409.45,24.)) ;
#23786 = CARTESIAN_POINT('',(75.,209.449999999999,24.)) ;
#23787 = CARTESIAN_POINT('Origin',(50.9999999999999,409.45,24.)) ;
#23788 = CARTESIAN_POINT('',(50.9999999999999,409.45,24.)) ;
#23789 = CARTESIAN_POINT('',(56.9999999999999,409.45,24.)) ;
#23790 = CARTESIAN_POINT('',(50.9999999999999,409.45,24.)) ;
#23791 = CARTESIAN_POINT('Origin',(51.0000000000001,209.449999999999,24.)) ;
#23792 = CARTESIAN_POINT('',(51.0000000000001,209.449999999999,24.)) ;
#23793 = CARTESIAN_POINT('',(51.0000000000001,259.449999999999,24.)) ;
#23794 = CARTESIAN_POINT('',(51.0000000000001,209.449999999999,24.)) ;
#23795 = CARTESIAN_POINT('Origin',(75.,209.449999999999,24.)) ;
#23796 = CARTESIAN_POINT('',(68.9999999999998,209.449999999999,24.)) ;
#23797 = CARTESIAN_POINT('Origin',(63.,309.45,24.)) ;
#23798 = CARTESIAN_POINT('',(0.,0.,0.)) ;
#23799 = CARTESIAN_POINT('Origin',(0.,0.,-328.125)) ;
#23800 = CARTESIAN_POINT('',(-3.75195406107394E-8,-19.425,-318.731323220285)) ;
#23801 = CARTESIAN_POINT('',(9.76712332682731E-9,-19.425,-318.518971385864)) ;
#23802 = CARTESIAN_POINT('',(-2.37887640734373E-15,-19.425,-328.125)) ;
#23803 = CARTESIAN_POINT('',(17.5361854501357,8.35622174666851,-318.250211755085)) ;
#23804 = CARTESIAN_POINT('Ctrl Pts',(17.5359434890344,8.35591472846589,-318.250416135478)) ;
#23805 = CARTESIAN_POINT('Ctrl Pts',(17.8361640444519,7.72586393628701,-318.258588076908)) ;
#23806 = CARTESIAN_POINT('Ctrl Pts',(18.1022112467557,7.08008972097568,-318.266685027288)) ;
#23807 = CARTESIAN_POINT('Ctrl Pts',(18.3886374715729,6.26235086001032,-318.277016532212)) ;
#23808 = CARTESIAN_POINT('Ctrl Pts',(18.4422758795157,6.10258032632359,-318.279037530685)) ;
#23809 = CARTESIAN_POINT('Ctrl Pts',(18.5317424236186,5.82413163966269,-318.282568096761)) ;
#23810 = CARTESIAN_POINT('Ctrl Pts',(18.5685261696438,5.70577097810744,-318.284071416777)) ;
#23811 = CARTESIAN_POINT('Ctrl Pts',(18.6384663337505,5.47287970534842,-318.287035700646)) ;
#23812 = CARTESIAN_POINT('Ctrl Pts',(18.6717060340157,5.35837972543229,-318.288496034413)) ;
#23813 = CARTESIAN_POINT('Ctrl Pts',(18.7405266390085,5.11289615809773,-318.291633941726)) ;
#23814 = CARTESIAN_POINT('Ctrl Pts',(18.7757930869953,4.98183096105143,-318.293313533209)) ;
#23815 = CARTESIAN_POINT('Ctrl Pts',(18.8670348664502,4.62799901878173,-318.297859564765)) ;
#23816 = CARTESIAN_POINT('Ctrl Pts',(18.9204374156704,4.40459161454828,-318.300742488007)) ;
#23817 = CARTESIAN_POINT('Ctrl Pts',(19.1395387183558,3.41032516101798,-318.313619447152)) ;
#23818 = CARTESIAN_POINT('Ctrl Pts',(19.2621762184986,2.63074481189291,-318.323872053442)) ;
#23819 = CARTESIAN_POINT('Ctrl Pts',(19.3564723693809,1.64291578597717,-318.336600535357)) ;
#23820 = CARTESIAN_POINT('Ctrl Pts',(19.3726502454238,1.43965881836873,-318.339203483527)) ;
#23821 = CARTESIAN_POINT('Ctrl Pts',(19.3923133935744,1.13130489355929,-318.343111699114)) ;
#23822 = CARTESIAN_POINT('Ctrl Pts',(19.3981501515743,1.02637237507932,-318.344434517958)) ;
#23823 = CARTESIAN_POINT('Ctrl Pts',(19.4034726746178,0.914288693855463,-318.345838106023)) ;
#23824 = CARTESIAN_POINT('Ctrl Pts',(19.4038063482354,0.907179613167534,-318.345927090444)) ;
#23825 = CARTESIAN_POINT('Ctrl Pts',(19.4043797672481,0.894817578832296,-318.346081755098)) ;
#23826 = CARTESIAN_POINT('Ctrl Pts',(19.404621286705,0.889564708458132,-318.346147452837)) ;
#23827 = CARTESIAN_POINT('Ctrl Pts',(19.4050409056885,0.88035681542777,-318.346262576645)) ;
#23828 = CARTESIAN_POINT('Ctrl Pts',(19.405219929107,0.876401835293624,-318.346312011936)) ;
#23829 = CARTESIAN_POINT('Ctrl Pts',(19.4055338043819,0.86942046457019,-318.346399252918)) ;
#23830 = CARTESIAN_POINT('Ctrl Pts',(19.4056691573984,0.866394096712561,-318.346437063653)) ;
#23831 = CARTESIAN_POINT('Ctrl Pts',(19.4059082495824,0.861020052690169,-318.346504192271)) ;
#23832 = CARTESIAN_POINT('Ctrl Pts',(19.4060122706947,0.858672389210068,-318.346533513009)) ;
#23833 = CARTESIAN_POINT('Ctrl Pts',(19.4064760354284,0.84816250658705,-318.346664753903)) ;
#23834 = CARTESIAN_POINT('Ctrl Pts',(19.4068310555369,0.840000079229425,-318.346766625959)) ;
#23835 = CARTESIAN_POINT('Ctrl Pts',(19.407500239987,0.824387673207127,-318.346961371011)) ;
#23836 = CARTESIAN_POINT('Ctrl Pts',(19.4078152645099,0.816937732942163,-318.347054252894)) ;
#23837 = CARTESIAN_POINT('Ctrl Pts',(19.4084142279498,0.802577095756465,-318.347233202422)) ;
#23838 = CARTESIAN_POINT('Ctrl Pts',(19.40869876572,0.795666424998969,-318.347319276348)) ;
#23839 = CARTESIAN_POINT('Ctrl Pts',(19.4092447198009,0.782232084142982,-318.347486523887)) ;
#23840 = CARTESIAN_POINT('Ctrl Pts',(19.4095065381935,0.775708431318012,-318.347567701776)) ;
#23841 = CARTESIAN_POINT('Ctrl Pts',(19.4100137933671,0.7629082489646,-318.347726909552)) ;
#23842 = CARTESIAN_POINT('Ctrl Pts',(19.4102594748316,0.756631729946837,-318.347804942071)) ;
#23843 = CARTESIAN_POINT('Ctrl Pts',(19.4107404722003,0.744189087075131,-318.347959565718)) ;
#23844 = CARTESIAN_POINT('Ctrl Pts',(19.4109758944565,0.738022967989215,-318.348036158001)) ;
#23845 = CARTESIAN_POINT('Ctrl Pts',(19.4137091817322,0.665527346705117,-318.34893626181)) ;
#23846 = CARTESIAN_POINT('Ctrl Pts',(19.4158699937519,0.599185489183012,-318.349756037201)) ;
#23847 = CARTESIAN_POINT('Ctrl Pts',(19.419423420364,0.469690434818989,-318.351347653963)) ;
#23848 = CARTESIAN_POINT('Ctrl Pts',(19.4208481061199,0.406538970002123,-318.352119923812)) ;
#23849 = CARTESIAN_POINT('Ctrl Pts',(19.4240711038294,0.224243411802522,-318.35433919791)) ;
#23850 = CARTESIAN_POINT('Ctrl Pts',(19.4250812068003,0.105088182032955,-318.355777493511)) ;
#23851 = CARTESIAN_POINT('Ctrl Pts',(19.4246389057749,-0.505599037037676,
-318.363101020354)) ;
#23852 = CARTESIAN_POINT('Ctrl Pts',(19.4056265118234,-0.996939939709481,
-318.368838635994)) ;
#23853 = CARTESIAN_POINT('Ctrl Pts',(19.3340458606877,-1.92925034319463,-318.379759743753)) ;
#23854 = CARTESIAN_POINT('Ctrl Pts',(19.2849577239435,-2.37017749952631,-318.384938958872)) ;
#23855 = CARTESIAN_POINT('Ctrl Pts',(19.1907765657816,-3.01461168345414,-318.392653256337)) ;
#23856 = CARTESIAN_POINT('Ctrl Pts',(19.1574365658758,-3.21969142248208,-318.395129309198)) ;
#23857 = CARTESIAN_POINT('Ctrl Pts',(19.091327592596,-3.58884584990186,-318.399634297491)) ;
#23858 = CARTESIAN_POINT('Ctrl Pts',(19.0597164221864,-3.75310719037178,-318.401656097661)) ;
#23859 = CARTESIAN_POINT('Ctrl Pts',(19.0042060176744,-4.02274123847243,-318.405006281912)) ;
#23860 = CARTESIAN_POINT('Ctrl Pts',(18.9815421653682,-4.12835929006944,-318.406326541001)) ;
#23861 = CARTESIAN_POINT('Ctrl Pts',(18.930433014569,-4.35721543798472,-318.409205254106)) ;
#23862 = CARTESIAN_POINT('Ctrl Pts',(18.9016626882452,-4.48037588405983,-318.410765808215)) ;
#23863 = CARTESIAN_POINT('Ctrl Pts',(18.834800682221,-4.7544865949519,-318.414264842707)) ;
#23864 = CARTESIAN_POINT('Ctrl Pts',(18.7960929691439,-4.90527761966604,-318.416207281625)) ;
#23865 = CARTESIAN_POINT('Ctrl Pts',(18.6123990748495,-5.58675833213696,-318.425064621203)) ;
#23866 = CARTESIAN_POINT('Ctrl Pts',(18.4467215570834,-6.11160604010705,-318.432111733988)) ;
#23867 = CARTESIAN_POINT('Ctrl Pts',(18.0783812130823,-7.12621109985498,-318.446026883841)) ;
#23868 = CARTESIAN_POINT('Ctrl Pts',(17.877512153499,-7.61612181226138,-318.452884693635)) ;
#23869 = CARTESIAN_POINT('Ctrl Pts',(17.5869727219576,-8.24967559074662,-318.461730250758)) ;
#23870 = CARTESIAN_POINT('Ctrl Pts',(17.5150853350643,-8.40122269285768,-318.463843721782)) ;
#23871 = CARTESIAN_POINT('Ctrl Pts',(17.4064633805098,-8.62275472449833,-318.466919799804)) ;
#23872 = CARTESIAN_POINT('Ctrl Pts',(17.3712500550719,-8.69347674990476,-318.467899764193)) ;
#23873 = CARTESIAN_POINT('Ctrl Pts',(17.3056289315658,-8.82327869990995,-318.469693205862)) ;
#23874 = CARTESIAN_POINT('Ctrl Pts',(17.2753476360861,-8.88242105382913,-318.470508222507)) ;
#23875 = CARTESIAN_POINT('Ctrl Pts',(17.1994145935773,-9.02886862829517,-318.472521891028)) ;
#23876 = CARTESIAN_POINT('Ctrl Pts',(17.1534009480539,-9.11598414992153,-318.473715902887)) ;
#23877 = CARTESIAN_POINT('Ctrl Pts',(16.9577496167712,-9.47967492743655,-318.478691632871)) ;
#23878 = CARTESIAN_POINT('Ctrl Pts',(16.8020697987869,-9.75294622576759,-318.482408942612)) ;
#23879 = CARTESIAN_POINT('Ctrl Pts',(16.5426809640306,-10.1836035601808,-318.488311133754)) ;
#23880 = CARTESIAN_POINT('Ctrl Pts',(16.4431973381435,-10.3434682917478,-318.490511919025)) ;
#23881 = CARTESIAN_POINT('Ctrl Pts',(16.0911232605261,-10.8913126181413,-318.498118923141)) ;
#23882 = CARTESIAN_POINT('Ctrl Pts',(15.8269989726428,-11.2716920415504,-318.503518932264)) ;
#23883 = CARTESIAN_POINT('Ctrl Pts',(15.4633360303461,-11.7574040645809,-318.510701428245)) ;
#23884 = CARTESIAN_POINT('Ctrl Pts',(15.3758574189166,-11.8715761424008,-318.512411095488)) ;
#23885 = CARTESIAN_POINT('Ctrl Pts',(15.1547786925007,-12.1535722008268,-318.516692273301)) ;
#23886 = CARTESIAN_POINT('Ctrl Pts',(15.0196516279904,-12.3201744801037,-318.519274310003)) ;
#23887 = CARTESIAN_POINT('Ctrl Pts',(14.7964408248314,-12.5862464781808,-318.523491569587)) ;
#23888 = CARTESIAN_POINT('Ctrl Pts',(14.7100472522316,-12.687110438287,-318.525112693334)) ;
#23889 = CARTESIAN_POINT('Ctrl Pts',(14.5395638958167,-12.8820661524688,-318.528291319787)) ;
#23890 = CARTESIAN_POINT('Ctrl Pts',(14.4555780735056,-12.9762401776811,-318.529847886303)) ;
#23891 = CARTESIAN_POINT('Ctrl Pts',(14.267065028334,-13.1835198982721,-318.533321653275)) ;
#23892 = CARTESIAN_POINT('Ctrl Pts',(14.162098234109,-13.2962143090171,-318.535242593247)) ;
#23893 = CARTESIAN_POINT('Ctrl Pts',(13.6772898161035,-13.8044593913075,-318.54405376234)) ;
#23894 = CARTESIAN_POINT('Ctrl Pts',(13.2821443593885,-14.1850623421511,-318.551075665434)) ;
#23895 = CARTESIAN_POINT('Ctrl Pts',(12.4755358261488,-14.8986926287413,-318.564956089729)) ;
#23896 = CARTESIAN_POINT('Ctrl Pts',(12.0655115682462,-15.2326447829125,-318.57180454189)) ;
#23897 = CARTESIAN_POINT('Ctrl Pts',(11.505796574595,-15.6517214019043,-318.580680703614)) ;
#23898 = CARTESIAN_POINT('Ctrl Pts',(11.3678723738325,-15.7521812937659,-318.582831255241)) ;
#23899 = CARTESIAN_POINT('Ctrl Pts',(11.1637120153642,-15.8968075622017,-318.585950979884)) ;
#23900 = CARTESIAN_POINT('Ctrl Pts',(11.0984995132176,-15.942404624404,-318.586938120349)) ;
#23901 = CARTESIAN_POINT('Ctrl Pts',(10.9783446230289,-16.0253232590335,-318.588738433228)) ;
#23902 = CARTESIAN_POINT('Ctrl Pts',(10.9234876020961,-16.0627661010884,-318.589553224272)) ;
#23903 = CARTESIAN_POINT('Ctrl Pts',(10.787308577303,-16.1546953073578,-318.591559071098)) ;
#23904 = CARTESIAN_POINT('Ctrl Pts',(10.7057646774855,-16.2088497285502,-318.592745594856)) ;
#23905 = CARTESIAN_POINT('Ctrl Pts',(10.3667465054018,-16.4303219284505,-318.597625436801)) ;
#23906 = CARTESIAN_POINT('Ctrl Pts',(10.1057316969341,-16.5921396875327,-318.601257392169)) ;
#23907 = CARTESIAN_POINT('Ctrl Pts',(9.47635769564765,-16.9619613836531,-318.609831168774)) ;
#23908 = CARTESIAN_POINT('Ctrl Pts',(9.10482459956954,-17.1642552598683,-318.614749280166)) ;
#23909 = CARTESIAN_POINT('Ctrl Pts',(8.29507997240903,-17.5714537898474,-318.62536471977)) ;
#23910 = CARTESIAN_POINT('Ctrl Pts',(7.85521804294205,-17.7724474425252,-318.631070562401)) ;
#23911 = CARTESIAN_POINT('Ctrl Pts',(7.25416743233182,-18.0204186077575,-318.638897510944)) ;
#23912 = CARTESIAN_POINT('Ctrl Pts',(7.09920454975442,-18.0820277233927,-318.64091754488)) ;
#23913 = CARTESIAN_POINT('Ctrl Pts',(6.82669164795596,-18.1863283928655,-318.644476427079)) ;
#23914 = CARTESIAN_POINT('Ctrl Pts',(6.70948677342134,-18.2298943074088,-318.646009128314)) ;
#23915 = CARTESIAN_POINT('Ctrl Pts',(6.46080727354764,-18.3196071804636,-318.649266252274)) ;
#23916 = CARTESIAN_POINT('Ctrl Pts',(6.32924021215035,-18.3654772914714,-318.650992475406)) ;
#23917 = CARTESIAN_POINT('Ctrl Pts',(5.96577894148348,-18.4878264385583,-318.655769724322)) ;
#23918 = CARTESIAN_POINT('Ctrl Pts',(5.73291888797409,-18.5613546244059,-318.658840020083)) ;
#23919 = CARTESIAN_POINT('Ctrl Pts',(5.29162843691991,-18.6916003365817,-318.664671321594)) ;
#23920 = CARTESIAN_POINT('Ctrl Pts',(5.08351716581555,-18.7492695245115,-318.667426575661)) ;
#23921 = CARTESIAN_POINT('Ctrl Pts',(4.30906359933547,-18.9500339164173,-318.677682130067)) ;
#23922 = CARTESIAN_POINT('Ctrl Pts',(3.73731666048703,-19.0710324107846,-318.685266965197)) ;
#23923 = CARTESIAN_POINT('Ctrl Pts',(2.89879228028493,-19.2093270458025,-318.696150089002)) ;
#23924 = CARTESIAN_POINT('Ctrl Pts',(2.6357350103506,-19.247185343998,-318.699528560866)) ;
#23925 = CARTESIAN_POINT('Ctrl Pts',(2.28062245314534,-19.290875030694,-318.704007561273)) ;
#23926 = CARTESIAN_POINT('Ctrl Pts',(2.18918235324355,-19.3014657184243,-318.705153577779)) ;
#23927 = CARTESIAN_POINT('Ctrl Pts',(2.03837205828987,-19.3178472436615,-318.707029707136)) ;
#23928 = CARTESIAN_POINT('Ctrl Pts',(1.97904441178138,-19.324015266403,-318.707764148417)) ;
#23929 = CARTESIAN_POINT('Ctrl Pts',(1.84031778419984,-19.3377924643283,-318.709472733874)) ;
#23930 = CARTESIAN_POINT('Ctrl Pts',(1.7608985974158,-19.3451860443713,-318.710444365842)) ;
#23931 = CARTESIAN_POINT('Ctrl Pts',(1.51018394198892,-19.3669697720635,-318.713494019274)) ;
#23932 = CARTESIAN_POINT('Ctrl Pts',(1.33874158295967,-19.3795754553743,-318.715553508113)) ;
#23933 = CARTESIAN_POINT('Ctrl Pts',(0.778478482824912,-19.4132998882475,
-318.722227322384)) ;
#23934 = CARTESIAN_POINT('Ctrl Pts',(0.389251165707532,-19.4250000007518,
-318.726776673746)) ;
#23935 = CARTESIAN_POINT('Ctrl Pts',(-3.75195408075513E-8,-19.425,-318.731323220285)) ;
#23936 = CARTESIAN_POINT('',(17.5359809117572,-8.35583619169778,-318.25)) ;
#23937 = CARTESIAN_POINT('Origin',(0.,0.,-318.25)) ;
#23938 = CARTESIAN_POINT('Ctrl Pts',(17.5359809117572,-8.35583619169781,-318.25)) ;
#23939 = CARTESIAN_POINT('Ctrl Pts',(17.5198792059969,-8.38962804668179,-318.250460037632)) ;
#23940 = CARTESIAN_POINT('Ctrl Pts',(17.5036798636303,-8.42337327821063,-318.250921300259)) ;
#23941 = CARTESIAN_POINT('Ctrl Pts',(17.4683361610756,-8.49645636247359,-318.251924139912)) ;
#23942 = CARTESIAN_POINT('Ctrl Pts',(17.4491562426748,-8.53577678780645,-318.252466131549)) ;
#23943 = CARTESIAN_POINT('Ctrl Pts',(17.3747570462932,-8.68700262016844,-318.254559570065)) ;
#23944 = CARTESIAN_POINT('Ctrl Pts',(17.318592799099,-8.79843965357187,-318.2561211156)) ;
#23945 = CARTESIAN_POINT('Ctrl Pts',(16.9574819793595,-9.49807307940423,-318.266027876778)) ;
#23946 = CARTESIAN_POINT('Ctrl Pts',(16.6236830848865,-10.0708862132213,-318.274585351295)) ;
#23947 = CARTESIAN_POINT('Ctrl Pts',(16.0460907785041,-10.9548319601542,-318.288061387794)) ;
#23948 = CARTESIAN_POINT('Ctrl Pts',(15.8209570947634,-11.2775303285937,-318.293046457475)) ;
#23949 = CARTESIAN_POINT('Ctrl Pts',(15.5094952734983,-11.6962682575552,-318.299568971753)) ;
#23950 = CARTESIAN_POINT('Ctrl Pts',(15.4317888945073,-11.798602728926,-318.301167631723)) ;
#23951 = CARTESIAN_POINT('Ctrl Pts',(15.2792878999389,-11.9953529513281,-318.304249729324)) ;
#23952 = CARTESIAN_POINT('Ctrl Pts',(15.2046191254482,-12.0898589093431,-318.305734047246)) ;
#23953 = CARTESIAN_POINT('Ctrl Pts',(15.05458867922,-12.2761593510363,-318.308667868868)) ;
#23954 = CARTESIAN_POINT('Ctrl Pts',(14.9792544271018,-12.3679693386124,-318.310117507856)) ;
#23955 = CARTESIAN_POINT('Ctrl Pts',(14.774242130377,-12.6131972834278,-318.314000571655)) ;
#23956 = CARTESIAN_POINT('Ctrl Pts',(14.6430183721534,-12.76530412388,-318.316420816178)) ;
#23957 = CARTESIAN_POINT('Ctrl Pts',(14.11937145961,-13.3535835191081,-318.325837903387)) ;
#23958 = CARTESIAN_POINT('Ctrl Pts',(13.7096294855631,-13.7739211730652,-318.3326820739)) ;
#23959 = CARTESIAN_POINT('Ctrl Pts',(12.9412265317647,-14.4938851277888,-318.34489605397)) ;
#23960 = CARTESIAN_POINT('Ctrl Pts',(12.58959139021,-14.8003458594248,-318.350279025558)) ;
#23961 = CARTESIAN_POINT('Ctrl Pts',(12.097352808699,-15.1990998134531,-318.35772399782)) ;
#23962 = CARTESIAN_POINT('Ctrl Pts',(11.9660813985514,-15.302662381079,-318.359701577825)) ;
#23963 = CARTESIAN_POINT('Ctrl Pts',(11.7781452047365,-15.4470317870343,-318.362532484224)) ;
#23964 = CARTESIAN_POINT('Ctrl Pts',(11.7225721416481,-15.4892478146926,-318.363369557972)) ;
#23965 = CARTESIAN_POINT('Ctrl Pts',(11.6116381886808,-15.5725797064156,-318.365041613266)) ;
#23966 = CARTESIAN_POINT('Ctrl Pts',(11.5562834452924,-15.6137020932165,-318.365876489156)) ;
#23967 = CARTESIAN_POINT('Ctrl Pts',(11.4523687553509,-15.6900437593506,-318.367445857157)) ;
#23968 = CARTESIAN_POINT('Ctrl Pts',(11.4038623722044,-15.725334536324,-318.368179319703)) ;
#23969 = CARTESIAN_POINT('Ctrl Pts',(11.2982164897377,-15.801451220993,-318.369779202226)) ;
#23970 = CARTESIAN_POINT('Ctrl Pts',(11.2410176229562,-15.8421930086534,-318.370646780637)) ;
#23971 = CARTESIAN_POINT('Ctrl Pts',(11.0868475315197,-15.9507504192236,-318.372987401497)) ;
#23972 = CARTESIAN_POINT('Ctrl Pts',(10.9894755363776,-16.017991587524,-318.374468024141)) ;
#23973 = CARTESIAN_POINT('Ctrl Pts',(10.5266240762749,-16.3314110326398,-318.381505375013)) ;
#23974 = CARTESIAN_POINT('Ctrl Pts',(10.1534516232657,-16.5659958926339,-318.387174199619)) ;
#23975 = CARTESIAN_POINT('Ctrl Pts',(9.3715428916209,-17.0211688971527,-318.398831704899)) ;
#23976 = CARTESIAN_POINT('Ctrl Pts',(8.962220594579,-17.2402033077897,-318.404816939237)) ;
#23977 = CARTESIAN_POINT('Ctrl Pts',(8.35539662660272,-17.5374672915959,-318.413419660947)) ;
#23978 = CARTESIAN_POINT('Ctrl Pts',(8.16383713678824,-17.6274551535937,-318.416098111544)) ;
#23979 = CARTESIAN_POINT('Ctrl Pts',(7.86067880717831,-17.7638663493227,-318.420274185247)) ;
#23980 = CARTESIAN_POINT('Ctrl Pts',(7.75005213757438,-17.8124089020029,-318.421785206438)) ;
#23981 = CARTESIAN_POINT('Ctrl Pts',(7.60390051266738,-17.8749203541796,-318.423764273037)) ;
#23982 = CARTESIAN_POINT('Ctrl Pts',(7.56877710392898,-17.889820955705,-318.424238590433)) ;
#23983 = CARTESIAN_POINT('Ctrl Pts',(7.42632280512932,-17.9497605273382,-318.426157089413)) ;
#23984 = CARTESIAN_POINT('Ctrl Pts',(7.31863194284603,-17.9939378658013,-318.427595353699)) ;
#23985 = CARTESIAN_POINT('Ctrl Pts',(7.09350300785435,-18.0839356773858,-318.430577222018)) ;
#23986 = CARTESIAN_POINT('Ctrl Pts',(6.97600279352915,-18.1295863046937,-318.432119592422)) ;
#23987 = CARTESIAN_POINT('Ctrl Pts',(6.68748025904288,-18.2384614516959,-318.435873898971)) ;
#23988 = CARTESIAN_POINT('Ctrl Pts',(6.51599603297857,-18.300427977921,-318.43807711471)) ;
#23989 = CARTESIAN_POINT('Ctrl Pts',(5.68044058268022,-18.5891257963158,-318.448687554087)) ;
#23990 = CARTESIAN_POINT('Ctrl Pts',(5.00528602135639,-18.7821754793875,-318.456860865535)) ;
#23991 = CARTESIAN_POINT('Ctrl Pts',(3.89849440260567,-19.0347136373014,-318.470116949714)) ;
#23992 = CARTESIAN_POINT('Ctrl Pts',(3.47270829007892,-19.1169787680542,-318.475189009329)) ;
#23993 = CARTESIAN_POINT('Ctrl Pts',(2.92407062282469,-19.2040441445099,-318.481844724358)) ;
#23994 = CARTESIAN_POINT('Ctrl Pts',(2.80343553201976,-19.2220251186595,-318.483315786842)) ;
#23995 = CARTESIAN_POINT('Ctrl Pts',(2.61309447505108,-19.2485659928119,-318.485653829477)) ;
#23996 = CARTESIAN_POINT('Ctrl Pts',(2.54349761241096,-19.2578860576797,-318.486512290162)) ;
#23997 = CARTESIAN_POINT('Ctrl Pts',(2.40300201308118,-19.2759256267124,-318.488253724751)) ;
#23998 = CARTESIAN_POINT('Ctrl Pts',(2.33210269302313,-19.2846318205587,-318.489136781985)) ;
#23999 = CARTESIAN_POINT('Ctrl Pts',(2.13717099809704,-19.3074780543583,-318.491574837144)) ;
#24000 = CARTESIAN_POINT('Ctrl Pts',(2.01304789948299,-19.320813822877,-318.493138550738)) ;
#24001 = CARTESIAN_POINT('Ctrl Pts',(1.58957877219779,-19.362186222767,-318.498502211751)) ;
#24002 = CARTESIAN_POINT('Ctrl Pts',(1.28971446400269,-19.3844693528092,-318.502348628073)) ;
#24003 = CARTESIAN_POINT('Ctrl Pts',(0.934551723804926,-19.4025838549164,
-318.506921303889)) ;
#24004 = CARTESIAN_POINT('Ctrl Pts',(0.879637174321103,-19.4051510071819,
-318.507628821915)) ;
#24005 = CARTESIAN_POINT('Ctrl Pts',(0.735946097340056,-19.4112570958334,
-318.509480978891)) ;
#24006 = CARTESIAN_POINT('Ctrl Pts',(0.647154892522766,-19.4144201366001,
-318.51062632345)) ;
#24007 = CARTESIAN_POINT('Ctrl Pts',(0.372263752904269,-19.4223247735594,
-318.514172668865)) ;
#24008 = CARTESIAN_POINT('Ctrl Pts',(0.18612948495482,-19.4249999999064,-318.516574511693)) ;
#24009 = CARTESIAN_POINT('Ctrl Pts',(9.76712256212098E-9,-19.425,-318.518971385864)) ;
#24010 = CARTESIAN_POINT('Origin',(0.,0.,-328.125)) ;
#24011 = CARTESIAN_POINT('',(-0.000449417202212064,-19.4250824346375,-320.231292904519)) ;
#24012 = CARTESIAN_POINT('',(-0.000295851126506864,-19.4249999967644,-320.018354299106)) ;
#24013 = CARTESIAN_POINT('',(-2.37887640734373E-15,-19.425,-328.125)) ;
#24014 = CARTESIAN_POINT('Ctrl Pts',(-3.75195408769402E-8,-19.425,-318.731323220285)) ;
#24015 = CARTESIAN_POINT('Ctrl Pts',(-0.286007459534617,-19.4249999994476,
-318.734663854929)) ;
#24016 = CARTESIAN_POINT('Ctrl Pts',(-0.572027782392097,-19.4186833807807,
-318.738002522882)) ;
#24017 = CARTESIAN_POINT('Ctrl Pts',(-1.14627823685766,-19.393298418784,-318.744751765226)) ;
#24018 = CARTESIAN_POINT('Ctrl Pts',(-1.43438419233051,-19.3741198251488,
-318.748161338625)) ;
#24019 = CARTESIAN_POINT('Ctrl Pts',(-1.94585854290658,-19.3286002949899,
-318.754288319144)) ;
#24020 = CARTESIAN_POINT('Ctrl Pts',(-2.16939892445428,-19.3047886001703,
-318.756991228773)) ;
#24021 = CARTESIAN_POINT('Ctrl Pts',(-2.52608639503362,-19.2605202271534,
-318.761352659256)) ;
#24022 = CARTESIAN_POINT('Ctrl Pts',(-2.65952133422362,-19.2425491583177,
-318.762995115991)) ;
#24023 = CARTESIAN_POINT('Ctrl Pts',(-2.91804790595291,-19.2049902411333,
-318.76619964914)) ;
#24024 = CARTESIAN_POINT('Ctrl Pts',(-3.04315622115263,-19.1855636849058,
-318.767760595865)) ;
#24025 = CARTESIAN_POINT('Ctrl Pts',(-3.34410870049375,-19.13581459057,-318.771540576724)) ;
#24026 = CARTESIAN_POINT('Ctrl Pts',(-3.51974228862563,-19.1042894956005,
-318.773767293134)) ;
#24027 = CARTESIAN_POINT('Ctrl Pts',(-4.41580901212489,-18.9306748653615,
-318.785231997198)) ;
#24028 = CARTESIAN_POINT('Ctrl Pts',(-5.12819980772471,-18.7502367586556,
-318.794718262101)) ;
#24029 = CARTESIAN_POINT('Ctrl Pts',(-6.21820311983242,-18.407371765267,-318.809451024768)) ;
#24030 = CARTESIAN_POINT('Ctrl Pts',(-6.60378877473305,-18.2725849320413,
-318.814700814828)) ;
#24031 = CARTESIAN_POINT('Ctrl Pts',(-7.09646490993294,-18.0827299214219,
-318.821351819026)) ;
#24032 = CARTESIAN_POINT('Ctrl Pts',(-7.20769100613827,-18.0386841552426,
-318.822849343208)) ;
#24033 = CARTESIAN_POINT('Ctrl Pts',(-7.38344274293308,-17.9672010350083,
-318.82520527028)) ;
#24034 = CARTESIAN_POINT('Ctrl Pts',(-7.44823886926803,-17.9404369384148,
-318.82607159725)) ;
#24035 = CARTESIAN_POINT('Ctrl Pts',(-7.57068731491574,-17.889081778305,-318.82770344851)) ;
#24036 = CARTESIAN_POINT('Ctrl Pts',(-7.62836824756348,-17.8645613207162,
-318.828469946132)) ;
#24037 = CARTESIAN_POINT('Ctrl Pts',(-7.79288254156359,-17.7936833985481,
-318.830651070199)) ;
#24038 = CARTESIAN_POINT('Ctrl Pts',(-7.89941913751624,-17.7466437543245,
-318.832057440686)) ;
#24039 = CARTESIAN_POINT('Ctrl Pts',(-8.32919216631633,-17.5522470329059,
-318.837717218088)) ;
#24040 = CARTESIAN_POINT('Ctrl Pts',(-8.64878179349487,-17.3969937795925,
-318.841895786816)) ;
#24041 = CARTESIAN_POINT('Ctrl Pts',(-9.58321805118889,-16.9109382977038,
-318.85422563345)) ;
#24042 = CARTESIAN_POINT('Ctrl Pts',(-10.1846887237055,-16.5556642431838,
-318.862326688989)) ;
#24043 = CARTESIAN_POINT('Ctrl Pts',(-10.9534643882013,-16.0437873841392,
-318.873345983863)) ;
#24044 = CARTESIAN_POINT('Ctrl Pts',(-11.1390100224788,-15.9155254769109,
-318.876057792405)) ;
#24045 = CARTESIAN_POINT('Ctrl Pts',(-11.4318026969099,-15.705498387101,-318.880430034651)) ;
#24046 = CARTESIAN_POINT('Ctrl Pts',(-11.540504887464,-15.6257972395733,-318.882074260238)) ;
#24047 = CARTESIAN_POINT('Ctrl Pts',(-11.7496542862082,-15.4690745761243,
-318.885280056272)) ;
#24048 = CARTESIAN_POINT('Ctrl Pts',(-11.8501956218692,-15.3921898299445,
-318.886840472017)) ;
#24049 = CARTESIAN_POINT('Ctrl Pts',(-12.0903676936717,-15.2047802985234,
-318.890615372731)) ;
#24050 = CARTESIAN_POINT('Ctrl Pts',(-12.2292439161095,-15.0933073910411,
-318.892837481342)) ;
#24051 = CARTESIAN_POINT('Ctrl Pts',(-12.6698705757445,-14.72955165818,-318.90001399427)) ;
#24052 = CARTESIAN_POINT('Ctrl Pts',(-12.9654982953675,-14.4700091632262,
-318.905024752178)) ;
#24053 = CARTESIAN_POINT('Ctrl Pts',(-13.6543603084029,-13.8271611091469,
-318.917123217825)) ;
#24054 = CARTESIAN_POINT('Ctrl Pts',(-14.0396227635746,-13.435807810924,-318.924246579844)) ;
#24055 = CARTESIAN_POINT('Ctrl Pts',(-14.4943566837919,-12.9329388101128,
-318.932924486614)) ;
#24056 = CARTESIAN_POINT('Ctrl Pts',(-14.5799644230022,-12.8363514837939,
-318.934570405797)) ;
#24057 = CARTESIAN_POINT('Ctrl Pts',(-14.7717783066041,-12.6155419555065,
-318.93828005332)) ;
#24058 = CARTESIAN_POINT('Ctrl Pts',(-14.8773922409784,-12.4908179645103,
-318.940338213387)) ;
#24059 = CARTESIAN_POINT('Ctrl Pts',(-15.0312891342176,-12.3043532871932,
-318.943351536856)) ;
#24060 = CARTESIAN_POINT('Ctrl Pts',(-15.0807924992862,-12.2436293829311,
-318.944323056544)) ;
#24061 = CARTESIAN_POINT('Ctrl Pts',(-15.1717600805074,-12.130654154376,-318.946111130847)) ;
#24062 = CARTESIAN_POINT('Ctrl Pts',(-15.2133250264288,-12.0784856577575,
-318.946929098896)) ;
#24063 = CARTESIAN_POINT('Ctrl Pts',(-15.3166239120342,-11.9474552520882,
-318.948965292312)) ;
#24064 = CARTESIAN_POINT('Ctrl Pts',(-15.3780182482045,-11.8683280145292,
-318.950178634034)) ;
#24065 = CARTESIAN_POINT('Ctrl Pts',(-15.6676038787213,-11.4890798474374,
-318.955925392695)) ;
#24066 = CARTESIAN_POINT('Ctrl Pts',(-15.8876381157418,-11.1828316396753,
-318.960364475648)) ;
#24067 = CARTESIAN_POINT('Ctrl Pts',(-16.2606980124245,-10.6303437739049,
-318.968170767709)) ;
#24068 = CARTESIAN_POINT('Ctrl Pts',(-16.417386715422,-10.386718544207,-318.971546590227)) ;
#24069 = CARTESIAN_POINT('Ctrl Pts',(-16.7564710752746,-9.83264365093919,
-318.979143420769)) ;
#24070 = CARTESIAN_POINT('Ctrl Pts',(-16.9358015468594,-9.52044271824114,
-318.983369685163)) ;
#24071 = CARTESIAN_POINT('Ctrl Pts',(-17.2294095101058,-8.97471617269769,
-318.990734379051)) ;
#24072 = CARTESIAN_POINT('Ctrl Pts',(-17.3478660158323,-8.74354772326497,
-318.993846875203)) ;
#24073 = CARTESIAN_POINT('Ctrl Pts',(-17.5233251881918,-8.38352654107101,
-318.998697116442)) ;
#24074 = CARTESIAN_POINT('Ctrl Pts',(-17.583621526928,-8.25631254541748,-319.00041140313)) ;
#24075 = CARTESIAN_POINT('Ctrl Pts',(-17.6947151141119,-8.01518775241271,
-319.003663016634)) ;
#24076 = CARTESIAN_POINT('Ctrl Pts',(-17.7458085444244,-7.90142118440228,
-319.005198129967)) ;
#24077 = CARTESIAN_POINT('Ctrl Pts',(-17.8603827240459,-7.63958802068494,
-319.008733909052)) ;
#24078 = CARTESIAN_POINT('Ctrl Pts',(-17.9231241475552,-7.49120797109105,
-319.010739625042)) ;
#24079 = CARTESIAN_POINT('Ctrl Pts',(-18.1466380638239,-6.94372205674883,
-319.0181469038)) ;
#24080 = CARTESIAN_POINT('Ctrl Pts',(-18.2959833775576,-6.54008712519531,
-319.02362366026)) ;
#24081 = CARTESIAN_POINT('Ctrl Pts',(-18.6052207054103,-5.61054354314534,
-319.036202366919)) ;
#24082 = CARTESIAN_POINT('Ctrl Pts',(-18.7564471686972,-5.08213784282851,
-319.043331739021)) ;
#24083 = CARTESIAN_POINT('Ctrl Pts',(-18.915303677657,-4.42250862607873,-319.0520162424)) ;
#24084 = CARTESIAN_POINT('Ctrl Pts',(-18.944281581646,-4.29668374092105,-319.053662866711)) ;
#24085 = CARTESIAN_POINT('Ctrl Pts',(-19.0070998763694,-4.01092274747163,
-319.0573737716)) ;
#24086 = CARTESIAN_POINT('Ctrl Pts',(-19.0401801607921,-3.85082933730122,
-319.05943248372)) ;
#24087 = CARTESIAN_POINT('Ctrl Pts',(-19.0861197738805,-3.61341873825023,
-319.062446363266)) ;
#24088 = CARTESIAN_POINT('Ctrl Pts',(-19.1005382664594,-3.53641074437951,
-319.063417899645)) ;
#24089 = CARTESIAN_POINT('Ctrl Pts',(-19.1263680184581,-3.39368821649319,
-319.065205913583)) ;
#24090 = CARTESIAN_POINT('Ctrl Pts',(-19.1379074354898,-3.32799823764049,
-319.066023805766)) ;
#24091 = CARTESIAN_POINT('Ctrl Pts',(-19.165922711895,-3.16355113880511,-319.068059572948)) ;
#24092 = CARTESIAN_POINT('Ctrl Pts',(-19.1819737961618,-3.06472356481236,
-319.06927256835)) ;
#24093 = CARTESIAN_POINT('Ctrl Pts',(-19.2545953664382,-2.59464926943222,
-319.075001102468)) ;
#24094 = CARTESIAN_POINT('Ctrl Pts',(-19.3011565997644,-2.22193672053857,
-319.079423081229)) ;
#24095 = CARTESIAN_POINT('Ctrl Pts',(-19.3770393798232,-1.4279701314104,-319.088763113019)) ;
#24096 = CARTESIAN_POINT('Ctrl Pts',(-19.4034904314886,-1.00663452578914,
-319.093673030672)) ;
#24097 = CARTESIAN_POINT('Ctrl Pts',(-19.4248948166236,-0.295944930719285,
-319.102021365853)) ;
#24098 = CARTESIAN_POINT('Ctrl Pts',(-19.4271478415352,-0.0069595709563066,
-319.10543382954)) ;
#24099 = CARTESIAN_POINT('Ctrl Pts',(-19.4196884454123,0.506870156982208,
-319.11156535498)) ;
#24100 = CARTESIAN_POINT('Ctrl Pts',(-19.4125174538411,0.731698390769262,
-319.114269886848)) ;
#24101 = CARTESIAN_POINT('Ctrl Pts',(-19.3948134566833,1.09085846674695,-319.118633375426)) ;
#24102 = CARTESIAN_POINT('Ctrl Pts',(-19.3867846151373,1.22529320652801,-319.120276243922)) ;
#24103 = CARTESIAN_POINT('Ctrl Pts',(-19.3684965380784,1.48593303008581,-319.123481250528)) ;
#24104 = CARTESIAN_POINT('Ctrl Pts',(-19.3584000000183,1.61214283027296,-319.125042255054)) ;
#24105 = CARTESIAN_POINT('Ctrl Pts',(-19.3336303569957,1.88783473977934,-319.128472339184)) ;
#24106 = CARTESIAN_POINT('Ctrl Pts',(-19.318455932172,2.03726363082032,-319.130344543198)) ;
#24107 = CARTESIAN_POINT('Ctrl Pts',(-19.25314781647,2.61377727702371,-319.137617418963)) ;
#24108 = CARTESIAN_POINT('Ctrl Pts',(-19.1905711747549,3.03932703729421,-319.143094303266)) ;
#24109 = CARTESIAN_POINT('Ctrl Pts',(-19.0173764027594,3.9954228492101,-319.155574852306)) ;
#24110 = CARTESIAN_POINT('Ctrl Pts',(-18.8985791057416,4.52412599122849,-319.162602881702)) ;
#24111 = CARTESIAN_POINT('Ctrl Pts',(-18.724527504751,5.170989811772,-319.171176061958)) ;
#24112 = CARTESIAN_POINT('Ctrl Pts',(-18.6899865524383,5.29447529288879,-319.172811095647)) ;
#24113 = CARTESIAN_POINT('Ctrl Pts',(-18.6088454376086,5.57386504444546,-319.176500694777)) ;
#24114 = CARTESIAN_POINT('Ctrl Pts',(-18.5615038098253,5.72954418035052,-319.178549686023)) ;
#24115 = CARTESIAN_POINT('Ctrl Pts',(-18.4885163252147,5.95915323007896,-319.181552393243)) ;
#24116 = CARTESIAN_POINT('Ctrl Pts',(-18.4643707752617,6.03355243794713,-319.182522309887)) ;
#24117 = CARTESIAN_POINT('Ctrl Pts',(-18.4187930541865,6.17115394140327,-319.184309172572)) ;
#24118 = CARTESIAN_POINT('Ctrl Pts',(-18.3974833250131,6.23439538672314,-319.185127510836)) ;
#24119 = CARTESIAN_POINT('Ctrl Pts',(-18.3433008693072,6.39249693441792,-319.187166994278)) ;
#24120 = CARTESIAN_POINT('Ctrl Pts',(-18.310017830893,6.48721441840174,-319.188383218009)) ;
#24121 = CARTESIAN_POINT('Ctrl Pts',(-18.1531698348957,6.92275044755156,-319.193958018758)) ;
#24122 = CARTESIAN_POINT('Ctrl Pts',(-18.0208131590611,7.26032665209868,-319.198229971217)) ;
#24123 = CARTESIAN_POINT('Ctrl Pts',(-17.8384470777989,7.6896838442158,-319.203694955434)) ;
#24124 = CARTESIAN_POINT('Ctrl Pts',(-17.7970392699325,7.78503853579107,-319.204910594097)) ;
#24125 = CARTESIAN_POINT('Ctrl Pts',(-17.5584583825457,8.32259461867351,-319.211783085014)) ;
#24126 = CARTESIAN_POINT('Ctrl Pts',(-17.345572051133,8.75763506388627,-319.217424338588)) ;
#24127 = CARTESIAN_POINT('Ctrl Pts',(-16.9707337335858,9.45621874933345,-319.226803067271)) ;
#24128 = CARTESIAN_POINT('Ctrl Pts',(-16.818351950779,9.72465493470311,-319.230486730623)) ;
#24129 = CARTESIAN_POINT('Ctrl Pts',(-16.5832574868462,10.1167315595443,-319.236011605052)) ;
#24130 = CARTESIAN_POINT('Ctrl Pts',(-16.5054168849176,10.2432367785327,-319.237816995416)) ;
#24131 = CARTESIAN_POINT('Ctrl Pts',(-16.3665888869429,10.4631657107685,-319.240997555763)) ;
#24132 = CARTESIAN_POINT('Ctrl Pts',(-16.3062332163227,10.5569800012248,-319.242367856849)) ;
#24133 = CARTESIAN_POINT('Ctrl Pts',(-16.1644949881051,10.7731762133207,-319.245557877206)) ;
#24134 = CARTESIAN_POINT('Ctrl Pts',(-16.0825249525402,10.8951647540438,-319.247382074004)) ;
#24135 = CARTESIAN_POINT('Ctrl Pts',(-15.830094880295,11.2617766245844,-319.252938310712)) ;
#24136 = CARTESIAN_POINT('Ctrl Pts',(-15.6553802985389,11.5034161787677,-319.256702401312)) ;
#24137 = CARTESIAN_POINT('Ctrl Pts',(-15.2005919979552,12.1028510703977,-319.266284355565)) ;
#24138 = CARTESIAN_POINT('Ctrl Pts',(-14.9133993252527,12.4550198886634,-319.27214469337)) ;
#24139 = CARTESIAN_POINT('Ctrl Pts',(-14.3014337225396,13.153893498165,-319.284129349596)) ;
#24140 = CARTESIAN_POINT('Ctrl Pts',(-13.9757578203743,13.4994116575871,-319.290249774535)) ;
#24141 = CARTESIAN_POINT('Ctrl Pts',(-13.5526641681001,13.916543997344,-319.297733878049)) ;
#24142 = CARTESIAN_POINT('Ctrl Pts',(-13.4668022349233,13.9996478710047,-319.299229649769)) ;
#24143 = CARTESIAN_POINT('Ctrl Pts',(-13.3343548476939,14.1254947315382,-319.301498226729)) ;
#24144 = CARTESIAN_POINT('Ctrl Pts',(-13.2883184836089,14.1688112593946,-319.302279711851)) ;
#24145 = CARTESIAN_POINT('Ctrl Pts',(-13.1912193463019,14.2592842788769,-319.303912487723)) ;
#24146 = CARTESIAN_POINT('Ctrl Pts',(-13.1401132729873,14.3063929472702,-319.304762904417)) ;
#24147 = CARTESIAN_POINT('Ctrl Pts',(-13.0026594517259,14.4317375502826,-319.307027912034)) ;
#24148 = CARTESIAN_POINT('Ctrl Pts',(-12.9158586748178,14.5094726399239,-319.30843500956)) ;
#24149 = CARTESIAN_POINT('Ctrl Pts',(-12.2152370283555,15.1256504256142,-319.319630140021)) ;
#24150 = CARTESIAN_POINT('Ctrl Pts',(-11.5687193323299,15.6256859697436,-319.329009437447)) ;
#24151 = CARTESIAN_POINT('Ctrl Pts',(-10.581632880336,16.2941945412504,-319.343037871547)) ;
#24152 = CARTESIAN_POINT('Ctrl Pts',(-10.2645659281097,16.4957696275153,-319.347497290025)) ;
#24153 = CARTESIAN_POINT('Ctrl Pts',(-9.80522660530929,16.7694200485499,-319.353941284508)) ;
#24154 = CARTESIAN_POINT('Ctrl Pts',(-9.667604152967,16.8491349153244,-319.355869657371)) ;
#24155 = CARTESIAN_POINT('Ctrl Pts',(-9.42052513919147,16.9882262797459,-319.359330097166)) ;
#24156 = CARTESIAN_POINT('Ctrl Pts',(-9.31144720129368,17.0482573009866,-319.360857201268)) ;
#24157 = CARTESIAN_POINT('Ctrl Pts',(-9.07673726510174,17.1745052760715,-319.364142671045)) ;
#24158 = CARTESIAN_POINT('Ctrl Pts',(-8.95094096972081,17.2404015772406,-319.365903276137)) ;
#24159 = CARTESIAN_POINT('Ctrl Pts',(-8.58654913872108,17.4262188413609,-319.371002531296)) ;
#24160 = CARTESIAN_POINT('Ctrl Pts',(-8.34618911471716,17.5426068772734,-319.374365648693)) ;
#24161 = CARTESIAN_POINT('Ctrl Pts',(-7.34958317248912,18.0000670383572,-319.388291465842)) ;
#24162 = CARTESIAN_POINT('Ctrl Pts',(-6.57427009648635,18.2974793099848,-319.399120297439)) ;
#24163 = CARTESIAN_POINT('Ctrl Pts',(-5.57823854312572,18.6080515203548,-319.412430109452)) ;
#24164 = CARTESIAN_POINT('Ctrl Pts',(-5.3731133531913,18.668314862405,-319.415137404912)) ;
#24165 = CARTESIAN_POINT('Ctrl Pts',(-5.08338582086082,18.7482624151904,-319.418895210974)) ;
#24166 = CARTESIAN_POINT('Ctrl Pts',(-4.99958272234323,18.770783884055,-319.41997441577)) ;
#24167 = CARTESIAN_POINT('Ctrl Pts',(-4.85210862625507,18.8093587905659,-319.421858268555)) ;
#24168 = CARTESIAN_POINT('Ctrl Pts',(-4.78850208370146,18.8256522873235,-319.422665692023)) ;
#24169 = CARTESIAN_POINT('Ctrl Pts',(-4.64100228455089,18.8626400298758,-319.424526291629)) ;
#24170 = CARTESIAN_POINT('Ctrl Pts',(-4.55705128569807,18.8830975930296,-319.425576703793)) ;
#24171 = CARTESIAN_POINT('Ctrl Pts',(-4.26191973839969,18.9529338055533,-319.429243483035)) ;
#24172 = CARTESIAN_POINT('Ctrl Pts',(-4.05005102379226,18.9993354280094,-319.431829396955)) ;
#24173 = CARTESIAN_POINT('Ctrl Pts',(-3.45867597488227,19.1185114874035,-319.438965655464)) ;
#24174 = CARTESIAN_POINT('Ctrl Pts',(-3.07770871133181,19.18352498438,-319.443471370064)) ;
#24175 = CARTESIAN_POINT('Ctrl Pts',(-2.50189577599105,19.2641943980974,-319.450262618639)) ;
#24176 = CARTESIAN_POINT('Ctrl Pts',(-2.30833870158,19.2883446849052,-319.45254192553)) ;
#24177 = CARTESIAN_POINT('Ctrl Pts',(-1.67336492210439,19.3578760347954,-319.460033375713)) ;
#24178 = CARTESIAN_POINT('Ctrl Pts',(-1.23075434875401,19.3910483792836,-319.465280469474)) ;
#24179 = CARTESIAN_POINT('Ctrl Pts',(-0.623320616382399,19.4156911297978,
-319.472599739241)) ;
#24180 = CARTESIAN_POINT('Ctrl Pts',(-0.459165776355288,19.4202666646659,
-319.474589088276)) ;
#24181 = CARTESIAN_POINT('Ctrl Pts',(-0.16991243671988,19.4246595459666,-319.478117245155)) ;
#24182 = CARTESIAN_POINT('Ctrl Pts',(-0.0448367083294808,19.4253509192243,
-319.479650332151)) ;
#24183 = CARTESIAN_POINT('Ctrl Pts',(0.21935368510912,19.4242596456323,-319.482905152556)) ;
#24184 = CARTESIAN_POINT('Ctrl Pts',(0.358460185782071,19.4221905317047,-319.484628652571)) ;
#24185 = CARTESIAN_POINT('Ctrl Pts',(0.747493509970748,19.4122229552821,-319.489476103244)) ;
#24186 = CARTESIAN_POINT('Ctrl Pts',(0.997307315390067,19.4009928708691,-319.492620766601)) ;
#24187 = CARTESIAN_POINT('Ctrl Pts',(1.58522149112291,19.3631783933155,-319.500089585227)) ;
#24188 = CARTESIAN_POINT('Ctrl Pts',(1.92298031716225,19.3325567558531,-319.504434253006)) ;
#24189 = CARTESIAN_POINT('Ctrl Pts',(2.93072117525097,19.2145220741525,-319.517496453928)) ;
#24190 = CARTESIAN_POINT('Ctrl Pts',(3.59712195098988,19.1009868442836,-319.5262798367)) ;
#24191 = CARTESIAN_POINT('Ctrl Pts',(4.36775995916229,18.9279253875368,-319.536218792138)) ;
#24192 = CARTESIAN_POINT('Ctrl Pts',(4.47904679191005,18.9019000745747,-319.537648164129)) ;
#24193 = CARTESIAN_POINT('Ctrl Pts',(4.65063233290984,18.8601729863577,-319.539839477076)) ;
#24194 = CARTESIAN_POINT('Ctrl Pts',(4.71109597756533,18.8451606751506,-319.5406092371)) ;
#24195 = CARTESIAN_POINT('Ctrl Pts',(4.83992806172283,18.8125146220046,-319.542243423241)) ;
#24196 = CARTESIAN_POINT('Ctrl Pts',(4.90827470886859,18.7947984676675,-319.543106761882)) ;
#24197 = CARTESIAN_POINT('Ctrl Pts',(5.09457423403305,18.7454221966875,-319.545451928985)) ;
#24198 = CARTESIAN_POINT('Ctrl Pts',(5.21232763872753,18.7130216857496,-319.546925321088)) ;
#24199 = CARTESIAN_POINT('Ctrl Pts',(5.74454508610029,18.5611657237391,-319.55355860564)) ;
#24200 = CARTESIAN_POINT('Ctrl Pts',(6.155266552297,18.4290359668572,-319.558608190151)) ;
#24201 = CARTESIAN_POINT('Ctrl Pts',(7.21925500414974,18.0472079326958,-319.571816545702)) ;
#24202 = CARTESIAN_POINT('Ctrl Pts',(7.86403413150695,17.7757228640842,-319.579964169707)) ;
#24203 = CARTESIAN_POINT('Ctrl Pts',(8.65627264809483,17.3905899661984,-319.590539817958)) ;
#24204 = CARTESIAN_POINT('Ctrl Pts',(8.81865051146814,17.3088150533775,-319.592737096492)) ;
#24205 = CARTESIAN_POINT('Ctrl Pts',(9.09147400862782,17.1665829427565,-319.596483433851)) ;
#24206 = CARTESIAN_POINT('Ctrl Pts',(9.20252330661169,17.1073093829274,-319.598023862791)) ;
#24207 = CARTESIAN_POINT('Ctrl Pts',(9.42996686121904,16.9830538481456,-319.601211861457)) ;
#24208 = CARTESIAN_POINT('Ctrl Pts',(9.54628416540355,16.9179446620544,-319.602860311755)) ;
#24209 = CARTESIAN_POINT('Ctrl Pts',(9.85043698043884,16.7435580642309,-319.607218931059)) ;
#24210 = CARTESIAN_POINT('Ctrl Pts',(10.037124720128,16.6323171106734,-319.609943317031)) ;
#24211 = CARTESIAN_POINT('Ctrl Pts',(10.3465566923133,16.4408295884237,-319.614539446108)) ;
#24212 = CARTESIAN_POINT('Ctrl Pts',(10.4703296399019,16.3622831570724,-319.616399948199)) ;
#24213 = CARTESIAN_POINT('Ctrl Pts',(10.9943619232276,16.0213506831903,-319.624366904326)) ;
#24214 = CARTESIAN_POINT('Ctrl Pts',(11.3857393299431,15.7456219411165,-319.630547899466)) ;
#24215 = CARTESIAN_POINT('Ctrl Pts',(12.116032479166,15.1896454514303,-319.642386349653)) ;
#24216 = CARTESIAN_POINT('Ctrl Pts',(12.4564073416982,14.911790272916,-319.648040808461)) ;
#24217 = CARTESIAN_POINT('Ctrl Pts',(12.8763387012517,14.5445725085118,-319.655066458539)) ;
#24218 = CARTESIAN_POINT('Ctrl Pts',(12.9648910773246,14.4656934579686,-319.65655069805)) ;
#24219 = CARTESIAN_POINT('Ctrl Pts',(13.0994104250053,14.3436413398267,-319.658805835417)) ;
#24220 = CARTESIAN_POINT('Ctrl Pts',(13.1458986479478,14.3010471335973,-319.659585261497)) ;
#24221 = CARTESIAN_POINT('Ctrl Pts',(13.2433232408229,14.210906710811,-319.661218038106)) ;
#24222 = CARTESIAN_POINT('Ctrl Pts',(13.2942128092271,14.1633112579453,-319.662070478705)) ;
#24223 = CARTESIAN_POINT('Ctrl Pts',(13.4301638188544,14.0347821586678,-319.664348217855)) ;
#24224 = CARTESIAN_POINT('Ctrl Pts',(13.5147494761151,13.953349314783,-319.665765874823)) ;
#24225 = CARTESIAN_POINT('Ctrl Pts',(14.0191878154656,13.4588229937113,-319.674240296478)) ;
#24226 = CARTESIAN_POINT('Ctrl Pts',(14.4208137413924,13.0275737888171,-319.681081538056)) ;
#24227 = CARTESIAN_POINT('Ctrl Pts',(14.9722594784799,12.3786517725441,-319.691032954735)) ;
#24228 = CARTESIAN_POINT('Ctrl Pts',(15.1382199895028,12.1751332232697,-319.694107094242)) ;
#24229 = CARTESIAN_POINT('Ctrl Pts',(15.5134298944664,11.6954739098415,-319.701285857854)) ;
#24230 = CARTESIAN_POINT('Ctrl Pts',(15.7195195733131,11.4169751131098,-319.705405497076)) ;
#24231 = CARTESIAN_POINT('Ctrl Pts',(16.0085774286592,11.0036821824669,-319.71148753106)) ;
#24232 = CARTESIAN_POINT('Ctrl Pts',(16.0975210870838,10.8731498482114,-319.713403808928)) ;
#24233 = CARTESIAN_POINT('Ctrl Pts',(16.2535385579529,10.638069998087,-319.716849015764)) ;
#24234 = CARTESIAN_POINT('Ctrl Pts',(16.3212203108627,10.5339364179202,-319.718373110447)) ;
#24235 = CARTESIAN_POINT('Ctrl Pts',(16.4654702984172,10.3072686946033,-319.721686940702)) ;
#24236 = CARTESIAN_POINT('Ctrl Pts',(16.5416794251544,10.1845148049907,-319.723479304229)) ;
#24237 = CARTESIAN_POINT('Ctrl Pts',(16.7626753827012,9.81952023836204,-319.728802147479)) ;
#24238 = CARTESIAN_POINT('Ctrl Pts',(16.9035606429977,9.57496218182493,-319.732360677361)) ;
#24239 = CARTESIAN_POINT('Ctrl Pts',(17.3549922644091,8.75029982847682,-319.744316544545)) ;
#24240 = CARTESIAN_POINT('Ctrl Pts',(17.6413915214249,8.15749990096506,-319.752854497285)) ;
#24241 = CARTESIAN_POINT('Ctrl Pts',(18.0279101210599,7.24142332345096,-319.76563659963)) ;
#24242 = CARTESIAN_POINT('Ctrl Pts',(18.1505922341871,6.92818572287452,-319.769934179204)) ;
#24243 = CARTESIAN_POINT('Ctrl Pts',(18.2986470218039,6.519192244981,-319.775388638042)) ;
#24244 = CARTESIAN_POINT('Ctrl Pts',(18.331507948968,6.42620935781394,-319.776618274191)) ;
#24245 = CARTESIAN_POINT('Ctrl Pts',(18.385338365181,6.27011800760672,-319.77866268873)) ;
#24246 = CARTESIAN_POINT('Ctrl Pts',(18.4066944075146,6.20714488752647,-319.779482061991)) ;
#24247 = CARTESIAN_POINT('Ctrl Pts',(18.4527532675439,6.06900176175195,-319.781267087575)) ;
#24248 = CARTESIAN_POINT('Ctrl Pts',(18.4773209549008,5.99378810833174,-319.782231158767)) ;
#24249 = CARTESIAN_POINT('Ctrl Pts',(18.5526270616485,5.75837577893185,-319.785227071815)) ;
#24250 = CARTESIAN_POINT('Ctrl Pts',(18.6017467860728,5.59766729655617,-319.787241281824)) ;
#24251 = CARTESIAN_POINT('Ctrl Pts',(18.7965748415917,4.92933096199668,-319.795523127758)) ;
#24252 = CARTESIAN_POINT('Ctrl Pts',(18.9236369358729,4.41650280620033,-319.801659121554)) ;
#24253 = CARTESIAN_POINT('Ctrl Pts',(19.1407324677365,3.35697276733582,-319.814302166083)) ;
#24254 = CARTESIAN_POINT('Ctrl Pts',(19.2285998746394,2.81031150364746,-319.820808521203)) ;
#24255 = CARTESIAN_POINT('Ctrl Pts',(19.310926550977,2.107712269778,-319.829317575429)) ;
#24256 = CARTESIAN_POINT('Ctrl Pts',(19.3270275158075,1.95456966864444,-319.831180468447)) ;
#24257 = CARTESIAN_POINT('Ctrl Pts',(19.3530051756656,1.6756293138922,-319.834591018595)) ;
#24258 = CARTESIAN_POINT('Ctrl Pts',(19.3634802149994,1.54989575190196,-319.83613473974)) ;
#24259 = CARTESIAN_POINT('Ctrl Pts',(19.3824641648942,1.29164219627096,-319.839319501247)) ;
#24260 = CARTESIAN_POINT('Ctrl Pts',(19.39084061465,1.15911900456988,-319.84096131771)) ;
#24261 = CARTESIAN_POINT('Ctrl Pts',(19.4091907277486,0.812362275099774,-319.845277357797)) ;
#24262 = CARTESIAN_POINT('Ctrl Pts',(19.416976473909,0.598031398985461,-319.847965278672)) ;
#24263 = CARTESIAN_POINT('Ctrl Pts',(19.4240515196692,0.239845096497573,-319.852488637292)) ;
#24264 = CARTESIAN_POINT('Ctrl Pts',(19.425294797375,0.0960473048833851,-319.854312971843)) ;
#24265 = CARTESIAN_POINT('Ctrl Pts',(19.4238035592789,-0.510584409799216,
-319.862040189592)) ;
#24266 = CARTESIAN_POINT('Ctrl Pts',(19.4061244350911,-0.973228774394006,
-319.868013287343)) ;
#24267 = CARTESIAN_POINT('Ctrl Pts',(19.3573626930666,-1.63158588178593,-319.876529758202)) ;
#24268 = CARTESIAN_POINT('Ctrl Pts',(19.3397897050108,-1.82814035011033,-319.879073856347)) ;
#24269 = CARTESIAN_POINT('Ctrl Pts',(19.2872448141822,-2.32958775406388,-319.885547524391)) ;
#24270 = CARTESIAN_POINT('Ctrl Pts',(19.2480369977297,-2.63398253625553,-319.889461733029)) ;
#24271 = CARTESIAN_POINT('Ctrl Pts',(19.1868400664284,-3.03403455816125,-319.894535741393)) ;
#24272 = CARTESIAN_POINT('Ctrl Pts',(19.1713150346135,-3.13063528946316,-319.895755464012)) ;
#24273 = CARTESIAN_POINT('Ctrl Pts',(19.1440301423152,-3.29258917814907,-319.897788763722)) ;
#24274 = CARTESIAN_POINT('Ctrl Pts',(19.1326638120382,-3.35800671164288,-319.898606816706)) ;
#24275 = CARTESIAN_POINT('Ctrl Pts',(19.1069434318142,-3.50166607401071,-319.900395601994)) ;
#24276 = CARTESIAN_POINT('Ctrl Pts',(19.0924437541368,-3.57988046125007,-319.90136468146)) ;
#24277 = CARTESIAN_POINT('Ctrl Pts',(19.0453427895433,-3.82552454708578,-319.904395924486)) ;
#24278 = CARTESIAN_POINT('Ctrl Pts',(19.011016352351,-3.99261536397352,-319.906439868259)) ;
#24279 = CARTESIAN_POINT('Ctrl Pts',(18.8612998114041,-4.67562491496626,-319.914755429211)) ;
#24280 = CARTESIAN_POINT('Ctrl Pts',(18.7270724414509,-5.18718219041252,-319.920896964146)) ;
#24281 = CARTESIAN_POINT('Ctrl Pts',(18.4113633395472,-6.21718044863164,-319.933491337464)) ;
#24282 = CARTESIAN_POINT('Ctrl Pts',(18.2284293175958,-6.73468601389578,-319.939942712156)) ;
#24283 = CARTESIAN_POINT('Ctrl Pts',(17.9663481508599,-7.38679396782988,-319.948396081849)) ;
#24284 = CARTESIAN_POINT('Ctrl Pts',(17.9071589631958,-7.52914661728683,-319.950261103953)) ;
#24285 = CARTESIAN_POINT('Ctrl Pts',(17.7964438069221,-7.786728505083,-319.953674257314)) ;
#24286 = CARTESIAN_POINT('Ctrl Pts',(17.7454772322504,-7.90218898381787,-319.955218430139)) ;
#24287 = CARTESIAN_POINT('Ctrl Pts',(17.6386136913809,-8.13803083715431,-319.958402788484)) ;
#24288 = CARTESIAN_POINT('Ctrl Pts',(17.5826008338157,-8.2583525428472,-319.96004373622)) ;
#24289 = CARTESIAN_POINT('Ctrl Pts',(17.4330234286783,-8.57123979643036,-319.964354199776)) ;
#24290 = CARTESIAN_POINT('Ctrl Pts',(17.3375008366692,-8.76284896724658,-319.967037345288)) ;
#24291 = CARTESIAN_POINT('Ctrl Pts',(17.1727224004742,-9.08013238251074,-319.971551198128)) ;
#24292 = CARTESIAN_POINT('Ctrl Pts',(17.105206232086,-9.20668878731601,-319.973370820631)) ;
#24293 = CARTESIAN_POINT('Ctrl Pts',(16.8148983557659,-9.73664090089767,-319.981067326744)) ;
#24294 = CARTESIAN_POINT('Ctrl Pts',(16.5791906918577,-10.1327892236922,-319.987013880993)) ;
#24295 = CARTESIAN_POINT('Ctrl Pts',(16.2347365115245,-10.6674574852521,-319.995219045869)) ;
#24296 = CARTESIAN_POINT('Ctrl Pts',(16.1378655561486,-10.8134459874558,-319.997478108299)) ;
#24297 = CARTESIAN_POINT('Ctrl Pts',(15.8532660786967,-11.2300053106622,-320.003962314034)) ;
#24298 = CARTESIAN_POINT('Ctrl Pts',(15.6606147021019,-11.4971393196055,-320.008168610392)) ;
#24299 = CARTESIAN_POINT('Ctrl Pts',(15.401255676348,-11.8381491529765,-320.013541816394)) ;
#24300 = CARTESIAN_POINT('Ctrl Pts',(15.340642454738,-11.9165909928463,-320.014777984915)) ;
#24301 = CARTESIAN_POINT('Ctrl Pts',(15.2383304843045,-12.0469224113029,-320.01682974958)) ;
#24302 = CARTESIAN_POINT('Ctrl Pts',(15.1969607062318,-12.0990677682819,-320.017650019072)) ;
#24303 = CARTESIAN_POINT('Ctrl Pts',(15.1059979787026,-12.2125209500564,-320.019432696106)) ;
#24304 = CARTESIAN_POINT('Ctrl Pts',(15.0562981778349,-12.2737414054994,-320.020393568594)) ;
#24305 = CARTESIAN_POINT('Ctrl Pts',(14.9005404323206,-12.4632347953278,-320.023367103946)) ;
#24306 = CARTESIAN_POINT('Ctrl Pts',(14.7932055954489,-12.5904485663399,-320.025362502473)) ;
#24307 = CARTESIAN_POINT('Ctrl Pts',(14.5974159250915,-12.8165388336824,-320.028921331156)) ;
#24308 = CARTESIAN_POINT('Ctrl Pts',(14.5095579535376,-12.915918372653,-320.030490098249)) ;
#24309 = CARTESIAN_POINT('Ctrl Pts',(14.0312113165347,-13.4459538114782,-320.038900796939)) ;
#24310 = CARTESIAN_POINT('Ctrl Pts',(13.6225568993258,-13.8598163825987,-320.045635080711)) ;
#24311 = CARTESIAN_POINT('Ctrl Pts',(12.906066784318,-14.5230892005215,-320.057113830224)) ;
#24312 = CARTESIAN_POINT('Ctrl Pts',(12.6080563836265,-14.7825435233644,-320.061799326824)) ;
#24313 = CARTESIAN_POINT('Ctrl Pts',(12.1790461947006,-15.1336328199938,-320.068480156693)) ;
#24314 = CARTESIAN_POINT('Ctrl Pts',(12.0545124738968,-15.2330147202168,-320.070411896682)) ;
#24315 = CARTESIAN_POINT('Ctrl Pts',(11.8304864172023,-15.4073269615523,-320.073876027723)) ;
#24316 = CARTESIAN_POINT('Ctrl Pts',(11.7314693973193,-15.4828537001632,-320.075403414269)) ;
#24317 = CARTESIAN_POINT('Ctrl Pts',(11.6040727697785,-15.5781036372578,-320.077364289323)) ;
#24318 = CARTESIAN_POINT('Ctrl Pts',(11.5763573826724,-15.5987104443636,-320.077790623979)) ;
#24319 = CARTESIAN_POINT('Ctrl Pts',(11.536965465186,-15.6278361188462,-320.078396214306)) ;
#24320 = CARTESIAN_POINT('Ctrl Pts',(11.5253341519739,-15.6364160403744,-320.078574983567)) ;
#24321 = CARTESIAN_POINT('Ctrl Pts',(11.5013343520194,-15.6540783373441,-320.078943761192)) ;
#24322 = CARTESIAN_POINT('Ctrl Pts',(11.4889646574522,-15.6631590545577,-320.079133782508)) ;
#24323 = CARTESIAN_POINT('Ctrl Pts',(11.3494818178547,-15.7653006805766,-320.081275938116)) ;
#24324 = CARTESIAN_POINT('Ctrl Pts',(11.2212519883264,-15.8568265048196,-320.083240115295)) ;
#24325 = CARTESIAN_POINT('Ctrl Pts',(10.9334497031553,-16.0570098881476,-320.087636653383)) ;
#24326 = CARTESIAN_POINT('Ctrl Pts',(10.7733421362647,-16.1648689453075,-320.090074571522)) ;
#24327 = CARTESIAN_POINT('Ctrl Pts',(10.2898271280426,-16.4802218539497,-320.097407787465)) ;
#24328 = CARTESIAN_POINT('Ctrl Pts',(9.96184416019737,-16.6805250139656,-320.102345417078)) ;
#24329 = CARTESIAN_POINT('Ctrl Pts',(9.10076366196011,-17.1719373173476,-320.115128779555)) ;
#24330 = CARTESIAN_POINT('Ctrl Pts',(8.55956732940584,-17.4480124475641,-320.122998913466)) ;
#24331 = CARTESIAN_POINT('Ctrl Pts',(7.90699649753113,-17.7432217520323,-320.132001980529)) ;
#24332 = CARTESIAN_POINT('Ctrl Pts',(7.80728493739994,-17.7873217126604,-320.133364258878)) ;
#24333 = CARTESIAN_POINT('Ctrl Pts',(7.65082907614626,-17.8549492246879,-320.135477957095)) ;
#24334 = CARTESIAN_POINT('Ctrl Pts',(7.59433550681355,-17.8790510261955,-320.136236353435)) ;
#24335 = CARTESIAN_POINT('Ctrl Pts',(7.49133427772186,-17.9224180769281,-320.137609682883)) ;
#24336 = CARTESIAN_POINT('Ctrl Pts',(7.44486426451642,-17.9417712356788,-320.138225831955)) ;
#24337 = CARTESIAN_POINT('Ctrl Pts',(7.32828074780718,-17.9897933290309,-320.139763597955)) ;
#24338 = CARTESIAN_POINT('Ctrl Pts',(7.2580737654951,-18.0182332089402,-320.140682406149)) ;
#24339 = CARTESIAN_POINT('Ctrl Pts',(6.950268086372,-18.1408300983097,-320.144682484297)) ;
#24340 = CARTESIAN_POINT('Ctrl Pts',(6.71099026965467,-18.2307035849578,-320.147719048505)) ;
#24341 = CARTESIAN_POINT('Ctrl Pts',(5.96525904222833,-18.4941307713049,-320.157042646806)) ;
#24342 = CARTESIAN_POINT('Ctrl Pts',(5.45335437292572,-18.6514909847323,-320.163251148029)) ;
#24343 = CARTESIAN_POINT('Ctrl Pts',(4.50900273328787,-18.899578534748,-320.174703850276)) ;
#24344 = CARTESIAN_POINT('Ctrl Pts',(4.07870795394553,-18.9970870043679,-320.179920710947)) ;
#24345 = CARTESIAN_POINT('Ctrl Pts',(3.48464881511938,-19.1105901213535,-320.187203008135)) ;
#24346 = CARTESIAN_POINT('Ctrl Pts',(3.32344711824944,-19.1392824134687,-320.189186663364)) ;
#24347 = CARTESIAN_POINT('Ctrl Pts',(3.03855365646183,-19.1862827463981,-320.192708423543)) ;
#24348 = CARTESIAN_POINT('Ctrl Pts',(2.91501170326987,-19.2054409131982,-320.194240878757)) ;
#24349 = CARTESIAN_POINT('Ctrl Pts',(2.67617180461992,-19.2401211510786,-320.197214383535)) ;
#24350 = CARTESIAN_POINT('Ctrl Pts',(2.5609023354619,-19.2558026741529,-320.198654322613)) ;
#24351 = CARTESIAN_POINT('Ctrl Pts',(2.30827514732471,-19.28786210294,-320.201820904053)) ;
#24352 = CARTESIAN_POINT('Ctrl Pts',(2.17086927092872,-19.3038101214256,-320.203550195971)) ;
#24353 = CARTESIAN_POINT('Ctrl Pts',(1.35770446560157,-19.3893980313548,-320.213823603408)) ;
#24354 = CARTESIAN_POINT('Ctrl Pts',(0.678840956636049,-19.4250170068381,
-320.222580491791)) ;
#24355 = CARTESIAN_POINT('Ctrl Pts',(-0.000486475511301404,-19.4249999939084,
-320.231344117963)) ;
#24356 = CARTESIAN_POINT('Ctrl Pts',(9.76712100086985E-9,-19.425,-318.518971385864)) ;
#24357 = CARTESIAN_POINT('Ctrl Pts',(-0.281309642560281,-19.4250000001414,
-318.522593938602)) ;
#24358 = CARTESIAN_POINT('Ctrl Pts',(-0.562608351426869,-19.4188891791731,
-318.52620480889)) ;
#24359 = CARTESIAN_POINT('Ctrl Pts',(-0.98839503799673,-19.4003782790569,
-318.531633105823)) ;
#24360 = CARTESIAN_POINT('Ctrl Pts',(-1.13301837794897,-19.3924694543237,
-318.53347047545)) ;
#24361 = CARTESIAN_POINT('Ctrl Pts',(-1.49304367215994,-19.3687400017827,
-318.538025821844)) ;
#24362 = CARTESIAN_POINT('Ctrl Pts',(-1.7082958740376,-19.3509429770943,-318.54073264566)) ;
#24363 = CARTESIAN_POINT('Ctrl Pts',(-2.05644308952404,-19.3163038514045,
-318.545081253135)) ;
#24364 = CARTESIAN_POINT('Ctrl Pts',(-2.18953891826495,-19.30167018793,-318.546736780915)) ;
#24365 = CARTESIAN_POINT('Ctrl Pts',(-2.44903474289518,-19.2704204422533,
-318.549951299789)) ;
#24366 = CARTESIAN_POINT('Ctrl Pts',(-2.57544357055276,-19.253933770986,-318.551511038845)) ;
#24367 = CARTESIAN_POINT('Ctrl Pts',(-2.85626281090689,-19.2144933483132,
-318.554963303093)) ;
#24368 = CARTESIAN_POINT('Ctrl Pts',(-3.01057738304826,-19.1909201390506,
-318.556851771086)) ;
#24369 = CARTESIAN_POINT('Ctrl Pts',(-3.70461599907052,-19.0763210064208,
-318.565312913879)) ;
#24370 = CARTESIAN_POINT('Ctrl Pts',(-4.24063143112721,-18.964367890893,-318.571751450696)) ;
#24371 = CARTESIAN_POINT('Ctrl Pts',(-5.19254844379973,-18.7231673640123,
-318.583240523233)) ;
#24372 = CARTESIAN_POINT('Ctrl Pts',(-5.61019155372591,-18.6022930116724,
-318.588302851206)) ;
#24373 = CARTESIAN_POINT('Ctrl Pts',(-6.1763337479905,-18.4176381295371,-318.595341812481)) ;
#24374 = CARTESIAN_POINT('Ctrl Pts',(-6.32861531634097,-18.3658683679347,
-318.59725336271)) ;
#24375 = CARTESIAN_POINT('Ctrl Pts',(-6.59606307380386,-18.2712252690202,
-318.600654534087)) ;
#24376 = CARTESIAN_POINT('Ctrl Pts',(-6.71149835490394,-18.2291390545479,
-318.602137165154)) ;
#24377 = CARTESIAN_POINT('Ctrl Pts',(-6.89323042781999,-18.1609216627391,
-318.604499547196)) ;
#24378 = CARTESIAN_POINT('Ctrl Pts',(-6.95979611729777,-18.1355159662169,
-318.605370888983)) ;
#24379 = CARTESIAN_POINT('Ctrl Pts',(-7.08445107702869,-18.0871523229644,
-318.607015200005)) ;
#24380 = CARTESIAN_POINT('Ctrl Pts',(-7.14257231876875,-18.0642793067054,
-318.607787063708)) ;
#24381 = CARTESIAN_POINT('Ctrl Pts',(-7.30763223389162,-17.9984005220407,
-318.609992827469)) ;
#24382 = CARTESIAN_POINT('Ctrl Pts',(-7.41429979558313,-17.9547227408593,
-318.611434720101)) ;
#24383 = CARTESIAN_POINT('Ctrl Pts',(-8.05855226592651,-17.6841967435869,
-318.620229844747)) ;
#24384 = CARTESIAN_POINT('Ctrl Pts',(-8.58608043785829,-17.4341704987621,
-318.627788409611)) ;
#24385 = CARTESIAN_POINT('Ctrl Pts',(-9.5766023086422,-16.9088280443761,-318.642248496006)) ;
#24386 = CARTESIAN_POINT('Ctrl Pts',(-10.0409869559877,-16.6372582347089,
-318.649149546914)) ;
#24387 = CARTESIAN_POINT('Ctrl Pts',(-10.6539918496282,-16.243751158889,-318.658318004136)) ;
#24388 = CARTESIAN_POINT('Ctrl Pts',(-10.8129520876239,-16.1383723268202,
-318.660701979693)) ;
#24389 = CARTESIAN_POINT('Ctrl Pts',(-11.0760522722631,-15.9583238825469,
-318.664657495471)) ;
#24390 = CARTESIAN_POINT('Ctrl Pts',(-11.1810513870136,-15.884933900105,-318.666238760988)) ;
#24391 = CARTESIAN_POINT('Ctrl Pts',(-11.3790104965478,-15.7436335116766,
-318.669225437135)) ;
#24392 = CARTESIAN_POINT('Ctrl Pts',(-11.4721077802981,-15.6759248258178,
-318.670632366494)) ;
#24393 = CARTESIAN_POINT('Ctrl Pts',(-11.716685426649,-15.4947003137914,-318.674335661906)) ;
#24394 = CARTESIAN_POINT('Ctrl Pts',(-11.8671178731669,-15.3797909198352,
-318.676620704043)) ;
#24395 = CARTESIAN_POINT('Ctrl Pts',(-12.4100687898402,-14.9523426553508,
-318.684904697639)) ;
#24396 = CARTESIAN_POINT('Ctrl Pts',(-12.7921186309444,-14.6268267404817,
-318.690800061353)) ;
#24397 = CARTESIAN_POINT('Ctrl Pts',(-13.4933998368074,-13.9808036454977,
-318.701941583293)) ;
#24398 = CARTESIAN_POINT('Ctrl Pts',(-13.8148835074953,-13.6632244498188,
-318.707191682889)) ;
#24399 = CARTESIAN_POINT('Ctrl Pts',(-14.286815456577,-13.163323743258,-318.715306283102)) ;
#24400 = CARTESIAN_POINT('Ctrl Pts',(-14.4454956396309,-12.9889893062894,
-318.718111007086)) ;
#24401 = CARTESIAN_POINT('Ctrl Pts',(-14.6592687562269,-12.7453630525265,
-318.722026148711)) ;
#24402 = CARTESIAN_POINT('Ctrl Pts',(-14.7171198130982,-12.6785182173073,
-318.723099953692)) ;
#24403 = CARTESIAN_POINT('Ctrl Pts',(-14.8169737794786,-12.5615361527424,
-318.724980614691)) ;
#24404 = CARTESIAN_POINT('Ctrl Pts',(-14.8591833934123,-12.5115774931384,
-318.725784347021)) ;
#24405 = CARTESIAN_POINT('Ctrl Pts',(-14.9550834583552,-12.3969018107208,
-318.727630644818)) ;
#24406 = CARTESIAN_POINT('Ctrl Pts',(-15.0086074605848,-12.3320475923666,
-318.728675615809)) ;
#24407 = CARTESIAN_POINT('Ctrl Pts',(-15.1834832746546,-12.1173283289809,
-318.732134973936)) ;
#24408 = CARTESIAN_POINT('Ctrl Pts',(-15.303024574892,-11.9660038788156,-318.734572358845)) ;
#24409 = CARTESIAN_POINT('Ctrl Pts',(-15.9423061939397,-11.1315018639262,
-318.747956071733)) ;
#24410 = CARTESIAN_POINT('Ctrl Pts',(-16.4185784480342,-10.4162254875563,
-318.75917431441)) ;
#24411 = CARTESIAN_POINT('Ctrl Pts',(-16.9790078444991,-9.44009013957686,
-318.773468010337)) ;
#24412 = CARTESIAN_POINT('Ctrl Pts',(-17.1072426802417,-9.20566442663661,
-318.776832953415)) ;
#24413 = CARTESIAN_POINT('Ctrl Pts',(-17.2962768300287,-8.84249209513793,
-318.781937011439)) ;
#24414 = CARTESIAN_POINT('Ctrl Pts',(-17.3605645323641,-8.71559853486529,
-318.783700558217)) ;
#24415 = CARTESIAN_POINT('Ctrl Pts',(-17.4786392289392,-8.47604724865055,
-318.786992917104)) ;
#24416 = CARTESIAN_POINT('Ctrl Pts',(-17.5327452632324,-8.36355485654717,
-318.78852395679)) ;
#24417 = CARTESIAN_POINT('Ctrl Pts',(-17.6535782295364,-8.10600350792921,
-318.791995949859)) ;
#24418 = CARTESIAN_POINT('Ctrl Pts',(-17.7196085051241,-7.96062759433623,
-318.793931894104)) ;
#24419 = CARTESIAN_POINT('Ctrl Pts',(-17.9372022810921,-7.46543590598969,
-318.800450722183)) ;
#24420 = CARTESIAN_POINT('Ctrl Pts',(-18.0802578902136,-7.1119782376013,-318.804975637053)) ;
#24421 = CARTESIAN_POINT('Ctrl Pts',(-18.417471675483,-6.20272105639672,-318.816386168539)) ;
#24422 = CARTESIAN_POINT('Ctrl Pts',(-18.5969383397456,-5.64188745504251,
-318.823205571547)) ;
#24423 = CARTESIAN_POINT('Ctrl Pts',(-18.7854897387201,-4.94507596005149,
-318.83171059127)) ;
#24424 = CARTESIAN_POINT('Ctrl Pts',(-18.8189884364033,-4.81602275262298,
-318.833287606221)) ;
#24425 = CARTESIAN_POINT('Ctrl Pts',(-18.8914683970381,-4.52448500263164,
-318.836862583972)) ;
#24426 = CARTESIAN_POINT('Ctrl Pts',(-18.9296870891624,-4.36182178552562,
-318.838865854972)) ;
#24427 = CARTESIAN_POINT('Ctrl Pts',(-18.9829081362497,-4.12141803792854,
-318.841850821195)) ;
#24428 = CARTESIAN_POINT('Ctrl Pts',(-18.9995415128459,-4.04404626993299,
-318.842815202196)) ;
#24429 = CARTESIAN_POINT('Ctrl Pts',(-19.0293177693786,-3.90129934197765,
-318.844602882531)) ;
#24430 = CARTESIAN_POINT('Ctrl Pts',(-19.0425976989024,-3.83595414033837,
-318.845424628392)) ;
#24431 = CARTESIAN_POINT('Ctrl Pts',(-19.0748294395548,-3.6730615720313,-318.847480901521)) ;
#24432 = CARTESIAN_POINT('Ctrl Pts',(-19.0933696769462,-3.5754347708675,-318.84872012183)) ;
#24433 = CARTESIAN_POINT('Ctrl Pts',(-19.1699793297289,-3.15443471089505,
-318.854087102997)) ;
#24434 = CARTESIAN_POINT('Ctrl Pts',(-19.2205886007562,-2.82975952166295,
-318.85828365467)) ;
#24435 = CARTESIAN_POINT('Ctrl Pts',(-19.3472024779211,-1.8557195114113,-318.870907862588)) ;
#24436 = CARTESIAN_POINT('Ctrl Pts',(-19.3986906192923,-1.20363816396453,
-318.879391869552)) ;
#24437 = CARTESIAN_POINT('Ctrl Pts',(-19.4229942398794,-0.345942738703501,
-318.890309916632)) ;
#24438 = CARTESIAN_POINT('Ctrl Pts',(-19.4255586998374,-0.141601557501543,
-318.89289464664)) ;
#24439 = CARTESIAN_POINT('Ctrl Pts',(-19.4243293951762,0.238989545311665,
-318.897673544698)) ;
#24440 = CARTESIAN_POINT('Ctrl Pts',(-19.4213614348628,0.415221148313284,
-318.899872358371)) ;
#24441 = CARTESIAN_POINT('Ctrl Pts',(-19.4121531722439,0.717539689643196,
-318.903619567498)) ;
#24442 = CARTESIAN_POINT('Ctrl Pts',(-19.407081366212,0.843650924975231,-318.905175322758)) ;
#24443 = CARTESIAN_POINT('Ctrl Pts',(-19.3940307038812,1.10475439300562,-318.908381531465)) ;
#24444 = CARTESIAN_POINT('Ctrl Pts',(-19.3858705420236,1.23973085745001,-318.910030725909)) ;
#24445 = CARTESIAN_POINT('Ctrl Pts',(-19.3601426778081,1.60238675401459,-318.91444132033)) ;
#24446 = CARTESIAN_POINT('Ctrl Pts',(-19.3399684821758,1.82985987867593,-318.917185930809)) ;
#24447 = CARTESIAN_POINT('Ctrl Pts',(-19.2315153508163,2.848301551117,-318.929400602154)) ;
#24448 = CARTESIAN_POINT('Ctrl Pts',(-19.0986877147631,3.63374849181006,-318.938588139787)) ;
#24449 = CARTESIAN_POINT('Ctrl Pts',(-18.8716089887424,4.60813179505011,-318.950346886867)) ;
#24450 = CARTESIAN_POINT('Ctrl Pts',(-18.8220148624354,4.80668917155145,-318.952764524926)) ;
#24451 = CARTESIAN_POINT('Ctrl Pts',(-18.7318332272153,5.14491890736277,-318.956942448483)) ;
#24452 = CARTESIAN_POINT('Ctrl Pts',(-18.6927974746998,5.2849871408575,-318.958690325869)) ;
#24453 = CARTESIAN_POINT('Ctrl Pts',(-18.6312341767884,5.49666905831746,-318.961366781977)) ;
#24454 = CARTESIAN_POINT('Ctrl Pts',(-18.609857994836,5.56861231194216,-318.962282579803)) ;
#24455 = CARTESIAN_POINT('Ctrl Pts',(-18.5686016729175,5.70457273291662,-318.964026421333)) ;
#24456 = CARTESIAN_POINT('Ctrl Pts',(-18.5488060791336,5.76861431843191,-318.964853487191)) ;
#24457 = CARTESIAN_POINT('Ctrl Pts',(-18.4966253480309,5.93438052676743,-318.967007935004)) ;
#24458 = CARTESIAN_POINT('Ctrl Pts',(-18.463732406974,6.03594293036196,-318.968341255345)) ;
#24459 = CARTESIAN_POINT('Ctrl Pts',(-18.2309585715872,6.73495917707555,-318.977597716277)) ;
#24460 = CARTESIAN_POINT('Ctrl Pts',(-18.0029523526304,7.32265194850747,-318.985770355803)) ;
#24461 = CARTESIAN_POINT('Ctrl Pts',(-17.5949113088679,8.23949358284055,-318.998706344651)) ;
#24462 = CARTESIAN_POINT('Ctrl Pts',(-17.4332163546212,8.5763119587949,-319.003503551503)) ;
#24463 = CARTESIAN_POINT('Ctrl Pts',(-17.1400142964417,9.14446202074354,-319.01162184168)) ;
#24464 = CARTESIAN_POINT('Ctrl Pts',(-17.0132826723432,9.37813888071287,-319.014969188932)) ;
#24465 = CARTESIAN_POINT('Ctrl Pts',(-16.8116435982421,9.73238796335473,-319.020050470095)) ;
#24466 = CARTESIAN_POINT('Ctrl Pts',(-16.7401440448032,9.85486242278771,-319.021808590269)) ;
#24467 = CARTESIAN_POINT('Ctrl Pts',(-16.6033408972646,10.0834125749074,-319.025092136772)) ;
#24468 = CARTESIAN_POINT('Ctrl Pts',(-16.5383456404657,10.1896644512946,-319.026619769169)) ;
#24469 = CARTESIAN_POINT('Ctrl Pts',(-16.3878492836484,10.4304568480525,-319.030085119356)) ;
#24470 = CARTESIAN_POINT('Ctrl Pts',(-16.3017048851415,10.5645848065078,-319.032017823272)) ;
#24471 = CARTESIAN_POINT('Ctrl Pts',(-15.9972008075659,11.0261076984492,-319.038681319967)) ;
#24472 = CARTESIAN_POINT('Ctrl Pts',(-15.7705506164876,11.3479169398191,-319.043349155503)) ;
#24473 = CARTESIAN_POINT('Ctrl Pts',(-15.184940038922,12.1279337945308,-319.054817237063)) ;
#24474 = CARTESIAN_POINT('Ctrl Pts',(-14.8148679480065,12.5773156145039,-319.061557857873)) ;
#24475 = CARTESIAN_POINT('Ctrl Pts',(-14.3363224859771,13.1079398816237,-319.069975444417)) ;
#24476 = CARTESIAN_POINT('Ctrl Pts',(-14.2464527234643,13.2055600074209,-319.071544724529)) ;
#24477 = CARTESIAN_POINT('Ctrl Pts',(-14.041585663632,13.4235692720284,-319.075104557132)) ;
#24478 = CARTESIAN_POINT('Ctrl Pts',(-13.9260266340707,13.543416185919,-319.077100443237)) ;
#24479 = CARTESIAN_POINT('Ctrl Pts',(-13.7534666466554,13.7178351715603,-319.080074754697)) ;
#24480 = CARTESIAN_POINT('Ctrl Pts',(-13.6976507680253,13.7735692545961,-319.081035916552)) ;
#24481 = CARTESIAN_POINT('Ctrl Pts',(-13.5940957996483,13.8757204367483,-319.082819134496)) ;
#24482 = CARTESIAN_POINT('Ctrl Pts',(-13.5464546343919,13.9222349158385,-319.083639655415)) ;
#24483 = CARTESIAN_POINT('Ctrl Pts',(-13.4272529093993,14.0374264579817,-319.085692330991)) ;
#24484 = CARTESIAN_POINT('Ctrl Pts',(-13.3554037623734,14.1058020885596,-319.086929164425)) ;
#24485 = CARTESIAN_POINT('Ctrl Pts',(-13.0430800892332,14.3985011130801,-319.092297491269)) ;
#24486 = CARTESIAN_POINT('Ctrl Pts',(-12.7974544051356,14.6172477753458,-319.096498007817)) ;
#24487 = CARTESIAN_POINT('Ctrl Pts',(-12.4521047642065,14.9094254161017,-319.102312037758)) ;
#24488 = CARTESIAN_POINT('Ctrl Pts',(-12.3570560226559,14.988296959111,-319.103903099836)) ;
#24489 = CARTESIAN_POINT('Ctrl Pts',(-11.9657294571611,15.3067673999572,-319.110408627166)) ;
#24490 = CARTESIAN_POINT('Ctrl Pts',(-11.6631843900081,15.5385308191745,-319.115332337856)) ;
#24491 = CARTESIAN_POINT('Ctrl Pts',(-11.032465958419,15.9928850761558,-319.12529673545)) ;
#24492 = CARTESIAN_POINT('Ctrl Pts',(-10.7038988152191,16.2146301114938,-319.130331621717)) ;
#24493 = CARTESIAN_POINT('Ctrl Pts',(-10.2339196797603,16.5112975471355,-319.137288657613)) ;
#24494 = CARTESIAN_POINT('Ctrl Pts',(-10.0980172924047,16.5947613891119,-319.139273005091)) ;
#24495 = CARTESIAN_POINT('Ctrl Pts',(-9.85437637253241,16.7402910866508,-319.142781867258)) ;
#24496 = CARTESIAN_POINT('Ctrl Pts',(-9.74704073897626,16.8030139033719,-319.144311232173)) ;
#24497 = CARTESIAN_POINT('Ctrl Pts',(-9.51455649186934,16.9358915135056,-319.147589070207)) ;
#24498 = CARTESIAN_POINT('Ctrl Pts',(-9.38921772309961,17.0056989627636,-319.149334899365)) ;
#24499 = CARTESIAN_POINT('Ctrl Pts',(-9.02067087819596,17.2056445089635,-319.15440884559)) ;
#24500 = CARTESIAN_POINT('Ctrl Pts',(-8.77545035467825,17.3319986599757,-319.157709701277)) ;
#24501 = CARTESIAN_POINT('Ctrl Pts',(-7.90574916523827,17.7569368184926,-319.169194684422)) ;
#24502 = CARTESIAN_POINT('Ctrl Pts',(-7.26808256790414,18.0273306093729,-319.177204314309)) ;
#24503 = CARTESIAN_POINT('Ctrl Pts',(-6.32345454911503,18.3696015485612,-319.189001075838)) ;
#24504 = CARTESIAN_POINT('Ctrl Pts',(-6.02703321474957,18.4689796230911,-319.192696813909)) ;
#24505 = CARTESIAN_POINT('Ctrl Pts',(-5.63427989693023,18.590191118835,-319.197649238454)) ;
#24506 = CARTESIAN_POINT('Ctrl Pts',(-5.53999659840101,18.6185056716164,-319.198842335518)) ;
#24507 = CARTESIAN_POINT('Ctrl Pts',(-5.38169521646288,18.6647368098396,-319.20085544333)) ;
#24508 = CARTESIAN_POINT('Ctrl Pts',(-5.31779301641488,18.6830436767091,-319.201670833769)) ;
#24509 = CARTESIAN_POINT('Ctrl Pts',(-5.17753837271423,18.7224463123878,-319.203467236348)) ;
#24510 = CARTESIAN_POINT('Ctrl Pts',(-5.10114848518211,18.7434037365707,-319.204449810701)) ;
#24511 = CARTESIAN_POINT('Ctrl Pts',(-4.8617830801725,18.8075014801824,-319.207539290597)) ;
#24512 = CARTESIAN_POINT('Ctrl Pts',(-4.69837293282371,18.8489877254449,-319.209663710756)) ;
#24513 = CARTESIAN_POINT('Ctrl Pts',(-4.02151656785325,19.0114777528298,-319.2184980939)) ;
#24514 = CARTESIAN_POINT('Ctrl Pts',(-3.50378669144107,19.1136694631686,-319.225331953445)) ;
#24515 = CARTESIAN_POINT('Ctrl Pts',(-2.43577292500802,19.2796216008331,-319.239263664763)) ;
#24516 = CARTESIAN_POINT('Ctrl Pts',(-1.8856225545396,19.3411796397485,-319.246350370911)) ;
#24517 = CARTESIAN_POINT('Ctrl Pts',(-1.18002345020777,19.3897360898768,-319.255222727326)) ;
#24518 = CARTESIAN_POINT('Ctrl Pts',(-1.02633135182892,19.3984784202595,-319.257142841635)) ;
#24519 = CARTESIAN_POINT('Ctrl Pts',(-0.746531880739883,19.4110594300021,
-319.26061536971)) ;
#24520 = CARTESIAN_POINT('Ctrl Pts',(-0.620460002500041,19.415498125939,-319.262171518501)) ;
#24521 = CARTESIAN_POINT('Ctrl Pts',(-0.361615415586241,19.4220876884012,
-319.265349473588)) ;
#24522 = CARTESIAN_POINT('Ctrl Pts',(-0.228845829115496,19.4241057844961,
-319.266970342065)) ;
#24523 = CARTESIAN_POINT('Ctrl Pts',(0.118422270441552,19.4258232120628,-319.271187264693)) ;
#24524 = CARTESIAN_POINT('Ctrl Pts',(0.332913498290453,19.423331334148,-319.273769216686)) ;
#24525 = CARTESIAN_POINT('Ctrl Pts',(0.691097371376012,19.4132351215999,-319.278050392725)) ;
#24526 = CARTESIAN_POINT('Ctrl Pts',(0.834825746196516,19.4075856172344,-319.279760140831)) ;
#24527 = CARTESIAN_POINT('Ctrl Pts',(1.44092500563573,19.3770163131899,-319.286943841325)) ;
#24528 = CARTESIAN_POINT('Ctrl Pts',(1.90239030063177,19.3371646729517,-319.292344948641)) ;
#24529 = CARTESIAN_POINT('Ctrl Pts',(2.54927461513781,19.2579185282765,-319.299957837074)) ;
#24530 = CARTESIAN_POINT('Ctrl Pts',(2.73621542702979,19.2322477154015,-319.302163367099)) ;
#24531 = CARTESIAN_POINT('Ctrl Pts',(3.23294661115451,19.1566471614693,-319.308062367286)) ;
#24532 = CARTESIAN_POINT('Ctrl Pts',(3.54195087193586,19.1019281088195,-319.31177164361)) ;
#24533 = CARTESIAN_POINT('Ctrl Pts',(3.94607148523922,19.0202222257233,-319.316739172532)) ;
#24534 = CARTESIAN_POINT('Ctrl Pts',(4.04249990231068,18.9999612679811,-319.317933340458)) ;
#24535 = CARTESIAN_POINT('Ctrl Pts',(4.20372436194343,18.9648028255723,-319.31994762389)) ;
#24536 = CARTESIAN_POINT('Ctrl Pts',(4.26860563362978,18.9503047647362,-319.320763104396)) ;
#24537 = CARTESIAN_POINT('Ctrl Pts',(4.41057961537276,18.9178138081743,-319.322558982284)) ;
#24538 = CARTESIAN_POINT('Ctrl Pts',(4.48763917291356,18.8996821787261,-319.323540933839)) ;
#24539 = CARTESIAN_POINT('Ctrl Pts',(4.7281420408479,18.8415395331534,-319.326625760228)) ;
#24540 = CARTESIAN_POINT('Ctrl Pts',(4.89117753658232,18.7998755657682,-319.328746074956)) ;
#24541 = CARTESIAN_POINT('Ctrl Pts',(5.56334159726219,18.6187674092852,-319.33758068225)) ;
#24542 = CARTESIAN_POINT('Ctrl Pts',(6.0672224142105,18.4607172509099,-319.344419276832)) ;
#24543 = CARTESIAN_POINT('Ctrl Pts',(7.0849251195189,18.0953242375593,-319.358357129462)) ;
#24544 = CARTESIAN_POINT('Ctrl Pts',(7.59758239100315,17.8861306180735,-319.365445277847)) ;
#24545 = CARTESIAN_POINT('Ctrl Pts',(8.24053287680013,17.5911325318351,-319.374319232124)) ;
#24546 = CARTESIAN_POINT('Ctrl Pts',(8.37969030386068,17.5252707923306,-319.376239541859)) ;
#24547 = CARTESIAN_POINT('Ctrl Pts',(8.6314383181823,17.4024370490482,-319.379712491934)) ;
#24548 = CARTESIAN_POINT('Ctrl Pts',(8.74428481201609,17.3460089317986,-319.381268866787)) ;
#24549 = CARTESIAN_POINT('Ctrl Pts',(8.9747747816275,17.2279331524601,-319.384447379039)) ;
#24550 = CARTESIAN_POINT('Ctrl Pts',(9.09235189995542,17.1661702213987,-319.386068577443)) ;
#24551 = CARTESIAN_POINT('Ctrl Pts',(9.39820217234182,17.0014839796763,-319.390286683647)) ;
#24552 = CARTESIAN_POINT('Ctrl Pts',(9.5854197004372,16.8966384515679,-319.392869480552)) ;
#24553 = CARTESIAN_POINT('Ctrl Pts',(9.89523116576786,16.7163312944322,-319.397152253011)) ;
#24554 = CARTESIAN_POINT('Ctrl Pts',(10.0187922188998,16.6425699426894,-319.398862753759)) ;
#24555 = CARTESIAN_POINT('Ctrl Pts',(10.5367482879582,16.3255105618358,-319.406051458614)) ;
#24556 = CARTESIAN_POINT('Ctrl Pts',(10.9231907820573,16.0695134679488,-319.411456733147)) ;
#24557 = CARTESIAN_POINT('Ctrl Pts',(11.4393971990231,15.7003229998558,-319.418870291716)) ;
#24558 = CARTESIAN_POINT('Ctrl Pts',(11.5773630273631,15.5988658520796,-319.420871955883)) ;
#24559 = CARTESIAN_POINT('Ctrl Pts',(11.9765916353141,15.297067129635,-319.426743336963)) ;
#24560 = CARTESIAN_POINT('Ctrl Pts',(12.2341240503698,15.0918924515503,-319.430631320507)) ;
#24561 = CARTESIAN_POINT('Ctrl Pts',(12.5622626184348,14.8165452073739,-319.435791589205)) ;
#24562 = CARTESIAN_POINT('Ctrl Pts',(12.6377194030083,14.7522371940441,-319.436992976174)) ;
#24563 = CARTESIAN_POINT('Ctrl Pts',(12.763012126789,14.6437897283367,-319.439015543221)) ;
#24564 = CARTESIAN_POINT('Ctrl Pts',(12.8131194532447,14.5999666452216,-319.439831995936)) ;
#24565 = CARTESIAN_POINT('Ctrl Pts',(12.9220889498549,14.5036705745683,-319.441624961875)) ;
#24566 = CARTESIAN_POINT('Ctrl Pts',(12.9808587361702,14.4510950939438,-319.442602975731)) ;
#24567 = CARTESIAN_POINT('Ctrl Pts',(13.1626774036782,14.2864359408839,-319.445660845915)) ;
#24568 = CARTESIAN_POINT('Ctrl Pts',(13.2846068537678,14.173127704085,-319.447757731575)) ;
#24569 = CARTESIAN_POINT('Ctrl Pts',(13.501065969841,13.9667261222266,-319.451552621445)) ;
#24570 = CARTESIAN_POINT('Ctrl Pts',(13.5961268684638,13.8742046626275,-319.453245088027)) ;
#24571 = CARTESIAN_POINT('Ctrl Pts',(14.1026834695256,13.3709741176509,-319.46238856836)) ;
#24572 = CARTESIAN_POINT('Ctrl Pts',(14.496531456211,12.942921118733,-319.469937593148)) ;
#24573 = CARTESIAN_POINT('Ctrl Pts',(15.124775587694,12.1954037912678,-319.482456125675)) ;
#24574 = CARTESIAN_POINT('Ctrl Pts',(15.3696779437044,11.885272879332,-319.487476581644)) ;
#24575 = CARTESIAN_POINT('Ctrl Pts',(15.699803610784,11.4399370657213,-319.494417871668)) ;
#24576 = CARTESIAN_POINT('Ctrl Pts',(15.7930770486984,11.3108227338175,-319.496400326873)) ;
#24577 = CARTESIAN_POINT('Ctrl Pts',(15.9564245101839,11.0787475722964,-319.499910428903)) ;
#24578 = CARTESIAN_POINT('Ctrl Pts',(16.0271161498356,10.9762324541092,-319.501442864822)) ;
#24579 = CARTESIAN_POINT('Ctrl Pts',(16.1762175280855,10.7554978102815,-319.504704586036)) ;
#24580 = CARTESIAN_POINT('Ctrl Pts',(16.2543279150401,10.6370846927523,-319.506431482649)) ;
#24581 = CARTESIAN_POINT('Ctrl Pts',(16.4752218762355,10.2941004329853,-319.511370527203)) ;
#24582 = CARTESIAN_POINT('Ctrl Pts',(16.6146969759507,10.0674368322498,-319.514557737471)) ;
#24583 = CARTESIAN_POINT('Ctrl Pts',(16.9390313838352,9.51524722024922,-319.522163407105)) ;
#24584 = CARTESIAN_POINT('Ctrl Pts',(17.1192242493347,9.18710375889944,-319.526553240275)) ;
#24585 = CARTESIAN_POINT('Ctrl Pts',(17.5762887518579,8.29455790863486,-319.538274792425)) ;
#24586 = CARTESIAN_POINT('Ctrl Pts',(17.835434727826,7.72158530093575,-319.545564656954)) ;
#24587 = CARTESIAN_POINT('Ctrl Pts',(18.1055920530098,7.03772475473517,-319.554405862526)) ;
#24588 = CARTESIAN_POINT('Ctrl Pts',(18.1440156535216,6.93806379558523,-319.555698077377)) ;
#24589 = CARTESIAN_POINT('Ctrl Pts',(18.2052237415366,6.77531926819771,-319.557817831679)) ;
#24590 = CARTESIAN_POINT('Ctrl Pts',(18.2285069520863,6.71242556551517,-319.558639365612)) ;
#24591 = CARTESIAN_POINT('Ctrl Pts',(18.2772007207493,6.57876976234691,-319.560391185835)) ;
#24592 = CARTESIAN_POINT('Ctrl Pts',(18.3025270558299,6.5079782670706,-319.56132243007)) ;
#24593 = CARTESIAN_POINT('Ctrl Pts',(18.3757438360789,6.2995166226579,-319.564072687228)) ;
#24594 = CARTESIAN_POINT('Ctrl Pts',(18.4224964161285,6.16145249913778,-319.565904363065)) ;
#24595 = CARTESIAN_POINT('Ctrl Pts',(18.5015169430172,5.91915517059847,-319.569128821231)) ;
#24596 = CARTESIAN_POINT('Ctrl Pts',(18.5344688824556,5.81515178982918,-319.570516063413)) ;
#24597 = CARTESIAN_POINT('Ctrl Pts',(18.684680673011,5.32680053795363,-319.577036745979)) ;
#24598 = CARTESIAN_POINT('Ctrl Pts',(18.7908721890419,4.93915153764358,-319.582230471955)) ;
#24599 = CARTESIAN_POINT('Ctrl Pts',(18.9276947719951,4.37107506445579,-319.58976736749)) ;
#24600 = CARTESIAN_POINT('Ctrl Pts',(18.9679231742898,4.1930677438476,-319.592118989836)) ;
#24601 = CARTESIAN_POINT('Ctrl Pts',(19.0957257404718,3.58802175684998,-319.60006284774)) ;
#24602 = CARTESIAN_POINT('Ctrl Pts',(19.1714323752068,3.15861110030695,-319.60561513026)) ;
#24603 = CARTESIAN_POINT('Ctrl Pts',(19.255610793609,2.56493228343429,-319.613129698851)) ;
#24604 = CARTESIAN_POINT('Ctrl Pts',(19.2765431084871,2.40256332806498,-319.615168827079)) ;
#24605 = CARTESIAN_POINT('Ctrl Pts',(19.3098362399808,2.11576887111567,-319.618741893899)) ;
#24606 = CARTESIAN_POINT('Ctrl Pts',(19.3230528431689,1.99145233401034,-319.620281258418)) ;
#24607 = CARTESIAN_POINT('Ctrl Pts',(19.3484645527746,1.72828536821113,-319.623520490304)) ;
#24608 = CARTESIAN_POINT('Ctrl Pts',(19.3603671214867,1.58941368103535,-319.625218378177)) ;
#24609 = CARTESIAN_POINT('Ctrl Pts',(19.3895556127815,1.19959459489223,-319.629954464472)) ;
#24610 = CARTESIAN_POINT('Ctrl Pts',(19.4034633545706,0.948421966995108,-319.632971044759)) ;
#24611 = CARTESIAN_POINT('Ctrl Pts',(19.4247704260956,0.355030743297774,-319.640033855164)) ;
#24612 = CARTESIAN_POINT('Ctrl Pts',(19.4280104723781,0.0127464750800942,
-319.644057303709)) ;
#24613 = CARTESIAN_POINT('Ctrl Pts',(19.4109258119925,-0.994469447955966,
-319.65584664851)) ;
#24614 = CARTESIAN_POINT('Ctrl Pts',(19.3654968887435,-1.65847345045228,-319.663542447662)) ;
#24615 = CARTESIAN_POINT('Ctrl Pts',(19.2721535258711,-2.43482484567934,-319.672924137038)) ;
#24616 = CARTESIAN_POINT('Ctrl Pts',(19.2571613486127,-2.55068819893634,-319.674334881957)) ;
#24617 = CARTESIAN_POINT('Ctrl Pts',(19.2325126297362,-2.72855628319807,-319.676521203806)) ;
#24618 = CARTESIAN_POINT('Ctrl Pts',(19.2235993182903,-2.79066133423313,-319.677288462859)) ;
#24619 = CARTESIAN_POINT('Ctrl Pts',(19.2040999190519,-2.9219986890197,-319.678920192542)) ;
#24620 = CARTESIAN_POINT('Ctrl Pts',(19.1934399819546,-2.99121909490093,-319.679785621922)) ;
#24621 = CARTESIAN_POINT('Ctrl Pts',(19.1636187141323,-3.17813824201646,-319.682135859549)) ;
#24622 = CARTESIAN_POINT('Ctrl Pts',(19.1437475537222,-3.29572062565021,-319.683628527363)) ;
#24623 = CARTESIAN_POINT('Ctrl Pts',(19.0516453757676,-3.81174554693782,-319.6902310191)) ;
#24624 = CARTESIAN_POINT('Ctrl Pts',(18.9680483907105,-4.20805595952492,-319.69543564422)) ;
#24625 = CARTESIAN_POINT('Ctrl Pts',(18.696546370881,-5.3215759478819,-319.710212277407)) ;
#24626 = CARTESIAN_POINT('Ctrl Pts',(18.479892395138,-6.03105317827658,-319.719789401176)) ;
#24627 = CARTESIAN_POINT('Ctrl Pts',(18.1618668340894,-6.89264958180068,-319.731323128647)) ;
#24628 = CARTESIAN_POINT('Ctrl Pts',(18.0982345214657,-7.05804027300622,-319.733534096698)) ;
#24629 = CARTESIAN_POINT('Ctrl Pts',(17.9853395516464,-7.33990263142604,-319.737296169189)) ;
#24630 = CARTESIAN_POINT('Ctrl Pts',(17.937186216287,-7.45680629481606,-319.738854764944)) ;
#24631 = CARTESIAN_POINT('Ctrl Pts',(17.835238496018,-7.69760575949502,-319.742061997978)) ;
#24632 = CARTESIAN_POINT('Ctrl Pts',(17.7812862177421,-7.82142743621631,-319.743709426064)) ;
#24633 = CARTESIAN_POINT('Ctrl Pts',(17.6331611894406,-8.15192185233348,-319.748103536506)) ;
#24634 = CARTESIAN_POINT('Ctrl Pts',(17.5366479334065,-8.35752253527709,-319.750833701538)) ;
#24635 = CARTESIAN_POINT('Ctrl Pts',(17.3676193906738,-8.70177470242162,-319.755408402899)) ;
#24636 = CARTESIAN_POINT('Ctrl Pts',(17.2969940729034,-8.84132808906969,-319.757263924998)) ;
#24637 = CARTESIAN_POINT('Ctrl Pts',(16.9754634801301,-9.45806048023715,-319.765480305192)) ;
#24638 = CARTESIAN_POINT('Ctrl Pts',(16.7064424421542,-9.92552513051495,-319.771744703688)) ;
#24639 = CARTESIAN_POINT('Ctrl Pts',(16.2286623120334,-10.6811560918468,-319.782210097808)) ;
#24640 = CARTESIAN_POINT('Ctrl Pts',(16.0308128962793,-10.9758650115822,-319.786384723742)) ;
#24641 = CARTESIAN_POINT('Ctrl Pts',(15.7574815395629,-11.3598396332507,-319.792040093532)) ;
#24642 = CARTESIAN_POINT('Ctrl Pts',(15.689109800906,-11.454082877267,-319.793446143421)) ;
#24643 = CARTESIAN_POINT('Ctrl Pts',(15.5826388633039,-11.5980997861228,-319.795626875622)) ;
#24644 = CARTESIAN_POINT('Ctrl Pts',(15.5451390825901,-11.6483133321948,-319.796393306092)) ;
#24645 = CARTESIAN_POINT('Ctrl Pts',(15.4651690207367,-11.754322135218,-319.798025258767)) ;
#24646 = CARTESIAN_POINT('Ctrl Pts',(15.422638318519,-11.8100706589939,-319.798891756021)) ;
#24647 = CARTESIAN_POINT('Ctrl Pts',(15.3067061273003,-11.9603383706976,-319.801248414546)) ;
#24648 = CARTESIAN_POINT('Ctrl Pts',(15.2327315358329,-12.0544114871995,-319.802746505928)) ;
#24649 = CARTESIAN_POINT('Ctrl Pts',(14.9022893818169,-12.4667337797591,-319.80940263346)) ;
#24650 = CARTESIAN_POINT('Ctrl Pts',(14.6366840169162,-12.7775255823434,-319.814657122216)) ;
#24651 = CARTESIAN_POINT('Ctrl Pts',(13.8676023164714,-13.6219747008256,-319.829383771116)) ;
#24652 = CARTESIAN_POINT('Ctrl Pts',(13.3434123698215,-14.1358389693269,-319.838859027163)) ;
#24653 = CARTESIAN_POINT('Ctrl Pts',(12.6570262819971,-14.736424319879,-319.850315376833)) ;
#24654 = CARTESIAN_POINT('Ctrl Pts',(12.5210150489641,-14.8521614022319,-319.85254399068)) ;
#24655 = CARTESIAN_POINT('Ctrl Pts',(12.2858598279487,-15.0467375248484,-319.85632626538)) ;
#24656 = CARTESIAN_POINT('Ctrl Pts',(12.1875052902613,-15.1265123773828,-319.857887629423)) ;
#24657 = CARTESIAN_POINT('Ctrl Pts',(11.997661978307,-15.2774396630474,-319.86086265066)) ;
#24658 = CARTESIAN_POINT('Ctrl Pts',(11.9063026660171,-15.3487462832055,-319.862277542121)) ;
#24659 = CARTESIAN_POINT('Ctrl Pts',(11.6709892955055,-15.5290448493576,-319.865880176186)) ;
#24660 = CARTESIAN_POINT('Ctrl Pts',(11.5261437010686,-15.636855073254,-319.868058406599)) ;
#24661 = CARTESIAN_POINT('Ctrl Pts',(11.1927040063727,-15.877887371847,-319.87298960823)) ;
#24662 = CARTESIAN_POINT('Ctrl Pts',(11.0031952466678,-16.0097977796998,-319.875733059635)) ;
#24663 = CARTESIAN_POINT('Ctrl Pts',(10.3488665902215,-16.4481460757579,-319.885033523324)) ;
#24664 = CARTESIAN_POINT('Ctrl Pts',(9.87324753800785,-16.7379667709284,-319.891497081867)) ;
#24665 = CARTESIAN_POINT('Ctrl Pts',(9.06903814116813,-17.181795687896,-319.902258499843)) ;
#24666 = CARTESIAN_POINT('Ctrl Pts',(8.74741430706783,-17.347746182655,-319.906522608289)) ;
#24667 = CARTESIAN_POINT('Ctrl Pts',(8.33090634608313,-17.5481251578087,-319.912088834451)) ;
#24668 = CARTESIAN_POINT('Ctrl Pts',(8.24013246321081,-17.5909327225883,-319.913304658191)) ;
#24669 = CARTESIAN_POINT('Ctrl Pts',(8.08942883746605,-17.660579753382,-319.915330616156)) ;
#24670 = CARTESIAN_POINT('Ctrl Pts',(8.02968740904654,-17.687822258951,-319.916135703589)) ;
#24671 = CARTESIAN_POINT('Ctrl Pts',(7.92432589743704,-17.7352240328544,-319.917559677219)) ;
#24672 = CARTESIAN_POINT('Ctrl Pts',(7.87876427070972,-17.7555114256233,-319.91817671134)) ;
#24673 = CARTESIAN_POINT('Ctrl Pts',(7.82757692958262,-17.7780679819389,-319.918871132564)) ;
#24674 = CARTESIAN_POINT('Ctrl Pts',(7.82202767007425,-17.7805102538582,-319.918946431086)) ;
#24675 = CARTESIAN_POINT('Ctrl Pts',(7.81074339996243,-17.7854702431278,-319.919099579988)) ;
#24676 = CARTESIAN_POINT('Ctrl Pts',(7.8050083132647,-17.7879877855563,-319.919177432436)) ;
#24677 = CARTESIAN_POINT('Ctrl Pts',(7.79323018271909,-17.7931512621709,-319.91933735082)) ;
#24678 = CARTESIAN_POINT('Ctrl Pts',(7.78718700660935,-17.7957968926211,-319.919419420311)) ;
#24679 = CARTESIAN_POINT('Ctrl Pts',(7.77466165931191,-17.8012727385397,-319.919589557151)) ;
#24680 = CARTESIAN_POINT('Ctrl Pts',(7.76817928770987,-17.8041024930389,-319.919677629826)) ;
#24681 = CARTESIAN_POINT('Ctrl Pts',(7.75462795187441,-17.8100092578932,-319.919861785609)) ;
#24682 = CARTESIAN_POINT('Ctrl Pts',(7.74755869847941,-17.8130856016534,-319.919957876307)) ;
#24683 = CARTESIAN_POINT('Ctrl Pts',(7.73266172770501,-17.819557806239,-319.920160414594)) ;
#24684 = CARTESIAN_POINT('Ctrl Pts',(7.72483360061325,-17.8229527196764,-319.920266872797)) ;
#24685 = CARTESIAN_POINT('Ctrl Pts',(7.71387065905006,-17.8276985645229,-319.920415999903)) ;
#24686 = CARTESIAN_POINT('Ctrl Pts',(7.7107377209296,-17.8290538293841,-319.920458620996)) ;
#24687 = CARTESIAN_POINT('Ctrl Pts',(7.70343575019896,-17.8322102743221,-319.920557968169)) ;
#24688 = CARTESIAN_POINT('Ctrl Pts',(7.69926644293814,-17.8340108182575,-319.920614701209)) ;
#24689 = CARTESIAN_POINT('Ctrl Pts',(7.60415275072753,-17.8750467479181,-319.921909108167)) ;
#24690 = CARTESIAN_POINT('Ctrl Pts',(7.51291029900293,-17.9135874157695,-319.923154281409)) ;
#24691 = CARTESIAN_POINT('Ctrl Pts',(7.25010073708382,-18.0222366455581,-319.926746682547)) ;
#24692 = CARTESIAN_POINT('Ctrl Pts',(7.07781985777919,-18.0905898278586,-319.929108699088)) ;
#24693 = CARTESIAN_POINT('Ctrl Pts',(6.34432215931883,-18.3695261993673,-319.939159988119)) ;
#24694 = CARTESIAN_POINT('Ctrl Pts',(5.77449513429753,-18.5565385838466,-319.946945282641)) ;
#24695 = CARTESIAN_POINT('Ctrl Pts',(4.83650765202176,-18.8169801384299,-319.959413796065)) ;
#24696 = CARTESIAN_POINT('Ctrl Pts',(4.47326465659935,-18.9066245590628,-319.964162979456)) ;
#24697 = CARTESIAN_POINT('Ctrl Pts',(3.9524197161255,-19.0193120515089,-319.970834996176)) ;
#24698 = CARTESIAN_POINT('Ctrl Pts',(3.79677353791587,-19.0509937620902,-319.972811781925)) ;
#24699 = CARTESIAN_POINT('Ctrl Pts',(3.51847864256827,-19.10409456639,-319.976315703288)) ;
#24700 = CARTESIAN_POINT('Ctrl Pts',(3.39597955153457,-19.1262501314918,-319.977847563879)) ;
#24701 = CARTESIAN_POINT('Ctrl Pts',(3.15827358304186,-19.1668866803756,-319.980800302581)) ;
#24702 = CARTESIAN_POINT('Ctrl Pts',(3.04309642511415,-19.185510189436,-319.982222054245)) ;
#24703 = CARTESIAN_POINT('Ctrl Pts',(2.78826725108276,-19.2243621692534,-319.985348862049)) ;
#24704 = CARTESIAN_POINT('Ctrl Pts',(2.64854841155588,-19.2441088765399,-319.987050791772)) ;
#24705 = CARTESIAN_POINT('Ctrl Pts',(1.67666385417762,-19.3706821099435,-319.998811253086)) ;
#24706 = CARTESIAN_POINT('Ctrl Pts',(0.838559641495929,-19.4250183449035,
-320.008511425644)) ;
#24707 = CARTESIAN_POINT('Ctrl Pts',(-0.00042484694712408,-19.4249999953541,
-320.018354222948)) ;
#24708 = CARTESIAN_POINT('Origin',(0.,0.,-328.125)) ;
#24709 = CARTESIAN_POINT('',(0.000290047970874232,-19.4246600253745,-321.730568038795)) ;
#24710 = CARTESIAN_POINT('',(0.0001668108406198,-19.4249999992838,-321.519753599958)) ;
#24711 = CARTESIAN_POINT('',(-2.37887640734373E-15,-19.425,-328.125)) ;
#24712 = CARTESIAN_POINT('Ctrl Pts',(0.000290047970874162,-19.4246600253745,
-321.730568038795)) ;
#24713 = CARTESIAN_POINT('Ctrl Pts',(0.414032815414898,-19.4247115091692,
-321.725584231456)) ;
#24714 = CARTESIAN_POINT('Ctrl Pts',(0.827728246191239,-19.4115727824527,
-321.720657750041)) ;
#24715 = CARTESIAN_POINT('Ctrl Pts',(1.24054323851937,-19.3852594821658,-321.715754611829)) ;
#24716 = CARTESIAN_POINT('Ctrl Pts',(1.67062772321509,-19.3578454046617,-321.710646358227)) ;
#24717 = CARTESIAN_POINT('Ctrl Pts',(2.09975668298582,-19.3161309520273,-321.705563481343)) ;
#24718 = CARTESIAN_POINT('Ctrl Pts',(2.52698399798445,-19.260178292411,-321.700440001018)) ;
#24719 = CARTESIAN_POINT('Ctrl Pts',(2.95421131298308,-19.2042256327946,-321.695316520694)) ;
#24720 = CARTESIAN_POINT('Ctrl Pts',(3.37953703303916,-19.1340344813326,-321.690152193862)) ;
#24721 = CARTESIAN_POINT('Ctrl Pts',(3.80200981619182,-19.049715863574,-321.68485585614)) ;
#24722 = CARTESIAN_POINT('Ctrl Pts',(4.19783357195257,-18.9707159533011,-321.679893604435)) ;
#24723 = CARTESIAN_POINT('Ctrl Pts',(4.59123122171946,-18.8792986800034,-321.674814568772)) ;
#24724 = CARTESIAN_POINT('Ctrl Pts',(4.98142637903984,-18.775681116706,-321.669695206077)) ;
#24725 = CARTESIAN_POINT('Ctrl Pts',(5.37132596310663,-18.6721420438249,-321.664579721305)) ;
#24726 = CARTESIAN_POINT('Ctrl Pts',(5.75802798036154,-18.556421336585,-321.659424136884)) ;
#24727 = CARTESIAN_POINT('Ctrl Pts',(6.14077663098242,-18.4287730500008,-321.654284881139)) ;
#24728 = CARTESIAN_POINT('Ctrl Pts',(6.52348420669083,-18.3011384620729,-321.649146176917)) ;
#24729 = CARTESIAN_POINT('Ctrl Pts',(6.9022393361505,-18.1615789550527,-321.644023901516)) ;
#24730 = CARTESIAN_POINT('Ctrl Pts',(7.27630416981867,-18.0103839021878,-321.638952587994)) ;
#24731 = CARTESIAN_POINT('Ctrl Pts',(7.65034627061387,-17.8591980378316,-321.63388158267)) ;
#24732 = CARTESIAN_POINT('Ctrl Pts',(8.01969870178435,-17.6963780755871,-321.628861579192)) ;
#24733 = CARTESIAN_POINT('Ctrl Pts',(8.38364048306132,-17.5222477356751,-321.623904110283)) ;
#24734 = CARTESIAN_POINT('Ctrl Pts',(8.74815140582929,-17.3478450862719,-321.618938888757)) ;
#24735 = CARTESIAN_POINT('Ctrl Pts',(9.1072347687062,-17.1620966214322,-321.614036396023)) ;
#24736 = CARTESIAN_POINT('Ctrl Pts',(9.46018237293682,-16.9653621203275,-321.609184808469)) ;
#24737 = CARTESIAN_POINT('Ctrl Pts',(9.81261504025612,-16.768914647255,-321.604340299193)) ;
#24738 = CARTESIAN_POINT('Ctrl Pts',(10.1589298376583,-16.561513099192,-321.59954647939)) ;
#24739 = CARTESIAN_POINT('Ctrl Pts',(10.4984375697143,-16.3435508740133,-321.59476878525)) ;
#24740 = CARTESIAN_POINT('Ctrl Pts',(10.838689380338,-16.1251109542049,-321.589980620126)) ;
#24741 = CARTESIAN_POINT('Ctrl Pts',(11.1721041965684,-15.896063872729,-321.585208539037)) ;
#24742 = CARTESIAN_POINT('Ctrl Pts',(11.4980047302109,-15.6568426433194,-321.58039616376)) ;
#24743 = CARTESIAN_POINT('Ctrl Pts',(11.8239052638534,-15.4176214139098,-321.575583788484)) ;
#24744 = CARTESIAN_POINT('Ctrl Pts',(12.1422913996453,-15.1682258645773,-321.570730933245)) ;
#24745 = CARTESIAN_POINT('Ctrl Pts',(12.4525035634766,-14.9091283489994,-321.565761898795)) ;
#24746 = CARTESIAN_POINT('Ctrl Pts',(12.7622922869302,-14.6503845021767,-321.560799647089)) ;
#24747 = CARTESIAN_POINT('Ctrl Pts',(13.064009807143,-14.3818973205538,-321.555720611426)) ;
#24748 = CARTESIAN_POINT('Ctrl Pts',(13.3570782099071,-14.1042288644385,-321.550601248731)) ;
#24749 = CARTESIAN_POINT('Ctrl Pts',(13.6499246130387,-13.8267707424795,-321.545485763959)) ;
#24750 = CARTESIAN_POINT('Ctrl Pts',(13.9341351493772,-13.5401453715385,-321.540330179538)) ;
#24751 = CARTESIAN_POINT('Ctrl Pts',(14.2091676755129,-13.2449374377241,-321.535190923794)) ;
#24752 = CARTESIAN_POINT('Ctrl Pts',(14.4841706863594,-12.9497611843355,-321.530052219571)) ;
#24753 = CARTESIAN_POINT('Ctrl Pts',(14.7499977679495,-12.6460042637827,-321.52492994417)) ;
#24754 = CARTESIAN_POINT('Ctrl Pts',(15.0061394366358,-12.3342737882764,-321.519858630649)) ;
#24755 = CARTESIAN_POINT('Ctrl Pts',(15.2622655389404,-12.0225622574252,-321.514787625324)) ;
#24756 = CARTESIAN_POINT('Ctrl Pts',(15.5087074709339,-11.7028781435391,-321.509767621847)) ;
#24757 = CARTESIAN_POINT('Ctrl Pts',(15.7449869947941,-11.3758506492204,-321.504810152937)) ;
#24758 = CARTESIAN_POINT('Ctrl Pts',(15.9816360186343,-11.0483117409178,-321.499844931411)) ;
#24759 = CARTESIAN_POINT('Ctrl Pts',(16.2080908308918,-10.7134064234155,-321.494942438677)) ;
#24760 = CARTESIAN_POINT('Ctrl Pts',(16.4239016690412,-10.3717894487278,-321.490090851123)) ;
#24761 = CARTESIAN_POINT('Ctrl Pts',(16.6393976475192,-10.0306708800022,-321.485246341847)) ;
#24762 = CARTESIAN_POINT('Ctrl Pts',(16.844280651551,-9.68286016179965,-321.480452522044)) ;
#24763 = CARTESIAN_POINT('Ctrl Pts',(17.0381336899874,-9.32903247602731,-321.475674827904)) ;
#24764 = CARTESIAN_POINT('Ctrl Pts',(17.2324115844077,-8.97442932750882,-321.470886662781)) ;
#24765 = CARTESIAN_POINT('Ctrl Pts',(17.4156109923312,-8.61378271078743,-321.466114581691)) ;
#24766 = CARTESIAN_POINT('Ctrl Pts',(17.5873443318877,-8.24779689888392,-321.461302206415)) ;
#24767 = CARTESIAN_POINT('Ctrl Pts',(17.7590776714444,-7.88181108697985,-321.456489831139)) ;
#24768 = CARTESIAN_POINT('Ctrl Pts',(17.9193447591344,-7.51048598400925,-321.4516369759)) ;
#24769 = CARTESIAN_POINT('Ctrl Pts',(18.0677923895257,-7.1345519336756,-321.446667941449)) ;
#24770 = CARTESIAN_POINT('Ctrl Pts',(18.2160373885304,-6.75913103426062,-321.441705689744)) ;
#24771 = CARTESIAN_POINT('Ctrl Pts',(18.3525333826738,-6.37901569349928,-321.436626654081)) ;
#24772 = CARTESIAN_POINT('Ctrl Pts',(18.4770417922726,-5.99497596097233,-321.431507291386)) ;
#24773 = CARTESIAN_POINT('Ctrl Pts',(18.6014558866162,-5.61122713895869,-321.426391806614)) ;
#24774 = CARTESIAN_POINT('Ctrl Pts',(18.7139007423434,-5.22355990194548,-321.421236222193)) ;
#24775 = CARTESIAN_POINT('Ctrl Pts',(18.8141800158724,-4.8327470542551,-321.416096966448)) ;
#24776 = CARTESIAN_POINT('Ctrl Pts',(18.9144485278681,-4.4419761468915,-321.410958262225)) ;
#24777 = CARTESIAN_POINT('Ctrl Pts',(19.002554191957,-4.04806029795157,-321.405835986825)) ;
#24778 = CARTESIAN_POINT('Ctrl Pts',(19.0783400732297,-3.65177637953315,-321.400764673303)) ;
#24779 = CARTESIAN_POINT('Ctrl Pts',(19.154121348801,-3.25551654429931,-321.395693667978)) ;
#24780 = CARTESIAN_POINT('Ctrl Pts',(19.2175843977007,-2.85688889856963,-321.390673664501)) ;
#24781 = CARTESIAN_POINT('Ctrl Pts',(19.2686102914582,-2.45667476388441,-321.385716195592)) ;
#24782 = CARTESIAN_POINT('Ctrl Pts',(19.3197159808173,-2.05583476406919,-321.380750974066)) ;
#24783 = CARTESIAN_POINT('Ctrl Pts',(19.3583455699864,-1.65340326862375,-321.375848481332)) ;
#24784 = CARTESIAN_POINT('Ctrl Pts',(19.3844173589335,-1.25017041148229,-321.370996893778)) ;
#24785 = CARTESIAN_POINT('Ctrl Pts',(19.4104511101483,-0.847525855492989,
-321.366152384502)) ;
#24786 = CARTESIAN_POINT('Ctrl Pts',(19.4239636157988,-0.444082237091322,
-321.361358564699)) ;
#24787 = CARTESIAN_POINT('Ctrl Pts',(19.4249117274997,-0.0406319516599588,
-321.356580870559)) ;
#24788 = CARTESIAN_POINT('Ctrl Pts',(19.4258619171197,0.363702551368296,-321.351792705436)) ;
#24789 = CARTESIAN_POINT('Ctrl Pts',(19.4141924266424,0.768043778808558,-321.347020624346)) ;
#24790 = CARTESIAN_POINT('Ctrl Pts',(19.3898998507143,1.17158785965311,-321.34220824907)) ;
#24791 = CARTESIAN_POINT('Ctrl Pts',(19.3656072747863,1.57513194049767,-321.337395873794)) ;
#24792 = CARTESIAN_POINT('Ctrl Pts',(19.3286914063978,1.9778788711547,-321.332543018555)) ;
#24793 = CARTESIAN_POINT('Ctrl Pts',(19.2791914999854,2.37901833372837,-321.327573984104)) ;
#24794 = CARTESIAN_POINT('Ctrl Pts',(19.229759161069,2.7796102399332,-321.322611732398)) ;
#24795 = CARTESIAN_POINT('Ctrl Pts',(19.1677637480264,3.17870345894468,-321.317532696735)) ;
#24796 = CARTESIAN_POINT('Ctrl Pts',(19.0933641677198,3.57550764575502,-321.312413334041)) ;
#24797 = CARTESIAN_POINT('Ctrl Pts',(19.0190209451758,3.97201125296411,-321.307297849269)) ;
#24798 = CARTESIAN_POINT('Ctrl Pts',(18.9322925248851,4.36622935674251,-321.302142264847)) ;
#24799 = CARTESIAN_POINT('Ctrl Pts',(18.8333762203775,4.7573893998477,-321.297003009103)) ;
#24800 = CARTESIAN_POINT('Ctrl Pts',(18.7344705311356,5.14850746536595,-321.29186430488)) ;
#24801 = CARTESIAN_POINT('Ctrl Pts',(18.6233796788519,5.53656819080653,-321.286742029479)) ;
#24802 = CARTESIAN_POINT('Ctrl Pts',(18.5003375290666,5.92081430096648,-321.281670715958)) ;
#24803 = CARTESIAN_POINT('Ctrl Pts',(18.3773028568661,6.30503705951135,-321.276599710633)) ;
#24804 = CARTESIAN_POINT('Ctrl Pts',(18.2423183775642,6.6854457198535,-321.271579707156)) ;
#24805 = CARTESIAN_POINT('Ctrl Pts',(18.0956534599684,7.06129728281752,-321.266622238246)) ;
#24806 = CARTESIAN_POINT('Ctrl Pts',(17.9487591840125,7.43773661209638,-321.26165701672)) ;
#24807 = CARTESIAN_POINT('Ctrl Pts',(17.790147875683,7.80960460824021,-321.256754523986)) ;
#24808 = CARTESIAN_POINT('Ctrl Pts',(17.6201258112138,8.17616834465075,-321.251902936432)) ;
#24809 = CARTESIAN_POINT('Ctrl Pts',(17.4503518023654,8.54219727873751,-321.247058427156)) ;
#24810 = CARTESIAN_POINT('Ctrl Pts',(17.2692002371063,8.9029374226659,-321.242264607353)) ;
#24811 = CARTESIAN_POINT('Ctrl Pts',(17.0770123269122,9.25767230804478,-321.237486913213)) ;
#24812 = CARTESIAN_POINT('Ctrl Pts',(16.8844032100947,9.61318464442543,-321.23269874809)) ;
#24813 = CARTESIAN_POINT('Ctrl Pts',(16.6807091725345,9.96266532240178,-321.227926667)) ;
#24814 = CARTESIAN_POINT('Ctrl Pts',(16.4663118154245,10.305406810545,-321.223114291724)) ;
#24815 = CARTESIAN_POINT('Ctrl Pts',(16.2519144583145,10.6481482986883,-321.218301916447)) ;
#24816 = CARTESIAN_POINT('Ctrl Pts',(16.0268136015923,10.9841504948062,-321.213449061208)) ;
#24817 = CARTESIAN_POINT('Ctrl Pts',(15.7914313915858,11.312720615757,-321.208480026758)) ;
#24818 = CARTESIAN_POINT('Ctrl Pts',(15.5563704788845,11.6408422376712,-321.203517775052)) ;
#24819 = CARTESIAN_POINT('Ctrl Pts',(15.3109945784651,11.9616373376846,-321.198438739389)) ;
#24820 = CARTESIAN_POINT('Ctrl Pts',(15.05582135137,12.2744879160667,-321.193319376694)) ;
#24821 = CARTESIAN_POINT('Ctrl Pts',(14.8008414182699,12.5871015097979,-321.188203891922)) ;
#24822 = CARTESIAN_POINT('Ctrl Pts',(14.536079127922,12.8917827560929,-321.183048307501)) ;
#24823 = CARTESIAN_POINT('Ctrl Pts',(14.2620773572675,13.1879476498576,-321.177909051757)) ;
#24824 = CARTESIAN_POINT('Ctrl Pts',(13.9881049912851,13.4840807605007,-321.172770347534)) ;
#24825 = CARTESIAN_POINT('Ctrl Pts',(13.7048951897873,13.7716994532655,-321.167648072133)) ;
#24826 = CARTESIAN_POINT('Ctrl Pts',(13.4130156157825,14.0502506300313,-321.162576758612)) ;
#24827 = CARTESIAN_POINT('Ctrl Pts',(13.1211537800441,14.3287848785315,-321.157505753287)) ;
#24828 = CARTESIAN_POINT('Ctrl Pts',(12.8206232331792,14.5982527781373,-321.15248574981)) ;
#24829 = CARTESIAN_POINT('Ctrl Pts',(12.5120159846361,14.8581307525481,-321.147528280901)) ;
#24830 = CARTESIAN_POINT('Ctrl Pts',(12.2029261281643,15.1184151307991,-321.142563059374)) ;
#24831 = CARTESIAN_POINT('Ctrl Pts',(11.8857342464352,15.3690795755255,-321.13766056664)) ;
#24832 = CARTESIAN_POINT('Ctrl Pts',(11.561059939402,15.6096270128608,-321.132808979086)) ;
#24833 = CARTESIAN_POINT('Ctrl Pts',(11.2368593196308,15.8498235007846,-321.127964469811)) ;
#24834 = CARTESIAN_POINT('Ctrl Pts',(10.9051980271681,16.0799324491565,-321.123170650007)) ;
#24835 = CARTESIAN_POINT('Ctrl Pts',(10.566718465597,16.2994879504073,-321.118392955867)) ;
#24836 = CARTESIAN_POINT('Ctrl Pts',(10.2274970788384,16.5195246381739,-321.113604790744)) ;
#24837 = CARTESIAN_POINT('Ctrl Pts',(9.88142739749476,16.7289614564954,-321.108832709654)) ;
#24838 = CARTESIAN_POINT('Ctrl Pts',(9.52918301685861,16.927359669034,-321.104020334378)) ;
#24839 = CARTESIAN_POINT('Ctrl Pts',(9.176938636223,17.1257578815723,-321.099207959102)) ;
#24840 = CARTESIAN_POINT('Ctrl Pts',(8.8185194470681,17.3131173124428,-321.094355103863)) ;
#24841 = CARTESIAN_POINT('Ctrl Pts',(8.45462759259423,17.489031573986,-321.089386069413)) ;
#24842 = CARTESIAN_POINT('Ctrl Pts',(8.09123245140864,17.6647057121238,-321.084423817707)) ;
#24843 = CARTESIAN_POINT('Ctrl Pts',(7.72228461027938,17.8290112787533,-321.079344782044)) ;
#24844 = CARTESIAN_POINT('Ctrl Pts',(7.3485343084101,17.9816532522498,-321.074225419349)) ;
#24845 = CARTESIAN_POINT('Ctrl Pts',(6.97506712280469,18.1341795992839,-321.069109934577)) ;
#24846 = CARTESIAN_POINT('Ctrl Pts',(6.59680479711167,18.2750602054356,-321.063954350156)) ;
#24847 = CARTESIAN_POINT('Ctrl Pts',(6.21450344947429,18.4040419646482,-321.058815094411)) ;
#24848 = CARTESIAN_POINT('Ctrl Pts',(5.83224312874678,18.533009882102,-321.053676390189)) ;
#24849 = CARTESIAN_POINT('Ctrl Pts',(5.44594465608023,18.6500816297685,-321.048554114788)) ;
#24850 = CARTESIAN_POINT('Ctrl Pts',(5.05637112832498,18.7550431001519,-321.043482801267)) ;
#24851 = CARTESIAN_POINT('Ctrl Pts',(4.66682127594615,18.8599981917593,-321.038411795942)) ;
#24852 = CARTESIAN_POINT('Ctrl Pts',(4.27399674213582,18.9528445387418,-321.033391792465)) ;
#24853 = CARTESIAN_POINT('Ctrl Pts',(3.87866787909253,19.0334056054948,-321.028434323556)) ;
#24854 = CARTESIAN_POINT('Ctrl Pts',(3.48272079062339,19.1140926557123,-321.023469102029)) ;
#24855 = CARTESIAN_POINT('Ctrl Pts',(3.08426149227695,19.1824559591042,-321.018566609295)) ;
#24856 = CARTESIAN_POINT('Ctrl Pts',(2.68407188485392,19.2383554525851,-321.013715021741)) ;
#24857 = CARTESIAN_POINT('Ctrl Pts',(2.28446613860959,19.2941733908642,-321.008870512465)) ;
#24858 = CARTESIAN_POINT('Ctrl Pts',(1.88313508674887,19.3375638027708,-321.004076692662)) ;
#24859 = CARTESIAN_POINT('Ctrl Pts',(1.48086574387704,19.3684249030544,-320.999298998522)) ;
#24860 = CARTESIAN_POINT('Ctrl Pts',(1.07771477159253,19.3993536397468,-320.994510833399)) ;
#24861 = CARTESIAN_POINT('Ctrl Pts',(0.673621351637577,19.4176979351181,-320.989738752309)) ;
#24862 = CARTESIAN_POINT('Ctrl Pts',(0.269386889573299,19.4233947866315,-320.984926377033)) ;
#24863 = CARTESIAN_POINT('Ctrl Pts',(-0.134847572490978,19.4290916381448,
-320.980114001757)) ;
#24864 = CARTESIAN_POINT('Ctrl Pts',(-0.53922308843213,19.4221408390945,-320.975261146517)) ;
#24865 = CARTESIAN_POINT('Ctrl Pts',(-0.942928660350018,19.4025214512654,
-320.970292112067)) ;
#24866 = CARTESIAN_POINT('Ctrl Pts',(-1.34608317314376,19.3829288439501,-320.965329860361)) ;
#24867 = CARTESIAN_POINT('Ctrl Pts',(-1.7486746688856,19.3506966200822,-320.960250824698)) ;
#24868 = CARTESIAN_POINT('Ctrl Pts',(-2.14990319542456,19.3059246454638,-320.955131462003)) ;
#24869 = CARTESIAN_POINT('Ctrl Pts',(-2.55082779093171,19.2611865856635,-320.950015977231)) ;
#24870 = CARTESIAN_POINT('Ctrl Pts',(-2.95039152971364,19.2039279540645,-320.94486039281)) ;
#24871 = CARTESIAN_POINT('Ctrl Pts',(-3.34780935058607,19.1342882363624,-320.939721137065)) ;
#24872 = CARTESIAN_POINT('Ctrl Pts',(-3.74518452231466,19.0646559920904,-320.934582432843)) ;
#24873 = CARTESIAN_POINT('Ctrl Pts',(-4.14041429297184,18.9826454288304,-320.929460157441)) ;
#24874 = CARTESIAN_POINT('Ctrl Pts',(-4.53272613103421,18.8884336168186,-320.92438884392)) ;
#24875 = CARTESIAN_POINT('Ctrl Pts',(-4.92501412730606,18.7942275302987,-320.919317838595)) ;
#24876 = CARTESIAN_POINT('Ctrl Pts',(-5.31438459612526,18.6878217196654,-320.914297835118)) ;
#24877 = CARTESIAN_POINT('Ctrl Pts',(-5.70007661014937,18.5694297192463,-320.909340366208)) ;
#24878 = CARTESIAN_POINT('Ctrl Pts',(-6.08637177921826,18.4508525743862,-320.904375144682)) ;
#24879 = CARTESIAN_POINT('Ctrl Pts',(-6.46897701035329,18.3202516908264,-320.899472651948)) ;
#24880 = CARTESIAN_POINT('Ctrl Pts',(-6.84713868439783,18.177878155596,-320.894621064394)) ;
#24881 = CARTESIAN_POINT('Ctrl Pts',(-7.22474863519534,18.0357123378434,-320.889776555118)) ;
#24882 = CARTESIAN_POINT('Ctrl Pts',(-7.59792799415087,17.8818081238135,-320.884982735315)) ;
#24883 = CARTESIAN_POINT('Ctrl Pts',(-7.9659369645801,17.7164526599707,-320.880205041174)) ;
#24884 = CARTESIAN_POINT('Ctrl Pts',(-8.33475247799237,17.5507347965677,-320.875416876051)) ;
#24885 = CARTESIAN_POINT('Ctrl Pts',(-8.69837487756646,17.3735152837348,-320.870644794961)) ;
#24886 = CARTESIAN_POINT('Ctrl Pts',(-9.05607028410433,17.1851222091369,-320.865832419686)) ;
#24887 = CARTESIAN_POINT('Ctrl Pts',(-9.41376569064274,16.9967291345388,-320.86102004441)) ;
#24888 = CARTESIAN_POINT('Ctrl Pts',(-9.76553401558552,16.7971623110319,-320.856167189171)) ;
#24889 = CARTESIAN_POINT('Ctrl Pts',(-10.110653081025,16.5867913533777,-320.851198154721)) ;
#24890 = CARTESIAN_POINT('Ctrl Pts',(-10.4553010580933,16.376707552597,-320.846235903015)) ;
#24891 = CARTESIAN_POINT('Ctrl Pts',(-10.7934075323238,16.1557939025365,-320.841156867352)) ;
#24892 = CARTESIAN_POINT('Ctrl Pts',(-11.1243178209923,15.9245208148808,-320.836037504658)) ;
#24893 = CARTESIAN_POINT('Ctrl Pts',(-11.4549774447451,15.693422916849,-320.830922019886)) ;
#24894 = CARTESIAN_POINT('Ctrl Pts',(-11.7784519136435,15.4519814121514,-320.825766435465)) ;
#24895 = CARTESIAN_POINT('Ctrl Pts',(-12.0941185762736,15.2006943796362,-320.820627179721)) ;
#24896 = CARTESIAN_POINT('Ctrl Pts',(-12.4097513629371,14.949434314147,-320.815488475499)) ;
#24897 = CARTESIAN_POINT('Ctrl Pts',(-12.7175781210385,14.6883309034558,-320.810366200098)) ;
#24898 = CARTESIAN_POINT('Ctrl Pts',(-13.0170051831817,14.41790923598,-320.805294886577)) ;
#24899 = CARTESIAN_POINT('Ctrl Pts',(-13.3164140483794,14.147504002718,-320.800223881253)) ;
#24900 = CARTESIAN_POINT('Ctrl Pts',(-13.6074243028103,13.8677816576701,-320.795203877776)) ;
#24901 = CARTESIAN_POINT('Ctrl Pts',(-13.8894699143559,13.5792937576966,-320.790246408867)) ;
#24902 = CARTESIAN_POINT('Ctrl Pts',(-14.1719565960832,13.2903547129251,-320.785281187341)) ;
#24903 = CARTESIAN_POINT('Ctrl Pts',(-14.4454505869314,12.9926226342601,-320.780378694607)) ;
#24904 = CARTESIAN_POINT('Ctrl Pts',(-14.7094102384387,12.6866785582528,-320.775527107052)) ;
#24905 = CARTESIAN_POINT('Ctrl Pts',(-14.9729847829978,12.3811808428493,-320.770682597777)) ;
#24906 = CARTESIAN_POINT('Ctrl Pts',(-15.2270527619927,12.0674950078586,-320.765888777975)) ;
#24907 = CARTESIAN_POINT('Ctrl Pts',(-15.4711019165878,11.7462271416504,-320.761111083835)) ;
#24908 = CARTESIAN_POINT('Ctrl Pts',(-15.7156859389862,11.424255172049,-320.756322918711)) ;
#24909 = CARTESIAN_POINT('Ctrl Pts',(-15.9502070688235,11.0946677862201,-320.751550837621)) ;
#24910 = CARTESIAN_POINT('Ctrl Pts',(-16.1741778308489,10.7581041931066,-320.746738462345)) ;
#24911 = CARTESIAN_POINT('Ctrl Pts',(-16.3981485928743,10.4215405999931,-320.741926087068)) ;
#24912 = CARTESIAN_POINT('Ctrl Pts',(-16.611568819787,10.0780006776278,-320.737073231829)) ;
#24913 = CARTESIAN_POINT('Ctrl Pts',(-16.8139811791531,9.72815450290812,-320.732104197378)) ;
#24914 = CARTESIAN_POINT('Ctrl Pts',(-17.0161172451294,9.37878586911457,-320.727141945672)) ;
#24915 = CARTESIAN_POINT('Ctrl Pts',(-17.2073277650371,9.02303684834942,-320.722062910009)) ;
#24916 = CARTESIAN_POINT('Ctrl Pts',(-17.3872628996133,8.66163373883787,-320.716943547313)) ;
#24917 = CARTESIAN_POINT('Ctrl Pts',(-17.5670617331351,8.30050439256336,-320.711828062541)) ;
#24918 = CARTESIAN_POINT('Ctrl Pts',(-17.7356024416079,7.93372958177536,-320.706672478119)) ;
#24919 = CARTESIAN_POINT('Ctrl Pts',(-17.8925765500298,7.56204457546894,-320.701533222374)) ;
#24920 = CARTESIAN_POINT('Ctrl Pts',(-18.0495338126759,7.19039945677411,-320.69639451815)) ;
#24921 = CARTESIAN_POINT('Ctrl Pts',(-18.1949270805422,6.81384520868004,-320.691272242749)) ;
#24922 = CARTESIAN_POINT('Ctrl Pts',(-18.3284862523631,6.43312695139845,-320.686200929227)) ;
#24923 = CARTESIAN_POINT('Ctrl Pts',(-18.462037307453,6.0524318313348,-320.681129923901)) ;
#24924 = CARTESIAN_POINT('Ctrl Pts',(-18.5837557672299,5.66757318835785,-320.676109920424)) ;
#24925 = CARTESIAN_POINT('Ctrl Pts',(-18.6934084609089,5.27930616398755,-320.671152451514)) ;
#24926 = CARTESIAN_POINT('Ctrl Pts',(-18.8032326322779,4.89043195770348,-320.666187229987)) ;
#24927 = CARTESIAN_POINT('Ctrl Pts',(-18.9009532611929,4.49813865880138,-320.661284737252)) ;
#24928 = CARTESIAN_POINT('Ctrl Pts',(-18.9863726926629,4.10319563002595,-320.656433149698)) ;
#24929 = CARTESIAN_POINT('Ctrl Pts',(-19.0716675004877,3.70882880784667,-320.651588640422)) ;
#24930 = CARTESIAN_POINT('Ctrl Pts',(-19.1446969235176,3.31181993588284,-320.646794820618)) ;
#24931 = CARTESIAN_POINT('Ctrl Pts',(-19.2053011000377,2.91294631488644,-320.642017126478)) ;
#24932 = CARTESIAN_POINT('Ctrl Pts',(-19.2660380990631,2.51319850671871,-320.637228961355)) ;
#24933 = CARTESIAN_POINT('Ctrl Pts',(-19.3142951818603,2.11157771646767,-320.632456880265)) ;
#24934 = CARTESIAN_POINT('Ctrl Pts',(-19.3499500955848,1.70887847193987,-320.627644504989)) ;
#24935 = CARTESIAN_POINT('Ctrl Pts',(-19.3856050093094,1.30617922741152,-320.622832129714)) ;
#24936 = CARTESIAN_POINT('Ctrl Pts',(-19.4086575486974,0.902401501544134,
-320.617979274475)) ;
#24937 = CARTESIAN_POINT('Ctrl Pts',(-19.4190266981606,0.498352507120491,
-320.613010240025)) ;
#24938 = CARTESIAN_POINT('Ctrl Pts',(-19.4293816937094,0.0948550405670599,
-320.60804798832)) ;
#24939 = CARTESIAN_POINT('Ctrl Pts',(-19.4270901203735,-0.30901817888565,
-320.602968952658)) ;
#24940 = CARTESIAN_POINT('Ctrl Pts',(-19.412192253063,-0.712461996250404,
-320.597849589965)) ;
#24941 = CARTESIAN_POINT('Ctrl Pts',(-19.3973056709019,-1.11560020451891,
-320.592734105193)) ;
#24942 = CARTESIAN_POINT('Ctrl Pts',(-19.3698320775587,-1.51830969525372,
-320.587578520773)) ;
#24943 = CARTESIAN_POINT('Ctrl Pts',(-19.329852362925,-1.91979722564955,-320.582439265029)) ;
#24944 = CARTESIAN_POINT('Ctrl Pts',(-19.2898769387396,-2.3212416701581,-320.577300560808)) ;
#24945 = CARTESIAN_POINT('Ctrl Pts',(-19.2373981910851,-2.72146446456308,
-320.572178285407)) ;
#24946 = CARTESIAN_POINT('Ctrl Pts',(-19.1725354199955,-3.11968207435652,
-320.567106971887)) ;
#24947 = CARTESIAN_POINT('Ctrl Pts',(-19.1076765907817,-3.5178754834518,-320.562035966563)) ;
#24948 = CARTESIAN_POINT('Ctrl Pts',(-19.0304352886145,-3.91406399891133,
-320.557015963087)) ;
#24949 = CARTESIAN_POINT('Ctrl Pts',(-18.9409680376835,-4.3074729546733,-320.552058494178)) ;
#24950 = CARTESIAN_POINT('Ctrl Pts',(-18.8513608755838,-4.70149713339378,
-320.547093272653)) ;
#24951 = CARTESIAN_POINT('Ctrl Pts',(-18.7494894677073,-5.09273308511964,
-320.542190779921)) ;
#24952 = CARTESIAN_POINT('Ctrl Pts',(-18.6355483294643,-5.48041064734489,
-320.537339192368)) ;
#24953 = CARTESIAN_POINT('Ctrl Pts',(-18.5217734269216,-5.86752260304727,
-320.532494683093)) ;
#24954 = CARTESIAN_POINT('Ctrl Pts',(-18.3959639164691,-6.25108655878862,
-320.527700863289)) ;
#24955 = CARTESIAN_POINT('Ctrl Pts',(-18.258351298614,-6.63034346269879,-320.522923169149)) ;
#24956 = CARTESIAN_POINT('Ctrl Pts',(-18.1204370835338,-7.01043156095392,
-320.518135004027)) ;
#24957 = CARTESIAN_POINT('Ctrl Pts',(-17.9706678151123,-7.38619368172872,
-320.513362922937)) ;
#24958 = CARTESIAN_POINT('Ctrl Pts',(-17.8093162611297,-7.75687363858416,
-320.508550547661)) ;
#24959 = CARTESIAN_POINT('Ctrl Pts',(-17.647964707147,-8.1275535954396,-320.503738172385)) ;
#24960 = CARTESIAN_POINT('Ctrl Pts',(-17.4750306744082,-8.49315131393668,
-320.498885317146)) ;
#24961 = CARTESIAN_POINT('Ctrl Pts',(-17.2908292111163,-8.85291919750511,
-320.493916282695)) ;
#24962 = CARTESIAN_POINT('Ctrl Pts',(-17.1068791832579,-9.21219599706071,
-320.488954030987)) ;
#24963 = CARTESIAN_POINT('Ctrl Pts',(-16.9116440705943,-9.5657523284759,-320.483874995323)) ;
#24964 = CARTESIAN_POINT('Ctrl Pts',(-16.7055444454999,-9.91290043052715,
-320.478755632626)) ;
#24965 = CARTESIAN_POINT('Ctrl Pts',(-16.4996009411783,-10.2597855673743,
-320.473640147854)) ;
#24966 = CARTESIAN_POINT('Ctrl Pts',(-16.2828095297037,-10.60027230135,-320.468484563432)) ;
#24967 = CARTESIAN_POINT('Ctrl Pts',(-16.0556207495516,-10.9337027628606,
-320.463345307687)) ;
#24968 = CARTESIAN_POINT('Ctrl Pts',(-15.8284563503074,-11.26709744207,-320.458206603465)) ;
#24969 = CARTESIAN_POINT('Ctrl Pts',(-15.5908968908092,-11.5934374597872,
-320.453084328063)) ;
#24970 = CARTESIAN_POINT('Ctrl Pts',(-15.3434219938976,-11.9120918479036,
-320.448013014542)) ;
#24971 = CARTESIAN_POINT('Ctrl Pts',(-15.0959621366668,-12.23072687058,-320.442942009217)) ;
#24972 = CARTESIAN_POINT('Ctrl Pts',(-14.8385880643354,-12.5416772609582,
-320.43792200574)) ;
#24973 = CARTESIAN_POINT('Ctrl Pts',(-14.5718078444623,-12.8443376475125,
-320.43296453683)) ;
#24974 = CARTESIAN_POINT('Ctrl Pts',(-14.3046104266468,-13.14747134236,-320.4279993153)) ;
#24975 = CARTESIAN_POINT('Ctrl Pts',(-14.0279773782128,-13.44228910014,-320.423096822563)) ;
#24976 = CARTESIAN_POINT('Ctrl Pts',(-13.7424479732906,-13.7282076799566,
-320.418245235006)) ;
#24977 = CARTESIAN_POINT('Ctrl Pts',(-13.4573351449372,-14.0137091154131,
-320.413400725732)) ;
#24978 = CARTESIAN_POINT('Ctrl Pts',(-13.1633518315393,-14.2903372997161,
-320.40860690593)) ;
#24979 = CARTESIAN_POINT('Ctrl Pts',(-12.8610644693045,-14.5575364431122,
-320.403829211792)) ;
#24980 = CARTESIAN_POINT('Ctrl Pts',(-12.5581146018111,-14.8253211910017,
-320.399041046665)) ;
#24981 = CARTESIAN_POINT('Ctrl Pts',(-12.2468241247313,-15.0836354265973,
-320.394268965572)) ;
#24982 = CARTESIAN_POINT('Ctrl Pts',(-11.9277943413587,-15.3319456196343,
-320.389456590294)) ;
#24983 = CARTESIAN_POINT('Ctrl Pts',(-11.6087645579866,-15.580255812671,-320.384644215016)) ;
#24984 = CARTESIAN_POINT('Ctrl Pts',(-11.2819953342844,-15.8185618053519,
-320.379791359776)) ;
#24985 = CARTESIAN_POINT('Ctrl Pts',(-10.9481209915988,-16.0463578384104,
-320.374822325325)) ;
#24986 = CARTESIAN_POINT('Ctrl Pts',(-10.6147023884452,-16.2738429291644,
-320.369860073621)) ;
#24987 = CARTESIAN_POINT('Ctrl Pts',(-10.2741108398708,-16.4909056522041,
-320.364781037961)) ;
#24988 = CARTESIAN_POINT('Ctrl Pts',(-9.92704470433196,-16.6971432767429,
-320.35966167527)) ;
#24989 = CARTESIAN_POINT('Ctrl Pts',(-9.58024147137529,-16.9032246762903,
-320.354546190495)) ;
#24990 = CARTESIAN_POINT('Ctrl Pts',(-9.22697353177151,-17.0984975505992,
-320.349390606071)) ;
#24991 = CARTESIAN_POINT('Ctrl Pts',(-8.86795125718945,-17.2825997540949,
-320.344251350324)) ;
#24992 = CARTESIAN_POINT('Ctrl Pts',(-8.50896751130765,-17.4666822005474,
-320.339112646099)) ;
#24993 = CARTESIAN_POINT('Ctrl Pts',(-8.14423068681169,-17.6395964952344,
-320.333990370695)) ;
#24994 = CARTESIAN_POINT('Ctrl Pts',(-7.77446382485693,-17.8010180302188,
-320.328919057171)) ;
#24995 = CARTESIAN_POINT('Ctrl Pts',(-7.40471943457631,-17.9624297552054,
-320.323848051844)) ;
#24996 = CARTESIAN_POINT('Ctrl Pts',(-7.02994560305102,-18.1123501810341,
-320.318828048364)) ;
#24997 = CARTESIAN_POINT('Ctrl Pts',(-6.65087810353198,-18.2504907855099,
-320.313870579451)) ;
#24998 = CARTESIAN_POINT('Ctrl Pts',(-6.27121780928545,-18.3888474175324,
-320.308905357931)) ;
#24999 = CARTESIAN_POINT('Ctrl Pts',(-5.8872503642293,-18.5153873501159,-320.304002865202)) ;
#25000 = CARTESIAN_POINT('Ctrl Pts',(-5.49972835716007,-18.6298564245958,
-320.299151277653)) ;
#25001 = CARTESIAN_POINT('Ctrl Pts',(-5.11277172896239,-18.7441584933445,
-320.294306768373)) ;
#25002 = CARTESIAN_POINT('Ctrl Pts',(-4.72227085317129,-18.8464248485324,
-320.289512948564)) ;
#25003 = CARTESIAN_POINT('Ctrl Pts',(-4.32898903709246,-18.936438432132,-320.284735254419)) ;
#25004 = CARTESIAN_POINT('Ctrl Pts',(-3.93484529019412,-19.0266492927953,
-320.279947089303)) ;
#25005 = CARTESIAN_POINT('Ctrl Pts',(-3.53790833891072,-19.1045534731966,
-320.275175008221)) ;
#25006 = CARTESIAN_POINT('Ctrl Pts',(-3.13896145884664,-19.1699701432719,
-320.270362632951)) ;
#25007 = CARTESIAN_POINT('Ctrl Pts',(-2.74001457878256,-19.2353868133472,
-320.265550257682)) ;
#25008 = CARTESIAN_POINT('Ctrl Pts',(-2.33905772772985,-19.2883157704039,
-320.260697402449)) ;
#25009 = CARTESIAN_POINT('Ctrl Pts',(-1.93688988906811,-19.328616367532,-320.255728368006)) ;
#25010 = CARTESIAN_POINT('Ctrl Pts',(-1.51041267919678,-19.3713529679437,
-320.250458976121)) ;
#25011 = CARTESIAN_POINT('Ctrl Pts',(-1.08250600421025,-19.3998956153957,
-320.245058602151)) ;
#25012 = CARTESIAN_POINT('Ctrl Pts',(-0.654080804362692,-19.4142304696164,
-320.239617595496)) ;
#25013 = CARTESIAN_POINT('Ctrl Pts',(-0.436310818107926,-19.4215169247729,
-320.236851913307)) ;
#25014 = CARTESIAN_POINT('Ctrl Pts',(-0.218406684945227,-19.425133126111,
-320.234075356998)) ;
#25015 = CARTESIAN_POINT('Ctrl Pts',(-0.000487082238699813,-19.4250810872335,
-320.231297307284)) ;
#25016 = CARTESIAN_POINT('Ctrl Pts',(-0.000424878507915977,-19.4249999953534,
-320.018354223318)) ;
#25017 = CARTESIAN_POINT('Ctrl Pts',(-0.220439294652272,-19.4249951830292,
-320.020935388206)) ;
#25018 = CARTESIAN_POINT('Ctrl Pts',(-0.440437550926895,-19.421252428869,
-320.023528335593)) ;
#25019 = CARTESIAN_POINT('Ctrl Pts',(-0.78548262287532,-19.4095163454399,
-320.027639313526)) ;
#25020 = CARTESIAN_POINT('Ctrl Pts',(-0.910596685962431,-19.4040490962108,
-320.029139135506)) ;
#25021 = CARTESIAN_POINT('Ctrl Pts',(-1.10739528474174,-19.3935417830338,
-320.031517929406)) ;
#25022 = CARTESIAN_POINT('Ctrl Pts',(-1.1791197437356,-19.3893131343616,-320.032389010415)) ;
#25023 = CARTESIAN_POINT('Ctrl Pts',(-1.31120037394053,-19.3807904809346,
-320.034001899657)) ;
#25024 = CARTESIAN_POINT('Ctrl Pts',(-1.37156315633409,-19.376612206174,-320.034742400884)) ;
#25025 = CARTESIAN_POINT('Ctrl Pts',(-1.4941388467024,-19.3675519431011,-320.036253803258)) ;
#25026 = CARTESIAN_POINT('Ctrl Pts',(-1.55634972259543,-19.3626520572994,
-320.037024904116)) ;
#25027 = CARTESIAN_POINT('Ctrl Pts',(-1.73302778372234,-19.3478794637681,
-320.03922516689)) ;
#25028 = CARTESIAN_POINT('Ctrl Pts',(-1.84743241083146,-19.3372908773168,
-320.040662246313)) ;
#25029 = CARTESIAN_POINT('Ctrl Pts',(-2.51899856859356,-19.269120696112,-320.049157452439)) ;
#25030 = CARTESIAN_POINT('Ctrl Pts',(-3.07355301092097,-19.1884766746646,
-320.05640503644)) ;
#25031 = CARTESIAN_POINT('Ctrl Pts',(-4.16681678102497,-18.9808775350747,
-320.070759059273)) ;
#25032 = CARTESIAN_POINT('Ctrl Pts',(-4.70514252555136,-18.8546469368251,
-320.077859132195)) ;
#25033 = CARTESIAN_POINT('Ctrl Pts',(-5.34313834958395,-18.6760157813397,
-320.086203723355)) ;
#25034 = CARTESIAN_POINT('Ctrl Pts',(-5.44867097281211,-18.6455001957067,
-320.087582024436)) ;
#25035 = CARTESIAN_POINT('Ctrl Pts',(-5.63606412821575,-18.5895871686054,
-320.090025512931)) ;
#25036 = CARTESIAN_POINT('Ctrl Pts',(-5.71802610910746,-18.5645400532082,
-320.091092896228)) ;
#25037 = CARTESIAN_POINT('Ctrl Pts',(-5.91077804529786,-18.5042385586038,
-320.093599832642)) ;
#25038 = CARTESIAN_POINT('Ctrl Pts',(-6.02142259752397,-18.4685303063039,
-320.095036323819)) ;
#25039 = CARTESIAN_POINT('Ctrl Pts',(-6.2515509311789,-18.391973228862,-320.098018954803)) ;
#25040 = CARTESIAN_POINT('Ctrl Pts',(-6.37097048712458,-18.3509482969429,
-320.09956381738)) ;
#25041 = CARTESIAN_POINT('Ctrl Pts',(-6.6355446054671,-18.2571636282723,-320.102980938717)) ;
#25042 = CARTESIAN_POINT('Ctrl Pts',(-6.78048715562218,-18.2038311895277,
-320.1048492048)) ;
#25043 = CARTESIAN_POINT('Ctrl Pts',(-7.73899609875098,-17.8381061373385,
-320.117188268857)) ;
#25044 = CARTESIAN_POINT('Ctrl Pts',(-8.5313808885285,-17.472997089213,-320.127261194052)) ;
#25045 = CARTESIAN_POINT('Ctrl Pts',(-9.49596775878819,-16.9472356014124,
-320.140149965992)) ;
#25046 = CARTESIAN_POINT('Ctrl Pts',(-9.69344674455519,-16.835061276245,-320.142826951084)) ;
#25047 = CARTESIAN_POINT('Ctrl Pts',(-9.9853888452008,-16.6623887308148,-320.146868864881)) ;
#25048 = CARTESIAN_POINT('Ctrl Pts',(-10.0813688111153,-16.6044931104927,
-320.148211648081)) ;
#25049 = CARTESIAN_POINT('Ctrl Pts',(-10.2547772128668,-16.4978344338597,
-320.150667449441)) ;
#25050 = CARTESIAN_POINT('Ctrl Pts',(-10.3323724986371,-16.4493487777329,
-320.15177733462)) ;
#25051 = CARTESIAN_POINT('Ctrl Pts',(-10.4496130117665,-16.3749337849397,
-320.153473094128)) ;
#25052 = CARTESIAN_POINT('Ctrl Pts',(-10.489510801058,-16.3494046286352,-320.15405351154)) ;
#25053 = CARTESIAN_POINT('Ctrl Pts',(-10.5820760261814,-16.2896971715659,
-320.155408340507)) ;
#25054 = CARTESIAN_POINT('Ctrl Pts',(-10.634671893511,-16.2554089666032,-320.156184354536)) ;
#25055 = CARTESIAN_POINT('Ctrl Pts',(-10.78487021505,-16.1564509623323,-320.158417125532)) ;
#25056 = CARTESIAN_POINT('Ctrl Pts',(-10.8820553881146,-16.0911529643991,
-320.159882160242)) ;
#25057 = CARTESIAN_POINT('Ctrl Pts',(-11.4454807756514,-15.7051526904405,
-320.168481132176)) ;
#25058 = CARTESIAN_POINT('Ctrl Pts',(-11.8981183463151,-15.3650782661189,
-320.175806095342)) ;
#25059 = CARTESIAN_POINT('Ctrl Pts',(-12.6441351764165,-14.7518250170382,
-320.188261826382)) ;
#25060 = CARTESIAN_POINT('Ctrl Pts',(-12.9450959374776,-14.4884432500845,
-320.193404852506)) ;
#25061 = CARTESIAN_POINT('Ctrl Pts',(-13.3819765467053,-14.0816258454257,
-320.200992949248)) ;
#25062 = CARTESIAN_POINT('Ctrl Pts',(-13.5241861620525,-13.9451020636554,
-320.203483890397)) ;
#25063 = CARTESIAN_POINT('Ctrl Pts',(-13.6755581650385,-13.7952885097983,
-320.206155988898)) ;
#25064 = CARTESIAN_POINT('Ctrl Pts',(-13.6868093607018,-13.7841258597643,
-320.206354727402)) ;
#25065 = CARTESIAN_POINT('Ctrl Pts',(-13.7077210526861,-13.7633278935611,
-320.206724341157)) ;
#25066 = CARTESIAN_POINT('Ctrl Pts',(-13.7173850829667,-13.753696145022,-320.20689524621)) ;
#25067 = CARTESIAN_POINT('Ctrl Pts',(-13.7354298052367,-13.7356737622817,
-320.207214535239)) ;
#25068 = CARTESIAN_POINT('Ctrl Pts',(-13.7438129768697,-13.727285620081,-320.207362940261)) ;
#25069 = CARTESIAN_POINT('Ctrl Pts',(-13.7595397355717,-13.7115206891985,
-320.207641479)) ;
#25070 = CARTESIAN_POINT('Ctrl Pts',(-13.7668850850061,-13.7041456647745,
-320.207771627753)) ;
#25071 = CARTESIAN_POINT('Ctrl Pts',(-13.7807298950954,-13.6902225576755,
-320.208017039606)) ;
#25072 = CARTESIAN_POINT('Ctrl Pts',(-13.7872306253495,-13.6836757416896,
-320.208132313584)) ;
#25073 = CARTESIAN_POINT('Ctrl Pts',(-13.7995408367887,-13.6712605812803,
-320.208350684669)) ;
#25074 = CARTESIAN_POINT('Ctrl Pts',(-13.8053512449818,-13.6653931590042,
-320.208453789746)) ;
#25075 = CARTESIAN_POINT('Ctrl Pts',(-13.8164050986895,-13.654216595234,-320.208650004132)) ;
#25076 = CARTESIAN_POINT('Ctrl Pts',(-13.8216492297861,-13.6489081339652,
-320.208743119351)) ;
#25077 = CARTESIAN_POINT('Ctrl Pts',(-13.8316712536273,-13.6387514701631,
-320.208921124481)) ;
#25078 = CARTESIAN_POINT('Ctrl Pts',(-13.8364496593592,-13.6339037754167,
-320.209006018826)) ;
#25079 = CARTESIAN_POINT('Ctrl Pts',(-13.8456226649469,-13.6245879679506,
-320.209169033249)) ;
#25080 = CARTESIAN_POINT('Ctrl Pts',(-13.8500176524653,-13.6201202381962,
-320.209247156683)) ;
#25081 = CARTESIAN_POINT('Ctrl Pts',(-13.8584920525939,-13.6114972334455,
-320.209397831947)) ;
#25082 = CARTESIAN_POINT('Ctrl Pts',(-13.8625717603932,-13.6073422495304,
-320.209470386336)) ;
#25083 = CARTESIAN_POINT('Ctrl Pts',(-13.870472820545,-13.5992881629975,-320.209610933356)) ;
#25084 = CARTESIAN_POINT('Ctrl Pts',(-13.874294398633,-13.595389282613,-320.209678927948)) ;
#25085 = CARTESIAN_POINT('Ctrl Pts',(-13.8817279186758,-13.5877990000008,
-320.209811216274)) ;
#25086 = CARTESIAN_POINT('Ctrl Pts',(-13.8853400331506,-13.5841077674006,
-320.209875511509)) ;
#25087 = CARTESIAN_POINT('Ctrl Pts',(-13.8923968514882,-13.5768906241003,
-320.210001148208)) ;
#25088 = CARTESIAN_POINT('Ctrl Pts',(-13.8958416861789,-13.5733648418761,
-320.21006249081)) ;
#25089 = CARTESIAN_POINT('Ctrl Pts',(-13.9026013145281,-13.5664411038134,
-320.210182884267)) ;
#25090 = CARTESIAN_POINT('Ctrl Pts',(-13.9059162054164,-13.5630432433836,
-320.210241935968)) ;
#25091 = CARTESIAN_POINT('Ctrl Pts',(-13.9124498383915,-13.5563411646504,
-320.210358348851)) ;
#25092 = CARTESIAN_POINT('Ctrl Pts',(-13.9156686496936,-13.5530370142669,
-320.210415710636)) ;
#25093 = CARTESIAN_POINT('Ctrl Pts',(-13.9220417488101,-13.5464902837687,
-320.210529305494)) ;
#25094 = CARTESIAN_POINT('Ctrl Pts',(-13.9251960814809,-13.5432477477215,
-320.210585538957)) ;
#25095 = CARTESIAN_POINT('Ctrl Pts',(-13.931470705277,-13.5367931594415,-320.210697419456)) ;
#25096 = CARTESIAN_POINT('Ctrl Pts',(-13.9345910189265,-13.5335811294995,
-320.210753066688)) ;
#25097 = CARTESIAN_POINT('Ctrl Pts',(-13.9408280595978,-13.5271563178918,
-320.210864317331)) ;
#25098 = CARTESIAN_POINT('Ctrl Pts',(-13.94394478741,-13.5239435373567,-320.210919920748)) ;
#25099 = CARTESIAN_POINT('Ctrl Pts',(-13.9502062814313,-13.517484608186,-320.211031648037)) ;
#25100 = CARTESIAN_POINT('Ctrl Pts',(-13.9533510257801,-13.5142384387133,
-320.211087771715)) ;
#25101 = CARTESIAN_POINT('Ctrl Pts',(-13.9597027356755,-13.5076772912768,
-320.211201150284)) ;
#25102 = CARTESIAN_POINT('Ctrl Pts',(-13.9629096531327,-13.5043622689905,
-320.211258404742)) ;
#25103 = CARTESIAN_POINT('Ctrl Pts',(-14.0477157293653,-13.4166348857031,
-320.212772766915)) ;
#25104 = CARTESIAN_POINT('Ctrl Pts',(-14.1285491719186,-13.3314855588383,
-320.214223113798)) ;
#25105 = CARTESIAN_POINT('Ctrl Pts',(-14.2950132691316,-13.1529190013186,
-320.217224662025)) ;
#25106 = CARTESIAN_POINT('Ctrl Pts',(-14.3805117772377,-13.0593860381604,
-320.218774661054)) ;
#25107 = CARTESIAN_POINT('Ctrl Pts',(-14.5695101725081,-12.8485203431736,
-320.22222086208)) ;
#25108 = CARTESIAN_POINT('Ctrl Pts',(-14.6725201117514,-12.7307602024706,
-320.224112820286)) ;
#25109 = CARTESIAN_POINT('Ctrl Pts',(-15.1257546229923,-12.1998171908184,
-320.232505599874)) ;
#25110 = CARTESIAN_POINT('Ctrl Pts',(-15.4600296210871,-11.7733375947971,
-320.238874299523)) ;
#25111 = CARTESIAN_POINT('Ctrl Pts',(-16.0847629805207,-10.9037150388822,
-320.251392503876)) ;
#25112 = CARTESIAN_POINT('Ctrl Pts',(-16.3757928387318,-10.4615490395309,
-320.257539348988)) ;
#25113 = CARTESIAN_POINT('Ctrl Pts',(-16.7364408429045,-9.86161087493845,
-320.265863726232)) ;
#25114 = CARTESIAN_POINT('Ctrl Pts',(-16.822538826032,-9.71401093370881,-320.267911140453)) ;
#25115 = CARTESIAN_POINT('Ctrl Pts',(-16.9458726195778,-9.49601819646844,
-320.270946504288)) ;
#25116 = CARTESIAN_POINT('Ctrl Pts',(-16.9846409317898,-9.42650162167603,
-320.271916164946)) ;
#25117 = CARTESIAN_POINT('Ctrl Pts',(-17.0549583465851,-9.29857128701474,
-320.273705393738)) ;
#25118 = CARTESIAN_POINT('Ctrl Pts',(-17.0866372854264,-9.24023043142591,
-320.274523300756)) ;
#25119 = CARTESIAN_POINT('Ctrl Pts',(-17.1642209598768,-9.0955867902831,-320.276555344582)) ;
#25120 = CARTESIAN_POINT('Ctrl Pts',(-17.2097744780778,-9.00909776812452,
-320.277773943801)) ;
#25121 = CARTESIAN_POINT('Ctrl Pts',(-17.3952865766884,-8.65033804646379,
-320.282837554016)) ;
#25122 = CARTESIAN_POINT('Ctrl Pts',(-17.529451757974,-8.3751217203075,-320.286742212298)) ;
#25123 = CARTESIAN_POINT('Ctrl Pts',(-17.6975743034572,-8.00849160484377,
-320.29192075144)) ;
#25124 = CARTESIAN_POINT('Ctrl Pts',(-17.7374285037688,-7.91982980088143,
-320.29317139258)) ;
#25125 = CARTESIAN_POINT('Ctrl Pts',(-17.9907817222782,-7.34470069695094,
-320.301266648444)) ;
#25126 = CARTESIAN_POINT('Ctrl Pts',(-18.1849138053504,-6.84994649390582,
-320.308143566171)) ;
#25127 = CARTESIAN_POINT('Ctrl Pts',(-18.4092407782897,-6.20117468916909,
-320.316902899096)) ;
#25128 = CARTESIAN_POINT('Ctrl Pts',(-18.4582001039537,-6.05388821777947,
-320.318875229424)) ;
#25129 = CARTESIAN_POINT('Ctrl Pts',(-18.5740815675654,-5.6907963777677,-320.323694232786)) ;
#25130 = CARTESIAN_POINT('Ctrl Pts',(-18.6390138265115,-5.47437972134774,
-320.32652927465)) ;
#25131 = CARTESIAN_POINT('Ctrl Pts',(-18.7366499761192,-5.12706126631921,
-320.331017010084)) ;
#25132 = CARTESIAN_POINT('Ctrl Pts',(-18.7717909360028,-4.99686648520311,
-320.332685539864)) ;
#25133 = CARTESIAN_POINT('Ctrl Pts',(-18.8372701690078,-4.74382610384772,
-320.335902121334)) ;
#25134 = CARTESIAN_POINT('Ctrl Pts',(-18.8677694392615,-4.62102910178874,
-320.337451177583)) ;
#25135 = CARTESIAN_POINT('Ctrl Pts',(-18.9382459441969,-4.32493835977142,
-320.341158712292)) ;
#25136 = CARTESIAN_POINT('Ctrl Pts',(-18.977047324828,-4.15137642439419,-320.343309341665)) ;
#25137 = CARTESIAN_POINT('Ctrl Pts',(-19.1644758795531,-3.25537664385854,
-320.354306568579)) ;
#25138 = CARTESIAN_POINT('Ctrl Pts',(-19.2742525205538,-2.52543123931449,
-320.362889314961)) ;
#25139 = CARTESIAN_POINT('Ctrl Pts',(-19.3797590953652,-1.38600334350933,
-320.376265983712)) ;
#25140 = CARTESIAN_POINT('Ctrl Pts',(-19.4045313966715,-0.9799120643945,-320.381035322936)) ;
#25141 = CARTESIAN_POINT('Ctrl Pts',(-19.4200624875907,-0.453945494692689,
-320.387345207962)) ;
#25142 = CARTESIAN_POINT('Ctrl Pts',(-19.422486762598,-0.334516708063532,
-320.38878697328)) ;
#25143 = CARTESIAN_POINT('Ctrl Pts',(-19.4245851967156,-0.145001878873325,
-320.391093834141)) ;
#25144 = CARTESIAN_POINT('Ctrl Pts',(-19.4249818940004,-0.0749267703727497,
-320.391950946931)) ;
#25145 = CARTESIAN_POINT('Ctrl Pts',(-19.4250150541863,0.0578554226074442,
-320.393584052569)) ;
#25146 = CARTESIAN_POINT('Ctrl Pts',(-19.4247270765315,0.120561588172162,
-320.39435905633)) ;
#25147 = CARTESIAN_POINT('Ctrl Pts',(-19.4230350858568,0.299894348324802,
-320.396585174918)) ;
#25148 = CARTESIAN_POINT('Ctrl Pts',(-19.4208843005822,0.416511092955219,
-320.398044493412)) ;
#25149 = CARTESIAN_POINT('Ctrl Pts',(-19.407867602269,0.890631409744478,-320.404015682221)) ;
#25150 = CARTESIAN_POINT('Ctrl Pts',(-19.3881791064578,1.2478218379844,-320.408601230701)) ;
#25151 = CARTESIAN_POINT('Ctrl Pts',(-19.3539944761441,1.66032754171005,-320.413931910504)) ;
#25152 = CARTESIAN_POINT('Ctrl Pts',(-19.3491049124066,1.71637082702257,-320.414656923074)) ;
#25153 = CARTESIAN_POINT('Ctrl Pts',(-19.2985323575846,2.26832211220699,-320.42180323578)) ;
#25154 = CARTESIAN_POINT('Ctrl Pts',(-19.234037892802,2.76232225453438,-320.428240690546)) ;
#25155 = CARTESIAN_POINT('Ctrl Pts',(-19.1255278930104,3.40106964613538,-320.436501444459)) ;
#25156 = CARTESIAN_POINT('Ctrl Pts',(-19.0987148116955,3.54854681973166,-320.438404787465)) ;
#25157 = CARTESIAN_POINT('Ctrl Pts',(-19.0282202711361,3.91230610441283,-320.443086677832)) ;
#25158 = CARTESIAN_POINT('Ctrl Pts',(-18.9825555397607,4.12818255053048,-320.445853828238)) ;
#25159 = CARTESIAN_POINT('Ctrl Pts',(-18.9032850203652,4.47374217000043,-320.450262368057)) ;
#25160 = CARTESIAN_POINT('Ctrl Pts',(-18.8719982506986,4.60393697273755,-320.451918592634)) ;
#25161 = CARTESIAN_POINT('Ctrl Pts',(-18.8087689258819,4.85557435039479,-320.455110716123)) ;
#25162 = CARTESIAN_POINT('Ctrl Pts',(-18.7769899514861,4.97705125441319,-320.456647614805)) ;
#25163 = CARTESIAN_POINT('Ctrl Pts',(-18.6968582450071,5.27166271158064,-320.460366005653)) ;
#25164 = CARTESIAN_POINT('Ctrl Pts',(-18.6472757201289,5.44445078285908,-320.462539193127)) ;
#25165 = CARTESIAN_POINT('Ctrl Pts',(-18.3852249421365,6.31205354173321,-320.473423790023)) ;
#25166 = CARTESIAN_POINT('Ctrl Pts',(-18.1362902433041,6.99524786991735,-320.481881513887)) ;
#25167 = CARTESIAN_POINT('Ctrl Pts',(-17.6870524790589,8.04168730111593,-320.495192208871)) ;
#25168 = CARTESIAN_POINT('Ctrl Pts',(-17.512416229709,8.41521457284197,-320.500024121433)) ;
#25169 = CARTESIAN_POINT('Ctrl Pts',(-17.271743548073,8.88998957720645,-320.506406327701)) ;
#25170 = CARTESIAN_POINT('Ctrl Pts',(-17.2164666140466,8.99657252163222,-320.507855314791)) ;
#25171 = CARTESIAN_POINT('Ctrl Pts',(-17.1273110968125,9.16464767802948,-320.510170913391)) ;
#25172 = CARTESIAN_POINT('Ctrl Pts',(-17.0940811056974,9.22648056486171,-320.511029439188)) ;
#25173 = CARTESIAN_POINT('Ctrl Pts',(-17.0305798548991,9.34312018154654,-320.512662730162)) ;
#25174 = CARTESIAN_POINT('Ctrl Pts',(-17.0003773554791,9.39796332623511,-320.513436483261)) ;
#25175 = CARTESIAN_POINT('Ctrl Pts',(-16.9134239713994,9.55406660408195,-320.515654344184)) ;
#25176 = CARTESIAN_POINT('Ctrl Pts',(-16.8560299035658,9.65496529993548,-320.51710656398)) ;
#25177 = CARTESIAN_POINT('Ctrl Pts',(-16.6219016059835,10.0581110375445,-320.522975151342)) ;
#25178 = CARTESIAN_POINT('Ctrl Pts',(-16.4379148097202,10.3560690711576,-320.527462080836)) ;
#25179 = CARTESIAN_POINT('Ctrl Pts',(-16.183145035555,10.7447465239927,-320.533445816465)) ;
#25180 = CARTESIAN_POINT('Ctrl Pts',(-16.1194665204469,10.8400442893461,-320.53492379121)) ;
#25181 = CARTESIAN_POINT('Ctrl Pts',(-15.7932932387923,11.3189472579906,-320.542398623993)) ;
#25182 = CARTESIAN_POINT('Ctrl Pts',(-15.5179327601823,11.693606908471,-320.548397870096)) ;
#25183 = CARTESIAN_POINT('Ctrl Pts',(-15.1399147823498,12.1710470397806,-320.556155319313)) ;
#25184 = CARTESIAN_POINT('Ctrl Pts',(-15.0491755006971,12.2830664929547,-320.557984274607)) ;
#25185 = CARTESIAN_POINT('Ctrl Pts',(-14.820130974883,12.5594781532492,-320.562516949373)) ;
#25186 = CARTESIAN_POINT('Ctrl Pts',(-14.6803295910188,12.7226057442818,-320.565209547733)) ;
#25187 = CARTESIAN_POINT('Ctrl Pts',(-14.4497402194546,12.982807156562,-320.569531050511)) ;
#25188 = CARTESIAN_POINT('Ctrl Pts',(-14.36061156515,13.0813267525219,-320.571173718456)) ;
#25189 = CARTESIAN_POINT('Ctrl Pts',(-14.1849078035738,13.2715833175637,-320.574358881148)) ;
#25190 = CARTESIAN_POINT('Ctrl Pts',(-14.0984358871806,13.3634067039217,-320.575902165546)) ;
#25191 = CARTESIAN_POINT('Ctrl Pts',(-13.8840386402038,13.5866749438975,-320.57967063276)) ;
#25192 = CARTESIAN_POINT('Ctrl Pts',(-13.7551340939057,13.717162650893,-320.581886926964)) ;
#25193 = CARTESIAN_POINT('Ctrl Pts',(-13.3626674665425,14.1033534505857,-320.588495604519)) ;
#25194 = CARTESIAN_POINT('Ctrl Pts',(-13.0936836223788,14.3534285210378,-320.592840551551)) ;
#25195 = CARTESIAN_POINT('Ctrl Pts',(-12.6501488333504,14.742934814927,-320.599772645628)) ;
#25196 = CARTESIAN_POINT('Ctrl Pts',(-12.4800008388558,14.8872419066598,-320.6023803057)) ;
#25197 = CARTESIAN_POINT('Ctrl Pts',(-12.0045330680007,15.2766181495714,-320.609558733597)) ;
#25198 = CARTESIAN_POINT('Ctrl Pts',(-11.6942327495527,15.5154373416621,-320.61412263542)) ;
#25199 = CARTESIAN_POINT('Ctrl Pts',(-11.1998693891695,15.8726579323129,-320.621336503789)) ;
#25200 = CARTESIAN_POINT('Ctrl Pts',(-11.0206641396424,15.9976031260581,-320.623940760451)) ;
#25201 = CARTESIAN_POINT('Ctrl Pts',(-10.767516506604,16.1678296302479,-320.627628782987)) ;
#25202 = CARTESIAN_POINT('Ctrl Pts',(-10.6953204971953,16.215679020884,-320.628681631217)) ;
#25203 = CARTESIAN_POINT('Ctrl Pts',(-10.5678376678042,16.2989491328382,-320.63054461717)) ;
#25204 = CARTESIAN_POINT('Ctrl Pts',(-10.5126869062606,16.3345752869121,-320.631351958675)) ;
#25205 = CARTESIAN_POINT('Ctrl Pts',(-10.3844049497662,16.4165237660093,-320.633233095546)) ;
#25206 = CARTESIAN_POINT('Ctrl Pts',(-10.3111427893368,16.4626380957567,-320.634309634482)) ;
#25207 = CARTESIAN_POINT('Ctrl Pts',(-10.0663560550385,16.6144422445951,-320.637910687091)) ;
#25208 = CARTESIAN_POINT('Ctrl Pts',(-9.89349586864448,16.7179530620042,-320.640460125705)) ;
#25209 = CARTESIAN_POINT('Ctrl Pts',(-9.46068789989389,16.9680598712658,-320.646831379844)) ;
#25210 = CARTESIAN_POINT('Ctrl Pts',(-9.19891270728211,17.111390243241,-320.650673969133)) ;
#25211 = CARTESIAN_POINT('Ctrl Pts',(-8.50643326368547,17.4700603984397,-320.660732148367)) ;
#25212 = CARTESIAN_POINT('Ctrl Pts',(-8.07084131796425,17.6755180700317,-320.666950914658)) ;
#25213 = CARTESIAN_POINT('Ctrl Pts',(-7.49279887847604,17.9223386716356,-320.674961274767)) ;
#25214 = CARTESIAN_POINT('Ctrl Pts',(-7.35687912924018,17.9785591200967,-320.676828208443)) ;
#25215 = CARTESIAN_POINT('Ctrl Pts',(-7.01813428340084,18.1141893332621,-320.681437243097)) ;
#25216 = CARTESIAN_POINT('Ctrl Pts',(-6.81458710223585,18.1917417221992,-320.684168079149)) ;
#25217 = CARTESIAN_POINT('Ctrl Pts',(-6.48435098185485,18.3112427076819,-320.688534230011)) ;
#25218 = CARTESIAN_POINT('Ctrl Pts',(-6.35845907498211,18.3553375181483,-320.690183854407)) ;
#25219 = CARTESIAN_POINT('Ctrl Pts',(-6.11294839453315,18.4385010000557,-320.693372456054)) ;
#25220 = CARTESIAN_POINT('Ctrl Pts',(-5.99338437971331,18.4777109223086,-320.694912332072)) ;
#25221 = CARTESIAN_POINT('Ctrl Pts',(-5.72816570492207,18.5618418644861,-320.698300422973)) ;
#25222 = CARTESIAN_POINT('Ctrl Pts',(-5.58234615835567,18.6062158214463,-320.7001448955)) ;
#25223 = CARTESIAN_POINT('Ctrl Pts',(-5.031149864548,18.7668858183006,-320.7070531202)) ;
#25224 = CARTESIAN_POINT('Ctrl Pts',(-4.62254402445215,18.8716867317456,-320.712042307311)) ;
#25225 = CARTESIAN_POINT('Ctrl Pts',(-3.68041795441686,19.0808904778501,-320.72336645772)) ;
#25226 = CARTESIAN_POINT('Ctrl Pts',(-3.14527728659802,19.1763679315871,-320.729666785354)) ;
#25227 = CARTESIAN_POINT('Ctrl Pts',(-2.47958132787475,19.2665200110759,-320.737585055342)) ;
#25228 = CARTESIAN_POINT('Ctrl Pts',(-2.35215451189201,19.2824916959373,-320.73910479281)) ;
#25229 = CARTESIAN_POINT('Ctrl Pts',(-2.06277002532154,19.3158519059493,-320.742572734726)) ;
#25230 = CARTESIAN_POINT('Ctrl Pts',(-1.9007332172356,19.3324692712325,-320.744526328699)) ;
#25231 = CARTESIAN_POINT('Ctrl Pts',(-1.6605742559612,19.3540497229004,-320.74745006302)) ;
#25232 = CARTESIAN_POINT('Ctrl Pts',(-1.58260008586275,19.3605817186337,-320.748403743372)) ;
#25233 = CARTESIAN_POINT('Ctrl Pts',(-1.43806326557867,19.3718107409448,-320.750181301689)) ;
#25234 = CARTESIAN_POINT('Ctrl Pts',(-1.37151190847322,19.3766362505788,-320.751003749072)) ;
#25235 = CARTESIAN_POINT('Ctrl Pts',(-1.20483191954692,19.3878588687708,-320.753072811733)) ;
#25236 = CARTESIAN_POINT('Ctrl Pts',(-1.10467614605483,19.3938232961496,-320.754324284472)) ;
#25237 = CARTESIAN_POINT('Ctrl Pts',(-0.658880831897908,19.4169065307049,
-320.759924364044)) ;
#25238 = CARTESIAN_POINT('Ctrl Pts',(-0.312866875711771,19.4255629692898,
-320.764349425013)) ;
#25239 = CARTESIAN_POINT('Ctrl Pts',(0.482373129114524,19.4242041047214,-320.774577596747)) ;
#25240 = CARTESIAN_POINT('Ctrl Pts',(0.931392678153338,19.407856583598,-320.780393716816)) ;
#25241 = CARTESIAN_POINT('Ctrl Pts',(1.66863256945528,19.3553699574858,-320.789881491135)) ;
#25242 = CARTESIAN_POINT('Ctrl Pts',(1.95732760782233,19.3283095464456,-320.793582032926)) ;
#25243 = CARTESIAN_POINT('Ctrl Pts',(2.46923212070005,19.268739925995,-320.800097748586)) ;
#25244 = CARTESIAN_POINT('Ctrl Pts',(2.69268498215345,19.2387861741158,-320.802926427065)) ;
#25245 = CARTESIAN_POINT('Ctrl Pts',(3.04880044857383,19.1847231241589,-320.807406743242)) ;
#25246 = CARTESIAN_POINT('Ctrl Pts',(3.18182084892681,19.1631104383089,-320.809074122292)) ;
#25247 = CARTESIAN_POINT('Ctrl Pts',(3.43931513789248,19.1185186468174,-320.812290028276)) ;
#25248 = CARTESIAN_POINT('Ctrl Pts',(3.56381063411769,19.0957036445271,-320.813839542661)) ;
#25249 = CARTESIAN_POINT('Ctrl Pts',(3.86294437716483,19.0378572536076,-320.817550782408)) ;
#25250 = CARTESIAN_POINT('Ctrl Pts',(4.03734118130923,19.0016374132105,-320.819704616067)) ;
#25251 = CARTESIAN_POINT('Ctrl Pts',(4.92975510516644,18.8034545099332,-320.830686450593)) ;
#25252 = CARTESIAN_POINT('Ctrl Pts',(5.63864549327814,18.6031734997548,-320.839252016077)) ;
#25253 = CARTESIAN_POINT('Ctrl Pts',(6.71965995391897,18.2302724701753,-320.852619371356)) ;
#25254 = CARTESIAN_POINT('Ctrl Pts',(7.10058737682417,18.0853067888293,-320.857397067941)) ;
#25255 = CARTESIAN_POINT('Ctrl Pts',(7.58699604262701,17.8824607981219,-320.863716616174)) ;
#25256 = CARTESIAN_POINT('Ctrl Pts',(7.6968929435045,17.8354352932725,-320.865159351578)) ;
#25257 = CARTESIAN_POINT('Ctrl Pts',(7.87053150959296,17.7592306034609,-320.867467385938)) ;
#25258 = CARTESIAN_POINT('Ctrl Pts',(7.93456141983906,17.7307155224725,-320.868324688334)) ;
#25259 = CARTESIAN_POINT('Ctrl Pts',(8.05556749265163,17.6760399360573,-320.869957816896)) ;
#25260 = CARTESIAN_POINT('Ctrl Pts',(8.11257407251907,17.649948933542,-320.870732650869)) ;
#25261 = CARTESIAN_POINT('Ctrl Pts',(8.27520288293987,17.5745619640171,-320.872957649764)) ;
#25262 = CARTESIAN_POINT('Ctrl Pts',(8.38050900071584,17.5245907173459,-320.874416005902)) ;
#25263 = CARTESIAN_POINT('Ctrl Pts',(8.80617290665142,17.3178848565147,-320.880373255798)) ;
#25264 = CARTESIAN_POINT('Ctrl Pts',(9.12263530593281,17.1532895233577,-320.884945401344)) ;
#25265 = CARTESIAN_POINT('Ctrl Pts',(9.90441567756516,16.7189205744363,-320.896462937509)) ;
#25266 = CARTESIAN_POINT('Ctrl Pts',(10.3634000346301,16.4383605213242,-320.903425238555)) ;
#25267 = CARTESIAN_POINT('Ctrl Pts',(10.9399206035668,16.0522010041459,-320.912280742381)) ;
#25268 = CARTESIAN_POINT('Ctrl Pts',(11.0686358361182,15.9637188866114,-320.914265845197)) ;
#25269 = CARTESIAN_POINT('Ctrl Pts',(11.3816877466164,15.7429124556655,-320.9191101012)) ;
#25270 = CARTESIAN_POINT('Ctrl Pts',(11.5647999683402,15.6088920334019,-320.92195758217)) ;
#25271 = CARTESIAN_POINT('Ctrl Pts',(11.8530671083957,15.3900505744603,-320.926459818943)) ;
#25272 = CARTESIAN_POINT('Ctrl Pts',(11.9597576369989,15.3072876070451,-320.928130596986)) ;
#25273 = CARTESIAN_POINT('Ctrl Pts',(12.1646731335807,15.1448783845089,-320.931348517156)) ;
#25274 = CARTESIAN_POINT('Ctrl Pts',(12.2630004098689,15.0653720407055,-320.93289669708)) ;
#25275 = CARTESIAN_POINT('Ctrl Pts',(12.4973284444706,14.872082802104,-320.936597098772)) ;
#25276 = CARTESIAN_POINT('Ctrl Pts',(12.6325612651791,14.7573866632655,-320.938741553452)) ;
#25277 = CARTESIAN_POINT('Ctrl Pts',(13.3243672541349,14.1541611685139,-320.949769471832)) ;
#25278 = CARTESIAN_POINT('Ctrl Pts',(13.8542418026504,13.6359460795332,-320.958386272018)) ;
#25279 = CARTESIAN_POINT('Ctrl Pts',(14.6263055216565,12.7892944932996,-320.971781120459)) ;
#25280 = CARTESIAN_POINT('Ctrl Pts',(14.8899398949859,12.4813683265295,-320.976533581835)) ;
#25281 = CARTESIAN_POINT('Ctrl Pts',(15.218453677588,12.0724281539511,-320.982823948413)) ;
#25282 = CARTESIAN_POINT('Ctrl Pts',(15.2923007197748,11.9787475348052,-320.984263749828)) ;
#25283 = CARTESIAN_POINT('Ctrl Pts',(15.4081331432415,11.8289882949567,-320.986568235784)) ;
#25284 = CARTESIAN_POINT('Ctrl Pts',(15.4506861856761,11.7733524294485,-320.987424965514)) ;
#25285 = CARTESIAN_POINT('Ctrl Pts',(15.5307792179003,11.6674529082228,-320.989058027819)) ;
#25286 = CARTESIAN_POINT('Ctrl Pts',(15.5683784395538,11.6172351802214,-320.989833377618)) ;
#25287 = CARTESIAN_POINT('Ctrl Pts',(15.6752763756413,11.4730107189607,-320.992061776468)) ;
#25288 = CARTESIAN_POINT('Ctrl Pts',(15.7439714073125,11.3785600440571,-320.993523054556)) ;
#25289 = CARTESIAN_POINT('Ctrl Pts',(16.1982568333234,10.7419598992156,-321.00336923584)) ;
#25290 = CARTESIAN_POINT('Ctrl Pts',(16.5566275747158,10.1809287656804,-321.012016483889)) ;
#25291 = CARTESIAN_POINT('Ctrl Pts',(17.0546710893243,9.30515560641771,-321.024988502965)) ;
#25292 = CARTESIAN_POINT('Ctrl Pts',(17.2159463323272,9.00327270330376,-321.029374058005)) ;
#25293 = CARTESIAN_POINT('Ctrl Pts',(17.4817758696224,8.47239031804388,-321.036902211097)) ;
#25294 = CARTESIAN_POINT('Ctrl Pts',(17.590010344414,8.24532726473637,-321.04006581322)) ;
#25295 = CARTESIAN_POINT('Ctrl Pts',(17.7513209149935,7.88927471557962,-321.044935165623)) ;
#25296 = CARTESIAN_POINT('Ctrl Pts',(17.8074687467393,7.76170771574798,-321.046661943751)) ;
#25297 = CARTESIAN_POINT('Ctrl Pts',(17.9113660019189,7.51859170549954,-321.049919341564)) ;
#25298 = CARTESIAN_POINT('Ctrl Pts',(17.9593822581987,7.40316433965779,-321.051451770685)) ;
#25299 = CARTESIAN_POINT('Ctrl Pts',(18.0676960301773,7.1355298002507,-321.054973261379)) ;
#25300 = CARTESIAN_POINT('Ctrl Pts',(18.1271903107961,6.98300772633619,-321.05695667622)) ;
#25301 = CARTESIAN_POINT('Ctrl Pts',(18.338879915505,6.41936755279624,-321.064206214334)) ;
#25302 = CARTESIAN_POINT('Ctrl Pts',(18.4790742807123,6.00388301523535,-321.06939175138)) ;
#25303 = CARTESIAN_POINT('Ctrl Pts',(18.6567789996028,5.4117974458981,-321.076643444932)) ;
#25304 = CARTESIAN_POINT('Ctrl Pts',(18.7060726261176,5.238874036943,-321.078745564338)) ;
#25305 = CARTESIAN_POINT('Ctrl Pts',(18.8577797882252,4.67721667632012,-321.08554193106)) ;
#25306 = CARTESIAN_POINT('Ctrl Pts',(18.9505295115635,4.28598236151558,-321.090226089239)) ;
#25307 = CARTESIAN_POINT('Ctrl Pts',(19.0620323075173,3.74077828601382,-321.096805966126)) ;
#25308 = CARTESIAN_POINT('Ctrl Pts',(19.0911836958801,3.58903926837595,-321.098643072822)) ;
#25309 = CARTESIAN_POINT('Ctrl Pts',(19.1396044020693,3.31969370155706,-321.10192490535)) ;
#25310 = CARTESIAN_POINT('Ctrl Pts',(19.1596076150798,3.20222718020609,-321.10336317344)) ;
#25311 = CARTESIAN_POINT('Ctrl Pts',(19.1896471867596,3.01545491216939,-321.105665805395)) ;
#25312 = CARTESIAN_POINT('Ctrl Pts',(19.2003917668734,2.94626602204398,-321.106522236242)) ;
#25313 = CARTESIAN_POINT('Ctrl Pts',(19.2200565493901,2.81495814737294,-321.10815526651)) ;
#25314 = CARTESIAN_POINT('Ctrl Pts',(19.2290502633462,2.75285108421927,-321.108930888095)) ;
#25315 = CARTESIAN_POINT('Ctrl Pts',(19.2539367053128,2.57492017768091,-321.111161076743)) ;
#25316 = CARTESIAN_POINT('Ctrl Pts',(19.2690849759452,2.45899505969869,-321.112623892772)) ;
#25317 = CARTESIAN_POINT('Ctrl Pts',(19.3582208492366,1.72537691252049,-321.121928203184)) ;
#25318 = CARTESIAN_POINT('Ctrl Pts',(19.403545405867,1.10456562239607,-321.130000011575)) ;
#25319 = CARTESIAN_POINT('Ctrl Pts',(19.4202525282254,0.432372943579887,-321.138665586218)) ;
#25320 = CARTESIAN_POINT('Ctrl Pts',(19.4213069343574,0.382088451540699,-321.139313465365)) ;
#25321 = CARTESIAN_POINT('Ctrl Pts',(19.4279410211256,-0.00624237521102015,
-321.144313284482)) ;
#25322 = CARTESIAN_POINT('Ctrl Pts',(19.4248895804184,-0.344378745654854,
-321.148644917905)) ;
#25323 = CARTESIAN_POINT('Ctrl Pts',(19.4042491011218,-0.931679827234011,
-321.156094792291)) ;
#25324 = CARTESIAN_POINT('Ctrl Pts',(19.3906775309003,-1.18090462179393,-321.159233390272)) ;
#25325 = CARTESIAN_POINT('Ctrl Pts',(19.3620736666084,-1.56845761567121,-321.164073822586)) ;
#25326 = CARTESIAN_POINT('Ctrl Pts',(19.3503513763003,-1.70700253145772,-321.165796269144)) ;
#25327 = CARTESIAN_POINT('Ctrl Pts',(19.3252584801268,-1.96993866947141,-321.169050264869)) ;
#25328 = CARTESIAN_POINT('Ctrl Pts',(19.3121716016006,-2.0943499619186,-321.170583566854)) ;
#25329 = CARTESIAN_POINT('Ctrl Pts',(19.2791097642132,-2.38192588923135,-321.174113888364)) ;
#25330 = CARTESIAN_POINT('Ctrl Pts',(19.2582636068129,-2.54498078475231,-321.176105162949)) ;
#25331 = CARTESIAN_POINT('Ctrl Pts',(19.1715556450661,-3.16093759698802,-321.18359390797)) ;
#25332 = CARTESIAN_POINT('Ctrl Pts',(19.0917650809629,-3.61172808235323,-321.189002233231)) ;
#25333 = CARTESIAN_POINT('Ctrl Pts',(18.8872496816849,-4.56879467090951,-321.200474374697)) ;
#25334 = CARTESIAN_POINT('Ctrl Pts',(18.7579163564014,-5.07372229097116,-321.206519474545)) ;
#25335 = CARTESIAN_POINT('Ctrl Pts',(18.5723616818639,-5.69331386978618,-321.214146099337)) ;
#25336 = CARTESIAN_POINT('Ctrl Pts',(18.5351124996305,-5.8134366637237,-321.215634965401)) ;
#25337 = CARTESIAN_POINT('Ctrl Pts',(18.4476431837861,-6.08612199518491,-321.219045306086)) ;
#25338 = CARTESIAN_POINT('Ctrl Pts',(18.3966921353373,-6.23844037526806,-321.220972195144)) ;
#25339 = CARTESIAN_POINT('Ctrl Pts',(18.3182471264915,-6.46362966199304,-321.223864064886)) ;
#25340 = CARTESIAN_POINT('Ctrl Pts',(18.2921943926042,-6.53699552376028,-321.224813090462)) ;
#25341 = CARTESIAN_POINT('Ctrl Pts',(18.2429555709759,-6.67305513481332,-321.226587461614)) ;
#25342 = CARTESIAN_POINT('Ctrl Pts',(18.2198856220572,-6.73578953642069,-321.227411444905)) ;
#25343 = CARTESIAN_POINT('Ctrl Pts',(18.1610926427764,-6.89315383377966,-321.22949230542)) ;
#25344 = CARTESIAN_POINT('Ctrl Pts',(18.124953443956,-6.98762608969736,-321.230754165314)) ;
#25345 = CARTESIAN_POINT('Ctrl Pts',(17.9542214534666,-7.42370286227686,-321.236630324036)) ;
#25346 = CARTESIAN_POINT('Ctrl Pts',(17.8106985502113,-7.76172973170638,-321.241330907462)) ;
#25347 = CARTESIAN_POINT('Ctrl Pts',(17.4277487012324,-8.59701101715748,-321.253157920627)) ;
#25348 = CARTESIAN_POINT('Ctrl Pts',(17.1765516085091,-9.08851472944457,-321.260305682385)) ;
#25349 = CARTESIAN_POINT('Ctrl Pts',(16.826810817791,-9.70639545373984,-321.269369310531)) ;
#25350 = CARTESIAN_POINT('Ctrl Pts',(16.7471663224401,-9.84317505923139,-321.271381466083)) ;
#25351 = CARTESIAN_POINT('Ctrl Pts',(16.6104204286298,-10.0715542089393,-321.274748298252)) ;
#25352 = CARTESIAN_POINT('Ctrl Pts',(16.554211111639,-10.1636787384439,-321.276108433978)) ;
#25353 = CARTESIAN_POINT('Ctrl Pts',(16.404548137358,-10.4044340847362,-321.27966750379)) ;
#25354 = CARTESIAN_POINT('Ctrl Pts',(16.3098420183649,-10.5522747158843,-321.281857556101)) ;
#25355 = CARTESIAN_POINT('Ctrl Pts',(16.1436423911797,-10.8041362103686,-321.285595750241)) ;
#25356 = CARTESIAN_POINT('Ctrl Pts',(16.0731153451493,-10.9087814194378,-321.287151133628)) ;
#25357 = CARTESIAN_POINT('Ctrl Pts',(15.9246811865839,-11.1244572482492,-321.290361871379)) ;
#25358 = CARTESIAN_POINT('Ctrl Pts',(15.8466207061054,-11.2353741468099,-321.292015909578)) ;
#25359 = CARTESIAN_POINT('Ctrl Pts',(15.6329138780215,-11.5323740712162,-321.296454331035)) ;
#25360 = CARTESIAN_POINT('Ctrl Pts',(15.4951097923419,-11.7168776052897,-321.299221569021)) ;
#25361 = CARTESIAN_POINT('Ctrl Pts',(14.869419234496,-12.5242546755011,-321.311401143046)) ;
#25362 = CARTESIAN_POINT('Ctrl Pts',(14.3470285630605,-13.1194264797603,-321.32053670096)) ;
#25363 = CARTESIAN_POINT('Ctrl Pts',(13.6459709550603,-13.8260553766132,-321.332237181178)) ;
#25364 = CARTESIAN_POINT('Ctrl Pts',(13.4998614933809,-13.9687533464353,-321.33465011243)) ;
#25365 = CARTESIAN_POINT('Ctrl Pts',(13.2460566205082,-14.2089301301279,-321.338821093324)) ;
#25366 = CARTESIAN_POINT('Ctrl Pts',(13.1394680563667,-14.3075536178086,-321.340566821618)) ;
#25367 = CARTESIAN_POINT('Ctrl Pts',(12.9761047335796,-14.4553439387318,-321.343241487496)) ;
#25368 = CARTESIAN_POINT('Ctrl Pts',(12.9201340552045,-14.5053920464456,-321.344157711655)) ;
#25369 = CARTESIAN_POINT('Ctrl Pts',(12.8135854618768,-14.5995601662011,-321.345903041322)) ;
#25370 = CARTESIAN_POINT('Ctrl Pts',(12.7630663755014,-14.6437449476966,-321.3467311779)) ;
#25371 = CARTESIAN_POINT('Ctrl Pts',(12.6313396693781,-14.7577557001439,-321.348891029275)) ;
#25372 = CARTESIAN_POINT('Ctrl Pts',(12.5497817585437,-14.8271734634048,-321.350228730606)) ;
#25373 = CARTESIAN_POINT('Ctrl Pts',(11.9865722969862,-15.2985712667869,-321.359456899253)) ;
#25374 = CARTESIAN_POINT('Ctrl Pts',(11.4862667574422,-15.6776871254774,-321.36759432973)) ;
#25375 = CARTESIAN_POINT('Ctrl Pts',(10.58061777079,-16.2973011699244,-321.38173947329)) ;
#25376 = CARTESIAN_POINT('Ctrl Pts',(10.1832354113472,-16.5485109988157,-321.387767673571)) ;
#25377 = CARTESIAN_POINT('Ctrl Pts',(9.59434973451866,-16.8915311307317,-321.396369168149)) ;
#25378 = CARTESIAN_POINT('Ctrl Pts',(9.40983873194986,-16.9950082679644,-321.399019596404)) ;
#25379 = CARTESIAN_POINT('Ctrl Pts',(9.1072776613571,-17.1582519711745,-321.403291850379)) ;
#25380 = CARTESIAN_POINT('Ctrl Pts',(8.99024255019759,-17.2198622541645,-321.404926846089)) ;
#25381 = CARTESIAN_POINT('Ctrl Pts',(8.76006304022102,-17.3380483411624,-321.408108574698)) ;
#25382 = CARTESIAN_POINT('Ctrl Pts',(8.64697706453917,-17.3947236955144,-321.409655973363)) ;
#25383 = CARTESIAN_POINT('Ctrl Pts',(8.39370823198772,-17.5185743819712,-321.413087543211)) ;
#25384 = CARTESIAN_POINT('Ctrl Pts',(8.25325625181947,-17.5851797712574,-321.414967597029)) ;
#25385 = CARTESIAN_POINT('Ctrl Pts',(7.61711711514107,-17.8775506690007,-321.423386416683)) ;
#25386 = CARTESIAN_POINT('Ctrl Pts',(7.11286595131701,-18.0840933047186,-321.429790962048)) ;
#25387 = CARTESIAN_POINT('Ctrl Pts',(6.10313375195545,-18.4489068358048,-321.442342410594)) ;
#25388 = CARTESIAN_POINT('Ctrl Pts',(5.59853202656793,-18.6082466071838,-321.448487168445)) ;
#25389 = CARTESIAN_POINT('Ctrl Pts',(4.92326852600235,-18.7915195884469,-321.456808079855)) ;
#25390 = CARTESIAN_POINT('Ctrl Pts',(4.75789531272295,-18.834070549204,-321.458854129379)) ;
#25391 = CARTESIAN_POINT('Ctrl Pts',(4.51466224231644,-18.8932469997572,-321.461887872693)) ;
#25392 = CARTESIAN_POINT('Ctrl Pts',(4.4372267699825,-18.9115831152886,-321.462857304731)) ;
#25393 = CARTESIAN_POINT('Ctrl Pts',(4.29498374693055,-18.9443434132671,-321.464646358844)) ;
#25394 = CARTESIAN_POINT('Ctrl Pts',(4.23021086537938,-18.9589121192833,-321.465464323057)) ;
#25395 = CARTESIAN_POINT('Ctrl Pts',(4.06985379793206,-18.994116906332,-321.467496859649)) ;
#25396 = CARTESIAN_POINT('Ctrl Pts',(3.9741861151502,-19.0143638250913,-321.468715899728)) ;
#25397 = CARTESIAN_POINT('Ctrl Pts',(3.5781198566014,-19.0950668025527,-321.473783559325)) ;
#25398 = CARTESIAN_POINT('Ctrl Pts',(3.27646481875271,-19.1491330235686,-321.477691933158)) ;
#25399 = CARTESIAN_POINT('Ctrl Pts',(2.55571883252368,-19.2607837616109,-321.487056220905)) ;
#25400 = CARTESIAN_POINT('Ctrl Pts',(2.13577667859977,-19.3118602947752,-321.492531580012)) ;
#25401 = CARTESIAN_POINT('Ctrl Pts',(1.38812085748488,-19.3781089649739,-321.502189177703)) ;
#25402 = CARTESIAN_POINT('Ctrl Pts',(1.06105900170137,-19.3987664805379,-321.506383987448)) ;
#25403 = CARTESIAN_POINT('Ctrl Pts',(0.48925235475261,-19.4203775300337,-321.51363416366)) ;
#25404 = CARTESIAN_POINT('Ctrl Pts',(0.244720710913186,-19.4249978991941,
-321.516708288758)) ;
#25405 = CARTESIAN_POINT('Ctrl Pts',(0.000166810840218079,-19.4249999992838,
-321.519753599958)) ;
#25406 = CARTESIAN_POINT('Origin',(0.,0.,-328.125)) ;
#25407 = CARTESIAN_POINT('',(-2.2413097626006E-5,-19.4249999999871,-323.232124485186)) ;
#25408 = CARTESIAN_POINT('',(0.00013264926062382,-19.425000134948,-323.017923319024)) ;
#25409 = CARTESIAN_POINT('',(-2.37887640734373E-15,-19.425,-328.125)) ;
#25410 = CARTESIAN_POINT('Ctrl Pts',(-2.2413097626006E-5,-19.4249999999871,
-323.232124485186)) ;
#25411 = CARTESIAN_POINT('Ctrl Pts',(0.0869997778376345,-19.4250001003957,
-323.231049337307)) ;
#25412 = CARTESIAN_POINT('Ctrl Pts',(0.174020913669814,-19.4244154237938,
-323.229967325262)) ;
#25413 = CARTESIAN_POINT('Ctrl Pts',(0.482637683223412,-19.4202678263039,
-323.226109168543)) ;
#25414 = CARTESIAN_POINT('Ctrl Pts',(0.704172780379017,-19.4134974171337,
-323.223301697483)) ;
#25415 = CARTESIAN_POINT('Ctrl Pts',(1.32702784953033,-19.3837864970045,-323.215343540241)) ;
#25416 = CARTESIAN_POINT('Ctrl Pts',(1.72782138467197,-19.3521785556824,-323.210148410201)) ;
#25417 = CARTESIAN_POINT('Ctrl Pts',(2.30672350311634,-19.2883959679957,-323.202636239244)) ;
#25418 = CARTESIAN_POINT('Ctrl Pts',(2.48581818589073,-19.2661335075859,-323.200310667552)) ;
#25419 = CARTESIAN_POINT('Ctrl Pts',(3.09821215149749,-19.181328219945,-323.192368330831)) ;
#25420 = CARTESIAN_POINT('Ctrl Pts',(3.52969452221682,-19.1066357356759,-323.18679188898)) ;
#25421 = CARTESIAN_POINT('Ctrl Pts',(4.11855605978414,-18.9840701809965,-323.179253949649)) ;
#25422 = CARTESIAN_POINT('Ctrl Pts',(4.27839924596018,-18.948686620764,-323.177214820923)) ;
#25423 = CARTESIAN_POINT('Ctrl Pts',(4.55948297852701,-18.8827267148357,-323.17364176892)) ;
#25424 = CARTESIAN_POINT('Ctrl Pts',(4.68091130540498,-18.852992404848,-323.17210241951)) ;
#25425 = CARTESIAN_POINT('Ctrl Pts',(4.93709217864169,-18.7876334562154,-323.168863237503)) ;
#25426 = CARTESIAN_POINT('Ctrl Pts',(5.07176550519992,-18.7517264482508,-323.167165384179)) ;
#25427 = CARTESIAN_POINT('Ctrl Pts',(5.44836162425121,-18.6469634004204,-323.16242946667)) ;
#25428 = CARTESIAN_POINT('Ctrl Pts',(5.68935053225407,-18.574853412416,-323.159413018638)) ;
#25429 = CARTESIAN_POINT('Ctrl Pts',(6.25475661969532,-18.3936335649466,-323.152350630556)) ;
#25430 = CARTESIAN_POINT('Ctrl Pts',(6.577825054827,-18.2805895444727,-323.148327468335)) ;
#25431 = CARTESIAN_POINT('Ctrl Pts',(7.51962474731159,-17.9228461192883,-323.136537018371)) ;
#25432 = CARTESIAN_POINT('Ctrl Pts',(8.12896320634184,-17.6548327693419,-323.128839886506)) ;
#25433 = CARTESIAN_POINT('Ctrl Pts',(8.82770544112915,-17.3036378776863,-323.119457046502)) ;
#25434 = CARTESIAN_POINT('Ctrl Pts',(8.93158973132352,-17.2502455625886,-323.118046626246)) ;
#25435 = CARTESIAN_POINT('Ctrl Pts',(9.0905223962333,-17.1667400313011,-323.115860700008)) ;
#25436 = CARTESIAN_POINT('Ctrl Pts',(9.14591704681406,-17.1372915625693,-323.115093507582)) ;
#25437 = CARTESIAN_POINT('Ctrl Pts',(9.2628527935397,-17.0743986373128,-323.113461784867)) ;
#25438 = CARTESIAN_POINT('Ctrl Pts',(9.32435759757997,-17.0408886525382,-323.112596294773)) ;
#25439 = CARTESIAN_POINT('Ctrl Pts',(9.49010526874783,-16.9494174772654,-323.11024568341)) ;
#25440 = CARTESIAN_POINT('Ctrl Pts',(9.5939977019496,-16.89082765475,-323.108752698418)) ;
#25441 = CARTESIAN_POINT('Ctrl Pts',(10.0483999403069,-16.6290238304381,-323.102147074575)) ;
#25442 = CARTESIAN_POINT('Ctrl Pts',(10.393041788145,-16.4158294452402,-323.096939538221)) ;
#25443 = CARTESIAN_POINT('Ctrl Pts',(11.3482469054453,-15.782796411105,-323.082165609928)) ;
#25444 = CARTESIAN_POINT('Ctrl Pts',(11.9418195589868,-15.3385893937751,-323.072594224182)) ;
#25445 = CARTESIAN_POINT('Ctrl Pts',(12.6441997119397,-14.7474155432783,-323.061064896001)) ;
#25446 = CARTESIAN_POINT('Ctrl Pts',(12.7782596458076,-14.6314090954591,-323.058852975362)) ;
#25447 = CARTESIAN_POINT('Ctrl Pts',(13.0051845529903,-14.4295456279523,-323.055089810607)) ;
#25448 = CARTESIAN_POINT('Ctrl Pts',(13.0988333805552,-14.3445870071012,-323.053531063806)) ;
#25449 = CARTESIAN_POINT('Ctrl Pts',(13.2907686917593,-14.1670154795538,-323.050323970256)) ;
#25450 = CARTESIAN_POINT('Ctrl Pts',(13.3889323875443,-14.0742797185615,-323.048676827952)) ;
#25451 = CARTESIAN_POINT('Ctrl Pts',(13.6494765392487,-13.8229494368484,-323.044284645697)) ;
#25452 = CARTESIAN_POINT('Ctrl Pts',(13.8100576455257,-13.6625198629165,-323.041556095821)) ;
#25453 = CARTESIAN_POINT('Ctrl Pts',(14.0763835575138,-13.3869514261829,-323.036984625653)) ;
#25454 = CARTESIAN_POINT('Ctrl Pts',(14.1836168091959,-13.2732835734265,-323.035130724143)) ;
#25455 = CARTESIAN_POINT('Ctrl Pts',(14.6540316274703,-12.762430383637,-323.026926743015)) ;
#25456 = CARTESIAN_POINT('Ctrl Pts',(15.0019856332515,-12.3515464247775,-323.020672813628)) ;
#25457 = CARTESIAN_POINT('Ctrl Pts',(15.5510335136416,-11.6457179741454,-323.01020523527)) ;
#25458 = CARTESIAN_POINT('Ctrl Pts',(15.7618710180762,-11.3587328275654,-323.00601743898)) ;
#25459 = CARTESIAN_POINT('Ctrl Pts',(16.0310779815112,-10.9703573067439,-323.000347403103)) ;
#25460 = CARTESIAN_POINT('Ctrl Pts',(16.0965916171744,-10.87400289397,-322.998940351682)) ;
#25461 = CARTESIAN_POINT('Ctrl Pts',(16.196012502994,-10.724911817012,-322.996758427174)) ;
#25462 = CARTESIAN_POINT('Ctrl Pts',(16.2305380165881,-10.672590602143,-322.995991819993)) ;
#25463 = CARTESIAN_POINT('Ctrl Pts',(16.3031357035559,-10.5614064136519,-322.9943599156)) ;
#25464 = CARTESIAN_POINT('Ctrl Pts',(16.3411437029352,-10.5025026378754,-322.993493646817)) ;
#25465 = CARTESIAN_POINT('Ctrl Pts',(16.4431219479328,-10.3425656996578,-322.991138362917)) ;
#25466 = CARTESIAN_POINT('Ctrl Pts',(16.5064794343286,-10.2411455056021,-322.989641432816)) ;
#25467 = CARTESIAN_POINT('Ctrl Pts',(16.7818098915375,-9.79121398340524,-322.982996830855)) ;
#25468 = CARTESIAN_POINT('Ctrl Pts',(16.9837109381512,-9.43666129196871,-322.97775306242)) ;
#25469 = CARTESIAN_POINT('Ctrl Pts',(17.5177863120818,-8.42604498324527,-322.963015347482)) ;
#25470 = CARTESIAN_POINT('Ctrl Pts',(17.824100386648,-7.75709514527957,-322.953517883187)) ;
#25471 = CARTESIAN_POINT('Ctrl Pts',(18.1566679898363,-6.90636035587834,-322.942044761967)) ;
#25472 = CARTESIAN_POINT('Ctrl Pts',(18.2192858205663,-6.7394384173965,-322.939820097018)) ;
#25473 = CARTESIAN_POINT('Ctrl Pts',(18.3224238904226,-6.452552427232,-322.936042346173)) ;
#25474 = CARTESIAN_POINT('Ctrl Pts',(18.3640851368324,-6.33301090976489,-322.934481604619)) ;
#25475 = CARTESIAN_POINT('Ctrl Pts',(18.4476612368103,-6.08543886559645,-322.931276415262)) ;
#25476 = CARTESIAN_POINT('Ctrl Pts',(18.4894187578426,-5.95736228129027,-322.929633108635)) ;
#25477 = CARTESIAN_POINT('Ctrl Pts',(18.5973986736284,-5.61409617397655,-322.925266613537)) ;
#25478 = CARTESIAN_POINT('Ctrl Pts',(18.6612178094072,-5.39817222670828,-322.922559555595)) ;
#25479 = CARTESIAN_POINT('Ctrl Pts',(18.7984514335964,-4.90230374157214,-322.916420747491)) ;
#25480 = CARTESIAN_POINT('Ctrl Pts',(18.8693924512028,-4.62172988671266,-322.913003583844)) ;
#25481 = CARTESIAN_POINT('Ctrl Pts',(19.0283262012247,-3.92830072628598,-322.904650841262)) ;
#25482 = CARTESIAN_POINT('Ctrl Pts',(19.1091814049624,-3.51396221886849,-322.899741097268)) ;
#25483 = CARTESIAN_POINT('Ctrl Pts',(19.2362322672417,-2.72735058505679,-322.89040993936)) ;
#25484 = CARTESIAN_POINT('Ctrl Pts',(19.2852691634251,-2.35573025466299,-322.885996787262)) ;
#25485 = CARTESIAN_POINT('Ctrl Pts',(19.3337443494514,-1.88334166999296,-322.880277645816)) ;
#25486 = CARTESIAN_POINT('Ctrl Pts',(19.3431934123166,-1.78368018165155,-322.879064817845)) ;
#25487 = CARTESIAN_POINT('Ctrl Pts',(19.3576533883666,-1.61750686075319,-322.877029230405)) ;
#25488 = CARTESIAN_POINT('Ctrl Pts',(19.3630928838455,-1.55103421284794,-322.876211348155)) ;
#25489 = CARTESIAN_POINT('Ctrl Pts',(19.3741783345324,-1.40640633281511,-322.874423193859)) ;
#25490 = CARTESIAN_POINT('Ctrl Pts',(19.3796939314511,-1.32824245298972,-322.873451505502)) ;
#25491 = CARTESIAN_POINT('Ctrl Pts',(19.395259761519,-1.08685999870199,-322.870436753541)) ;
#25492 = CARTESIAN_POINT('Ctrl Pts',(19.4037220083472,-0.923546399624622,
-322.868377309549)) ;
#25493 = CARTESIAN_POINT('Ctrl Pts',(19.4151763502325,-0.631062792373783,
-322.864664816512)) ;
#25494 = CARTESIAN_POINT('Ctrl Pts',(19.4189437520683,-0.501932728601272,
-322.863017335223)) ;
#25495 = CARTESIAN_POINT('Ctrl Pts',(19.4319767935828,0.177083646483194,-322.854324418943)) ;
#25496 = CARTESIAN_POINT('Ctrl Pts',(19.4191746899495,0.727142348784302,-322.847187379231)) ;
#25497 = CARTESIAN_POINT('Ctrl Pts',(19.3550134811969,1.70184655988742,-322.834645257377)) ;
#25498 = CARTESIAN_POINT('Ctrl Pts',(19.3129441715516,2.12673872818456,-322.829211689476)) ;
#25499 = CARTESIAN_POINT('Ctrl Pts',(19.2356352008606,2.71057807836531,-322.821833289147)) ;
#25500 = CARTESIAN_POINT('Ctrl Pts',(19.2123488441196,2.87098364563849,-322.819814949636)) ;
#25501 = CARTESIAN_POINT('Ctrl Pts',(19.167580379941,3.15437285205711,-322.816265108653)) ;
#25502 = CARTESIAN_POINT('Ctrl Pts',(19.1469150626167,3.27747606302304,-322.814728415509)) ;
#25503 = CARTESIAN_POINT('Ctrl Pts',(19.100516605888,3.53843974095426,-322.811481671427)) ;
#25504 = CARTESIAN_POINT('Ctrl Pts',(19.0744741479358,3.67623808495461,-322.809773743679)) ;
#25505 = CARTESIAN_POINT('Ctrl Pts',(18.9965782629021,4.06527284869614,-322.804968073117)) ;
#25506 = CARTESIAN_POINT('Ctrl Pts',(18.941237079387,4.31578118990166,-322.801893061239)) ;
#25507 = CARTESIAN_POINT('Ctrl Pts',(18.7980024091233,4.9081876643326,-322.794647366709)) ;
#25508 = CARTESIAN_POINT('Ctrl Pts',(18.7057190569609,5.24893091513465,-322.790501345458)) ;
#25509 = CARTESIAN_POINT('Ctrl Pts',(18.5401987527362,5.8001014298908,-322.783769405367)) ;
#25510 = CARTESIAN_POINT('Ctrl Pts',(18.4725363289533,6.01211676226762,-322.781173246079)) ;
#25511 = CARTESIAN_POINT('Ctrl Pts',(18.350723583399,6.37231830452902,-322.776729223834)) ;
#25512 = CARTESIAN_POINT('Ctrl Pts',(18.2983835519658,6.52109315654854,-322.774883799043)) ;
#25513 = CARTESIAN_POINT('Ctrl Pts',(18.1397591947078,6.95502442022907,-322.769456480611)) ;
#25514 = CARTESIAN_POINT('Ctrl Pts',(18.0285791309943,7.23833973377031,-322.765856298736)) ;
#25515 = CARTESIAN_POINT('Ctrl Pts',(17.873042257305,7.60884324873802,-322.761013632062)) ;
#25516 = CARTESIAN_POINT('Ctrl Pts',(17.8346182488141,7.69847562818859,-322.759831463014)) ;
#25517 = CARTESIAN_POINT('Ctrl Pts',(17.7689167814171,7.84860655399534,-322.757830693935)) ;
#25518 = CARTESIAN_POINT('Ctrl Pts',(17.7420013016323,7.90926154858949,-322.757016572187)) ;
#25519 = CARTESIAN_POINT('Ctrl Pts',(17.6820657839034,8.04248286297659,-322.755214997895)) ;
#25520 = CARTESIAN_POINT('Ctrl Pts',(17.6489088123999,8.11498605652443,-322.754225897238)) ;
#25521 = CARTESIAN_POINT('Ctrl Pts',(17.5429593346683,8.34294110824593,-322.751091263241)) ;
#25522 = CARTESIAN_POINT('Ctrl Pts',(17.4685522507388,8.497633238349,-322.74892751584)) ;
#25523 = CARTESIAN_POINT('Ctrl Pts',(17.1558907389562,9.12618965355925,-322.740014412872)) ;
#25524 = CARTESIAN_POINT('Ctrl Pts',(16.9003271319231,9.59118695496446,-322.733141999619)) ;
#25525 = CARTESIAN_POINT('Ctrl Pts',(16.3585805094029,10.4878502518783,-322.719640244599)) ;
#25526 = CARTESIAN_POINT('Ctrl Pts',(16.0735284448559,10.9196998698081,-322.713014586628)) ;
#25527 = CARTESIAN_POINT('Ctrl Pts',(15.664660186896,11.4883677227629,-322.704210293706)) ;
#25528 = CARTESIAN_POINT('Ctrl Pts',(15.5556409618938,11.6355578342765,-322.701923136603)) ;
#25529 = CARTESIAN_POINT('Ctrl Pts',(15.3680848490691,11.8814347246312,-322.698089202648)) ;
#25530 = CARTESIAN_POINT('Ctrl Pts',(15.2906389954855,11.9809382855656,-322.69653385234)) ;
#25531 = CARTESIAN_POINT('Ctrl Pts',(15.1295726469833,12.1837729746726,-322.69335506498)) ;
#25532 = CARTESIAN_POINT('Ctrl Pts',(15.0458492040519,12.2870140458884,-322.691732591438)) ;
#25533 = CARTESIAN_POINT('Ctrl Pts',(14.8238137630592,12.55513773662,-322.687505534836)) ;
#25534 = CARTESIAN_POINT('Ctrl Pts',(14.683809735164,12.7185954391102,-322.684915184268)) ;
#25535 = CARTESIAN_POINT('Ctrl Pts',(14.4452889975934,12.9878843306704,-322.680617572545)) ;
#25536 = CARTESIAN_POINT('Ctrl Pts',(14.3482549464116,13.0950026215281,-322.678899759297)) ;
#25537 = CARTESIAN_POINT('Ctrl Pts',(13.9327305659614,13.5435462271936,-322.671662845646)) ;
#25538 = CARTESIAN_POINT('Ctrl Pts',(13.6031803182369,13.8745130010345,-322.666217699342)) ;
#25539 = CARTESIAN_POINT('Ctrl Pts',(13.2003545699369,14.2509083301663,-322.659777343217)) ;
#25540 = CARTESIAN_POINT('Ctrl Pts',(13.1383082215875,14.3081307681494,-322.658790975433)) ;
#25541 = CARTESIAN_POINT('Ctrl Pts',(13.0014293858998,14.4327266141721,-322.656625541003)) ;
#25542 = CARTESIAN_POINT('Ctrl Pts',(12.9264419980141,14.4999262362785,-322.655446052979)) ;
#25543 = CARTESIAN_POINT('Ctrl Pts',(12.6171521406402,14.7727888438875,-322.650603143933)) ;
#25544 = CARTESIAN_POINT('Ctrl Pts',(12.3784377761401,14.9733795716315,-322.646917022754)) ;
#25545 = CARTESIAN_POINT('Ctrl Pts',(12.0581948446088,15.2295842633598,-322.641975519103)) ;
#25546 = CARTESIAN_POINT('Ctrl Pts',(11.9809240431651,15.290446650764,-322.640783389535)) ;
#25547 = CARTESIAN_POINT('Ctrl Pts',(11.8506719919057,15.3914461831979,-322.638771371947)) ;
#25548 = CARTESIAN_POINT('Ctrl Pts',(11.7979409598654,15.4319030383557,-322.637956091592)) ;
#25549 = CARTESIAN_POINT('Ctrl Pts',(11.6818711338585,15.520012699695,-322.636159177546)) ;
#25550 = CARTESIAN_POINT('Ctrl Pts',(11.6184463498184,15.5675499607975,-322.635175973614)) ;
#25551 = CARTESIAN_POINT('Ctrl Pts',(11.4189926511198,15.7151438608799,-322.632082387631)) ;
#25552 = CARTESIAN_POINT('Ctrl Pts',(11.281949002343,15.8138156776445,-322.629954429962)) ;
#25553 = CARTESIAN_POINT('Ctrl Pts',(10.7118192459671,16.2131270586636,-322.621120132497)) ;
#25554 = CARTESIAN_POINT('Ctrl Pts',(10.2678688598499,16.4978613562975,-322.614290258458)) ;
#25555 = CARTESIAN_POINT('Ctrl Pts',(9.33536068872856,17.0437035113906,-322.600362669254)) ;
#25556 = CARTESIAN_POINT('Ctrl Pts',(8.84610710733002,17.3026928852136,-322.593276145969)) ;
#25557 = CARTESIAN_POINT('Ctrl Pts',(8.20749016137047,17.6065731344844,-322.584404332839)) ;
#25558 = CARTESIAN_POINT('Ctrl Pts',(8.06773385525448,17.6710492845382,-322.582484584167)) ;
#25559 = CARTESIAN_POINT('Ctrl Pts',(7.8120588445231,17.7853387757181,-322.579012390081)) ;
#25560 = CARTESIAN_POINT('Ctrl Pts',(7.69639287358411,17.8356966654461,-322.57745621456)) ;
#25561 = CARTESIAN_POINT('Ctrl Pts',(7.45796239913722,17.9367516803025,-322.574277865685)) ;
#25562 = CARTESIAN_POINT('Ctrl Pts',(7.3351518966843,17.987323611267,-322.572656633783)) ;
#25563 = CARTESIAN_POINT('Ctrl Pts',(7.01255981392454,18.1163099983745,-322.568437900182)) ;
#25564 = CARTESIAN_POINT('Ctrl Pts',(6.81198033543965,18.1926800451154,-322.565854520478)) ;
#25565 = CARTESIAN_POINT('Ctrl Pts',(6.47481819673122,18.3146956206919,-322.561570585785)) ;
#25566 = CARTESIAN_POINT('Ctrl Pts',(6.33891956713202,18.3621743030175,-322.559859502709)) ;
#25567 = CARTESIAN_POINT('Ctrl Pts',(5.76310794750276,18.5561903862949,-322.552667030541)) ;
#25568 = CARTESIAN_POINT('Ctrl Pts',(5.31854983005023,18.6884628297979,-322.547258659107)) ;
#25569 = CARTESIAN_POINT('Ctrl Pts',(4.71461716494869,18.8448578886458,-322.539971153993)) ;
#25570 = CARTESIAN_POINT('Ctrl Pts',(4.55905775957654,18.8830949838841,-322.538098866466)) ;
#25571 = CARTESIAN_POINT('Ctrl Pts',(4.17441555221242,18.972611351941,-322.533467813402)) ;
#25572 = CARTESIAN_POINT('Ctrl Pts',(3.94484234042544,19.0216704146268,-322.53070254467)) ;
#25573 = CARTESIAN_POINT('Ctrl Pts',(3.55850844385497,19.0969337617057,-322.526014091636)) ;
#25574 = CARTESIAN_POINT('Ctrl Pts',(3.40221342063259,19.1253968625489,-322.524107755234)) ;
#25575 = CARTESIAN_POINT('Ctrl Pts',(3.16912874001578,19.1648966028949,-322.521240436452)) ;
#25576 = CARTESIAN_POINT('Ctrl Pts',(3.09259350308339,19.1773956567416,-322.520295025345)) ;
#25577 = CARTESIAN_POINT('Ctrl Pts',(2.949860083551,19.1998289335079,-322.518523056933)) ;
#25578 = CARTESIAN_POINT('Ctrl Pts',(2.88368155280495,19.2098799125099,-322.517697808486)) ;
#25579 = CARTESIAN_POINT('Ctrl Pts',(2.71672680244498,19.2343542694947,-322.515607439356)) ;
#25580 = CARTESIAN_POINT('Ctrl Pts',(2.61588671427294,19.2483278582912,-322.514337235252)) ;
#25581 = CARTESIAN_POINT('Ctrl Pts',(2.10089796422886,19.3155690424,-322.507819484516)) ;
#25582 = CARTESIAN_POINT('Ctrl Pts',(1.68521943037275,19.3562654979736,-322.502459398614)) ;
#25583 = CARTESIAN_POINT('Ctrl Pts',(0.489751691572928,19.434502805936,-322.487019752218)) ;
#25584 = CARTESIAN_POINT('Ctrl Pts',(-0.291419212319321,19.4384886585489,
-322.476926688712)) ;
#25585 = CARTESIAN_POINT('Ctrl Pts',(-1.22337185668507,19.3870411261111,-322.465220392933)) ;
#25586 = CARTESIAN_POINT('Ctrl Pts',(-1.37593116208305,19.3768112920489,-322.463313575677)) ;
#25587 = CARTESIAN_POINT('Ctrl Pts',(-1.65389300600906,19.3548733181328,-322.459857110122)) ;
#25588 = CARTESIAN_POINT('Ctrl Pts',(-1.77933287456766,19.3437446686656,-322.458303854341)) ;
#25589 = CARTESIAN_POINT('Ctrl Pts',(-2.03721168180052,19.3183367610048,-322.455123859811)) ;
#25590 = CARTESIAN_POINT('Ctrl Pts',(-2.169629875131,19.3039134091911,-322.453498141629)) ;
#25591 = CARTESIAN_POINT('Ctrl Pts',(-2.51711581112937,19.2624436450665,-322.449249348791)) ;
#25592 = CARTESIAN_POINT('Ctrl Pts',(-2.73189749187674,19.2331573980715,-322.446640796656)) ;
#25593 = CARTESIAN_POINT('Ctrl Pts',(-3.09050272956732,19.1781320235074,-322.442307412956)) ;
#25594 = CARTESIAN_POINT('Ctrl Pts',(-3.2346069067873,19.1543538979184,-322.440571967631)) ;
#25595 = CARTESIAN_POINT('Ctrl Pts',(-3.84667863159392,19.0462538334518,-322.433217279741)) ;
#25596 = CARTESIAN_POINT('Ctrl Pts',(-4.31173384204213,18.9463894494896,-322.427674506825)) ;
#25597 = CARTESIAN_POINT('Ctrl Pts',(-4.87226877282771,18.8043128681415,-322.420918391098)) ;
#25598 = CARTESIAN_POINT('Ctrl Pts',(-4.97168077436332,18.778274034338,-322.419717054076)) ;
#25599 = CARTESIAN_POINT('Ctrl Pts',(-5.40511072537198,18.6610632491404,-322.414459404615)) ;
#25600 = CARTESIAN_POINT('Ctrl Pts',(-5.73686314199073,18.5617591803445,-322.410384389416)) ;
#25601 = CARTESIAN_POINT('Ctrl Pts',(-6.17581623915929,18.4174736120994,-322.404839499393)) ;
#25602 = CARTESIAN_POINT('Ctrl Pts',(-6.28552371482691,18.3803218699986,-322.403440602502)) ;
#25603 = CARTESIAN_POINT('Ctrl Pts',(-6.45396983264457,18.321594166538,-322.401268358509)) ;
#25604 = CARTESIAN_POINT('Ctrl Pts',(-6.51294756114321,18.3007118292949,-322.40050316236)) ;
#25605 = CARTESIAN_POINT('Ctrl Pts',(-6.63793235574191,18.2557775603373,-322.398870769856)) ;
#25606 = CARTESIAN_POINT('Ctrl Pts',(-6.70391188855861,18.2316517534617,-322.398002573236)) ;
#25607 = CARTESIAN_POINT('Ctrl Pts',(-6.88255835819828,18.1652277215225,-322.395635746618)) ;
#25608 = CARTESIAN_POINT('Ctrl Pts',(-6.99496539828431,18.1222395619581,-322.394129074699)) ;
#25609 = CARTESIAN_POINT('Ctrl Pts',(-7.49299741770808,17.9264515681888,-322.387387202085)) ;
#25610 = CARTESIAN_POINT('Ctrl Pts',(-7.8740689591123,17.7623678941348,-322.382052883541)) ;
#25611 = CARTESIAN_POINT('Ctrl Pts',(-8.90420875761483,17.2791350405659,-322.367380541591)) ;
#25612 = CARTESIAN_POINT('Ctrl Pts',(-9.54117056944496,16.9357466142364,-322.358042458411)) ;
#25613 = CARTESIAN_POINT('Ctrl Pts',(-10.3108819180533,16.4635572473466,-322.346697155179)) ;
#25614 = CARTESIAN_POINT('Ctrl Pts',(-10.4629454964899,16.3673386609066,-322.344451163442)) ;
#25615 = CARTESIAN_POINT('Ctrl Pts',(-10.7188359308319,16.2003998151189,-322.340664497575)) ;
#25616 = CARTESIAN_POINT('Ctrl Pts',(-10.823353544009,16.1307599322396,-322.339115753194)) ;
#25617 = CARTESIAN_POINT('Ctrl Pts',(-11.0378449485883,15.9848214658981,-322.335932657128)) ;
#25618 = CARTESIAN_POINT('Ctrl Pts',(-11.1477203510333,15.9083899071589,-322.334299454614)) ;
#25619 = CARTESIAN_POINT('Ctrl Pts',(-11.4363541859676,15.7031515991841,-322.3300005706)) ;
#25620 = CARTESIAN_POINT('Ctrl Pts',(-11.6137261738016,15.5724285775482,-322.327350088126)) ;
#25621 = CARTESIAN_POINT('Ctrl Pts',(-11.9077179901487,15.3479396202782,-322.322933961974)) ;
#25622 = CARTESIAN_POINT('Ctrl Pts',(-12.0255473918856,15.2557926147761,-322.321157568217)) ;
#25623 = CARTESIAN_POINT('Ctrl Pts',(-12.5295593962879,14.8521686361351,-322.313521385374)) ;
#25624 = CARTESIAN_POINT('Ctrl Pts',(-12.9047947148662,14.5273206550763,-322.307744282539)) ;
#25625 = CARTESIAN_POINT('Ctrl Pts',(-13.341653473265,14.1188279630559,-322.300753330409)) ;
#25626 = CARTESIAN_POINT('Ctrl Pts',(-13.4155765591881,14.0486058392722,-322.299560518826)) ;
#25627 = CARTESIAN_POINT('Ctrl Pts',(-13.7385750969175,13.7369038965997,-322.294298777419)) ;
#25628 = CARTESIAN_POINT('Ctrl Pts',(-13.9817081523641,13.4893591561411,-322.290206945558)) ;
#25629 = CARTESIAN_POINT('Ctrl Pts',(-14.2864287851527,13.1620150377113,-322.28482103629)) ;
#25630 = CARTESIAN_POINT('Ctrl Pts',(-14.3542069338745,13.0880644308583,-322.283605792094)) ;
#25631 = CARTESIAN_POINT('Ctrl Pts',(-14.4661094303812,12.9640562662635,-322.281567437303)) ;
#25632 = CARTESIAN_POINT('Ctrl Pts',(-14.5105541479562,12.9142903504261,-322.280749235464)) ;
#25633 = CARTESIAN_POINT('Ctrl Pts',(-14.606567617893,12.8056601376005,-322.278962027649)) ;
#25634 = CARTESIAN_POINT('Ctrl Pts',(-14.6580387321836,12.7467113264984,-322.277991622682)) ;
#25635 = CARTESIAN_POINT('Ctrl Pts',(-14.8155764736944,12.5640705249583,-322.27498555188)) ;
#25636 = CARTESIAN_POINT('Ctrl Pts',(-14.9204440074153,12.4393538772248,-322.272933634802)) ;
#25637 = CARTESIAN_POINT('Ctrl Pts',(-15.1051789891208,12.2139552390321,-322.269237627923)) ;
#25638 = CARTESIAN_POINT('Ctrl Pts',(-15.1856400342428,12.1137719797313,-322.267599110672)) ;
#25639 = CARTESIAN_POINT('Ctrl Pts',(-15.6014937969851,11.5853314127671,-322.258992659673)) ;
#25640 = CARTESIAN_POINT('Ctrl Pts',(-15.9197826657461,11.1439236060407,-322.251934361317)) ;
#25641 = CARTESIAN_POINT('Ctrl Pts',(-16.449567940532,10.34010110995,-322.239570016606)) ;
#25642 = CARTESIAN_POINT('Ctrl Pts',(-16.668643711703,9.98310045591224,-322.234236073943)) ;
#25643 = CARTESIAN_POINT('Ctrl Pts',(-16.9518879398559,9.48617933383256,-322.227061899713)) ;
#25644 = CARTESIAN_POINT('Ctrl Pts',(-17.0261878783808,9.35216710152718,-322.225150869763)) ;
#25645 = CARTESIAN_POINT('Ctrl Pts',(-17.1586827863538,9.10637722992468,-322.221689284653)) ;
#25646 = CARTESIAN_POINT('Ctrl Pts',(-17.2173904885116,8.99488554854081,-322.220135082108)) ;
#25647 = CARTESIAN_POINT('Ctrl Pts',(-17.3358608066736,8.76448873391843,-322.216955650361)) ;
#25648 = CARTESIAN_POINT('Ctrl Pts',(-17.395494676012,8.64552472141425,-322.215331415742)) ;
#25649 = CARTESIAN_POINT('Ctrl Pts',(-17.5487275487607,8.3318342604138,-322.211092559301)) ;
#25650 = CARTESIAN_POINT('Ctrl Pts',(-17.6403085221292,8.13614258631874,-322.208492327156)) ;
#25651 = CARTESIAN_POINT('Ctrl Pts',(-17.9560938653736,7.43095811739825,-322.199262648058)) ;
#25652 = CARTESIAN_POINT('Ctrl Pts',(-18.1616415910947,6.91340879581943,-322.192754902568)) ;
#25653 = CARTESIAN_POINT('Ctrl Pts',(-18.3948655766226,6.24362363387668,-322.184471623747)) ;
#25654 = CARTESIAN_POINT('Ctrl Pts',(-18.4433507829266,6.09891199690866,-322.182689407968)) ;
#25655 = CARTESIAN_POINT('Ctrl Pts',(-18.6006950984343,5.61025058015102,-322.176681020637)) ;
#25656 = CARTESIAN_POINT('Ctrl Pts',(-18.7016767652763,5.26384410957424,-322.172439057617)) ;
#25657 = CARTESIAN_POINT('Ctrl Pts',(-18.8225206854836,4.80177012775681,-322.166708719203)) ;
#25658 = CARTESIAN_POINT('Ctrl Pts',(-18.851067287678,4.68844786379004,-322.165297582483)) ;
#25659 = CARTESIAN_POINT('Ctrl Pts',(-18.8933671775832,4.5138939691891,-322.163110804998)) ;
#25660 = CARTESIAN_POINT('Ctrl Pts',(-18.9078492453798,4.45284167415197,-322.162343487938)) ;
#25661 = CARTESIAN_POINT('Ctrl Pts',(-18.9378675667605,4.32350562990393,-322.160711802385)) ;
#25662 = CARTESIAN_POINT('Ctrl Pts',(-18.9533308846873,4.2552059008357,-322.159846476585)) ;
#25663 = CARTESIAN_POINT('Ctrl Pts',(-18.9941181061296,4.07041922116845,-322.157496851858)) ;
#25664 = CARTESIAN_POINT('Ctrl Pts',(-19.0187395997611,3.95378037315729,-322.156004700023)) ;
#25665 = CARTESIAN_POINT('Ctrl Pts',(-19.0584857145935,3.75652413665362,-322.153470173061)) ;
#25666 = CARTESIAN_POINT('Ctrl Pts',(-19.0741762133927,3.67602408678508,-322.152432740773)) ;
#25667 = CARTESIAN_POINT('Ctrl Pts',(-19.1869287925475,3.07738195450072,-322.14470050552)) ;
#25668 = CARTESIAN_POINT('Ctrl Pts',(-19.2633726920502,2.55557985530033,-322.137871018886)) ;
#25669 = CARTESIAN_POINT('Ctrl Pts',(-19.3762796102483,1.48179737095789,-322.12395418446)) ;
#25670 = CARTESIAN_POINT('Ctrl Pts',(-19.4105879310623,0.930061611787838,
-322.116877906103)) ;
#25671 = CARTESIAN_POINT('Ctrl Pts',(-19.4243187996811,0.223860244337423,
-322.108017542089)) ;
#25672 = CARTESIAN_POINT('Ctrl Pts',(-19.4254823281291,0.0700760075874453,
-322.106099376195)) ;
#25673 = CARTESIAN_POINT('Ctrl Pts',(-19.4242761611515,-0.209827369957383,
-322.102629109354)) ;
#25674 = CARTESIAN_POINT('Ctrl Pts',(-19.4225043666603,-0.335940598764716,
-322.10107329333)) ;
#25675 = CARTESIAN_POINT('Ctrl Pts',(-19.4163444496347,-0.594848308822051,
-322.097894755938)) ;
#25676 = CARTESIAN_POINT('Ctrl Pts',(-19.4118218219957,-0.727633083781163,
-322.096272985603)) ;
#25677 = CARTESIAN_POINT('Ctrl Pts',(-19.3964204866916,-1.07501902176696,
-322.092050642375)) ;
#25678 = CARTESIAN_POINT('Ctrl Pts',(-19.383342643812,-1.28950446306553,-322.08946423936)) ;
#25679 = CARTESIAN_POINT('Ctrl Pts',(-19.3555463204165,-1.64749671126433,
-322.0851743744)) ;
#25680 = CARTESIAN_POINT('Ctrl Pts',(-19.3427829286629,-1.79113578601075,
-322.083460373931)) ;
#25681 = CARTESIAN_POINT('Ctrl Pts',(-19.2821030922746,-2.39737667679644,
-322.076248671407)) ;
#25682 = CARTESIAN_POINT('Ctrl Pts',(-19.219180869292,-2.85832147729128,-322.070824391367)) ;
#25683 = CARTESIAN_POINT('Ctrl Pts',(-19.1215975061618,-3.42147194416013,
-322.064147839149)) ;
#25684 = CARTESIAN_POINT('Ctrl Pts',(-19.1025564455917,-3.52623009582374,
-322.062903520324)) ;
#25685 = CARTESIAN_POINT('Ctrl Pts',(-19.01593727303,-3.98147736549663,-322.057479100484)) ;
#25686 = CARTESIAN_POINT('Ctrl Pts',(-18.9395672420655,-4.33022216782846,
-322.053280957858)) ;
#25687 = CARTESIAN_POINT('Ctrl Pts',(-18.8255646696006,-4.78981534358015,
-322.047599401192)) ;
#25688 = CARTESIAN_POINT('Ctrl Pts',(-18.7964791567579,-4.90271224993069,
-322.046191565082)) ;
#25689 = CARTESIAN_POINT('Ctrl Pts',(-18.7501913649732,-5.07591171248897,
-322.044008708593)) ;
#25690 = CARTESIAN_POINT('Ctrl Pts',(-18.7337104324694,-5.13640432185019,
-322.043241965212)) ;
#25691 = CARTESIAN_POINT('Ctrl Pts',(-18.6981863458054,-5.26434844868946,
-322.041610104164)) ;
#25692 = CARTESIAN_POINT('Ctrl Pts',(-18.6790704253005,-5.33177880579128,
-322.040744017672)) ;
#25693 = CARTESIAN_POINT('Ctrl Pts',(-18.6263729945161,-5.513903919051,-322.038389827069)) ;
#25694 = CARTESIAN_POINT('Ctrl Pts',(-18.5920972888899,-5.62839459316946,
-322.036893819974)) ;
#25695 = CARTESIAN_POINT('Ctrl Pts',(-18.4363693228443,-6.13162083053171,
-322.030258358534)) ;
#25696 = CARTESIAN_POINT('Ctrl Pts',(-18.3037658065016,-6.51679708026814,
-322.025023089399)) ;
#25697 = CARTESIAN_POINT('Ctrl Pts',(-17.8976377207438,-7.58601374652019,
-322.01027662991)) ;
#25698 = CARTESIAN_POINT('Ctrl Pts',(-17.597176331973,-8.25908191593055,-322.000761582616)) ;
#25699 = CARTESIAN_POINT('Ctrl Pts',(-17.1775331646046,-9.07164117981292,
-321.989275165638)) ;
#25700 = CARTESIAN_POINT('Ctrl Pts',(-17.0936710434952,-9.22869057382707,
-321.987053607131)) ;
#25701 = CARTESIAN_POINT('Ctrl Pts',(-16.9465216151526,-9.49536971034638,
-321.983279413837)) ;
#25702 = CARTESIAN_POINT('Ctrl Pts',(-16.8842999371922,-9.60557423944086,
-321.981719160736)) ;
#25703 = CARTESIAN_POINT('Ctrl Pts',(-16.7535935894244,-9.83188153246851,
-321.978513521547)) ;
#25704 = CARTESIAN_POINT('Ctrl Pts',(-16.684968377873,-9.94789540133737,-321.976869291936)) ;
#25705 = CARTESIAN_POINT('Ctrl Pts',(-16.4982782810744,-10.2561359936287,
-321.972496617361)) ;
#25706 = CARTESIAN_POINT('Ctrl Pts',(-16.3780630092293,-10.4470361380337,
-321.969784389133)) ;
#25707 = CARTESIAN_POINT('Ctrl Pts',(-16.0956551439354,-10.878636305276,-321.963630698536)) ;
#25708 = CARTESIAN_POINT('Ctrl Pts',(-15.9313382249562,-11.1178822212779,
-321.96020393827)) ;
#25709 = CARTESIAN_POINT('Ctrl Pts',(-15.5150628733721,-11.6957920631672,
-321.951842159534)) ;
#25710 = CARTESIAN_POINT('Ctrl Pts',(-15.2573090139932,-12.030097648066,-321.946932734982)) ;
#25711 = CARTESIAN_POINT('Ctrl Pts',(-14.751487024472,-12.6437152653019,-321.937619599178)) ;
#25712 = CARTESIAN_POINT('Ctrl Pts',(-14.5058532489479,-12.9247872463635,
-321.933224410298)) ;
#25713 = CARTESIAN_POINT('Ctrl Pts',(-14.1842744019425,-13.2720383144944,
-321.927524343496)) ;
#25714 = CARTESIAN_POINT('Ctrl Pts',(-14.1157060249559,-13.3449422894551,
-321.926311816486)) ;
#25715 = CARTESIAN_POINT('Ctrl Pts',(-14.0005123595303,-13.465538472383,-321.924276573522)) ;
#25716 = CARTESIAN_POINT('Ctrl Pts',(-13.9541993190358,-13.5135263367605,
-321.923458730857)) ;
#25717 = CARTESIAN_POINT('Ctrl Pts',(-13.8711575136069,-13.5986890923662,
-321.921992373221)) ;
#25718 = CARTESIAN_POINT('Ctrl Pts',(-13.8345242301836,-13.6359559663533,
-321.921345616515)) ;
#25719 = CARTESIAN_POINT('Ctrl Pts',(-13.7971649502257,-13.6736558756643,
-321.920686384005)) ;
#25720 = CARTESIAN_POINT('Ctrl Pts',(-13.7965888289167,-13.6742371763707,
-321.920676217995)) ;
#25721 = CARTESIAN_POINT('Ctrl Pts',(-13.795426520587,-13.6754097857558,-321.920655708525)) ;
#25722 = CARTESIAN_POINT('Ctrl Pts',(-13.7948403323311,-13.6760010931102,
-321.920645365048)) ;
#25723 = CARTESIAN_POINT('Ctrl Pts',(-13.7936573054439,-13.6771942977524,
-321.920624490337)) ;
#25724 = CARTESIAN_POINT('Ctrl Pts',(-13.7930604654103,-13.6777961936868,
-321.920613959083)) ;
#25725 = CARTESIAN_POINT('Ctrl Pts',(-13.7918555253142,-13.6790111818994,
-321.920592698075)) ;
#25726 = CARTESIAN_POINT('Ctrl Pts',(-13.7912474237859,-13.679624272676,-321.920581968299)) ;
#25727 = CARTESIAN_POINT('Ctrl Pts',(-13.7900193246764,-13.6808622827647,
-321.920560299035)) ;
#25728 = CARTESIAN_POINT('Ctrl Pts',(-13.7893993254175,-13.6814872005603,
-321.920549359522)) ;
#25729 = CARTESIAN_POINT('Ctrl Pts',(-13.7881467659951,-13.6827495250698,
-321.920527259068)) ;
#25730 = CARTESIAN_POINT('Ctrl Pts',(-13.7875142041195,-13.6833869300559,
-321.920516098101)) ;
#25731 = CARTESIAN_POINT('Ctrl Pts',(-13.7862358240191,-13.6846749192253,
-321.920493542483)) ;
#25732 = CARTESIAN_POINT('Ctrl Pts',(-13.7855900039887,-13.6853255015095,
-321.920482147804)) ;
#25733 = CARTESIAN_POINT('Ctrl Pts',(-13.7842843795546,-13.6866405673725,
-321.920459111935)) ;
#25734 = CARTESIAN_POINT('Ctrl Pts',(-13.7836245731173,-13.6873050489948,
-321.920447470712)) ;
#25735 = CARTESIAN_POINT('Ctrl Pts',(-13.7822902124971,-13.6886486701486,
-321.920423928303)) ;
#25736 = CARTESIAN_POINT('Ctrl Pts',(-13.7816156561877,-13.6893278075067,
-321.920412027083)) ;
#25737 = CARTESIAN_POINT('Ctrl Pts',(-13.7802509950926,-13.6907015331921,
-321.920387950571)) ;
#25738 = CARTESIAN_POINT('Ctrl Pts',(-13.7795608879517,-13.6913961192396,
-321.920375775243)) ;
#25739 = CARTESIAN_POINT('Ctrl Pts',(-13.7781642840296,-13.6928015747971,
-321.920351135693)) ;
#25740 = CARTESIAN_POINT('Ctrl Pts',(-13.7774577847946,-13.6935124417614,
-321.920338671434)) ;
#25741 = CARTESIAN_POINT('Ctrl Pts',(-13.7760275127563,-13.694951333307,-321.92031343845)) ;
#25742 = CARTESIAN_POINT('Ctrl Pts',(-13.7753037372358,-13.6956793552114,
-321.920300669684)) ;
#25743 = CARTESIAN_POINT('Ctrl Pts',(-13.7738379827284,-13.697153475549,-321.920274811305)) ;
#25744 = CARTESIAN_POINT('Ctrl Pts',(-13.77309600078,-13.6978995711201,-321.920261721648)) ;
#25745 = CARTESIAN_POINT('Ctrl Pts',(-13.7715928542687,-13.6994108056173,
-321.920235204237)) ;
#25746 = CARTESIAN_POINT('Ctrl Pts',(-13.7708316865645,-13.7001759413929,
-321.920221776437)) ;
#25747 = CARTESIAN_POINT('Ctrl Pts',(-13.7692891369936,-13.7017262740489,
-321.920194564574)) ;
#25748 = CARTESIAN_POINT('Ctrl Pts',(-13.7685077517204,-13.7025114675343,
-321.920180780459)) ;
#25749 = CARTESIAN_POINT('Ctrl Pts',(-13.7669236793154,-13.7041029878782,
-321.920152836808)) ;
#25750 = CARTESIAN_POINT('Ctrl Pts',(-13.7661209885129,-13.7049093110496,
-321.920138677218)) ;
#25751 = CARTESIAN_POINT('Ctrl Pts',(-13.7644931574563,-13.7065442211285,
-321.920109962406)) ;
#25752 = CARTESIAN_POINT('Ctrl Pts',(-13.7636680132028,-13.7073728040697,
-321.920095407126)) ;
#25753 = CARTESIAN_POINT('Ctrl Pts',(-13.7619940636091,-13.7090534260987,
-321.920065879599)) ;
#25754 = CARTESIAN_POINT('Ctrl Pts',(-13.7611452539216,-13.7099054609035,
-321.920050907287)) ;
#25755 = CARTESIAN_POINT('Ctrl Pts',(-13.7594226931801,-13.711634245506,-321.920020523155)) ;
#25756 = CARTESIAN_POINT('Ctrl Pts',(-13.7585489375027,-13.712510990569,-321.920005111267)) ;
#25757 = CARTESIAN_POINT('Ctrl Pts',(-13.7567751315302,-13.7142905250557,
-321.919973824156)) ;
#25758 = CARTESIAN_POINT('Ctrl Pts',(-13.7558750761642,-13.7151933093954,
-321.919957948858)) ;
#25759 = CARTESIAN_POINT('Ctrl Pts',(-13.7540472394486,-13.7170263272011,
-321.919925709733)) ;
#25760 = CARTESIAN_POINT('Ctrl Pts',(-13.7531194525344,-13.7179565552028,
-321.919909345821)) ;
#25761 = CARTESIAN_POINT('Ctrl Pts',(-13.7512346375733,-13.7198459458662,
-321.919876102798)) ;
#25762 = CARTESIAN_POINT('Ctrl Pts',(-13.7502776035718,-13.7208051024933,
-321.919859223599)) ;
#25763 = CARTESIAN_POINT('Ctrl Pts',(-13.7483326902503,-13.7227539216271,
-321.919824921764)) ;
#25764 = CARTESIAN_POINT('Ctrl Pts',(-13.7473448043854,-13.7237435776349,
-321.919807499033)) ;
#25765 = CARTESIAN_POINT('Ctrl Pts',(-13.7453364876211,-13.7257550585561,
-321.919772080225)) ;
#25766 = CARTESIAN_POINT('Ctrl Pts',(-13.7443160496214,-13.7267768763656,
-321.919754084043)) ;
#25767 = CARTESIAN_POINT('Ctrl Pts',(-13.7422408269565,-13.7288544416897,
-321.919717486633)) ;
#25768 = CARTESIAN_POINT('Ctrl Pts',(-13.7411860345493,-13.7299101814644,
-321.91969888529)) ;
#25769 = CARTESIAN_POINT('Ctrl Pts',(-13.7390401924381,-13.7320574559098,
-321.919661043943)) ;
#25770 = CARTESIAN_POINT('Ctrl Pts',(-13.737949134304,-13.7331489821204,-321.919641803815)) ;
#25771 = CARTESIAN_POINT('Ctrl Pts',(-13.7357287336744,-13.7353698059295,
-321.919602649239)) ;
#25772 = CARTESIAN_POINT('Ctrl Pts',(-13.7345993819667,-13.7364990942964,
-321.919582734656)) ;
#25773 = CARTESIAN_POINT('Ctrl Pts',(-13.7323002426266,-13.7387975376917,
-321.919542193329)) ;
#25774 = CARTESIAN_POINT('Ctrl Pts',(-13.7311304449302,-13.7399666826247,
-321.919521566438)) ;
#25775 = CARTESIAN_POINT('Ctrl Pts',(-13.7287481290465,-13.7423470610551,
-321.919479560317)) ;
#25776 = CARTESIAN_POINT('Ctrl Pts',(-13.7275355998298,-13.7435582835266,
-321.919458180928)) ;
#25777 = CARTESIAN_POINT('Ctrl Pts',(-13.7250653940659,-13.7460251741028,
-321.919414627141)) ;
#25778 = CARTESIAN_POINT('Ctrl Pts',(-13.7238077054677,-13.7472808301059,
-321.919392452569)) ;
#25779 = CARTESIAN_POINT('Ctrl Pts',(-13.7212446021085,-13.7498390888763,
-321.919347263082)) ;
#25780 = CARTESIAN_POINT('Ctrl Pts',(-13.7199391741447,-13.7511416783716,
-321.919324247977)) ;
#25781 = CARTESIAN_POINT('Ctrl Pts',(-13.717277850786,-13.7537964588403,-321.919277329243)) ;
#25782 = CARTESIAN_POINT('Ctrl Pts',(-13.7159219408863,-13.7551486352706,
-321.919253425406)) ;
#25783 = CARTESIAN_POINT('Ctrl Pts',(-13.7131567386621,-13.7579054081601,
-321.919204677983)) ;
#25784 = CARTESIAN_POINT('Ctrl Pts',(-13.7117474304253,-13.7593099886303,
-321.91917983417)) ;
#25785 = CARTESIAN_POINT('Ctrl Pts',(-13.7088723308401,-13.7621745627954,
-321.91912915232)) ;
#25786 = CARTESIAN_POINT('Ctrl Pts',(-13.7074065220258,-13.7636345388873,
-321.919103314035)) ;
#25787 = CARTESIAN_POINT('Ctrl Pts',(-13.70441512222,-13.76661308352,-321.919050585294)) ;
#25788 = CARTESIAN_POINT('Ctrl Pts',(-13.7028895119838,-13.7681316327177,
-321.919023694564)) ;
#25789 = CARTESIAN_POINT('Ctrl Pts',(-13.6997749979669,-13.771230701275,-321.918968799274)) ;
#25790 = CARTESIAN_POINT('Ctrl Pts',(-13.6981860730402,-13.7728111992804,
-321.918940794414)) ;
#25791 = CARTESIAN_POINT('Ctrl Pts',(-13.6949411915582,-13.7760377544292,
-321.918883605238)) ;
#25792 = CARTESIAN_POINT('Ctrl Pts',(-13.6932852116582,-13.7776837880639,
-321.918854420593)) ;
#25793 = CARTESIAN_POINT('Ctrl Pts',(-13.6899022395683,-13.7810452287258,
-321.918794801983)) ;
#25794 = CARTESIAN_POINT('Ctrl Pts',(-13.6881752216315,-13.7827606097994,
-321.918764367658)) ;
#25795 = CARTESIAN_POINT('Ctrl Pts',(-13.684645933437,-13.7862647995924,-321.918702175293)) ;
#25796 = CARTESIAN_POINT('Ctrl Pts',(-13.6828436347763,-13.7880535796128,
-321.918670416859)) ;
#25797 = CARTESIAN_POINT('Ctrl Pts',(-13.6804789199589,-13.7903996369732,
-321.91862874977)) ;
#25798 = CARTESIAN_POINT('Ctrl Pts',(-13.6799168203588,-13.7909572334532,
-321.918618845509)) ;
#25799 = CARTESIAN_POINT('Ctrl Pts',(-13.6787263080345,-13.7921380638829,
-321.918597868814)) ;
#25800 = CARTESIAN_POINT('Ctrl Pts',(-13.6780978868282,-13.7927612892295,
-321.918586796262)) ;
#25801 = CARTESIAN_POINT('Ctrl Pts',(-13.6767665319042,-13.7940814558863,
-321.918563338617)) ;
#25802 = CARTESIAN_POINT('Ctrl Pts',(-13.6760635875719,-13.7947783863508,
-321.918550953377)) ;
#25803 = CARTESIAN_POINT('Ctrl Pts',(-13.6745738944745,-13.7962551089636,
-321.91852470677)) ;
#25804 = CARTESIAN_POINT('Ctrl Pts',(-13.6737871322104,-13.7970348876143,
-321.918510845216)) ;
#25805 = CARTESIAN_POINT('Ctrl Pts',(-13.6721192576387,-13.7986876746815,
-321.918481460347)) ;
#25806 = CARTESIAN_POINT('Ctrl Pts',(-13.6712381284496,-13.7995606659679,
-321.9184659368)) ;
#25807 = CARTESIAN_POINT('Ctrl Pts',(-13.669369535232,-13.8014116466694,-321.918433017009)) ;
#25808 = CARTESIAN_POINT('Ctrl Pts',(-13.6683820498343,-13.8023896145311,
-321.91841562047)) ;
#25809 = CARTESIAN_POINT('Ctrl Pts',(-13.6662871039958,-13.8044639236585,
-321.918378714664)) ;
#25810 = CARTESIAN_POINT('Ctrl Pts',(-13.6651796165536,-13.8055602376637,
-321.918359205026)) ;
#25811 = CARTESIAN_POINT('Ctrl Pts',(-13.6628291206958,-13.8078864594264,
-321.918317799503)) ;
#25812 = CARTESIAN_POINT('Ctrl Pts',(-13.6615860781113,-13.8091163326297,
-321.918295903151)) ;
#25813 = CARTESIAN_POINT('Ctrl Pts',(-13.6589467303143,-13.8117270127501,
-321.918249412119)) ;
#25814 = CARTESIAN_POINT('Ctrl Pts',(-13.6575503817547,-13.8131077758095,
-321.918224816848)) ;
#25815 = CARTESIAN_POINT('Ctrl Pts',(-13.6545841492008,-13.8160400109437,
-321.918172571458)) ;
#25816 = CARTESIAN_POINT('Ctrl Pts',(-13.6530142101109,-13.8175914272391,
-321.918144920593)) ;
#25817 = CARTESIAN_POINT('Ctrl Pts',(-13.649677605723,-13.8208875411423,-321.918086156294)) ;
#25818 = CARTESIAN_POINT('Ctrl Pts',(-13.6479108702678,-13.8226321676554,
-321.918055041915)) ;
#25819 = CARTESIAN_POINT('Ctrl Pts',(-13.6441541200476,-13.8263404834621,
-321.917988883907)) ;
#25820 = CARTESIAN_POINT('Ctrl Pts',(-13.6421640157737,-13.8283040819532,
-321.917953839078)) ;
#25821 = CARTESIAN_POINT('Ctrl Pts',(-13.6379301046876,-13.8324797989296,
-321.917879285671)) ;
#25822 = CARTESIAN_POINT('Ctrl Pts',(-13.635686183427,-13.8346918012378,-321.917839775566)) ;
#25823 = CARTESIAN_POINT('Ctrl Pts',(-13.6309097684997,-13.83939798248,-321.917755679256)) ;
#25824 = CARTESIAN_POINT('Ctrl Pts',(-13.6283771282392,-13.841892012472,-321.917711091107)) ;
#25825 = CARTESIAN_POINT('Ctrl Pts',(-13.6229833098943,-13.8472006863084,
-321.917616137236)) ;
#25826 = CARTESIAN_POINT('Ctrl Pts',(-13.620121943785,-13.8500151387998,-321.917565769039)) ;
#25827 = CARTESIAN_POINT('Ctrl Pts',(-13.6140248907664,-13.8560085107072,
-321.917458451974)) ;
#25828 = CARTESIAN_POINT('Ctrl Pts',(-13.6107889622523,-13.8591871839666,
-321.917401499953)) ;
#25829 = CARTESIAN_POINT('Ctrl Pts',(-13.6038903909734,-13.8659589482889,
-321.917280096852)) ;
#25830 = CARTESIAN_POINT('Ctrl Pts',(-13.6002274374487,-13.8695517222049,
-321.917215641754)) ;
#25831 = CARTESIAN_POINT('Ctrl Pts',(-13.5924149577786,-13.8772084494627,
-321.917078184163)) ;
#25832 = CARTESIAN_POINT('Ctrl Pts',(-13.5882650315659,-13.8812719938123,
-321.917005176554)) ;
#25833 = CARTESIAN_POINT('Ctrl Pts',(-13.5794103844198,-13.8899345533679,
-321.916849420367)) ;
#25834 = CARTESIAN_POINT('Ctrl Pts',(-13.5747051482798,-13.8945330408254,
-321.916766665283)) ;
#25835 = CARTESIAN_POINT('Ctrl Pts',(-13.4660251496906,-14.0006394956279,
-321.914855492211)) ;
#25836 = CARTESIAN_POINT('Ctrl Pts',(-13.360917067357,-14.1009799181697,-321.913013011225)) ;
#25837 = CARTESIAN_POINT('Ctrl Pts',(-12.9934555293007,-14.4439760356215,
-321.906606112049)) ;
#25838 = CARTESIAN_POINT('Ctrl Pts',(-12.7255388078101,-14.6805651119825,
-321.901995665326)) ;
#25839 = CARTESIAN_POINT('Ctrl Pts',(-11.9679977559987,-15.3131987308327,
-321.889261891804)) ;
#25840 = CARTESIAN_POINT('Ctrl Pts',(-11.465409817794,-15.6930369365424,-321.881155919804)) ;
#25841 = CARTESIAN_POINT('Ctrl Pts',(-10.7901467633406,-16.1535944146192,
-321.870873886645)) ;
#25842 = CARTESIAN_POINT('Ctrl Pts',(-10.6335025923433,-16.257136970012,-321.868527818771)) ;
#25843 = CARTESIAN_POINT('Ctrl Pts',(-10.3696157153385,-16.426121533064,-321.864641237735)) ;
#25844 = CARTESIAN_POINT('Ctrl Pts',(-10.2631951885802,-16.4928233869235,
-321.863091264631)) ;
#25845 = CARTESIAN_POINT('Ctrl Pts',(-10.0642590600527,-16.6148406963404,
-321.860225666613)) ;
#25846 = CARTESIAN_POINT('Ctrl Pts',(-9.97191543731357,-16.67042723909,-321.858908027175)) ;
#25847 = CARTESIAN_POINT('Ctrl Pts',(-9.73799206223305,-16.8085989687794,
-321.855600934164)) ;
#25848 = CARTESIAN_POINT('Ctrl Pts',(-9.59582074590066,-16.8901661628774,
-321.85361907834)) ;
#25849 = CARTESIAN_POINT('Ctrl Pts',(-9.27499232951797,-17.0688748920229,
-321.849205477607)) ;
#25850 = CARTESIAN_POINT('Ctrl Pts',(-9.09580766392284,-17.1650300288908,
-321.846780560478)) ;
#25851 = CARTESIAN_POINT('Ctrl Pts',(-8.71562730490277,-17.3614197574898,
-321.841708755823)) ;
#25852 = CARTESIAN_POINT('Ctrl Pts',(-8.51433595414785,-17.4610176884455,
-321.839065541142)) ;
#25853 = CARTESIAN_POINT('Ctrl Pts',(-7.92989044423887,-17.7376885444461,
-321.831484049055)) ;
#25854 = CARTESIAN_POINT('Ctrl Pts',(-7.54263405977385,-17.9057931541581,
-321.82657566955)) ;
#25855 = CARTESIAN_POINT('Ctrl Pts',(-6.83548122026538,-18.1857471782768,
-321.817656725286)) ;
#25856 = CARTESIAN_POINT('Ctrl Pts',(-6.51754975639907,-18.302096823207,-321.813661608518)) ;
#25857 = CARTESIAN_POINT('Ctrl Pts',(-6.10252592606983,-18.4417917957282,
-321.808386735216)) ;
#25858 = CARTESIAN_POINT('Ctrl Pts',(-6.00806810705088,-18.4727806487798,
-321.807182168297)) ;
#25859 = CARTESIAN_POINT('Ctrl Pts',(-5.84993811696017,-18.523317319709,-321.805156017952)) ;
#25860 = CARTESIAN_POINT('Ctrl Pts',(-5.78639575683629,-18.5432652101179,
-321.804339204036)) ;
#25861 = CARTESIAN_POINT('Ctrl Pts',(-5.66352047137734,-18.5811464308203,
-321.802753922913)) ;
#25862 = CARTESIAN_POINT('Ctrl Pts',(-5.60420196725724,-18.5991232888309,
-321.801986167679)) ;
#25863 = CARTESIAN_POINT('Ctrl Pts',(-5.44976255011084,-18.6451212430377,
-321.79998185025)) ;
#25864 = CARTESIAN_POINT('Ctrl Pts',(-5.35451135023511,-18.6726984173206,
-321.798740356006)) ;
#25865 = CARTESIAN_POINT('Ctrl Pts',(-5.23329529387914,-18.7067891771549,
-321.797155511464)) ;
#25866 = CARTESIAN_POINT('Ctrl Pts',(-5.20752237901617,-18.7139801117475,
-321.796818259972)) ;
#25867 = CARTESIAN_POINT('Ctrl Pts',(-4.88067279530254,-18.8044473503303,
-321.792538034086)) ;
#25868 = CARTESIAN_POINT('Ctrl Pts',(-4.5776449616963,-18.8805024603371,-321.788535774688)) ;
#25869 = CARTESIAN_POINT('Ctrl Pts',(-3.82995213981358,-19.0491019582444,
-321.778670535125)) ;
#25870 = CARTESIAN_POINT('Ctrl Pts',(-3.38362170254857,-19.1334242537664,
-321.772792219302)) ;
#25871 = CARTESIAN_POINT('Ctrl Pts',(-2.54134139382648,-19.2621544093536,
-321.761866201931)) ;
#25872 = CARTESIAN_POINT('Ctrl Pts',(-2.14617973628184,-19.3101766546514,
-321.756807599584)) ;
#25873 = CARTESIAN_POINT('Ctrl Pts',(-1.59033795421999,-19.3604517857785,
-321.749818056103)) ;
#25874 = CARTESIAN_POINT('Ctrl Pts',(-1.43068176917797,-19.3729042203815,
-321.74782460285)) ;
#25875 = CARTESIAN_POINT('Ctrl Pts',(-1.15143259223858,-19.3912134571859,
-321.744362943065)) ;
#25876 = CARTESIAN_POINT('Ctrl Pts',(-1.03190551029623,-19.397941319024,-321.742889227387)) ;
#25877 = CARTESIAN_POINT('Ctrl Pts',(-0.796102252058334,-19.4090284021025,
-321.739997183021)) ;
#25878 = CARTESIAN_POINT('Ctrl Pts',(-0.679833882419814,-19.4134486436397,
-321.738578519148)) ;
#25879 = CARTESIAN_POINT('Ctrl Pts',(-0.375642228969848,-19.4222771708154,
-321.73488496426)) ;
#25880 = CARTESIAN_POINT('Ctrl Pts',(-0.187682302120229,-19.4250027819016,
-321.732620827941)) ;
#25881 = CARTESIAN_POINT('Ctrl Pts',(0.000287704542308483,-19.4249999978694,
-321.730371769961)) ;
#25882 = CARTESIAN_POINT('Ctrl Pts',(0.000166810840220334,-19.4249999992838,
-321.519753599958)) ;
#25883 = CARTESIAN_POINT('Ctrl Pts',(-0.137993919525454,-19.4250011857295,
-321.521474048577)) ;
#25884 = CARTESIAN_POINT('Ctrl Pts',(-0.276150831818518,-19.4235283656108,
-321.523185239571)) ;
#25885 = CARTESIAN_POINT('Ctrl Pts',(-0.53957842532853,-19.4179089211439,
-321.526430631963)) ;
#25886 = CARTESIAN_POINT('Ctrl Pts',(-0.664847763116804,-19.4140235202933,
-321.527966437048)) ;
#25887 = CARTESIAN_POINT('Ctrl Pts',(-0.959143785326477,-19.4020437386808,
-321.531557767981)) ;
#25888 = CARTESIAN_POINT('Ctrl Pts',(-1.12811975032796,-19.3929524306718,
-321.533606773427)) ;
#25889 = CARTESIAN_POINT('Ctrl Pts',(-1.82385781940178,-19.346395966334,-321.541996772373)) ;
#25890 = CARTESIAN_POINT('Ctrl Pts',(-2.34910384164736,-19.2896658081241,
-321.548214171527)) ;
#25891 = CARTESIAN_POINT('Ctrl Pts',(-3.4541968831645,-19.1244975507954,-321.561283593549)) ;
#25892 = CARTESIAN_POINT('Ctrl Pts',(-4.03274157583352,-19.0109146101146,
-321.568117561937)) ;
#25893 = CARTESIAN_POINT('Ctrl Pts',(-4.74844141749848,-18.8362592300831,
-321.5769081418)) ;
#25894 = CARTESIAN_POINT('Ctrl Pts',(-4.89125599936391,-18.7996801120878,
-321.578679877863)) ;
#25895 = CARTESIAN_POINT('Ctrl Pts',(-5.10655323721792,-18.7419166053703,
-321.581385834935)) ;
#25896 = CARTESIAN_POINT('Ctrl Pts',(-5.1793516369488,-18.7219294040292,-321.582306896747)) ;
#25897 = CARTESIAN_POINT('Ctrl Pts',(-5.31724060076121,-18.6832054254666,
-321.584064563423)) ;
#25898 = CARTESIAN_POINT('Ctrl Pts',(-5.38235319448009,-18.6645516053336,
-321.584900229818)) ;
#25899 = CARTESIAN_POINT('Ctrl Pts',(-5.54987476571115,-18.6156095752097,
-321.587063843937)) ;
#25900 = CARTESIAN_POINT('Ctrl Pts',(-5.65213392953952,-18.5848166998563,
-321.588397649147)) ;
#25901 = CARTESIAN_POINT('Ctrl Pts',(-5.88117861791001,-18.5137801639357,
-321.591410553692)) ;
#25902 = CARTESIAN_POINT('Ctrl Pts',(-6.00781521955603,-18.4730743005298,
-321.593093934034)) ;
#25903 = CARTESIAN_POINT('Ctrl Pts',(-6.42275009447146,-18.3349803013719,
-321.59865700866)) ;
#25904 = CARTESIAN_POINT('Ctrl Pts',(-6.70917858998817,-18.2321184654356,
-321.602572211709)) ;
#25905 = CARTESIAN_POINT('Ctrl Pts',(-7.67103749769757,-17.8609598394091,
-321.615865964881)) ;
#25906 = CARTESIAN_POINT('Ctrl Pts',(-8.33379196344689,-17.5615096785485,
-321.625252196394)) ;
#25907 = CARTESIAN_POINT('Ctrl Pts',(-9.13759232078629,-17.1425592042303,
-321.636640143357)) ;
#25908 = CARTESIAN_POINT('Ctrl Pts',(-9.29581612929397,-17.0572779809668,
-321.638883515212)) ;
#25909 = CARTESIAN_POINT('Ctrl Pts',(-9.56252306762809,-16.9087120347454,
-321.642667179836)) ;
#25910 = CARTESIAN_POINT('Ctrl Pts',(-9.67161745506976,-16.8465487843646,
-321.644215511052)) ;
#25911 = CARTESIAN_POINT('Ctrl Pts',(-9.89579471499568,-16.7159146321512,
-321.647398929157)) ;
#25912 = CARTESIAN_POINT('Ctrl Pts',(-10.0107877640252,-16.6473025872586,
-321.649032854664)) ;
#25913 = CARTESIAN_POINT('Ctrl Pts',(-10.3133823722953,-16.462486543861,-321.653336574777)) ;
#25914 = CARTESIAN_POINT('Ctrl Pts',(-10.4997290232265,-16.3442653500482,
-321.655991104438)) ;
#25915 = CARTESIAN_POINT('Ctrl Pts',(-11.0107845513228,-16.0076960674286,
-321.663296403465)) ;
#25916 = CARTESIAN_POINT('Ctrl Pts',(-11.330971816777,-15.7826736711742,-321.667900800916)) ;
#25917 = CARTESIAN_POINT('Ctrl Pts',(-12.1840755435748,-15.1437762679862,
-321.680375958236)) ;
#25918 = CARTESIAN_POINT('Ctrl Pts',(-12.702574619797,-14.7115684999939,-321.688178121742)) ;
#25919 = CARTESIAN_POINT('Ctrl Pts',(-13.2815616675023,-14.1754667738344,
-321.697649881584)) ;
#25920 = CARTESIAN_POINT('Ctrl Pts',(-13.3648980395466,-14.0969230302277,
-321.699033277616)) ;
#25921 = CARTESIAN_POINT('Ctrl Pts',(-13.4925199781998,-13.9744916075537,
-321.701187145043)) ;
#25922 = CARTESIAN_POINT('Ctrl Pts',(-13.5372970155398,-13.9311198600096,
-321.70194968251)) ;
#25923 = CARTESIAN_POINT('Ctrl Pts',(-13.6323036452477,-13.8382043555132,
-321.703583200554)) ;
#25924 = CARTESIAN_POINT('Ctrl Pts',(-13.6824736613103,-13.7886009786697,
-321.704455236815)) ;
#25925 = CARTESIAN_POINT('Ctrl Pts',(-13.8185575841274,-13.6525799847649,
-321.706844956081)) ;
#25926 = CARTESIAN_POINT('Ctrl Pts',(-13.9039302876838,-13.565625545279,-321.708370934074)) ;
#25927 = CARTESIAN_POINT('Ctrl Pts',(-14.2859818476908,-13.169100072345,-321.715310012587)) ;
#25928 = CARTESIAN_POINT('Ctrl Pts',(-14.5731792235212,-12.8505610933593,
-321.72082848209)) ;
#25929 = CARTESIAN_POINT('Ctrl Pts',(-15.3020610583068,-11.9862480059601,
-321.73541065802)) ;
#25930 = CARTESIAN_POINT('Ctrl Pts',(-15.7251142087192,-11.4255855040086,
-321.74446844012)) ;
#25931 = CARTESIAN_POINT('Ctrl Pts',(-16.2184492557989,-10.6923162048437,
-321.755575729801)) ;
#25932 = CARTESIAN_POINT('Ctrl Pts',(-16.3178770547089,-10.5399530671514,
-321.757847133281)) ;
#25933 = CARTESIAN_POINT('Ctrl Pts',(-16.4824639559744,-10.2798276497053,
-321.761662955554)) ;
#25934 = CARTESIAN_POINT('Ctrl Pts',(-16.5487420876878,-10.172787716823,-321.763215754428)) ;
#25935 = CARTESIAN_POINT('Ctrl Pts',(-16.6830241611637,-9.95113501770478,
-321.766396031634)) ;
#25936 = CARTESIAN_POINT('Ctrl Pts',(-16.7508986650605,-9.83645145731254,
-321.768022476734)) ;
#25937 = CARTESIAN_POINT('Ctrl Pts',(-16.9262338974671,-9.53311930498286,
-321.772276136057)) ;
#25938 = CARTESIAN_POINT('Ctrl Pts',(-17.031721455623,-9.34335176009869,-321.774888762541)) ;
#25939 = CARTESIAN_POINT('Ctrl Pts',(-17.2029754883793,-9.02273179961395,
-321.779230165537)) ;
#25940 = CARTESIAN_POINT('Ctrl Pts',(-17.2704831731612,-8.89283227116158,
-321.780969569412)) ;
#25941 = CARTESIAN_POINT('Ctrl Pts',(-17.5518823967115,-8.33606659766567,
-321.788350972823)) ;
#25942 = CARTESIAN_POINT('Ctrl Pts',(-17.7514653072975,-7.9021555119831,-321.793915925178)) ;
#25943 = CARTESIAN_POINT('Ctrl Pts',(-18.0129624793137,-7.27359294896615,
-321.801870197743)) ;
#25944 = CARTESIAN_POINT('Ctrl Pts',(-18.0881141909734,-7.08463807105786,
-321.804248659626)) ;
#25945 = CARTESIAN_POINT('Ctrl Pts',(-18.2612309716059,-6.62864667907774,
-321.809985652093)) ;
#25946 = CARTESIAN_POINT('Ctrl Pts',(-18.3563246673777,-6.36057053072341,
-321.81335592492)) ;
#25947 = CARTESIAN_POINT('Ctrl Pts',(-18.4753554835077,-6.00007776171063,
-321.817933958195)) ;
#25948 = CARTESIAN_POINT('Ctrl Pts',(-18.5045478651989,-5.90943327729716,
-321.819088963623)) ;
#25949 = CARTESIAN_POINT('Ctrl Pts',(-18.5528726745015,-5.7555112692649,-321.821059410071)) ;
#25950 = CARTESIAN_POINT('Ctrl Pts',(-18.5723507722436,-5.69234409038847,
-321.821870724917)) ;
#25951 = CARTESIAN_POINT('Ctrl Pts',(-18.6150049985991,-5.5514673381143,-321.82368666578)) ;
#25952 = CARTESIAN_POINT('Ctrl Pts',(-18.6380176541675,-5.4737097661826,-321.824693166421)) ;
#25953 = CARTESIAN_POINT('Ctrl Pts',(-18.7105700238134,-5.22279906336804,
-321.82795180155)) ;
#25954 = CARTESIAN_POINT('Ctrl Pts',(-18.7581887316726,-5.04910051344394,
-321.830224146284)) ;
#25955 = CARTESIAN_POINT('Ctrl Pts',(-18.8743149182203,-4.60116809336992,
-321.836105119959)) ;
#25956 = CARTESIAN_POINT('Ctrl Pts',(-18.9392648631523,-4.32605566155452,
-321.839736903673)) ;
#25957 = CARTESIAN_POINT('Ctrl Pts',(-19.1617721700492,-3.28219698126016,
-321.853490887193)) ;
#25958 = CARTESIAN_POINT('Ctrl Pts',(-19.2787063760172,-2.50555798944725,
-321.863640031432)) ;
#25959 = CARTESIAN_POINT('Ctrl Pts',(-19.3619035059237,-1.57183035006413,
-321.875396848927)) ;
#25960 = CARTESIAN_POINT('Ctrl Pts',(-19.3736651547587,-1.41952688539306,
-321.877301810919)) ;
#25961 = CARTESIAN_POINT('Ctrl Pts',(-19.3918416028456,-1.14147036985379,
-321.88075602338)) ;
#25962 = CARTESIAN_POINT('Ctrl Pts',(-19.3988324445314,-1.01576335473321,
-321.88230886377)) ;
#25963 = CARTESIAN_POINT('Ctrl Pts',(-19.4107060822563,-0.756882535287205,
-321.885489115068)) ;
#25964 = CARTESIAN_POINT('Ctrl Pts',(-19.4154415234315,-0.623708498257451,
-321.887115493897)) ;
#25965 = CARTESIAN_POINT('Ctrl Pts',(-19.4242874661633,-0.273496505423218,
-321.891368709497)) ;
#25966 = CARTESIAN_POINT('Ctrl Pts',(-19.426130878585,-0.0564199848549467,
-321.893980964478)) ;
#25967 = CARTESIAN_POINT('Ctrl Pts',(-19.4231253852299,0.306995018624896,
-321.898321636079)) ;
#25968 = CARTESIAN_POINT('Ctrl Pts',(-19.4202610138816,0.453329770050739,
-321.900060678823)) ;
#25969 = CARTESIAN_POINT('Ctrl Pts',(-19.4010106240392,1.07666074869678,-321.907439640759)) ;
#25970 = CARTESIAN_POINT('Ctrl Pts',(-19.368701749369,1.55299853504544,-321.913002565655)) ;
#25971 = CARTESIAN_POINT('Ctrl Pts',(-19.3064972400198,2.14566234795309,-321.91996522085)) ;
#25972 = CARTESIAN_POINT('Ctrl Pts',(-19.2930312948164,2.26354722416188,-321.921352459695)) ;
#25973 = CARTESIAN_POINT('Ctrl Pts',(-19.2345354755949,2.73711638167395,-321.926943506424)) ;
#25974 = CARTESIAN_POINT('Ctrl Pts',(-19.18074258187,3.09164582336676,-321.931169354635)) ;
#25975 = CARTESIAN_POINT('Ctrl Pts',(-19.0993957261344,3.54312782823735,-321.936694207466)) ;
#25976 = CARTESIAN_POINT('Ctrl Pts',(-19.0808587260183,3.6416345435994,-321.93790854326)) ;
#25977 = CARTESIAN_POINT('Ctrl Pts',(-19.0487157364733,3.8054571728456,-321.939945857371)) ;
#25978 = CARTESIAN_POINT('Ctrl Pts',(-19.0355341776143,3.87085443867606,-321.940763938792)) ;
#25979 = CARTESIAN_POINT('Ctrl Pts',(-19.0061507414482,4.01285298058675,-321.942551501063)) ;
#25980 = CARTESIAN_POINT('Ctrl Pts',(-18.9898221312005,4.089426665838,-321.943522387402)) ;
#25981 = CARTESIAN_POINT('Ctrl Pts',(-18.9380397034528,4.32526279607029,-321.946531711417)) ;
#25982 = CARTESIAN_POINT('Ctrl Pts',(-18.9010419519967,4.48417874869191,-321.948586448672)) ;
#25983 = CARTESIAN_POINT('Ctrl Pts',(-18.831275264322,4.76762764335202,-321.952288629498)) ;
#25984 = CARTESIAN_POINT('Ctrl Pts',(-18.7992617566922,4.89233674040736,-321.953930502264)) ;
#25985 = CARTESIAN_POINT('Ctrl Pts',(-18.6249503843949,5.54438235124987,-321.962569197615)) ;
#25986 = CARTESIAN_POINT('Ctrl Pts',(-18.4616973416045,6.06586223043786,-321.969656847603)) ;
#25987 = CARTESIAN_POINT('Ctrl Pts',(-18.1386381233472,6.96322698490873,-321.98190487759)) ;
#25988 = CARTESIAN_POINT('Ctrl Pts',(-17.9885556775987,7.3422468648902,-321.987096612051)) ;
#25989 = CARTESIAN_POINT('Ctrl Pts',(-17.7645531369485,7.85975337840269,-321.994173851226)) ;
#25990 = CARTESIAN_POINT('Ctrl Pts',(-17.7007141651313,8.0024864548459,-321.996124914457)) ;
#25991 = CARTESIAN_POINT('Ctrl Pts',(-17.5820381049605,8.25945598079471,-321.999635349625)) ;
#25992 = CARTESIAN_POINT('Ctrl Pts',(-17.5277931988091,8.37395621271068,-322.001198750424)) ;
#25993 = CARTESIAN_POINT('Ctrl Pts',(-17.414777989142,8.60659873425551,-322.004374064247)) ;
#25994 = CARTESIAN_POINT('Ctrl Pts',(-17.3559162529916,8.72468940752645,-322.005985219887)) ;
#25995 = CARTESIAN_POINT('Ctrl Pts',(-17.2003629633093,9.02896164959694,-322.010136253277)) ;
#25996 = CARTESIAN_POINT('Ctrl Pts',(-17.1018502710109,9.21419296780131,-322.012662896466)) ;
#25997 = CARTESIAN_POINT('Ctrl Pts',(-16.9329772955244,9.51967968871202,-322.016835976153)) ;
#25998 = CARTESIAN_POINT('Ctrl Pts',(-16.8642891225149,9.64083885914976,-322.018492737576)) ;
#25999 = CARTESIAN_POINT('Ctrl Pts',(-16.5740093021148,10.1402675240861,-322.025336187019)) ;
#26000 = CARTESIAN_POINT('Ctrl Pts',(-16.3409469725165,10.5117202349637,-322.030456974303)) ;
#26001 = CARTESIAN_POINT('Ctrl Pts',(-16.0100360596828,11.0014855310064,-322.037360339665)) ;
#26002 = CARTESIAN_POINT('Ctrl Pts',(-15.9230660812538,11.1269899378105,-322.03914365802)) ;
#26003 = CARTESIAN_POINT('Ctrl Pts',(-15.6303717899033,11.5389103634005,-322.045059472361)) ;
#26004 = CARTESIAN_POINT('Ctrl Pts',(-15.4183288133193,11.8207491411684,-322.049208084551)) ;
#26005 = CARTESIAN_POINT('Ctrl Pts',(-15.1263313986596,12.1876265316248,-322.054834489446)) ;
#26006 = CARTESIAN_POINT('Ctrl Pts',(-15.0531150864741,12.2779423435435,-322.056238562421)) ;
#26007 = CARTESIAN_POINT('Ctrl Pts',(-14.9392095913001,12.415899715649,-322.058416950197)) ;
#26008 = CARTESIAN_POINT('Ctrl Pts',(-14.8990933033547,12.4640108989375,-322.059183041143)) ;
#26009 = CARTESIAN_POINT('Ctrl Pts',(-14.8135567080289,12.5655912905736,-322.060815116098)) ;
#26010 = CARTESIAN_POINT('Ctrl Pts',(-14.7680780506843,12.6190101627988,-322.061682082124)) ;
#26011 = CARTESIAN_POINT('Ctrl Pts',(-14.6441203401758,12.76302198776,-322.064041544328)) ;
#26012 = CARTESIAN_POINT('Ctrl Pts',(-14.565090606265,12.853136829778,-322.065542001388)) ;
#26013 = CARTESIAN_POINT('Ctrl Pts',(-14.2117989258282,13.2485400587148,-322.072221649667)) ;
#26014 = CARTESIAN_POINT('Ctrl Pts',(-13.9287368160246,13.5458234214669,-322.077498021253)) ;
#26015 = CARTESIAN_POINT('Ctrl Pts',(-13.1165490400812,14.3464192405241,-322.092202639988)) ;
#26016 = CARTESIAN_POINT('Ctrl Pts',(-12.5681446078452,14.8292060812908,-322.101633139377)) ;
#26017 = CARTESIAN_POINT('Ctrl Pts',(-11.8529139010312,15.3906194530765,-322.113055541061)) ;
#26018 = CARTESIAN_POINT('Ctrl Pts',(-11.7104338918001,15.4993055746845,-322.115291985747)) ;
#26019 = CARTESIAN_POINT('Ctrl Pts',(-11.4656620440075,15.680719482441,-322.11906771863)) ;
#26020 = CARTESIAN_POINT('Ctrl Pts',(-11.3641320675004,15.75445562357,-322.120614961322)) ;
#26021 = CARTESIAN_POINT('Ctrl Pts',(-11.1526571158441,15.9049312733297,-322.123799258323)) ;
#26022 = CARTESIAN_POINT('Ctrl Pts',(-11.0426176480786,15.9815266820436,-322.125435118724)) ;
#26023 = CARTESIAN_POINT('Ctrl Pts',(-10.7486246860528,16.1816808284978,-322.129751783756)) ;
#26024 = CARTESIAN_POINT('Ctrl Pts',(-10.5633347891934,16.3032415623709,-322.132417146455)) ;
#26025 = CARTESIAN_POINT('Ctrl Pts',(-10.1370283418555,16.5726036544938,-322.13843654961)) ;
#26026 = CARTESIAN_POINT('Ctrl Pts',(-9.89478328088476,16.7183671346557,-322.14177691235)) ;
#26027 = CARTESIAN_POINT('Ctrl Pts',(-9.32727839399568,17.0431891181357,-322.149458386695)) ;
#26028 = CARTESIAN_POINT('Ctrl Pts',(-8.99989390334472,17.2183137186226,-322.153783072134)) ;
#26029 = CARTESIAN_POINT('Ctrl Pts',(-8.30784773249189,17.563370164023,-322.162823789283)) ;
#26030 = CARTESIAN_POINT('Ctrl Pts',(-7.94251862548703,17.7315735880065,-322.167540085576)) ;
#26031 = CARTESIAN_POINT('Ctrl Pts',(-7.46279669768633,17.9346428207089,-322.173787619969)) ;
#26032 = CARTESIAN_POINT('Ctrl Pts',(-7.35293636587208,17.9799631366386,-322.175222148817)) ;
#26033 = CARTESIAN_POINT('Ctrl Pts',(-7.18412166801338,18.0477977016755,-322.177436751616)) ;
#26034 = CARTESIAN_POINT('Ctrl Pts',(-7.12546187302847,18.0710375769158,-322.178208168271)) ;
#26035 = CARTESIAN_POINT('Ctrl Pts',(-7.00183167015459,18.1193219106397,-322.17983891258)) ;
#26036 = CARTESIAN_POINT('Ctrl Pts',(-6.93683777270874,18.1443036494965,-322.180699117302)) ;
#26037 = CARTESIAN_POINT('Ctrl Pts',(-6.76212671099227,18.2103814857112,-322.18301783578)) ;
#26038 = CARTESIAN_POINT('Ctrl Pts',(-6.65216974764954,18.250835298664,-322.184483865171)) ;
#26039 = CARTESIAN_POINT('Ctrl Pts',(-6.46647331192613,18.317252987594,-322.186966981986)) ;
#26040 = CARTESIAN_POINT('Ctrl Pts',(-6.39092702273029,18.3437478689615,-322.187979194431)) ;
#26041 = CARTESIAN_POINT('Ctrl Pts',(-6.19050273883427,18.4126503612684,-322.190668040386)) ;
#26042 = CARTESIAN_POINT('Ctrl Pts',(-6.06535299929608,18.4542545346315,-322.192350529913)) ;
#26043 = CARTESIAN_POINT('Ctrl Pts',(-5.39307697334305,18.6701652400179,-322.201391544757)) ;
#26044 = CARTESIAN_POINT('Ctrl Pts',(-4.83884768270826,18.8214214061858,-322.20884663313)) ;
#26045 = CARTESIAN_POINT('Ctrl Pts',(-4.00110471714039,19.0105968930812,-322.219861174234)) ;
#26046 = CARTESIAN_POINT('Ctrl Pts',(-3.72213119814023,19.0671805195667,-322.223489568204)) ;
#26047 = CARTESIAN_POINT('Ctrl Pts',(-3.23009299049653,19.1557691316164,-322.229802649641)) ;
#26048 = CARTESIAN_POINT('Ctrl Pts',(-3.01755101323832,19.1903980642888,-322.232501748979)) ;
#26049 = CARTESIAN_POINT('Ctrl Pts',(-2.67292870491131,19.24067957461,-322.236830843358)) ;
#26050 = CARTESIAN_POINT('Ctrl Pts',(-2.54118668679324,19.2585219742975,-322.238474694233)) ;
#26051 = CARTESIAN_POINT('Ctrl Pts',(-2.2827284418658,19.2908278533652,-322.241678298675)) ;
#26052 = CARTESIAN_POINT('Ctrl Pts',(-2.15603229868407,19.3053985502647,-322.24323867526)) ;
#26053 = CARTESIAN_POINT('Ctrl Pts',(-1.84594096685738,19.3379699557666,-322.247034308825)) ;
#26054 = CARTESIAN_POINT('Ctrl Pts',(-1.66241537467799,19.3546106994087,-322.249260695636)) ;
#26055 = CARTESIAN_POINT('Ctrl Pts',(-1.26196896667993,19.3851824084985,-322.254080335228)) ;
#26056 = CARTESIAN_POINT('Ctrl Pts',(-1.04499468819214,19.3980887969072,-322.256667314832)) ;
#26057 = CARTESIAN_POINT('Ctrl Pts',(-0.341764790536675,19.4280861127892,
-322.264993508244)) ;
#26058 = CARTESIAN_POINT('Ctrl Pts',(0.144927519837056,19.4305514446397,-322.270661568477)) ;
#26059 = CARTESIAN_POINT('Ctrl Pts',(0.753617700200657,19.4107621670884,-322.277778530952)) ;
#26060 = CARTESIAN_POINT('Ctrl Pts',(0.875997487490465,19.405624337621,-322.279211151562)) ;
#26061 = CARTESIAN_POINT('Ctrl Pts',(1.33998658650594,19.3817467183513,-322.284658631148)) ;
#26062 = CARTESIAN_POINT('Ctrl Pts',(1.6811279580789,19.35514085907,-322.288695501083)) ;
#26063 = CARTESIAN_POINT('Ctrl Pts',(2.12046180633606,19.3091737247416,-322.294016213876)) ;
#26064 = CARTESIAN_POINT('Ctrl Pts',(2.21945497267446,19.2980456987227,-322.295223215219)) ;
#26065 = CARTESIAN_POINT('Ctrl Pts',(2.38450901996773,19.2782048157456,-322.297252142653)) ;
#26066 = CARTESIAN_POINT('Ctrl Pts',(2.45061858922249,19.2699126288385,-322.298069267512)) ;
#26067 = CARTESIAN_POINT('Ctrl Pts',(2.59462631556501,19.2510965389534,-322.299859768106)) ;
#26068 = CARTESIAN_POINT('Ctrl Pts',(2.67250573269195,19.2404396196522,-322.300834602459)) ;
#26069 = CARTESIAN_POINT('Ctrl Pts',(2.91362721410149,19.205952641226,-322.30387072156)) ;
#26070 = CARTESIAN_POINT('Ctrl Pts',(3.07663180624033,19.1805155556675,-322.305948706644)) ;
#26071 = CARTESIAN_POINT('Ctrl Pts',(3.36835222313166,19.1311777265822,-322.309701919699)) ;
#26072 = CARTESIAN_POINT('Ctrl Pts',(3.49718814234211,19.108046288207,-322.31137159351)) ;
#26073 = CARTESIAN_POINT('Ctrl Pts',(4.18102974980211,18.9781201975067,-322.320283188385)) ;
#26074 = CARTESIAN_POINT('Ctrl Pts',(4.73141064502779,18.8484431840874,-322.327619836129)) ;
#26075 = CARTESIAN_POINT('Ctrl Pts',(5.59989972668357,18.6033724321149,-322.339198251705)) ;
#26076 = CARTESIAN_POINT('Ctrl Pts',(5.92200733024302,18.5033557152875,-322.343494847032)) ;
#26077 = CARTESIAN_POINT('Ctrl Pts',(6.42546501764056,18.3325346259777,-322.350189287347)) ;
#26078 = CARTESIAN_POINT('Ctrl Pts',(6.60863371843887,18.2673037707899,-322.352620635035)) ;
#26079 = CARTESIAN_POINT('Ctrl Pts',(6.89979450310611,18.1586617486847,-322.35647739956)) ;
#26080 = CARTESIAN_POINT('Ctrl Pts',(7.00842901518905,18.1170108866149,-322.357914608821)) ;
#26081 = CARTESIAN_POINT('Ctrl Pts',(7.23591754646221,18.0274386223259,-322.360920717728)) ;
#26082 = CARTESIAN_POINT('Ctrl Pts',(7.3546848296242,17.9793119203311,-322.362488109231)) ;
#26083 = CARTESIAN_POINT('Ctrl Pts',(7.646525336519,17.8576770672284,-322.366335649204)) ;
#26084 = CARTESIAN_POINT('Ctrl Pts',(7.81902408683818,17.7828243661498,-322.368606316912)) ;
#26085 = CARTESIAN_POINT('Ctrl Pts',(8.45803550430294,17.4944411709327,-322.377014616087)) ;
#26086 = CARTESIAN_POINT('Ctrl Pts',(8.91711818994298,17.2649599188393,-322.383043225155)) ;
#26087 = CARTESIAN_POINT('Ctrl Pts',(9.91905429851975,16.7134881588428,-322.39641287395)) ;
#26088 = CARTESIAN_POINT('Ctrl Pts',(10.4563932133784,16.3826786531704,-322.403726392021)) ;
#26089 = CARTESIAN_POINT('Ctrl Pts',(11.065599604178,15.9654234142734,-322.412603058772)) ;
#26090 = CARTESIAN_POINT('Ctrl Pts',(11.154005389719,15.9037858107882,-322.413906645861)) ;
#26091 = CARTESIAN_POINT('Ctrl Pts',(11.2967194220409,15.8025085018902,-322.416039819654)) ;
#26092 = CARTESIAN_POINT('Ctrl Pts',(11.3513429377013,15.7633168518619,-322.416863249034)) ;
#26093 = CARTESIAN_POINT('Ctrl Pts',(11.466345344481,15.6798963976054,-322.418612675989)) ;
#26094 = CARTESIAN_POINT('Ctrl Pts',(11.5266742085929,15.6356006686421,-322.419539568829)) ;
#26095 = CARTESIAN_POINT('Ctrl Pts',(11.7022667328295,15.5051054183458,-322.422262384819)) ;
#26096 = CARTESIAN_POINT('Ctrl Pts',(11.8168300768498,15.4179722256755,-322.424070610583)) ;
#26097 = CARTESIAN_POINT('Ctrl Pts',(12.0149512620729,15.2637821733769,-322.427246038466)) ;
#26098 = CARTESIAN_POINT('Ctrl Pts',(12.0989425021021,15.1972922050473,-322.428607722149)) ;
#26099 = CARTESIAN_POINT('Ctrl Pts',(12.4858361754489,14.8857752884396,-322.434944918395)) ;
#26100 = CARTESIAN_POINT('Ctrl Pts',(12.7818733456633,14.6323656460322,-322.439978125299)) ;
#26101 = CARTESIAN_POINT('Ctrl Pts',(13.2283466654119,14.226286705167,-322.447763732511)) ;
#26102 = CARTESIAN_POINT('Ctrl Pts',(13.3842156105213,14.0797429482958,-322.450521116386)) ;
#26103 = CARTESIAN_POINT('Ctrl Pts',(13.8405425313196,13.6362902740204,-322.458690877162)) ;
#26104 = CARTESIAN_POINT('Ctrl Pts',(14.1337717066096,13.3321239459225,-322.464067745774)) ;
#26105 = CARTESIAN_POINT('Ctrl Pts',(14.5263715320709,12.89735859959,-322.471408681557)) ;
#26106 = CARTESIAN_POINT('Ctrl Pts',(14.6343561248546,12.7746995913693,-322.473444060024)) ;
#26107 = CARTESIAN_POINT('Ctrl Pts',(14.8221730074186,12.5558524902735,-322.477012914539)) ;
#26108 = CARTESIAN_POINT('Ctrl Pts',(14.9026486345367,12.4602290565838,-322.478551774362)) ;
#26109 = CARTESIAN_POINT('Ctrl Pts',(15.0710021850157,12.2562223100951,-322.481792261368)) ;
#26110 = CARTESIAN_POINT('Ctrl Pts',(15.1586465097661,12.1476552565352,-322.483491883823)) ;
#26111 = CARTESIAN_POINT('Ctrl Pts',(15.4015300358421,11.8400676341461,-322.488240004634)) ;
#26112 = CARTESIAN_POINT('Ctrl Pts',(15.5540710314681,11.6389520019424,-322.49126669368)) ;
#26113 = CARTESIAN_POINT('Ctrl Pts',(15.9051959723939,11.1567805860924,-322.498360920711)) ;
#26114 = CARTESIAN_POINT('Ctrl Pts',(16.1003165449625,10.873307664811,-322.502405360083)) ;
#26115 = CARTESIAN_POINT('Ctrl Pts',(16.607514919402,10.0928350404621,-322.513297769457)) ;
#26116 = CARTESIAN_POINT('Ctrl Pts',(16.9047702995967,9.58663698366048,-322.520099352405)) ;
#26117 = CARTESIAN_POINT('Ctrl Pts',(17.2543284449089,8.92440767078751,-322.529015093809)) ;
#26118 = CARTESIAN_POINT('Ctrl Pts',(17.328202007139,8.78010919164021,-322.530959551231)) ;
#26119 = CARTESIAN_POINT('Ctrl Pts',(17.4349837030527,8.56493256596178,-322.533872388238)) ;
#26120 = CARTESIAN_POINT('Ctrl Pts',(17.4692843499664,8.4947531373728,-322.534824481347)) ;
#26121 = CARTESIAN_POINT('Ctrl Pts',(17.5321155740631,8.36420982414766,-322.536600941388)) ;
#26122 = CARTESIAN_POINT('Ctrl Pts',(17.5607599820299,8.30390217316753,-322.537423900966)) ;
#26123 = CARTESIAN_POINT('Ctrl Pts',(17.6317875276063,8.1523502884539,-322.539496931454)) ;
#26124 = CARTESIAN_POINT('Ctrl Pts',(17.6737737663007,8.06092224635881,-322.540751901965)) ;
#26125 = CARTESIAN_POINT('Ctrl Pts',(17.8737773937493,7.6163247774033,-322.54686824153)) ;
#26126 = CARTESIAN_POINT('Ctrl Pts',(18.0219293393609,7.25881418096625,-322.55182632041)) ;
#26127 = CARTESIAN_POINT('Ctrl Pts',(18.4495936129414,6.13282434307509,-322.567337205528)) ;
#26128 = CARTESIAN_POINT('Ctrl Pts',(18.691342319068,5.35096005747389,-322.577926246698)) ;
#26129 = CARTESIAN_POINT('Ctrl Pts',(18.9186342108558,4.40895083119452,-322.590076449937)) ;
#26130 = CARTESIAN_POINT('Ctrl Pts',(18.9524383080937,4.26129676235897,-322.591964995753)) ;
#26131 = CARTESIAN_POINT('Ctrl Pts',(19.0111131611252,3.99048654752953,-322.595399308466)) ;
#26132 = CARTESIAN_POINT('Ctrl Pts',(19.0365226431029,3.86745552245288,-322.596948510254)) ;
#26133 = CARTESIAN_POINT('Ctrl Pts',(19.0865217833814,3.6129221452482,-322.60013125896)) ;
#26134 = CARTESIAN_POINT('Ctrl Pts',(19.1109500252098,3.48139475013887,-322.601763670123)) ;
#26135 = CARTESIAN_POINT('Ctrl Pts',(19.1719449121388,3.1329745247032,-322.606057258534)) ;
#26136 = CARTESIAN_POINT('Ctrl Pts',(19.2061897498079,2.91569487581688,-322.608703308823)) ;
#26137 = CARTESIAN_POINT('Ctrl Pts',(19.2755731146343,2.42096961665071,-322.614667768628)) ;
#26138 = CARTESIAN_POINT('Ctrl Pts',(19.3084251679495,2.14325235131007,-322.617972907592)) ;
#26139 = CARTESIAN_POINT('Ctrl Pts',(19.3712810694384,1.49157069937497,-322.625665929551)) ;
#26140 = CARTESIAN_POINT('Ctrl Pts',(19.3964702207311,1.11725397078053,-322.630035863361)) ;
#26141 = CARTESIAN_POINT('Ctrl Pts',(19.4238456911595,0.401536211112973,-322.638409144621)) ;
#26142 = CARTESIAN_POINT('Ctrl Pts',(19.4279018549825,0.0603451208772657,
-322.642408773378)) ;
#26143 = CARTESIAN_POINT('Ctrl Pts',(19.4207056058857,-0.437465243863178,
-322.648341074187)) ;
#26144 = CARTESIAN_POINT('Ctrl Pts',(19.4165445020235,-0.594122496938241,
-322.650222095652)) ;
#26145 = CARTESIAN_POINT('Ctrl Pts',(19.4075059715968,-0.827823698301524,
-322.653059142511)) ;
#26146 = CARTESIAN_POINT('Ctrl Pts',(19.4040641485014,-0.904916910112894,
-322.654000063747)) ;
#26147 = CARTESIAN_POINT('Ctrl Pts',(19.3967727894313,-1.0489651345334,-322.65576914048)) ;
#26148 = CARTESIAN_POINT('Ctrl Pts',(19.393035730014,-1.11592456502311,-322.656596053999)) ;
#26149 = CARTESIAN_POINT('Ctrl Pts',(19.3827016065989,-1.28531678165452,-322.658698684292)) ;
#26150 = CARTESIAN_POINT('Ctrl Pts',(19.3756392530886,-1.38771909676743,-322.659979614227)) ;
#26151 = CARTESIAN_POINT('Ctrl Pts',(19.3334879781438,-1.93560021469249,-322.66687697107)) ;
#26152 = CARTESIAN_POINT('Ctrl Pts',(19.2838466744928,-2.37982390098811,-322.67262216572)) ;
#26153 = CARTESIAN_POINT('Ctrl Pts',(19.1135824941099,-3.53941527140412,-322.687734748529)) ;
#26154 = CARTESIAN_POINT('Ctrl Pts',(18.9681395997243,-4.25043342405456,-322.697100920326)) ;
#26155 = CARTESIAN_POINT('Ctrl Pts',(18.7374211684101,-5.12562614107244,-322.708472414391)) ;
#26156 = CARTESIAN_POINT('Ctrl Pts',(18.6891432179249,-5.29895473644626,-322.710718129449)) ;
#26157 = CARTESIAN_POINT('Ctrl Pts',(18.6030893080468,-5.59208952525797,-322.714504478491)) ;
#26158 = CARTESIAN_POINT('Ctrl Pts',(18.5665465005512,-5.71224545628891,-322.716053179363)) ;
#26159 = CARTESIAN_POINT('Ctrl Pts',(18.4886555040694,-5.95971121910292,-322.719236309663)) ;
#26160 = CARTESIAN_POINT('Ctrl Pts',(18.4471514274265,-6.08696512510024,-322.720869588631)) ;
#26161 = CARTESIAN_POINT('Ctrl Pts',(18.3338456394452,-6.42256080602345,-322.72516898316)) ;
#26162 = CARTESIAN_POINT('Ctrl Pts',(18.2598082240209,-6.63012723024059,-322.727819892744)) ;
#26163 = CARTESIAN_POINT('Ctrl Pts',(18.1296007348864,-6.97643077307825,-322.732236864083)) ;
#26164 = CARTESIAN_POINT('Ctrl Pts',(18.075329986854,-7.11585940440395,-322.734013677263)) ;
#26165 = CARTESIAN_POINT('Ctrl Pts',(17.8340828202528,-7.71508112543066,-322.74165280418)) ;
#26166 = CARTESIAN_POINT('Ctrl Pts',(17.631132195215,-8.16824121288439,-322.747432365097)) ;
#26167 = CARTESIAN_POINT('Ctrl Pts',(17.3686908151508,-8.69875452392265,-322.75435074638)) ;
#26168 = CARTESIAN_POINT('Ctrl Pts',(17.3257015301958,-8.78406610742526,-322.755468300551)) ;
#26169 = CARTESIAN_POINT('Ctrl Pts',(17.1200548013404,-9.18478561513482,-322.760746816746)) ;
#26170 = CARTESIAN_POINT('Ctrl Pts',(16.9494035152645,-9.49601403439818,-322.764931174595)) ;
#26171 = CARTESIAN_POINT('Ctrl Pts',(16.7201446782959,-9.88823920657591,-322.770403673749)) ;
#26172 = CARTESIAN_POINT('Ctrl Pts',(16.6693077448104,-9.97370001252993,-322.771608559738)) ;
#26173 = CARTESIAN_POINT('Ctrl Pts',(16.5833280863899,-10.1157446863749,-322.773635073962)) ;
#26174 = CARTESIAN_POINT('Ctrl Pts',(16.5485464651738,-10.1725449558792,-322.774451928531)) ;
#26175 = CARTESIAN_POINT('Ctrl Pts',(16.4720324121002,-10.2960655693814,-322.77624330347)) ;
#26176 = CARTESIAN_POINT('Ctrl Pts',(16.4301853513035,-10.3627133172376,-322.777219298011)) ;
#26177 = CARTESIAN_POINT('Ctrl Pts',(16.2990757509775,-10.5687344061151,-322.780263328802)) ;
#26178 = CARTESIAN_POINT('Ctrl Pts',(16.2084362314163,-10.7072224253812,-322.782348184611)) ;
#26179 = CARTESIAN_POINT('Ctrl Pts',(16.0426081037255,-10.9536592200321,-322.78611652708)) ;
#26180 = CARTESIAN_POINT('Ctrl Pts',(15.9680716300936,-11.0620347786483,-322.787794465269)) ;
#26181 = CARTESIAN_POINT('Ctrl Pts',(15.5641149076755,-11.6367941532706,-322.796789246488)) ;
#26182 = CARTESIAN_POINT('Ctrl Pts',(15.2153517394306,-12.089239997936,-322.80420199761)) ;
#26183 = CARTESIAN_POINT('Ctrl Pts',(14.6516767220508,-12.7573862988255,-322.815414800771)) ;
#26184 = CARTESIAN_POINT('Ctrl Pts',(14.4507890553021,-12.9844996882753,-322.819278912699)) ;
#26185 = CARTESIAN_POINT('Ctrl Pts',(14.103420788886,-13.3591656750899,-322.825724215304)) ;
#26186 = CARTESIAN_POINT('Ctrl Pts',(13.9597383439891,-13.5092372493731,-322.828326197325)) ;
#26187 = CARTESIAN_POINT('Ctrl Pts',(13.7211677593507,-13.7505452056138,-322.832541873817)) ;
#26188 = CARTESIAN_POINT('Ctrl Pts',(13.6277109279214,-13.8431727957304,-322.83416806751)) ;
#26189 = CARTESIAN_POINT('Ctrl Pts',(13.4411783322032,-14.0243305738142,-322.837364752507)) ;
#26190 = CARTESIAN_POINT('Ctrl Pts',(13.3481511496616,-14.1129013295838,-322.838935570202)) ;
#26191 = CARTESIAN_POINT('Ctrl Pts',(13.1261199870023,-14.3201368594211,-322.842630921113)) ;
#26192 = CARTESIAN_POINT('Ctrl Pts',(12.9963747851105,-14.4379911397491,-322.844748326307)) ;
#26193 = CARTESIAN_POINT('Ctrl Pts',(12.2370340099874,-15.1092093244002,-322.856913022308)) ;
#26194 = CARTESIAN_POINT('Ctrl Pts',(11.5737450844556,-15.6231120215995,-322.866606528407)) ;
#26195 = CARTESIAN_POINT('Ctrl Pts',(10.6026776546373,-16.2796000475014,-322.880355191387)) ;
#26196 = CARTESIAN_POINT('Ctrl Pts',(10.3212369001265,-16.4594720161391,-322.884297958115)) ;
#26197 = CARTESIAN_POINT('Ctrl Pts',(9.95197561359519,-16.6822743362106,-322.889493266984)) ;
#26198 = CARTESIAN_POINT('Ctrl Pts',(9.86827447074587,-16.731923218094,-322.890672413436)) ;
#26199 = CARTESIAN_POINT('Ctrl Pts',(9.74073238547206,-16.8062872103374,-322.892473935217)) ;
#26200 = CARTESIAN_POINT('Ctrl Pts',(9.69716259894677,-16.8314644260805,-322.893090191981)) ;
#26201 = CARTESIAN_POINT('Ctrl Pts',(9.61185976675107,-16.8803163153879,-322.894298813693)) ;
#26202 = CARTESIAN_POINT('Ctrl Pts',(9.57013585944713,-16.9040062325456,-322.894890949063)) ;
#26203 = CARTESIAN_POINT('Ctrl Pts',(9.46867694390825,-16.9611163270856,-322.896332749112)) ;
#26204 = CARTESIAN_POINT('Ctrl Pts',(9.40885224689384,-16.9943758200189,-322.897184504911)) ;
#26205 = CARTESIAN_POINT('Ctrl Pts',(9.26175212567027,-17.0751411752099,-322.899281585752)) ;
#26206 = CARTESIAN_POINT('Ctrl Pts',(9.17428560077857,-17.1222948891907,-322.900530864548)) ;
#26207 = CARTESIAN_POINT('Ctrl Pts',(8.92179119011246,-17.2559258920544,-322.904139893733)) ;
#26208 = CARTESIAN_POINT('Ctrl Pts',(8.75587601677594,-17.340702738409,-322.906514579502)) ;
#26209 = CARTESIAN_POINT('Ctrl Pts',(8.04393633664461,-17.6916558625468,-322.916682092757)) ;
#26210 = CARTESIAN_POINT('Ctrl Pts',(7.4868072470979,-17.9345286581561,-322.924572516332)) ;
#26211 = CARTESIAN_POINT('Ctrl Pts',(6.57490146321972,-18.2821518305876,-322.937066907569)) ;
#26212 = CARTESIAN_POINT('Ctrl Pts',(6.22692190783548,-18.4035825160469,-322.941742950214)) ;
#26213 = CARTESIAN_POINT('Ctrl Pts',(5.72417099986703,-18.5631291656674,-322.948344820402)) ;
#26214 = CARTESIAN_POINT('Ctrl Pts',(5.57205838008161,-18.6093541952061,-322.95032272096)) ;
#26215 = CARTESIAN_POINT('Ctrl Pts',(5.30006249758082,-18.6883761953486,-322.953824508075)) ;
#26216 = CARTESIAN_POINT('Ctrl Pts',(5.18039961511664,-18.7218996678123,-322.955353172802)) ;
#26217 = CARTESIAN_POINT('Ctrl Pts',(4.94753469589348,-18.7847330854415,-322.958305386963)) ;
#26218 = CARTESIAN_POINT('Ctrl Pts',(4.83437337503027,-18.8141736668697,-322.959729753044)) ;
#26219 = CARTESIAN_POINT('Ctrl Pts',(4.58250643362185,-18.8772781531852,-322.962878235672)) ;
#26220 = CARTESIAN_POINT('Ctrl Pts',(4.44368160306907,-18.9104386401209,-322.964599035349)) ;
#26221 = CARTESIAN_POINT('Ctrl Pts',(3.70405155802869,-19.0785164167593,-322.97369633314)) ;
#26222 = CARTESIAN_POINT('Ctrl Pts',(3.09745009698045,-19.1863386514346,-322.980897528552)) ;
#26223 = CARTESIAN_POINT('Ctrl Pts',(2.20442059347208,-19.3016112149995,-322.991413987379)) ;
#26224 = CARTESIAN_POINT('Ctrl Pts',(1.92131974369172,-19.3318440886322,-322.994737745289)) ;
#26225 = CARTESIAN_POINT('Ctrl Pts',(1.36637633688919,-19.3787966821376,-323.001293732493)) ;
#26226 = CARTESIAN_POINT('Ctrl Pts',(1.09464332293375,-19.3960434259652,-323.004522971869)) ;
#26227 = CARTESIAN_POINT('Ctrl Pts',(0.737648523269101,-19.4111755419578,
-323.008833033094)) ;
#26228 = CARTESIAN_POINT('Ctrl Pts',(0.652635922886302,-19.4142197265943,
-323.009864465169)) ;
#26229 = CARTESIAN_POINT('Ctrl Pts',(0.501713535925727,-19.4186316221097,
-323.011706476176)) ;
#26230 = CARTESIAN_POINT('Ctrl Pts',(0.435811563933142,-19.4202224198884,
-323.012514542114)) ;
#26231 = CARTESIAN_POINT('Ctrl Pts',(0.312331841668734,-19.4225742223848,
-323.014036349015)) ;
#26232 = CARTESIAN_POINT('Ctrl Pts',(0.254756450495114,-19.4234147292876,
-323.014748980697)) ;
#26233 = CARTESIAN_POINT('Ctrl Pts',(0.131498421320462,-19.4246659545244,
-323.016280492723)) ;
#26234 = CARTESIAN_POINT('Ctrl Pts',(0.0658157106903807,-19.4249995511085,
-323.017100204061)) ;
#26235 = CARTESIAN_POINT('Ctrl Pts',(0.000132620481587507,-19.4249999995473,
-323.017923084864)) ;
#26236 = CARTESIAN_POINT('Origin',(0.,0.,-328.125)) ;
#26237 = CARTESIAN_POINT('',(-0.000256514499293202,-19.4249998742613,-324.730315018138)) ;
#26238 = CARTESIAN_POINT('',(-0.000363249087843348,-19.4249999966036,-324.51951242736)) ;
#26239 = CARTESIAN_POINT('',(-2.37887640734373E-15,-19.425,-328.125)) ;
#26240 = CARTESIAN_POINT('Ctrl Pts',(-0.000256517197342009,-19.4249999983063,
-324.730314803303)) ;
#26241 = CARTESIAN_POINT('Ctrl Pts',(0.125871645587764,-19.4250016638941,
-324.728731715617)) ;
#26242 = CARTESIAN_POINT('Ctrl Pts',(0.25199692284909,-19.4237748883942,-324.727155907634)) ;
#26243 = CARTESIAN_POINT('Ctrl Pts',(0.492716637007198,-19.4190884685471,
-324.724162542893)) ;
#26244 = CARTESIAN_POINT('Ctrl Pts',(0.607309956047675,-19.4158425335503,
-324.722743703952)) ;
#26245 = CARTESIAN_POINT('Ctrl Pts',(0.841981751499335,-19.4071156800803,
-324.719850540467)) ;
#26246 = CARTESIAN_POINT('Ctrl Pts',(0.962051638294548,-19.4015341913279,
-324.71837692661)) ;
#26247 = CARTESIAN_POINT('Ctrl Pts',(1.24291559657716,-19.3858644433473,-324.71494477395)) ;
#26248 = CARTESIAN_POINT('Ctrl Pts',(1.40365138829175,-19.3748894776853,-324.712992043177)) ;
#26249 = CARTESIAN_POINT('Ctrl Pts',(1.97416110602041,-19.3287984997702,-324.706096689383)) ;
#26250 = CARTESIAN_POINT('Ctrl Pts',(2.38293536698671,-19.2826705519056,-324.701223762598)) ;
#26251 = CARTESIAN_POINT('Ctrl Pts',(3.24382563400641,-19.1577288385263,-324.691005652723)) ;
#26252 = CARTESIAN_POINT('Ctrl Pts',(3.69523829679299,-19.0758012305962,-324.685674552727)) ;
#26253 = CARTESIAN_POINT('Ctrl Pts',(4.15399625952156,-18.9756438451624,-324.680170582219)) ;
#26254 = CARTESIAN_POINT('Ctrl Pts',(4.16466371469226,-18.9733054686336,-324.680042548669)) ;
#26255 = CARTESIAN_POINT('Ctrl Pts',(4.18908042593862,-18.9679315804666,-324.679749373779)) ;
#26256 = CARTESIAN_POINT('Ctrl Pts',(4.20282836465936,-18.964890112875,-324.679584213758)) ;
#26257 = CARTESIAN_POINT('Ctrl Pts',(4.23441152255483,-18.9578669160457,-324.679204583377)) ;
#26258 = CARTESIAN_POINT('Ctrl Pts',(4.25224445378373,-18.9538749614433,-324.67899007854)) ;
#26259 = CARTESIAN_POINT('Ctrl Pts',(4.34722066756254,-18.9324734687161,-324.677846790306)) ;
#26260 = CARTESIAN_POINT('Ctrl Pts',(4.42426270576187,-18.9146181214092,-324.67691636852)) ;
#26261 = CARTESIAN_POINT('Ctrl Pts',(4.74203652589619,-18.8389227732947,-324.673063179854)) ;
#26262 = CARTESIAN_POINT('Ctrl Pts',(4.9817603298835,-18.7769535668658,-324.670119833988)) ;
#26263 = CARTESIAN_POINT('Ctrl Pts',(5.28873764727473,-18.69130646114,-324.66627164003)) ;
#26264 = CARTESIAN_POINT('Ctrl Pts',(5.35713633672492,-18.6718176239355,-324.665409090905)) ;
#26265 = CARTESIAN_POINT('Ctrl Pts',(5.49060971635529,-18.6329932727356,-324.663714641459)) ;
#26266 = CARTESIAN_POINT('Ctrl Pts',(5.55569319506363,-18.6136913719743,-324.662883119783)) ;
#26267 = CARTESIAN_POINT('Ctrl Pts',(5.6926242952028,-18.5722993589952,-324.661121449546)) ;
#26268 = CARTESIAN_POINT('Ctrl Pts',(5.76444747070642,-18.5501326190803,-324.660190453576)) ;
#26269 = CARTESIAN_POINT('Ctrl Pts',(5.97506666101891,-18.4837880062138,-324.657441766396)) ;
#26270 = CARTESIAN_POINT('Ctrl Pts',(6.11349644899662,-18.4384652757121,-324.655611433014)) ;
#26271 = CARTESIAN_POINT('Ctrl Pts',(6.81086585539274,-18.2014255570839,-324.646292685717)) ;
#26272 = CARTESIAN_POINT('Ctrl Pts',(7.3613598910765,-17.9858323805382,-324.638626154682)) ;
#26273 = CARTESIAN_POINT('Ctrl Pts',(8.22659800554869,-17.6005855038616,-324.626424379731)) ;
#26274 = CARTESIAN_POINT('Ctrl Pts',(8.54798077629938,-17.4467633158693,-324.621854655847)) ;
#26275 = CARTESIAN_POINT('Ctrl Pts',(9.02988234878637,-17.1995990524533,-324.614982922847)) ;
#26276 = CARTESIAN_POINT('Ctrl Pts',(9.19359363643251,-17.1126508462491,-324.612644624789)) ;
#26277 = CARTESIAN_POINT('Ctrl Pts',(9.49452168690257,-16.9472609693741,-324.60834219153)) ;
#26278 = CARTESIAN_POINT('Ctrl Pts',(9.63207400723271,-16.869461960622,-324.606373869676)) ;
#26279 = CARTESIAN_POINT('Ctrl Pts',(9.85656108998313,-16.738852116167,-324.603159025708)) ;
#26280 = CARTESIAN_POINT('Ctrl Pts',(9.94405743788405,-16.6870215552464,-324.601905350647)) ;
#26281 = CARTESIAN_POINT('Ctrl Pts',(10.1306587110563,-16.5744949803651,-324.599230028075)) ;
#26282 = CARTESIAN_POINT('Ctrl Pts',(10.2296341597051,-16.5135918191769,-324.597810005638)) ;
#26283 = CARTESIAN_POINT('Ctrl Pts',(10.4864027606522,-16.3523985072033,-324.594122521985)) ;
#26284 = CARTESIAN_POINT('Ctrl Pts',(10.6433050625315,-16.2507119009682,-324.591865741618)) ;
#26285 = CARTESIAN_POINT('Ctrl Pts',(11.2854290470963,-15.8212692710672,-324.582604346409)) ;
#26286 = CARTESIAN_POINT('Ctrl Pts',(11.7571769603466,-15.4739219791359,-324.57574898153)) ;
#26287 = CARTESIAN_POINT('Ctrl Pts',(12.511190882758,-14.8643278951423,-324.564424003201)) ;
#26288 = CARTESIAN_POINT('Ctrl Pts',(12.8026405330555,-14.614052679681,-324.55994474344)) ;
#26289 = CARTESIAN_POINT('Ctrl Pts',(13.1980202915024,-14.2536194184083,-324.553615417755)) ;
#26290 = CARTESIAN_POINT('Ctrl Pts',(13.3083734269114,-14.1506396596358,-324.551819844298)) ;
#26291 = CARTESIAN_POINT('Ctrl Pts',(13.4204144461015,-14.0436148185614,-324.549960967423)) ;
#26292 = CARTESIAN_POINT('Ctrl Pts',(13.4233129959695,-14.0408443225285,-324.549912852529)) ;
#26293 = CARTESIAN_POINT('Ctrl Pts',(13.4282718711619,-14.0361015844445,-324.549830494091)) ;
#26294 = CARTESIAN_POINT('Ctrl Pts',(13.4303326202965,-14.034129785736,-324.549796255889)) ;
#26295 = CARTESIAN_POINT('Ctrl Pts',(13.4338560439608,-14.0307569607785,-324.549737694403)) ;
#26296 = CARTESIAN_POINT('Ctrl Pts',(13.4353189337409,-14.0293561595305,-324.54971337385)) ;
#26297 = CARTESIAN_POINT('Ctrl Pts',(13.437819155381,-14.0269613035568,-324.54967179665)) ;
#26298 = CARTESIAN_POINT('Ctrl Pts',(13.4388565949491,-14.0259673635935,-324.549654541409)) ;
#26299 = CARTESIAN_POINT('Ctrl Pts',(13.4446378196615,-14.0204273140564,-324.549558366964)) ;
#26300 = CARTESIAN_POINT('Ctrl Pts',(13.4493794080407,-14.0158789131888,-324.549479419718)) ;
#26301 = CARTESIAN_POINT('Ctrl Pts',(13.4583102900934,-14.007303198867,-324.549330592116)) ;
#26302 = CARTESIAN_POINT('Ctrl Pts',(13.4625000861162,-14.0032764094957,-324.549260718279)) ;
#26303 = CARTESIAN_POINT('Ctrl Pts',(13.4703934737861,-13.9956833022396,-324.549128977615)) ;
#26304 = CARTESIAN_POINT('Ctrl Pts',(13.4740974577576,-13.9921173928056,-324.54906711594)) ;
#26305 = CARTESIAN_POINT('Ctrl Pts',(13.481077610462,-13.9853920994617,-324.548950457728)) ;
#26306 = CARTESIAN_POINT('Ctrl Pts',(13.4843540854478,-13.9822330338629,-324.548895665254)) ;
#26307 = CARTESIAN_POINT('Ctrl Pts',(13.4905306476756,-13.9762736126845,-324.548792311602)) ;
#26308 = CARTESIAN_POINT('Ctrl Pts',(13.4934309740496,-13.9734735052188,-324.548743753624)) ;
#26309 = CARTESIAN_POINT('Ctrl Pts',(13.498900431314,-13.9681897508018,-324.548652132908)) ;
#26310 = CARTESIAN_POINT('Ctrl Pts',(13.5014697490095,-13.9657062974099,-324.548609072691)) ;
#26311 = CARTESIAN_POINT('Ctrl Pts',(13.5063168374287,-13.9610186066021,-324.548527799163)) ;
#26312 = CARTESIAN_POINT('Ctrl Pts',(13.5085947541932,-13.9588145203626,-324.548489587838)) ;
#26313 = CARTESIAN_POINT('Ctrl Pts',(13.5128937890432,-13.9546527854814,-324.548417441894)) ;
#26314 = CARTESIAN_POINT('Ctrl Pts',(13.5149150214764,-13.9526952550243,-324.548383508838)) ;
#26315 = CARTESIAN_POINT('Ctrl Pts',(13.5187311246206,-13.9489978145049,-324.548319418425)) ;
#26316 = CARTESIAN_POINT('Ctrl Pts',(13.5205260849428,-13.9472579970125,-324.548289262301)) ;
#26317 = CARTESIAN_POINT('Ctrl Pts',(13.5239163009915,-13.9439706620255,-324.548232285751)) ;
#26318 = CARTESIAN_POINT('Ctrl Pts',(13.5255116270924,-13.9424232171111,-324.548205466298)) ;
#26319 = CARTESIAN_POINT('Ctrl Pts',(13.5285259267417,-13.9394983826594,-324.548154776697)) ;
#26320 = CARTESIAN_POINT('Ctrl Pts',(13.5299449555774,-13.9381210501894,-324.548130907318)) ;
#26321 = CARTESIAN_POINT('Ctrl Pts',(13.5326271279239,-13.9355168945112,-324.548085778468)) ;
#26322 = CARTESIAN_POINT('Ctrl Pts',(13.5338903150372,-13.9342901161548,-324.548064519603)) ;
#26323 = CARTESIAN_POINT('Ctrl Pts',(13.5362787561782,-13.9319698857294,-324.548024313505)) ;
#26324 = CARTESIAN_POINT('Ctrl Pts',(13.5374040445636,-13.9308764690549,-324.548005366752)) ;
#26325 = CARTESIAN_POINT('Ctrl Pts',(13.5395324490336,-13.9288078462888,-324.547969522558)) ;
#26326 = CARTESIAN_POINT('Ctrl Pts',(13.5405355922734,-13.9278326681378,-324.547952625497)) ;
#26327 = CARTESIAN_POINT('Ctrl Pts',(13.5424335578306,-13.9259872141917,-324.547920649783)) ;
#26328 = CARTESIAN_POINT('Ctrl Pts',(13.5433284016245,-13.9251169605083,-324.547905571433)) ;
#26329 = CARTESIAN_POINT('Ctrl Pts',(13.5450219554417,-13.9234696275172,-324.547877029699)) ;
#26330 = CARTESIAN_POINT('Ctrl Pts',(13.5458206825035,-13.922692565709,-324.547863566554)) ;
#26331 = CARTESIAN_POINT('Ctrl Pts',(13.5473327385723,-13.9212212704635,-324.547838075791)) ;
#26332 = CARTESIAN_POINT('Ctrl Pts',(13.5480460810647,-13.9205270509469,-324.547826048364)) ;
#26333 = CARTESIAN_POINT('Ctrl Pts',(13.549396836602,-13.9192123037056,-324.547803270597)) ;
#26334 = CARTESIAN_POINT('Ctrl Pts',(13.5500342603979,-13.9185917870089,-324.547792520409)) ;
#26335 = CARTESIAN_POINT('Ctrl Pts',(13.5512415398332,-13.917416368053,-324.547772157067)) ;
#26336 = CARTESIAN_POINT('Ctrl Pts',(13.5518114039996,-13.9168614745954,-324.547762544035)) ;
#26337 = CARTESIAN_POINT('Ctrl Pts',(13.5541461590969,-13.9145877756753,-324.547723154738)) ;
#26338 = CARTESIAN_POINT('Ctrl Pts',(13.5559107570913,-13.9128686695055,-324.547693374316)) ;
#26339 = CARTESIAN_POINT('Ctrl Pts',(13.5593667439018,-13.909500497307,-324.547635029041)) ;
#26340 = CARTESIAN_POINT('Ctrl Pts',(13.5610581590446,-13.907851458339,-324.547606464563)) ;
#26341 = CARTESIAN_POINT('Ctrl Pts',(13.6113030912996,-13.8588474662358,-324.546757653284)) ;
#26342 = CARTESIAN_POINT('Ctrl Pts',(13.6596085349735,-13.8112388870189,-324.545933864278)) ;
#26343 = CARTESIAN_POINT('Ctrl Pts',(13.7417232814844,-13.729456544378,-324.544519251147)) ;
#26344 = CARTESIAN_POINT('Ctrl Pts',(13.7756568982474,-13.6954084556214,-324.543930456384)) ;
#26345 = CARTESIAN_POINT('Ctrl Pts',(13.8531958091174,-13.6170282215136,-324.542574888772)) ;
#26346 = CARTESIAN_POINT('Ctrl Pts',(13.8967153045163,-13.5726119610664,-324.541806627025)) ;
#26347 = CARTESIAN_POINT('Ctrl Pts',(14.0191406703622,-13.44645778366,-324.539625352577)) ;
#26348 = CARTESIAN_POINT('Ctrl Pts',(14.0975437442527,-13.3642355706125,-324.53820463081)) ;
#26349 = CARTESIAN_POINT('Ctrl Pts',(14.5608120248477,-12.8697873477605,-324.529679537809)) ;
#26350 = CARTESIAN_POINT('Ctrl Pts',(14.9282977049269,-12.441647794467,-324.522381766745)) ;
#26351 = CARTESIAN_POINT('Ctrl Pts',(15.5267684436833,-11.6796441076633,-324.509883731573)) ;
#26352 = CARTESIAN_POINT('Ctrl Pts',(15.7668828777971,-11.3534149082756,-324.50467318165)) ;
#26353 = CARTESIAN_POINT('Ctrl Pts',(16.1549650848596,-10.7900708977611,-324.495976068044)) ;
#26354 = CARTESIAN_POINT('Ctrl Pts',(16.3083332618964,-10.5568363432292,-324.492457391103)) ;
#26355 = CARTESIAN_POINT('Ctrl Pts',(16.5331213324466,-10.1983947721088,-324.487180013928)) ;
#26356 = CARTESIAN_POINT('Ctrl Pts',(16.6082614965002,-10.0755648505417,-324.485394011543)) ;
#26357 = CARTESIAN_POINT('Ctrl Pts',(16.7456823833816,-9.84521117381113,-324.482085994218)) ;
#26358 = CARTESIAN_POINT('Ctrl Pts',(16.8083105032362,-9.73790324533171,-324.480561428218)) ;
#26359 = CARTESIAN_POINT('Ctrl Pts',(16.9485635630967,-9.49220694874396,-324.477107203508)) ;
#26360 = CARTESIAN_POINT('Ctrl Pts',(17.0255310828992,-9.35345342896753,-324.475182485457)) ;
#26361 = CARTESIAN_POINT('Ctrl Pts',(17.2751091842933,-8.8902357013305,-324.468838184852)) ;
#26362 = CARTESIAN_POINT('Ctrl Pts',(17.4402116662648,-8.5618167475796,-324.464472037462)) ;
#26363 = CARTESIAN_POINT('Ctrl Pts',(17.6094478464844,-8.19993869350873,-324.459768034931)) ;
#26364 = CARTESIAN_POINT('Ctrl Pts',(17.6229258741506,-8.17093211757172,-324.459391704819)) ;
#26365 = CARTESIAN_POINT('Ctrl Pts',(17.8806613827085,-7.61264556268122,-324.452161847256)) ;
#26366 = CARTESIAN_POINT('Ctrl Pts',(18.101043099233,-7.07267000009167,-324.445409332011)) ;
#26367 = CARTESIAN_POINT('Ctrl Pts',(18.3414122534194,-6.39850458998067,-324.436978036906)) ;
#26368 = CARTESIAN_POINT('Ctrl Pts',(18.3847315455827,-6.27295069197035,-324.435407301272)) ;
#26369 = CARTESIAN_POINT('Ctrl Pts',(18.4794735006115,-5.98894257655249,-324.43184483854)) ;
#26370 = CARTESIAN_POINT('Ctrl Pts',(18.5301522950866,-5.83025126503291,-324.429847776945)) ;
#26371 = CARTESIAN_POINT('Ctrl Pts',(18.6018111209536,-5.59548654778721,-324.426872262453)) ;
#26372 = CARTESIAN_POINT('Ctrl Pts',(18.6243788989533,-5.51990555113917,-324.425911106243)) ;
#26373 = CARTESIAN_POINT('Ctrl Pts',(18.6651392612199,-5.38030028139642,-324.424128222736)) ;
#26374 = CARTESIAN_POINT('Ctrl Pts',(18.6834642997845,-5.31631606303256,-324.42330803459)) ;
#26375 = CARTESIAN_POINT('Ctrl Pts',(18.7282510747588,-5.15684538950689,-324.421256930535)) ;
#26376 = CARTESIAN_POINT('Ctrl Pts',(18.7543117240835,-5.06124830529967,-324.420021348324)) ;
#26377 = CARTESIAN_POINT('Ctrl Pts',(18.8622572587937,-4.65299210361357,-324.414725295977)) ;
#26378 = CARTESIAN_POINT('Ctrl Pts',(18.9370633718439,-4.33851524724382,-324.410598301299)) ;
#26379 = CARTESIAN_POINT('Ctrl Pts',(19.0415365913418,-3.8449175000952,-324.404115201769)) ;
#26380 = CARTESIAN_POINT('Ctrl Pts',(19.0765989743507,-3.66699848317527,-324.401777065726)) ;
#26381 = CARTESIAN_POINT('Ctrl Pts',(19.1919333517009,-3.03524524941692,-324.393492217077)) ;
#26382 = CARTESIAN_POINT('Ctrl Pts',(19.258541045613,-2.57907301058873,-324.387545118158)) ;
#26383 = CARTESIAN_POINT('Ctrl Pts',(19.3245237143148,-1.97837914170319,-324.37984798158)) ;
#26384 = CARTESIAN_POINT('Ctrl Pts',(19.3386060076449,-1.83562484007966,-324.378028262132)) ;
#26385 = CARTESIAN_POINT('Ctrl Pts',(19.3697622472116,-1.47944957823182,-324.373514213664)) ;
#26386 = CARTESIAN_POINT('Ctrl Pts',(19.3848914093966,-1.26587749898368,-324.370830969847)) ;
#26387 = CARTESIAN_POINT('Ctrl Pts',(19.4036754400626,-0.919575220124958,
-324.366520391534)) ;
#26388 = CARTESIAN_POINT('Ctrl Pts',(19.4095053918465,-0.786981365495109,
-324.364879425956)) ;
#26389 = CARTESIAN_POINT('Ctrl Pts',(19.4182273292702,-0.528204614963243,
-324.361695059482)) ;
#26390 = CARTESIAN_POINT('Ctrl Pts',(19.4212492529852,-0.402032621095737,
-324.360150896082)) ;
#26391 = CARTESIAN_POINT('Ctrl Pts',(19.425230488021,-0.121697365432233,-324.35673779676)) ;
#26392 = CARTESIAN_POINT('Ctrl Pts',(19.4255845678111,0.0324660379283422,
-324.354872818804)) ;
#26393 = CARTESIAN_POINT('Ctrl Pts',(19.418832499331,0.735256114931439,-324.346419201716)) ;
#26394 = CARTESIAN_POINT('Ctrl Pts',(19.3903191585564,1.28342579855236,-324.339967550575)) ;
#26395 = CARTESIAN_POINT('Ctrl Pts',(19.2888463679684,2.35594981702353,-324.327372985851)) ;
#26396 = CARTESIAN_POINT('Ctrl Pts',(19.2175889248286,2.87999431961308,-324.321231531113)) ;
#26397 = CARTESIAN_POINT('Ctrl Pts',(19.0951867294415,3.56841175327356,-324.312916103241)) ;
#26398 = CARTESIAN_POINT('Ctrl Pts',(19.0631169427811,3.73594578876227,-324.310872211801)) ;
#26399 = CARTESIAN_POINT('Ctrl Pts',(19.0128619591295,3.98095875729358,-324.307841030905)) ;
#26400 = CARTESIAN_POINT('Ctrl Pts',(18.99640049962,4.05878313548917,-324.306871960192)) ;
#26401 = CARTESIAN_POINT('Ctrl Pts',(18.9653222899369,4.20137883114159,-324.305083181363)) ;
#26402 = CARTESIAN_POINT('Ctrl Pts',(18.9508506017545,4.26618038530291,-324.304265125958)) ;
#26403 = CARTESIAN_POINT('Ctrl Pts',(18.9142329262094,4.42628405720179,-324.302231806478)) ;
#26404 = CARTESIAN_POINT('Ctrl Pts',(18.8916986239486,4.52149541707464,-324.301012066303)) ;
#26405 = CARTESIAN_POINT('Ctrl Pts',(18.7955134697668,4.91461827353979,-324.295937893922)) ;
#26406 = CARTESIAN_POINT('Ctrl Pts',(18.7155274983197,5.21093361934284,-324.292023534478)) ;
#26407 = CARTESIAN_POINT('Ctrl Pts',(18.6013865024622,5.59716314591487,-324.286852454013)) ;
#26408 = CARTESIAN_POINT('Ctrl Pts',(18.5735372737967,5.68889516736497,-324.285619062832)) ;
#26409 = CARTESIAN_POINT('Ctrl Pts',(18.3868376954508,6.28787365493976,-324.277537520985)) ;
#26410 = CARTESIAN_POINT('Ctrl Pts',(18.2079028459711,6.7886251379805,-324.270656866799)) ;
#26411 = CARTESIAN_POINT('Ctrl Pts',(17.9504630604211,7.42533520745249,-324.261893320593)) ;
#26412 = CARTESIAN_POINT('Ctrl Pts',(17.8905452777847,7.56856107608931,-324.259920427049)) ;
#26413 = CARTESIAN_POINT('Ctrl Pts',(17.7392134782481,7.91845906840116,-324.255100309245)) ;
#26414 = CARTESIAN_POINT('Ctrl Pts',(17.6458975447267,8.12428390398573,-324.252264717981)) ;
#26415 = CARTESIAN_POINT('Ctrl Pts',(17.4911916777543,8.45026776639919,-324.247776341995)) ;
#26416 = CARTESIAN_POINT('Ctrl Pts',(17.4321044106705,8.57149622335695,-324.246107712866)) ;
#26417 = CARTESIAN_POINT('Ctrl Pts',(17.3151450670212,8.80524752328319,-324.242891072728)) ;
#26418 = CARTESIAN_POINT('Ctrl Pts',(17.257426476415,8.91783965421954,-324.241342055688)) ;
#26419 = CARTESIAN_POINT('Ctrl Pts',(17.1159536176771,9.18729419968506,-324.237634838935)) ;
#26420 = CARTESIAN_POINT('Ctrl Pts',(17.0311373660391,9.34358620124853,-324.235484484652)) ;
#26421 = CARTESIAN_POINT('Ctrl Pts',(16.5834638954172,10.1421659680954,-324.224485926699)) ;
#26422 = CARTESIAN_POINT('Ctrl Pts',(16.1863780064869,10.7645702498429,-324.215901696527)) ;
#26423 = CARTESIAN_POINT('Ctrl Pts',(15.516966172878,11.6927232401586,-324.202524228862)) ;
#26424 = CARTESIAN_POINT('Ctrl Pts',(15.2687729781095,12.0150150328863,-324.197755617331)) ;
#26425 = CARTESIAN_POINT('Ctrl Pts',(14.9348352809406,12.4215774745786,-324.191446573768)) ;
#26426 = CARTESIAN_POINT('Ctrl Pts',(14.8581732385816,12.5131762464725,-324.190004892964)) ;
#26427 = CARTESIAN_POINT('Ctrl Pts',(14.7352030803571,12.6573822567672,-324.187698134258)) ;
#26428 = CARTESIAN_POINT('Ctrl Pts',(14.6894466234363,12.7104560620122,-324.186841037902)) ;
#26429 = CARTESIAN_POINT('Ctrl Pts',(14.6022016638557,12.8105528302915,-324.185207934169)) ;
#26430 = CARTESIAN_POINT('Ctrl Pts',(14.5607706929394,12.8576247443385,-324.184432915606)) ;
#26431 = CARTESIAN_POINT('Ctrl Pts',(14.4416251738034,12.9916778148437,-324.182206699129)) ;
#26432 = CARTESIAN_POINT('Ctrl Pts',(14.3633541926598,13.0781606650973,-324.180747296458)) ;
#26433 = CARTESIAN_POINT('Ctrl Pts',(14.0418659142358,13.4270106545796,-324.174774885447)) ;
#26434 = CARTESIAN_POINT('Ctrl Pts',(13.7922015111667,13.683339876464,-324.170188161503)) ;
#26435 = CARTESIAN_POINT('Ctrl Pts',(13.4309912329852,14.0342570680523,-324.163702478683)) ;
#26436 = CARTESIAN_POINT('Ctrl Pts',(13.3252393669374,14.1347052588773,-324.161820737723)) ;
#26437 = CARTESIAN_POINT('Ctrl Pts',(12.8966576208982,14.5327078769028,-324.154274561331)) ;
#26438 = CARTESIAN_POINT('Ctrl Pts',(12.5649123835614,14.8204707748305,-324.148615306103)) ;
#26439 = CARTESIAN_POINT('Ctrl Pts',(12.063003476793,15.2268620032086,-324.140395103994)) ;
#26440 = CARTESIAN_POINT('Ctrl Pts',(11.9002372904511,15.354404318099,-324.137778867419)) ;
#26441 = CARTESIAN_POINT('Ctrl Pts',(11.5937868949547,15.5867360511484,-324.1329489242)) ;
#26442 = CARTESIAN_POINT('Ctrl Pts',(11.4506398493319,15.6921981401101,-324.130730385727)) ;
#26443 = CARTESIAN_POINT('Ctrl Pts',(11.2031853435626,15.8693185102424,-324.126959649701)) ;
#26444 = CARTESIAN_POINT('Ctrl Pts',(11.0995885623812,15.9419498687279,-324.125399870103)) ;
#26445 = CARTESIAN_POINT('Ctrl Pts',(10.8841097264858,16.0899027035284,-324.122193784817)) ;
#26446 = CARTESIAN_POINT('Ctrl Pts',(10.7721378284229,16.1650815095757,-324.120548650556)) ;
#26447 = CARTESIAN_POINT('Ctrl Pts',(10.4704479396077,16.3631117657161,-324.116169918292)) ;
#26448 = CARTESIAN_POINT('Ctrl Pts',(10.2793534988691,16.4838283964614,-324.113452621711)) ;
#26449 = CARTESIAN_POINT('Ctrl Pts',(9.86464297391063,16.7357894524273,-324.107663512867)) ;
#26450 = CARTESIAN_POINT('Ctrl Pts',(9.64041745778643,16.8659473822315,-324.104598986468)) ;
#26451 = CARTESIAN_POINT('Ctrl Pts',(8.90740023340052,17.2720527066333,-324.094748363309)) ;
#26452 = CARTESIAN_POINT('Ctrl Pts',(8.38886557993144,17.5297608709405,-324.088043465915)) ;
#26453 = CARTESIAN_POINT('Ctrl Pts',(7.73855120047659,17.8174906185905,-324.079665980757)) ;
#26454 = CARTESIAN_POINT('Ctrl Pts',(7.61695685527719,17.8698101512118,-324.078100401765)) ;
#26455 = CARTESIAN_POINT('Ctrl Pts',(7.42078717273703,17.9518518614838,-324.0755701538)) ;
#26456 = CARTESIAN_POINT('Ctrl Pts',(7.34654577283159,17.9823617111985,-324.074611542018)) ;
#26457 = CARTESIAN_POINT('Ctrl Pts',(7.16327429091798,18.0563535704242,-324.072240492881)) ;
#26458 = CARTESIAN_POINT('Ctrl Pts',(7.05403516699561,18.0993091202385,-324.070823222436)) ;
#26459 = CARTESIAN_POINT('Ctrl Pts',(6.87934636894805,18.1661793633048,-324.06854594957)) ;
#26460 = CARTESIAN_POINT('Ctrl Pts',(6.81414564487461,18.1907366055378,-324.067693583296)) ;
#26461 = CARTESIAN_POINT('Ctrl Pts',(6.68968579680111,18.2368501955939,-324.066060807299)) ;
#26462 = CARTESIAN_POINT('Ctrl Pts',(6.63045108654184,18.2584698015542,-324.065281306199)) ;
#26463 = CARTESIAN_POINT('Ctrl Pts',(6.45948572471922,18.3199273962544,-324.063025681475)) ;
#26464 = CARTESIAN_POINT('Ctrl Pts',(6.3474941456886,18.3590308469753,-324.061541024162)) ;
#26465 = CARTESIAN_POINT('Ctrl Pts',(5.81915797722385,18.538094667918,-324.054515197923)) ;
#26466 = CARTESIAN_POINT('Ctrl Pts',(5.39850248749337,18.6649329852563,-324.048861014837)) ;
#26467 = CARTESIAN_POINT('Ctrl Pts',(4.5113039961088,18.8999413257944,-324.037023178291)) ;
#26468 = CARTESIAN_POINT('Ctrl Pts',(4.04432598583278,19.0053433169365,-324.030842521955)) ;
#26469 = CARTESIAN_POINT('Ctrl Pts',(3.42985226523001,19.1203615292352,-324.022875955431)) ;
#26470 = CARTESIAN_POINT('Ctrl Pts',(3.28547088461554,19.1456990652919,-324.021015511383)) ;
#26471 = CARTESIAN_POINT('Ctrl Pts',(2.92637835450433,19.2045346957661,-324.016419498541)) ;
#26472 = CARTESIAN_POINT('Ctrl Pts',(2.71136555680763,19.2360687306529,-324.013695170536)) ;
#26473 = CARTESIAN_POINT('Ctrl Pts',(2.36367789851189,19.2811156199011,-324.009336618072)) ;
#26474 = CARTESIAN_POINT('Ctrl Pts',(2.23131414254014,19.2968813545335,-324.007688177499)) ;
#26475 = CARTESIAN_POINT('Ctrl Pts',(1.97365977504464,19.3248838745931,-324.004500181916)) ;
#26476 = CARTESIAN_POINT('Ctrl Pts',(1.84839171316729,19.3372675887003,-324.002959746504)) ;
#26477 = CARTESIAN_POINT('Ctrl Pts',(1.54192781274599,19.3645587392681,-323.999213364857)) ;
#26478 = CARTESIAN_POINT('Ctrl Pts',(1.36062595790063,19.3781416468176,-323.997016048999)) ;
#26479 = CARTESIAN_POINT('Ctrl Pts',(0.481697117337168,19.4315940296009,-323.986444469316)) ;
#26480 = CARTESIAN_POINT('Ctrl Pts',(-0.217547312467332,19.4363461749917,
-323.978300685476)) ;
#26481 = CARTESIAN_POINT('Ctrl Pts',(-1.34665732998864,19.3830707002484,-323.965093091122)) ;
#26482 = CARTESIAN_POINT('Ctrl Pts',(-1.77699310810494,19.3483645174177,-323.960040303611)) ;
#26483 = CARTESIAN_POINT('Ctrl Pts',(-2.32718005746257,19.2854810742828,-323.953403329958)) ;
#26484 = CARTESIAN_POINT('Ctrl Pts',(-2.44841304287205,19.270464986377,-323.951929586599)) ;
#26485 = CARTESIAN_POINT('Ctrl Pts',(-2.63948654898389,19.2449661380225,-323.949583993282)) ;
#26486 = CARTESIAN_POINT('Ctrl Pts',(-2.70942545630609,19.2352443337843,-323.948720584755)) ;
#26487 = CARTESIAN_POINT('Ctrl Pts',(-2.84096362654731,19.2162283322199,-323.94708638334)) ;
#26488 = CARTESIAN_POINT('Ctrl Pts',(-2.90257422886891,19.2070187295803,-323.946316678993)) ;
#26489 = CARTESIAN_POINT('Ctrl Pts',(-3.07706368467753,19.1800771629516,-323.944125735647)) ;
#26490 = CARTESIAN_POINT('Ctrl Pts',(-3.18983180186316,19.1616453864455,-323.942696681624)) ;
#26491 = CARTESIAN_POINT('Ctrl Pts',(-3.96824790430937,19.0273524374654,-323.932756716078)) ;
#26492 = CARTESIAN_POINT('Ctrl Pts',(-4.62761855989996,18.8778250618139,-323.923971883679)) ;
#26493 = CARTESIAN_POINT('Ctrl Pts',(-5.60415085812844,18.6021255205123,-323.910908739748)) ;
#26494 = CARTESIAN_POINT('Ctrl Pts',(-5.92797981419138,18.5014766084425,-323.90656452254)) ;
#26495 = CARTESIAN_POINT('Ctrl Pts',(-6.48574386535623,18.3119705275486,-323.899096358991)) ;
#26496 = CARTESIAN_POINT('Ctrl Pts',(-6.72090440067535,18.2269740352565,-323.895951905491)) ;
#26497 = CARTESIAN_POINT('Ctrl Pts',(-7.08425283639934,18.0876571089554,-323.891104698753)) ;
#26498 = CARTESIAN_POINT('Ctrl Pts',(-7.21360812391362,18.0364585171606,-323.889381236262)) ;
#26499 = CARTESIAN_POINT('Ctrl Pts',(-7.45819832737231,17.9365979636946,-323.88612644729)) ;
#26500 = CARTESIAN_POINT('Ctrl Pts',(-7.57353504542024,17.8882038160591,-323.884593354671)) ;
#26501 = CARTESIAN_POINT('Ctrl Pts',(-7.83920315812354,17.7737020941868,-323.881065128646)) ;
#26502 = CARTESIAN_POINT('Ctrl Pts',(-7.98917974606112,17.7067952880801,-323.879075716891)) ;
#26503 = CARTESIAN_POINT('Ctrl Pts',(-8.54045436631188,17.4524334512764,-323.871766159098)) ;
#26504 = CARTESIAN_POINT('Ctrl Pts',(-8.93615502989921,17.2531715535896,-323.866528474948)) ;
#26505 = CARTESIAN_POINT('Ctrl Pts',(-9.4963717609437,16.9466175085144,-323.859038723582)) ;
#26506 = CARTESIAN_POINT('Ctrl Pts',(-9.66661576643364,16.8500878710835,-323.856751827851)) ;
#26507 = CARTESIAN_POINT('Ctrl Pts',(-10.2965813990487,16.4802027576613,-323.84821915828)) ;
#26508 = CARTESIAN_POINT('Ctrl Pts',(-10.7464086564466,16.1904715545451,-323.841990346003)) ;
#26509 = CARTESIAN_POINT('Ctrl Pts',(-11.2811101066073,15.8139613020223,-323.834147853795)) ;
#26510 = CARTESIAN_POINT('Ctrl Pts',(-11.3778829491473,15.7444782966092,-323.832709865522)) ;
#26511 = CARTESIAN_POINT('Ctrl Pts',(-11.5305041852741,15.6327540779715,-323.830407571966)) ;
#26512 = CARTESIAN_POINT('Ctrl Pts',(-11.5867739897787,15.5910934617566,-323.829551195723)) ;
#26513 = CARTESIAN_POINT('Ctrl Pts',(-11.693053531867,15.5115138757633,-323.827918171387)) ;
#26514 = CARTESIAN_POINT('Ctrl Pts',(-11.7431071278147,15.4736549848682,-323.827142500227)) ;
#26515 = CARTESIAN_POINT('Ctrl Pts',(-11.8858919402527,15.3645654186613,-323.824911984799)) ;
#26516 = CARTESIAN_POINT('Ctrl Pts',(-11.9781645725456,15.2927391638277,-323.823448887924)) ;
#26517 = CARTESIAN_POINT('Ctrl Pts',(-12.3532041578665,14.9953264616059,-323.817422531285)) ;
#26518 = CARTESIAN_POINT('Ctrl Pts',(-12.6302917279212,14.7626961879381,-323.812783894701)) ;
#26519 = CARTESIAN_POINT('Ctrl Pts',(-13.2996874857151,14.1680528040269,-323.801251471557)) ;
#26520 = CARTESIAN_POINT('Ctrl Pts',(-13.6838801597236,13.7973487684485,-323.794342853331)) ;
#26521 = CARTESIAN_POINT('Ctrl Pts',(-14.1597301004758,13.2987544949148,-323.785547788573)) ;
#26522 = CARTESIAN_POINT('Ctrl Pts',(-14.2657833881751,13.1849251810078,-323.78357069257)) ;
#26523 = CARTESIAN_POINT('Ctrl Pts',(-14.5227155517269,12.9024248212297,-323.778742262111)) ;
#26524 = CARTESIAN_POINT('Ctrl Pts',(-14.6720363590043,12.732367517934,-323.775902574225)) ;
#26525 = CARTESIAN_POINT('Ctrl Pts',(-14.9055849419306,12.4568200054184,-323.77140942221)) ;
#26526 = CARTESIAN_POINT('Ctrl Pts',(-14.9917433325266,12.3529939294072,-323.769740052485)) ;
#26527 = CARTESIAN_POINT('Ctrl Pts',(-15.1565737827816,12.1500986511782,-323.766522973728)) ;
#26528 = CARTESIAN_POINT('Ctrl Pts',(-15.2353735282519,12.0511418367658,-323.764974247692)) ;
#26529 = CARTESIAN_POINT('Ctrl Pts',(-15.4224964045813,11.8113837425712,-323.761269393801)) ;
#26530 = CARTESIAN_POINT('Ctrl Pts',(-15.5298656485882,11.6698523695491,-323.759121084207)) ;
#26531 = CARTESIAN_POINT('Ctrl Pts',(-16.0736049585664,10.9323132982139,-323.748112522918)) ;
#26532 = CARTESIAN_POINT('Ctrl Pts',(-16.4776618053925,10.3132396543224,-323.739517163243)) ;
#26533 = CARTESIAN_POINT('Ctrl Pts',(-17.0477482798001,9.32040262183154,-323.726133710761)) ;
#26534 = CARTESIAN_POINT('Ctrl Pts',(-17.2389175073694,8.96188306883237,-323.721370567336)) ;
#26535 = CARTESIAN_POINT('Ctrl Pts',(-17.4715480200683,8.49057646834734,-323.71506784694)) ;
#26536 = CARTESIAN_POINT('Ctrl Pts',(-17.523402668829,8.38303273438424,-323.713626801781)) ;
#26537 = CARTESIAN_POINT('Ctrl Pts',(-17.6041095747364,8.21162955901805,-323.711320811837)) ;
#26538 = CARTESIAN_POINT('Ctrl Pts',(-17.6336134515915,8.14808017680627,-323.710463839554)) ;
#26539 = CARTESIAN_POINT('Ctrl Pts',(-17.6888743853544,8.02734584519176,-323.708830750218)) ;
#26540 = CARTESIAN_POINT('Ctrl Pts',(-17.7146995681574,7.97019306780394,-323.70805561994)) ;
#26541 = CARTESIAN_POINT('Ctrl Pts',(-17.7877822310987,7.80634645500603,-323.705828667086)) ;
#26542 = CARTESIAN_POINT('Ctrl Pts',(-17.8343556715796,7.69935058278744,-323.704368631563)) ;
#26543 = CARTESIAN_POINT('Ctrl Pts',(-18.0200488044502,7.26202027723913,-323.698387031033)) ;
#26544 = CARTESIAN_POINT('Ctrl Pts',(-18.1509768795058,6.92828513897287,-323.693791468658)) ;
#26545 = CARTESIAN_POINT('Ctrl Pts',(-18.3217870991037,6.45474707416447,-323.687308233108)) ;
#26546 = CARTESIAN_POINT('Ctrl Pts',(-18.3694499854059,6.31782791147704,-323.685437792121)) ;
#26547 = CARTESIAN_POINT('Ctrl Pts',(-18.5552836343323,5.76410319740506,-323.677902025856)) ;
#26548 = CARTESIAN_POINT('Ctrl Pts',(-18.6808364219737,5.34320018011998,-323.672241864091)) ;
#26549 = CARTESIAN_POINT('Ctrl Pts',(-18.8273153261259,4.78354020869679,-323.664878221018)) ;
#26550 = CARTESIAN_POINT('Ctrl Pts',(-18.8611603269011,4.64829974240889,-323.663110816821)) ;
#26551 = CARTESIAN_POINT('Ctrl Pts',(-18.9423153746605,4.30852434499854,-323.65870269278)) ;
#26552 = CARTESIAN_POINT('Ctrl Pts',(-18.9877710768902,4.10356473473042,-323.656072847981)) ;
#26553 = CARTESIAN_POINT('Ctrl Pts',(-19.0563773488577,3.76862351583381,-323.651824633378)) ;
#26554 = CARTESIAN_POINT('Ctrl Pts',(-19.0815407143368,3.63907198188087,-323.650193380017)) ;
#26555 = CARTESIAN_POINT('Ctrl Pts',(-19.1282676049678,3.38467888108712,-323.647013177503)) ;
#26556 = CARTESIAN_POINT('Ctrl Pts',(-19.1499338733852,3.2598627868882,-323.645463624505)) ;
#26557 = CARTESIAN_POINT('Ctrl Pts',(-19.2005335405463,2.95043276379485,-323.641647721112)) ;
#26558 = CARTESIAN_POINT('Ctrl Pts',(-19.228026923018,2.76559623389185,-323.639390818261)) ;
#26559 = CARTESIAN_POINT('Ctrl Pts',(-19.3003523500571,2.22596088937323,-323.632859614584)) ;
#26560 = CARTESIAN_POINT('Ctrl Pts',(-19.3380592406342,1.87028559468797,-323.628628607325)) ;
#26561 = CARTESIAN_POINT('Ctrl Pts',(-19.409703432285,0.953730138556838,-323.61783122505)) ;
#26562 = CARTESIAN_POINT('Ctrl Pts',(-19.4291657242124,0.392053781323674,
-323.61132066603)) ;
#26563 = CARTESIAN_POINT('Ctrl Pts',(-19.4231189534842,-0.300180780468465,
-323.603163308272)) ;
#26564 = CARTESIAN_POINT('Ctrl Pts',(-19.4206637161338,-0.430672913210518,
-323.601619289569)) ;
#26565 = CARTESIAN_POINT('Ctrl Pts',(-19.4121373626804,-0.72571188962875,
-323.598106246829)) ;
#26566 = CARTESIAN_POINT('Ctrl Pts',(-19.4052887613691,-0.890226192792095,
-323.596131857322)) ;
#26567 = CARTESIAN_POINT('Ctrl Pts',(-19.392084821417,-1.13306723477477,-323.593183337395)) ;
#26568 = CARTESIAN_POINT('Ctrl Pts',(-19.3873444389983,-1.21147458190062,
-323.592226064955)) ;
#26569 = CARTESIAN_POINT('Ctrl Pts',(-19.3777034784967,-1.35634584573807,
-323.590445978822)) ;
#26570 = CARTESIAN_POINT('Ctrl Pts',(-19.3729362000099,-1.42281731370898,
-323.589624648043)) ;
#26571 = CARTESIAN_POINT('Ctrl Pts',(-19.3601814528439,-1.5886924852847,-323.58756436198)) ;
#26572 = CARTESIAN_POINT('Ctrl Pts',(-19.3517703978409,-1.68806164873633,
-323.586320642559)) ;
#26573 = CARTESIAN_POINT('Ctrl Pts',(-19.3109055945624,-2.13029524959461,
-323.580749921347)) ;
#26574 = CARTESIAN_POINT('Ctrl Pts',(-19.2701022439277,-2.472325105742,-323.576346942396)) ;
#26575 = CARTESIAN_POINT('Ctrl Pts',(-19.137644587618,-3.37733276370464,-323.564584168215)) ;
#26576 = CARTESIAN_POINT('Ctrl Pts',(-19.0302544704618,-3.93766857669095,
-323.557191003107)) ;
#26577 = CARTESIAN_POINT('Ctrl Pts',(-18.8611536591895,-4.64902164722299,
-323.547853577139)) ;
#26578 = CARTESIAN_POINT('Ctrl Pts',(-18.8219937848632,-4.80510870572095,
-323.545807051461)) ;
#26579 = CARTESIAN_POINT('Ctrl Pts',(-18.7217748465601,-5.18453198790289,
-323.540841931866)) ;
#26580 = CARTESIAN_POINT('Ctrl Pts',(-18.658653576193,-5.40729806358084,-323.537935197315)) ;
#26581 = CARTESIAN_POINT('Ctrl Pts',(-18.5521989494274,-5.75890569536453,
-323.533363931289)) ;
#26582 = CARTESIAN_POINT('Ctrl Pts',(-18.5114695706259,-5.88851212651266,
-323.531682480159)) ;
#26583 = CARTESIAN_POINT('Ctrl Pts',(-18.4303192367839,-6.13757762864983,
-323.528457903134)) ;
#26584 = CARTESIAN_POINT('Ctrl Pts',(-18.3900879269123,-6.25709136951226,
-323.526913584495)) ;
#26585 = CARTESIAN_POINT('Ctrl Pts',(-18.2912709921966,-6.5414551680368,-323.52324533772)) ;
#26586 = CARTESIAN_POINT('Ctrl Pts',(-18.2316164370514,-6.70592219155419,
-323.521128808011)) ;
#26587 = CARTESIAN_POINT('Ctrl Pts',(-17.8615467149122,-7.68474363911383,
-323.508550855591)) ;
#26588 = CARTESIAN_POINT('Ctrl Pts',(-17.4988365365402,-8.47825756652103,
-323.498482177846)) ;
#26589 = CARTESIAN_POINT('Ctrl Pts',(-16.9783588271972,-9.44008994187764,
-323.485646558628)) ;
#26590 = CARTESIAN_POINT('Ctrl Pts',(-16.8692999707021,-9.63362262312248,
-323.483026867081)) ;
#26591 = CARTESIAN_POINT('Ctrl Pts',(-16.6791509620289,-9.9579216801876,-323.478545482386)) ;
#26592 = CARTESIAN_POINT('Ctrl Pts',(-16.5997827615458,-10.0896725987044,
-323.476698594713)) ;
#26593 = CARTESIAN_POINT('Ctrl Pts',(-16.4785276852816,-10.2856514586877,
-323.473902421987)) ;
#26594 = CARTESIAN_POINT('Ctrl Pts',(-16.4378115151813,-10.3505967545955,
-323.472967621136)) ;
#26595 = CARTESIAN_POINT('Ctrl Pts',(-16.3610693846082,-10.4714112008615,
-323.471211808896)) ;
#26596 = CARTESIAN_POINT('Ctrl Pts',(-16.3251390349912,-10.5273396162912,
-323.470392048358)) ;
#26597 = CARTESIAN_POINT('Ctrl Pts',(-16.2327475477995,-10.6695437209957,
-323.468290817608)) ;
#26598 = CARTESIAN_POINT('Ctrl Pts',(-16.1758852825917,-10.7555563057642,
-323.467003982076)) ;
#26599 = CARTESIAN_POINT('Ctrl Pts',(-15.9800496913339,-11.0467206105465,
-323.462599038316)) ;
#26600 = CARTESIAN_POINT('Ctrl Pts',(-15.8378370685598,-11.2496640395573,
-323.459445708451)) ;
#26601 = CARTESIAN_POINT('Ctrl Pts',(-15.1492639469477,-12.1933407660628,
-323.444481118247)) ;
#26602 = CARTESIAN_POINT('Ctrl Pts',(-14.554583351921,-12.8973593787649,-323.432482732829)) ;
#26603 = CARTESIAN_POINT('Ctrl Pts',(-13.7857370178849,-13.6863777352626,
-323.418638470101)) ;
#26604 = CARTESIAN_POINT('Ctrl Pts',(-13.6574251855423,-13.81442065674,-323.416375570281)) ;
#26605 = CARTESIAN_POINT('Ctrl Pts',(-13.4361608112116,-14.02912503643,-323.412553926382)) ;
#26606 = CARTESIAN_POINT('Ctrl Pts',(-13.3441157417402,-14.1167043517115,
-323.410987064035)) ;
#26607 = CARTESIAN_POINT('Ctrl Pts',(-13.1533962175897,-14.2946385471667,
-323.407786699666)) ;
#26608 = CARTESIAN_POINT('Ctrl Pts',(-13.0546340901228,-14.3848897139084,
-323.406154156418)) ;
#26609 = CARTESIAN_POINT('Ctrl Pts',(-12.7910127909742,-14.6208419937983,
-323.401859683262)) ;
#26610 = CARTESIAN_POINT('Ctrl Pts',(-12.6245970202311,-14.7647749434726,
-323.399212892351)) ;
#26611 = CARTESIAN_POINT('Ctrl Pts',(-12.2459747382249,-15.0811629940521,
-323.39332195572)) ;
#26612 = CARTESIAN_POINT('Ctrl Pts',(-12.0324993525569,-15.2520272154325,
-323.390089569789)) ;
#26613 = CARTESIAN_POINT('Ctrl Pts',(-11.3581347485751,-15.7688113265417,
-323.380103799924)) ;
#26614 = CARTESIAN_POINT('Ctrl Pts',(-10.8854138524811,-16.0987701141266,
-323.37342807247)) ;
#26615 = CARTESIAN_POINT('Ctrl Pts',(-10.2871542479516,-16.4779407566661,
-323.365083574892)) ;
#26616 = CARTESIAN_POINT('Ctrl Pts',(-10.1748625083327,-16.5475148281444,
-323.363521179059)) ;
#26617 = CARTESIAN_POINT('Ctrl Pts',(-9.99331188975665,-16.6574537742026,
-323.360995506104)) ;
#26618 = CARTESIAN_POINT('Ctrl Pts',(-9.9244975549191,-16.6985447579445,-323.360038262407)) ;
#26619 = CARTESIAN_POINT('Ctrl Pts',(-9.75438705056792,-16.7986995717895,
-323.357670028279)) ;
#26620 = CARTESIAN_POINT('Ctrl Pts',(-9.65280668031727,-16.8572743101659,
-323.356254208695)) ;
#26621 = CARTESIAN_POINT('Ctrl Pts',(-9.4900543498643,-16.949169426556,-323.353978685847)) ;
#26622 = CARTESIAN_POINT('Ctrl Pts',(-9.4292226447491,-16.9830867667616,-323.353126598324)) ;
#26623 = CARTESIAN_POINT('Ctrl Pts',(-9.31295212156922,-17.0470973083787,
-323.351493826643)) ;
#26624 = CARTESIAN_POINT('Ctrl Pts',(-9.25754657869402,-17.0772490522363,
-323.350714046218)) ;
#26625 = CARTESIAN_POINT('Ctrl Pts',(-9.09742170144324,-17.1633808768052,
-323.348456597574)) ;
#26626 = CARTESIAN_POINT('Ctrl Pts',(-8.99233473141471,-17.2186712830012,
-323.346970375143)) ;
#26627 = CARTESIAN_POINT('Ctrl Pts',(-8.49628707071214,-17.4738818263802,
-323.339944465932)) ;
#26628 = CARTESIAN_POINT('Ctrl Pts',(-8.09912762548097,-17.6614713642143,
-323.334291916759)) ;
#26629 = CARTESIAN_POINT('Ctrl Pts',(-7.25661199318999,-18.0250150484085,
-323.322456552779)) ;
#26630 = CARTESIAN_POINT('Ctrl Pts',(-6.81041448258537,-18.1982922578074,
-323.316276734357)) ;
#26631 = CARTESIAN_POINT('Ctrl Pts',(-6.21977718436647,-18.4028932538056,
-323.308311131244)) ;
#26632 = CARTESIAN_POINT('Ctrl Pts',(-6.08074092390645,-18.4493007513255,
-323.306450830368)) ;
#26633 = CARTESIAN_POINT('Ctrl Pts',(-5.7343191259791,-18.5605878798342,-323.301855104929)) ;
#26634 = CARTESIAN_POINT('Ctrl Pts',(-5.52634483295248,-18.623569778894,-323.299130920621)) ;
#26635 = CARTESIAN_POINT('Ctrl Pts',(-5.18915502957829,-18.7195369145831,
-323.294772535929)) ;
#26636 = CARTESIAN_POINT('Ctrl Pts',(-5.06058028526859,-18.7547039286553,
-323.293124121493)) ;
#26637 = CARTESIAN_POINT('Ctrl Pts',(-4.80990127159673,-18.8205026423085,
-323.289936139191)) ;
#26638 = CARTESIAN_POINT('Ctrl Pts',(-4.68784101703242,-18.8512762591514,
-323.288395691329)) ;
#26639 = CARTESIAN_POINT('Ctrl Pts',(-4.41711430663743,-18.9167393818612,
-323.28500422521)) ;
#26640 = CARTESIAN_POINT('Ctrl Pts',(-4.26832054143699,-18.950867195877,-323.283156978403)) ;
#26641 = CARTESIAN_POINT('Ctrl Pts',(-3.64749333363458,-19.0855794166643,
-323.275513482985)) ;
#26642 = CARTESIAN_POINT('Ctrl Pts',(-3.17219600264366,-19.1703083756524,
-323.26981953233)) ;
#26643 = CARTESIAN_POINT('Ctrl Pts',(-2.5943557281925,-19.2512367216642,-323.262986970316)) ;
#26644 = CARTESIAN_POINT('Ctrl Pts',(-2.49436698198753,-19.2644473142325,
-323.261807687158)) ;
#26645 = CARTESIAN_POINT('Ctrl Pts',(-1.97755099516221,-19.3286383146348,
-323.255722233387)) ;
#26646 = CARTESIAN_POINT('Ctrl Pts',(-1.55925382385643,-19.3668710345487,
-323.250832730254)) ;
#26647 = CARTESIAN_POINT('Ctrl Pts',(-0.913545351985959,-19.4048329170795,
-323.243188570478)) ;
#26648 = CARTESIAN_POINT('Ctrl Pts',(-0.68682738132068,-19.4141797007271,
-323.240485793241)) ;
#26649 = CARTESIAN_POINT('Ctrl Pts',(-0.372335173539643,-19.4216291966745,
-323.236683945311)) ;
#26650 = CARTESIAN_POINT('Ctrl Pts',(-0.284659071174872,-19.4231120915325,
-323.235618343446)) ;
#26651 = CARTESIAN_POINT('Ctrl Pts',(-0.131326814215122,-19.4246670120776,
-323.233742695222)) ;
#26652 = CARTESIAN_POINT('Ctrl Pts',(-0.0656749078580174,-19.4249999242354,
-323.232935613241)) ;
#26653 = CARTESIAN_POINT('Ctrl Pts',(-2.2413097626006E-5,-19.4249999999871,
-323.232124485186)) ;
#26654 = CARTESIAN_POINT('Ctrl Pts',(0.000132646322085553,-19.4249999995471,
-323.01792308454)) ;
#26655 = CARTESIAN_POINT('Ctrl Pts',(-0.143386424633033,-19.4250009795871,
-323.019721098121)) ;
#26656 = CARTESIAN_POINT('Ctrl Pts',(-0.286900965316344,-19.4234114015544,
-323.021534137457)) ;
#26657 = CARTESIAN_POINT('Ctrl Pts',(-0.892780897527133,-19.4099840984498,
-323.029234622781)) ;
#26658 = CARTESIAN_POINT('Ctrl Pts',(-1.35466350679508,-19.383225395553,-323.035215324363)) ;
#26659 = CARTESIAN_POINT('Ctrl Pts',(-2.21603517801831,-19.3023816737848,
-323.046374478159)) ;
#26660 = CARTESIAN_POINT('Ctrl Pts',(-2.61565493465555,-19.2523011719939,
-323.051554477303)) ;
#26661 = CARTESIAN_POINT('Ctrl Pts',(-3.20887809445812,-19.1591458208909,
-323.059188247264)) ;
#26662 = CARTESIAN_POINT('Ctrl Pts',(-3.403846742271,-19.1254697911577,-323.061688538205)) ;
#26663 = CARTESIAN_POINT('Ctrl Pts',(-3.72974769344513,-19.0640370476888,
-323.065849842204)) ;
#26664 = CARTESIAN_POINT('Ctrl Pts',(-3.86096882826084,-19.0378950038165,
-323.067520446422)) ;
#26665 = CARTESIAN_POINT('Ctrl Pts',(-4.1055476061043,-18.9865369903663,-323.070624669101)) ;
#26666 = CARTESIAN_POINT('Ctrl Pts',(-4.21896954152059,-18.9616561533648,
-323.072060375519)) ;
#26667 = CARTESIAN_POINT('Ctrl Pts',(-4.45544312413976,-18.9075552462617,
-323.075045806443)) ;
#26668 = CARTESIAN_POINT('Ctrl Pts',(-4.57844631081098,-18.8781473733737,
-323.076594211844)) ;
#26669 = CARTESIAN_POINT('Ctrl Pts',(-4.873327380895,-18.8045950062122,-323.080296453797)) ;
#26670 = CARTESIAN_POINT('Ctrl Pts',(-5.0449047280323,-18.7592923512697,-323.082442502117)) ;
#26671 = CARTESIAN_POINT('Ctrl Pts',(-5.92843454562076,-18.5130100050128,
-323.093462328778)) ;
#26672 = CARTESIAN_POINT('Ctrl Pts',(-6.62910384577733,-18.273829870117,-323.102070183016)) ;
#26673 = CARTESIAN_POINT('Ctrl Pts',(-7.59162490930686,-17.8826003263373,
-323.114216110483)) ;
#26674 = CARTESIAN_POINT('Ctrl Pts',(-7.8661894456942,-17.7635364260414,-323.117722856702)) ;
#26675 = CARTESIAN_POINT('Ctrl Pts',(-8.25753035144572,-17.5829797630774,
-323.122837994371)) ;
#26676 = CARTESIAN_POINT('Ctrl Pts',(-8.37660260771509,-17.5265659368768,
-323.124410372325)) ;
#26677 = CARTESIAN_POINT('Ctrl Pts',(-8.56740842014738,-17.4337776870325,
-323.126961997382)) ;
#26678 = CARTESIAN_POINT('Ctrl Pts',(-8.63950615788171,-17.3981615352633,
-323.127933593836)) ;
#26679 = CARTESIAN_POINT('Ctrl Pts',(-8.72039468690472,-17.3575759601992,
-323.129033079265)) ;
#26680 = CARTESIAN_POINT('Ctrl Pts',(-8.72940525285799,-17.3530461487548,
-323.129155688443)) ;
#26681 = CARTESIAN_POINT('Ctrl Pts',(-8.74650660093109,-17.3444322311362,
-323.129388645558)) ;
#26682 = CARTESIAN_POINT('Ctrl Pts',(-8.75459806064397,-17.3403494756347,
-323.129498976926)) ;
#26683 = CARTESIAN_POINT('Ctrl Pts',(-8.7706232512677,-17.3322494750861,-323.129717706229)) ;
#26684 = CARTESIAN_POINT('Ctrl Pts',(-8.77855708681536,-17.3282324417637,
-323.129826101507)) ;
#26685 = CARTESIAN_POINT('Ctrl Pts',(-8.79537798527605,-17.3197012229957,
-323.130056142232)) ;
#26686 = CARTESIAN_POINT('Ctrl Pts',(-8.80426433755254,-17.3151856424404,
-323.130177805386)) ;
#26687 = CARTESIAN_POINT('Ctrl Pts',(-8.86959167477885,-17.2819264060786,
-323.13107320469)) ;
#26688 = CARTESIAN_POINT('Ctrl Pts',(-8.92589517362289,-17.2529137288977,
-323.131850483198)) ;
#26689 = CARTESIAN_POINT('Ctrl Pts',(-9.05279843305058,-17.1867341591782,
-323.133615584406)) ;
#26690 = CARTESIAN_POINT('Ctrl Pts',(-9.12331297511337,-17.1494067204736,
-323.134605446849)) ;
#26691 = CARTESIAN_POINT('Ctrl Pts',(-9.33344809044489,-17.036507163536,-323.137580153682)) ;
#26692 = CARTESIAN_POINT('Ctrl Pts',(-9.47237412502849,-16.9596567740692,
-323.139579849131)) ;
#26693 = CARTESIAN_POINT('Ctrl Pts',(-10.1570596056975,-16.569868368094,-323.149572018442)) ;
#26694 = CARTESIAN_POINT('Ctrl Pts',(-10.6883341102687,-16.232249143419,-323.157748498575)) ;
#26695 = CARTESIAN_POINT('Ctrl Pts',(-11.4636366688155,-15.6849608839045,
-323.169954118049)) ;
#26696 = CARTESIAN_POINT('Ctrl Pts',(-11.7203885274914,-15.4940458542533,
-323.174047239196)) ;
#26697 = CARTESIAN_POINT('Ctrl Pts',(-12.1098852388484,-15.1892009672042,
-323.18031153823)) ;
#26698 = CARTESIAN_POINT('Ctrl Pts',(-12.2460031514858,-15.0796735194339,
-323.182511743866)) ;
#26699 = CARTESIAN_POINT('Ctrl Pts',(-12.4775701246374,-14.8881394669293,
-323.186271927244)) ;
#26700 = CARTESIAN_POINT('Ctrl Pts',(-12.5737338567238,-14.8070142145534,
-323.1878386812)) ;
#26701 = CARTESIAN_POINT('Ctrl Pts',(-12.713759455592,-14.6865385970889,-323.190127695147)) ;
#26702 = CARTESIAN_POINT('Ctrl Pts',(-12.7582411459618,-14.6479137874618,
-323.190855996472)) ;
#26703 = CARTESIAN_POINT('Ctrl Pts',(-12.8959578814861,-14.5272269246428,
-323.193114482445)) ;
#26704 = CARTESIAN_POINT('Ctrl Pts',(-12.988582089848,-14.444472546375,-323.194638684284)) ;
#26705 = CARTESIAN_POINT('Ctrl Pts',(-13.1973025715893,-14.2543618308937,
-323.198086021243)) ;
#26706 = CARTESIAN_POINT('Ctrl Pts',(-13.3128945278941,-14.146464779333,-323.200004296898)) ;
#26707 = CARTESIAN_POINT('Ctrl Pts',(-13.6826711172453,-13.7927575400755,
-323.206174862732)) ;
#26708 = CARTESIAN_POINT('Ctrl Pts',(-13.9314651080532,-13.5414153676737,
-323.210378580259)) ;
#26709 = CARTESIAN_POINT('Ctrl Pts',(-14.3477302531199,-13.0972652068633,
-323.217551605327)) ;
#26710 = CARTESIAN_POINT('Ctrl Pts',(-14.518515690468,-12.9076884681071,-323.220538395394)) ;
#26711 = CARTESIAN_POINT('Ctrl Pts',(-15.0718096362092,-12.2686374358373,
-323.230416289805)) ;
#26712 = CARTESIAN_POINT('Ctrl Pts',(-15.4375674512257,-11.8051013117611,
-323.237270876837)) ;
#26713 = CARTESIAN_POINT('Ctrl Pts',(-15.8496772546526,-11.2308489446518,
-323.245751564206)) ;
#26714 = CARTESIAN_POINT('Ctrl Pts',(-15.9168461291785,-11.1354499835129,
-323.247160461846)) ;
#26715 = CARTESIAN_POINT('Ctrl Pts',(-16.0226687870724,-10.9822377054587,
-323.24942763978)) ;
#26716 = CARTESIAN_POINT('Ctrl Pts',(-16.0618786815928,-10.9248118197246,
-323.250278401492)) ;
#26717 = CARTESIAN_POINT('Ctrl Pts',(-16.1361270207473,-10.8148056821631,
-323.251911177553)) ;
#26718 = CARTESIAN_POINT('Ctrl Pts',(-16.171218900861,-10.7622626069916,-323.252692311706)) ;
#26719 = CARTESIAN_POINT('Ctrl Pts',(-16.271846793337,-10.6099890620111,-323.254958586621)) ;
#26720 = CARTESIAN_POINT('Ctrl Pts',(-16.3367208932937,-10.5098247536915,
-323.256452381128)) ;
#26721 = CARTESIAN_POINT('Ctrl Pts',(-16.6354949905299,-10.0390723121715,
-323.263475450053)) ;
#26722 = CARTESIAN_POINT('Ctrl Pts',(-16.8577340450092,-9.66123534115661,
-323.269116717026)) ;
#26723 = CARTESIAN_POINT('Ctrl Pts',(-17.29544083861,-8.85591229306789,-323.280938996491)) ;
#26724 = CARTESIAN_POINT('Ctrl Pts',(-17.5082752987824,-8.42732186496238,
-323.287117038402)) ;
#26725 = CARTESIAN_POINT('Ctrl Pts',(-17.7653603303499,-7.85773973904837,
-323.2950805989)) ;
#26726 = CARTESIAN_POINT('Ctrl Pts',(-17.8241359323304,-7.72348883613966,
-323.296940596201)) ;
#26727 = CARTESIAN_POINT('Ctrl Pts',(-17.9662626870975,-7.3885880259425,-323.30153571232)) ;
#26728 = CARTESIAN_POINT('Ctrl Pts',(-18.0477773443667,-7.18718033204947,
-323.304259592017)) ;
#26729 = CARTESIAN_POINT('Ctrl Pts',(-18.1738218749033,-6.86007212346064,
-323.308617621235)) ;
#26730 = CARTESIAN_POINT('Ctrl Pts',(-18.2204660110835,-6.73520671371519,
-323.310265980438)) ;
#26731 = CARTESIAN_POINT('Ctrl Pts',(-18.3086550532496,-6.49150373083635,
-323.313453935068)) ;
#26732 = CARTESIAN_POINT('Ctrl Pts',(-18.3503371909897,-6.37272277535232,
-323.314994409628)) ;
#26733 = CARTESIAN_POINT('Ctrl Pts',(-18.44939668465,-6.08140169775523,-323.318741096068)) ;
#26734 = CARTESIAN_POINT('Ctrl Pts',(-18.5055117099719,-5.90844489898369,
-323.32093867402)) ;
#26735 = CARTESIAN_POINT('Ctrl Pts',(-18.7660168079652,-5.06537689677788,
-323.331532370737)) ;
#26736 = CARTESIAN_POINT('Ctrl Pts',(-18.9364813393758,-4.38532840550178,
-323.339696610419)) ;
#26737 = CARTESIAN_POINT('Ctrl Pts',(-19.1516948471729,-3.27538460645364,
-323.352907442427)) ;
#26738 = CARTESIAN_POINT('Ctrl Pts',(-19.2195110323268,-2.85060586610566,
-323.357942311224)) ;
#26739 = CARTESIAN_POINT('Ctrl Pts',(-19.2883953883009,-2.3028916600985,-323.364558645826)) ;
#26740 = CARTESIAN_POINT('Ctrl Pts',(-19.3024772982789,-2.1817141738926,-323.366030422663)) ;
#26741 = CARTESIAN_POINT('Ctrl Pts',(-19.32290299794,-1.99023263802887,-323.368373631185)) ;
#26742 = CARTESIAN_POINT('Ctrl Pts',(-19.3300066506805,-1.92001278487359,
-323.369236649854)) ;
#26743 = CARTESIAN_POINT('Ctrl Pts',(-19.3426617857914,-1.78772024384861,
-323.37087076424)) ;
#26744 = CARTESIAN_POINT('Ctrl Pts',(-19.3482975541984,-1.7256565049681,-323.371640777361)) ;
#26745 = CARTESIAN_POINT('Ctrl Pts',(-19.3634319781995,-1.54958535661214,
-323.373833784115)) ;
#26746 = CARTESIAN_POINT('Ctrl Pts',(-19.3722222731532,-1.43551972988006,
-323.375264615431)) ;
#26747 = CARTESIAN_POINT('Ctrl Pts',(-19.4236591336926,-0.681123474079131,
-323.384779930384)) ;
#26748 = CARTESIAN_POINT('Ctrl Pts',(-19.4355585149201,-0.0390939553886075,
-323.393112368081)) ;
#26749 = CARTESIAN_POINT('Ctrl Pts',(-19.4045562047933,0.960219865977938,
-323.40599348878)) ;
#26750 = CARTESIAN_POINT('Ctrl Pts',(-19.3835609533153,1.31772121561742,-323.410587095107)) ;
#26751 = CARTESIAN_POINT('Ctrl Pts',(-19.3303837156406,1.93232920996966,-323.418415075141)) ;
#26752 = CARTESIAN_POINT('Ctrl Pts',(-19.3029176722244,2.18974895868517,-323.421673040308)) ;
#26753 = CARTESIAN_POINT('Ctrl Pts',(-19.2526030924553,2.58605417937906,-323.426651323357)) ;
#26754 = CARTESIAN_POINT('Ctrl Pts',(-19.2333763714757,2.72536886953968,-323.428394268476)) ;
#26755 = CARTESIAN_POINT('Ctrl Pts',(-19.1942435908834,2.98784182698217,-323.431664770204)) ;
#26756 = CARTESIAN_POINT('Ctrl Pts',(-19.1746606018074,3.11104108970512,-323.433194344231)) ;
#26757 = CARTESIAN_POINT('Ctrl Pts',(-19.1270270339797,3.39315488800447,-323.436685015405)) ;
#26758 = CARTESIAN_POINT('Ctrl Pts',(-19.0981802034418,3.55192571237075,-323.438640809748)) ;
#26759 = CARTESIAN_POINT('Ctrl Pts',(-18.9853611507544,4.13170374116557,-323.445756059982)) ;
#26760 = CARTESIAN_POINT('Ctrl Pts',(-18.8894174812303,4.55025518098348,-323.450838260009)) ;
#26761 = CARTESIAN_POINT('Ctrl Pts',(-18.6392171875696,5.49656215316194,-323.462327161267)) ;
#26762 = CARTESIAN_POINT('Ctrl Pts',(-18.4762677729012,6.0216393554429,-323.468698120952)) ;
#26763 = CARTESIAN_POINT('Ctrl Pts',(-18.247806316017,6.66069553474473,-323.476696830969)) ;
#26764 = CARTESIAN_POINT('Ctrl Pts',(-18.2031244281092,6.78185530371852,-323.47822483961)) ;
#26765 = CARTESIAN_POINT('Ctrl Pts',(-18.0991443561076,7.05537567603066,-323.481708164781)) ;
#26766 = CARTESIAN_POINT('Ctrl Pts',(-18.0391241018999,7.20745127241923,-323.48366886308)) ;
#26767 = CARTESIAN_POINT('Ctrl Pts',(-17.9475099913573,7.4312615961913,-323.486601067615)) ;
#26768 = CARTESIAN_POINT('Ctrl Pts',(-17.9173901477882,7.50359207795672,-323.487555978367)) ;
#26769 = CARTESIAN_POINT('Ctrl Pts',(-17.8608219159182,7.63715352240042,-323.489334396038)) ;
#26770 = CARTESIAN_POINT('Ctrl Pts',(-17.8344942318668,7.69843418456466,-323.490156454413)) ;
#26771 = CARTESIAN_POINT('Ctrl Pts',(-17.7678566609664,7.85136414646085,-323.492222479649)) ;
#26772 = CARTESIAN_POINT('Ctrl Pts',(-17.7271528389148,7.94283963524125,-323.493471271692)) ;
#26773 = CARTESIAN_POINT('Ctrl Pts',(-17.5304216763139,8.37591637697794,-323.499438296061)) ;
#26774 = CARTESIAN_POINT('Ctrl Pts',(-17.3652169912488,8.71325984865016,-323.504247640434)) ;
#26775 = CARTESIAN_POINT('Ctrl Pts',(-16.9938018453592,9.41910038404857,-323.514515425724)) ;
#26776 = CARTESIAN_POINT('Ctrl Pts',(-16.7851448551763,9.78609553769101,-323.519977023167)) ;
#26777 = CARTESIAN_POINT('Ctrl Pts',(-16.4137775995368,10.3924020520023,-323.529103359175)) ;
#26778 = CARTESIAN_POINT('Ctrl Pts',(-16.2573764524252,10.6354044033376,-323.532791125172)) ;
#26779 = CARTESIAN_POINT('Ctrl Pts',(-15.9696948736269,11.0611961013223,-323.539287580104)) ;
#26780 = CARTESIAN_POINT('Ctrl Pts',(-15.8405494446539,11.2453638048455,-323.542109648654)) ;
#26781 = CARTESIAN_POINT('Ctrl Pts',(-15.6290127539202,11.5361484432598,-323.546582257078)) ;
#26782 = CARTESIAN_POINT('Ctrl Pts',(-15.5486602988448,11.6442227536989,-323.548248440002)) ;
#26783 = CARTESIAN_POINT('Ctrl Pts',(-15.3905966080659,11.8522652181337,-323.551463650068)) ;
#26784 = CARTESIAN_POINT('Ctrl Pts',(-15.3130189126214,11.9523264088609,-323.553013646823)) ;
#26785 = CARTESIAN_POINT('Ctrl Pts',(-15.1237890434908,12.1915320905379,-323.556728773702)) ;
#26786 = CARTESIAN_POINT('Ctrl Pts',(-15.0111874100405,12.3299108843271,-323.55888596738)) ;
#26787 = CARTESIAN_POINT('Ctrl Pts',(-14.4253167372631,13.0299777560931,-323.569851873545)) ;
#26788 = CARTESIAN_POINT('Ctrl Pts',(-13.9223705892237,13.566048829545,-323.578399615859)) ;
#26789 = CARTESIAN_POINT('Ctrl Pts',(-13.0945376844315,14.3537578057832,-323.591757265473)) ;
#26790 = CARTESIAN_POINT('Ctrl Pts',(-12.7899972030179,14.625773496284,-323.596543579263)) ;
#26791 = CARTESIAN_POINT('Ctrl Pts',(-12.3854347032698,14.9648234389019,-323.602873089819)) ;
#26792 = CARTESIAN_POINT('Ctrl Pts',(-12.2930480739379,15.0408079016813,-323.60431682358)) ;
#26793 = CARTESIAN_POINT('Ctrl Pts',(-12.1454093999765,15.1599660522091,-323.606626065588)) ;
#26794 = CARTESIAN_POINT('Ctrl Pts',(-12.090615197618,15.2037023232426,-323.607483563056)) ;
#26795 = CARTESIAN_POINT('Ctrl Pts',(-11.9863866292015,15.2859768849173,-323.609116715607)) ;
#26796 = CARTESIAN_POINT('Ctrl Pts',(-11.9370001648602,15.3245744085783,-323.609891375306)) ;
#26797 = CARTESIAN_POINT('Ctrl Pts',(-11.7953043855647,15.4342148290028,-323.612115224577)) ;
#26798 = CARTESIAN_POINT('Ctrl Pts',(-11.7025417703818,15.5046673292005,-323.613572592589)) ;
#26799 = CARTESIAN_POINT('Ctrl Pts',(-11.3240513924708,15.7867960512071,-323.61951556186)) ;
#26800 = CARTESIAN_POINT('Ctrl Pts',(-11.033170284997,15.9914421550908,-323.624073979175)) ;
#26801 = CARTESIAN_POINT('Ctrl Pts',(-10.2880324070921,16.485661935317,-323.63558847017)) ;
#26802 = CARTESIAN_POINT('Ctrl Pts',(-9.82704166035124,16.7645433664448,-323.642561898039)) ;
#26803 = CARTESIAN_POINT('Ctrl Pts',(-9.21806634349993,17.0991904042027,-323.651429917981)) ;
#26804 = CARTESIAN_POINT('Ctrl Pts',(-9.08016877566304,17.1728155720452,-323.653416670403)) ;
#26805 = CARTESIAN_POINT('Ctrl Pts',(-8.73985357585639,17.3492687095376,-323.658264184836)) ;
#26806 = CARTESIAN_POINT('Ctrl Pts',(-8.53649293002245,17.4502279070833,-323.66111326938)) ;
#26807 = CARTESIAN_POINT('Ctrl Pts',(-8.20941454368964,17.605521164429,-323.665617375329)) ;
#26808 = CARTESIAN_POINT('Ctrl Pts',(-8.08681909811009,17.6621691633769,-323.667288443016)) ;
#26809 = CARTESIAN_POINT('Ctrl Pts',(-7.84832005389831,17.7693692500818,-323.6705065373)) ;
#26810 = CARTESIAN_POINT('Ctrl Pts',(-7.73249386650602,17.820077156609,-323.672054605962)) ;
#26811 = CARTESIAN_POINT('Ctrl Pts',(-7.45312609622506,17.9391458215196,-323.675754098106)) ;
#26812 = CARTESIAN_POINT('Ctrl Pts',(-7.2891277173627,18.0064060450117,-323.677897764949)) ;
#26813 = CARTESIAN_POINT('Ctrl Pts',(-6.43491789120533,18.343158289268,-323.688929736911)) ;
#26814 = CARTESIAN_POINT('Ctrl Pts',(-5.73061961604093,18.5752422166151,-323.697551008809)) ;
#26815 = CARTESIAN_POINT('Ctrl Pts',(-4.62345263128522,18.8710993944514,-323.710948207612)) ;
#26816 = CARTESIAN_POINT('Ctrl Pts',(-4.22893946590713,18.9634062371226,-323.715698412016)) ;
#26817 = CARTESIAN_POINT('Ctrl Pts',(-3.7149116230149,19.0668371837529,-323.721986168133)) ;
#26818 = CARTESIAN_POINT('Ctrl Pts',(-3.59777842990869,19.0892859705462,-323.723425706394)) ;
#26819 = CARTESIAN_POINT('Ctrl Pts',(-3.41154072054601,19.1232037154467,-323.725729874141)) ;
#26820 = CARTESIAN_POINT('Ctrl Pts',(-3.3425679997651,19.135380048266,-323.726586552559)) ;
#26821 = CARTESIAN_POINT('Ctrl Pts',(-3.21169119646415,19.1577556251621,-323.728219609246)) ;
#26822 = CARTESIAN_POINT('Ctrl Pts',(-3.14980061866052,19.1680285106877,-323.728995005584)) ;
#26823 = CARTESIAN_POINT('Ctrl Pts',(-2.97253816018169,19.1965696445581,-323.731223710988)) ;
#26824 = CARTESIAN_POINT('Ctrl Pts',(-2.85704988817862,19.214097301432,-323.732685252504)) ;
#26825 = CARTESIAN_POINT('Ctrl Pts',(-2.08286541049713,19.3244609707748,-323.742530722904)) ;
#26826 = CARTESIAN_POINT('Ctrl Pts',(-1.41993272885781,19.38445024856,-323.75117690688)) ;
#26827 = CARTESIAN_POINT('Ctrl Pts',(-0.41326624759806,19.4236184554067,-323.764148208138)) ;
#26828 = CARTESIAN_POINT('Ctrl Pts',(-0.0710077632526839,19.4278846366049,
-323.768534071267)) ;
#26829 = CARTESIAN_POINT('Ctrl Pts',(0.522687238255438,19.419595486858,-323.776062670934)) ;
#26830 = CARTESIAN_POINT('Ctrl Pts',(0.774098068005405,19.4111994314001,-323.779226415267)) ;
#26831 = CARTESIAN_POINT('Ctrl Pts',(1.16445555781883,19.3905671281626,-323.784095932084)) ;
#26832 = CARTESIAN_POINT('Ctrl Pts',(1.30355284956452,19.3817130391547,-323.78582273479)) ;
#26833 = CARTESIAN_POINT('Ctrl Pts',(1.56721041596976,19.362079038365,-323.789080152039)) ;
#26834 = CARTESIAN_POINT('Ctrl Pts',(1.69178548551039,19.3515920558029,-323.79061257634)) ;
#26835 = CARTESIAN_POINT('Ctrl Pts',(1.97923801521736,19.3245967881544,-323.794134017637)) ;
#26836 = CARTESIAN_POINT('Ctrl Pts',(2.14202542972823,19.3072305446627,-323.796117388452)) ;
#26837 = CARTESIAN_POINT('Ctrl Pts',(2.73838514779966,19.2359754257731,-323.803349105952)) ;
#26838 = CARTESIAN_POINT('Ctrl Pts',(3.17032460713276,19.1695213001071,-323.808517517856)) ;
#26839 = CARTESIAN_POINT('Ctrl Pts',(4.12898455655346,18.9887404643677,-323.819962149067)) ;
#26840 = CARTESIAN_POINT('Ctrl Pts',(4.65393141807666,18.8669472566369,-323.82620882754)) ;
#26841 = CARTESIAN_POINT('Ctrl Pts',(5.29639084717439,18.6894414181096,-323.834065921175)) ;
#26842 = CARTESIAN_POINT('Ctrl Pts',(5.41930664523481,18.6541708999714,-323.835579298324)) ;
#26843 = CARTESIAN_POINT('Ctrl Pts',(5.69752939147568,18.5713532688025,-323.839035396755)) ;
#26844 = CARTESIAN_POINT('Ctrl Pts',(5.85260623832162,18.5230667946202,-323.840983513214)) ;
#26845 = CARTESIAN_POINT('Ctrl Pts',(6.0813938881543,18.4486688776541,-323.84390071498)) ;
#26846 = CARTESIAN_POINT('Ctrl Pts',(6.15558211518285,18.4240479749458,-323.844853444417)) ;
#26847 = CARTESIAN_POINT('Ctrl Pts',(6.29284282748865,18.3775735491629,-323.846630343352)) ;
#26848 = CARTESIAN_POINT('Ctrl Pts',(6.35595505133229,18.3558414613773,-323.847453096178)) ;
#26849 = CARTESIAN_POINT('Ctrl Pts',(6.51380439161475,18.3005758589561,-323.849524529215)) ;
#26850 = CARTESIAN_POINT('Ctrl Pts',(6.60839560648056,18.2666316514541,-323.850778092066)) ;
#26851 = CARTESIAN_POINT('Ctrl Pts',(7.04447919596128,18.1063117196939,-323.85660706349)) ;
#26852 = CARTESIAN_POINT('Ctrl Pts',(7.38263851109961,17.9710839668721,-323.861267609204)) ;
#26853 = CARTESIAN_POINT('Ctrl Pts',(8.22600338520252,17.6060039231026,-323.873094471585)) ;
#26854 = CARTESIAN_POINT('Ctrl Pts',(8.72553351070651,17.3638582330167,-323.880283893682)) ;
#26855 = CARTESIAN_POINT('Ctrl Pts',(9.35374781505606,17.0253699520917,-323.889394129695)) ;
#26856 = CARTESIAN_POINT('Ctrl Pts',(9.49255657955187,16.9483683537343,-323.891412233581)) ;
#26857 = CARTESIAN_POINT('Ctrl Pts',(9.8296202460706,16.7559485142312,-323.896321544975)) ;
#26858 = CARTESIAN_POINT('Ctrl Pts',(10.0268045249737,16.6387029569601,-323.899200977598)) ;
#26859 = CARTESIAN_POINT('Ctrl Pts',(10.3370635211211,16.4467046892308,-323.90374044758)) ;
#26860 = CARTESIAN_POINT('Ctrl Pts',(10.451512022963,16.3742136870409,-323.905416988784)) ;
#26861 = CARTESIAN_POINT('Ctrl Pts',(10.6711397595513,16.2318619219588,-323.908638443262)) ;
#26862 = CARTESIAN_POINT('Ctrl Pts',(10.7764146434824,16.1621611395826,-323.910184478566)) ;
#26863 = CARTESIAN_POINT('Ctrl Pts',(11.0268075031128,15.992845930002,-323.913867177838)) ;
#26864 = CARTESIAN_POINT('Ctrl Pts',(11.1712657574136,15.8922756756911,-323.915996277857)) ;
#26865 = CARTESIAN_POINT('Ctrl Pts',(11.9232446476411,15.3534362615982,-323.927113703577)) ;
#26866 = CARTESIAN_POINT('Ctrl Pts',(12.5064039418228,14.8822588539162,-323.935827359411)) ;
#26867 = CARTESIAN_POINT('Ctrl Pts',(13.2795314224237,14.179982956458,-323.948038726717)) ;
#26868 = CARTESIAN_POINT('Ctrl Pts',(13.4936125245616,13.9764191427277,-323.951501221385)) ;
#26869 = CARTESIAN_POINT('Ctrl Pts',(13.7956691979493,13.6757903738945,-323.956560046464)) ;
#26870 = CARTESIAN_POINT('Ctrl Pts',(13.8874361360587,13.5825935841234,-323.958121153379)) ;
#26871 = CARTESIAN_POINT('Ctrl Pts',(14.0514941146829,13.4125785278567,-323.96096289631)) ;
#26872 = CARTESIAN_POINT('Ctrl Pts',(14.1241140162456,13.3360846140068,-323.962239289385)) ;
#26873 = CARTESIAN_POINT('Ctrl Pts',(14.2421887244028,13.2096647617785,-323.964348603576)) ;
#26874 = CARTESIAN_POINT('Ctrl Pts',(14.2880126852939,13.1600864851035,-323.965175811265)) ;
#26875 = CARTESIAN_POINT('Ctrl Pts',(14.3848666498527,13.0541951678067,-323.966943576037)) ;
#26876 = CARTESIAN_POINT('Ctrl Pts',(14.4358264469138,12.9978196167208,-323.967885132581)) ;
#26877 = CARTESIAN_POINT('Ctrl Pts',(14.5864912996801,12.8291638130494,-323.970701156253)) ;
#26878 = CARTESIAN_POINT('Ctrl Pts',(14.6852265873954,12.7160250290335,-323.972589169031)) ;
#26879 = CARTESIAN_POINT('Ctrl Pts',(15.1732287810414,12.1435681074222,-323.982112541924)) ;
#26880 = CARTESIAN_POINT('Ctrl Pts',(15.5423042402199,11.6674717484546,-323.989928289688)) ;
#26881 = CARTESIAN_POINT('Ctrl Pts',(16.1220994874027,10.8431163544081,-324.002906787567)) ;
#26882 = CARTESIAN_POINT('Ctrl Pts',(16.3450717740052,10.5039941954433,-324.008103154881)) ;
#26883 = CARTESIAN_POINT('Ctrl Pts',(16.6718083210111,9.97142986490923,-324.015996500905)) ;
#26884 = CARTESIAN_POINT('Ctrl Pts',(16.783190469953,9.78279735743369,-324.018743251148)) ;
#26885 = CARTESIAN_POINT('Ctrl Pts',(16.9573374918235,9.47613750782843,-324.023127980214)) ;
#26886 = CARTESIAN_POINT('Ctrl Pts',(17.0221158998602,9.35927599917526,-324.024780498107)) ;
#26887 = CARTESIAN_POINT('Ctrl Pts',(17.145491023379,9.13118639641089,-324.027970614032)) ;
#26888 = CARTESIAN_POINT('Ctrl Pts',(17.2042238226143,9.02003936511063,-324.029509155398)) ;
#26889 = CARTESIAN_POINT('Ctrl Pts',(17.3315178345717,8.77337886275919,-324.032889319376)) ;
#26890 = CARTESIAN_POINT('Ctrl Pts',(17.399577133164,8.6376155729785,-324.034727267962)) ;
#26891 = CARTESIAN_POINT('Ctrl Pts',(17.819715586545,7.77441180646962,-324.046279914371)) ;
#26892 = CARTESIAN_POINT('Ctrl Pts',(18.127700411271,7.02639447393589,-324.055659154228)) ;
#26893 = CARTESIAN_POINT('Ctrl Pts',(18.4750496852388,6.00631038139689,-324.068270333796)) ;
#26894 = CARTESIAN_POINT('Ctrl Pts',(18.556584792282,5.74946830278234,-324.071434887027)) ;
#26895 = CARTESIAN_POINT('Ctrl Pts',(18.6821350400666,5.32343651612519,-324.076714048854)) ;
#26896 = CARTESIAN_POINT('Ctrl Pts',(18.7292565434663,5.15520078681904,-324.078806455304)) ;
#26897 = CARTESIAN_POINT('Ctrl Pts',(18.794695643267,4.90881621843598,-324.081895175818)) ;
#26898 = CARTESIAN_POINT('Ctrl Pts',(18.8148085691335,4.83115301708702,-324.0828722933)) ;
#26899 = CARTESIAN_POINT('Ctrl Pts',(18.8506528809163,4.68912580615298,-324.084667315452)) ;
#26900 = CARTESIAN_POINT('Ctrl Pts',(18.8665371296415,4.62480178668731,-324.085483453268)) ;
#26901 = CARTESIAN_POINT('Ctrl Pts',(18.9047823430172,4.46644945151271,-324.087499872155)) ;
#26902 = CARTESIAN_POINT('Ctrl Pts',(18.9267712161514,4.37233317980457,-324.088704447505)) ;
#26903 = CARTESIAN_POINT('Ctrl Pts',(19.0129342588639,3.99070612638146,-324.093608070745)) ;
#26904 = CARTESIAN_POINT('Ctrl Pts',(19.0712666876844,3.70191718677557,-324.09736235941)) ;
#26905 = CARTESIAN_POINT('Ctrl Pts',(19.1571413140811,3.22060930498687,-324.103635621354)) ;
#26906 = CARTESIAN_POINT('Ctrl Pts',(19.1884011865441,3.0288029762415,-324.106139960428)) ;
#26907 = CARTESIAN_POINT('Ctrl Pts',(19.2860810594539,2.3670534054374,-324.114768260717)) ;
#26908 = CARTESIAN_POINT('Ctrl Pts',(19.3381545187024,1.89516375334783,-324.120896549801)) ;
#26909 = CARTESIAN_POINT('Ctrl Pts',(19.3835718623038,1.27634272530671,-324.128802861905)) ;
#26910 = CARTESIAN_POINT('Ctrl Pts',(19.3926110283401,1.13072828685348,-324.13065431783)) ;
#26911 = CARTESIAN_POINT('Ctrl Pts',(19.4109922510037,0.768711476549691,-324.135232277737)) ;
#26912 = CARTESIAN_POINT('Ctrl Pts',(19.4183568186144,0.552228398323954,-324.137947574658)) ;
#26913 = CARTESIAN_POINT('Ctrl Pts',(19.4244007697893,0.20251831684377,-324.142295582733)) ;
#26914 = CARTESIAN_POINT('Ctrl Pts',(19.4253326789454,0.0693491450277581,
-324.143942380656)) ;
#26915 = CARTESIAN_POINT('Ctrl Pts',(19.4244813800595,-0.189764089123379,
-324.147129549792)) ;
#26916 = CARTESIAN_POINT('Ctrl Pts',(19.4228427253298,-0.31570208922855,-324.148670775783)) ;
#26917 = CARTESIAN_POINT('Ctrl Pts',(19.4158360611705,-0.623819279378259,
-324.15242332307)) ;
#26918 = CARTESIAN_POINT('Ctrl Pts',(19.4091286623342,-0.805956048857765,
-324.154625942019)) ;
#26919 = CARTESIAN_POINT('Ctrl Pts',(19.3810162464742,-1.35797283713606,-324.161261337898)) ;
#26920 = CARTESIAN_POINT('Ctrl Pts',(19.3515919324436,-1.72735966439392,-324.165645236293)) ;
#26921 = CARTESIAN_POINT('Ctrl Pts',(19.2512512259567,-2.65199640169618,-324.176567253709)) ;
#26922 = CARTESIAN_POINT('Ctrl Pts',(19.1668694517215,-3.20544419908358,-324.183053050338)) ;
#26923 = CARTESIAN_POINT('Ctrl Pts',(19.0335344359576,-3.88228826772713,-324.191182299165)) ;
#26924 = CARTESIAN_POINT('Ctrl Pts',(19.0070706603997,-4.00984540605621,-324.192723510309)) ;
#26925 = CARTESIAN_POINT('Ctrl Pts',(18.9443021007148,-4.29780008340211,-324.196231347359)) ;
#26926 = CARTESIAN_POINT('Ctrl Pts',(18.9072395071955,-4.45802217470933,-324.198203341717)) ;
#26927 = CARTESIAN_POINT('Ctrl Pts',(18.849482261209,-4.69401833178835,-324.201149008251)) ;
#26928 = CARTESIAN_POINT('Ctrl Pts',(18.8303552874522,-4.77016869120389,-324.202105868501)) ;
#26929 = CARTESIAN_POINT('Ctrl Pts',(18.7941388073036,-4.91074473973838,-324.203885661795)) ;
#26930 = CARTESIAN_POINT('Ctrl Pts',(18.7771784120087,-4.9752023330357,-324.204707117914)) ;
#26931 = CARTESIAN_POINT('Ctrl Pts',(18.7339968130889,-5.1359465412719,-324.206768397711)) ;
#26932 = CARTESIAN_POINT('Ctrl Pts',(18.7073647501064,-5.23212074926365,-324.208012996101)) ;
#26933 = CARTESIAN_POINT('Ctrl Pts',(18.5851013659566,-5.66076987653046,-324.213604220541)) ;
#26934 = CARTESIAN_POINT('Ctrl Pts',(18.4813394813232,-5.99085958224712,-324.21802752766)) ;
#26935 = CARTESIAN_POINT('Ctrl Pts',(18.1530169867385,-6.94541723367151,-324.231010153445)) ;
#26936 = CARTESIAN_POINT('Ctrl Pts',(17.9052108432216,-7.56136729532687,-324.239617472846)) ;
#26937 = CARTESIAN_POINT('Ctrl Pts',(17.5125146059858,-8.40927233045729,-324.251488432656)) ;
#26938 = CARTESIAN_POINT('Ctrl Pts',(17.3935235064486,-8.65270879152121,-324.254901801307)) ;
#26939 = CARTESIAN_POINT('Ctrl Pts',(17.2041666955727,-9.02040039306527,-324.260058709053)) ;
#26940 = CARTESIAN_POINT('Ctrl Pts',(17.1374589745752,-9.14650069182183,-324.261827616468)) ;
#26941 = CARTESIAN_POINT('Ctrl Pts',(17.0099864066733,-9.38117608735243,-324.265120334795)) ;
#26942 = CARTESIAN_POINT('Ctrl Pts',(16.9495556620643,-9.48992440657347,-324.266646487876)) ;
#26943 = CARTESIAN_POINT('Ctrl Pts',(16.8100068467778,-9.73546424320192,-324.270093818968)) ;
#26944 = CARTESIAN_POINT('Ctrl Pts',(16.730255858124,-9.87188600178964,-324.272010182737)) ;
#26945 = CARTESIAN_POINT('Ctrl Pts',(16.4578490221333,-10.3250803138368,-324.278384292262)) ;
#26946 = CARTESIAN_POINT('Ctrl Pts',(16.2577906060784,-10.6373080887085,-324.282787409926)) ;
#26947 = CARTESIAN_POINT('Ctrl Pts',(15.9478116237152,-11.0918951451245,-324.289264240264)) ;
#26948 = CARTESIAN_POINT('Ctrl Pts',(15.8446536467219,-11.2387625815284,-324.291367731757)) ;
#26949 = CARTESIAN_POINT('Ctrl Pts',(15.468094697273,-11.7593833529207,-324.298883542137)) ;
#26950 = CARTESIAN_POINT('Ctrl Pts',(15.1833848718419,-12.124762808691,-324.304266229413)) ;
#26951 = CARTESIAN_POINT('Ctrl Pts',(14.7794880161957,-12.6065375627144,-324.311688107612)) ;
#26952 = CARTESIAN_POINT('Ctrl Pts',(14.6714657692087,-12.7320912425245,-324.31365422033)) ;
#26953 = CARTESIAN_POINT('Ctrl Pts',(14.4789375459549,-12.9501616596825,-324.317138572761)) ;
#26954 = CARTESIAN_POINT('Ctrl Pts',(14.3951173055137,-13.0432709532823,-324.318649183161)) ;
#26955 = CARTESIAN_POINT('Ctrl Pts',(14.2622324450179,-13.1880409837315,-324.321039527313)) ;
#26956 = CARTESIAN_POINT('Ctrl Pts',(14.2137742598569,-13.2402537958351,-324.321910281528)) ;
#26957 = CARTESIAN_POINT('Ctrl Pts',(14.1226895817937,-13.337319542058,-324.32354652899)) ;
#26958 = CARTESIAN_POINT('Ctrl Pts',(14.0801338407855,-13.3822376530489,-324.324310825099)) ;
#26959 = CARTESIAN_POINT('Ctrl Pts',(13.9600900650932,-13.5077388280364,-324.326465270509)) ;
#26960 = CARTESIAN_POINT('Ctrl Pts',(13.8821199813453,-13.587857360246,-324.327862836662)) ;
#26961 = CARTESIAN_POINT('Ctrl Pts',(13.3198593051154,-14.1557197237068,-324.337913664347)) ;
#26962 = CARTESIAN_POINT('Ctrl Pts',(12.81067339067,-14.618129177171,-324.346853736898)) ;
#26963 = CARTESIAN_POINT('Ctrl Pts',(12.0183225785821,-15.2644322009246,-324.360015005856)) ;
#26964 = CARTESIAN_POINT('Ctrl Pts',(11.7531520033427,-15.4695309119914,-324.364308383037)) ;
#26965 = CARTESIAN_POINT('Ctrl Pts',(11.3881690686964,-15.7370263250289,-324.370044077578)) ;
#26966 = CARTESIAN_POINT('Ctrl Pts',(11.2929040829425,-15.8055278209848,-324.371525822738)) ;
#26967 = CARTESIAN_POINT('Ctrl Pts',(11.0448875511486,-15.9804801788329,-324.375342920027)) ;
#26968 = CARTESIAN_POINT('Ctrl Pts',(10.8912156756376,-16.0856056467634,-324.377668735046)) ;
#26969 = CARTESIAN_POINT('Ctrl Pts',(10.6295171300252,-16.2591615213897,-324.381562964749)) ;
#26970 = CARTESIAN_POINT('Ctrl Pts',(10.5222830843481,-16.3287637786815,-324.383140271606)) ;
#26971 = CARTESIAN_POINT('Ctrl Pts',(10.3158913591436,-16.4598487383366,-324.386141494111)) ;
#26972 = CARTESIAN_POINT('Ctrl Pts',(10.2168514799252,-16.5215066170698,-324.387566706128)) ;
#26973 = CARTESIAN_POINT('Ctrl Pts',(9.94955033317331,-16.6845938176103,-324.391374301421)) ;
#26974 = CARTESIAN_POINT('Ctrl Pts',(9.78029569111016,-16.7843688905172,-324.393744250283)) ;
#26975 = CARTESIAN_POINT('Ctrl Pts',(9.26246603281474,-17.0791351057108,-324.400881323137)) ;
#26976 = CARTESIAN_POINT('Ctrl Pts',(8.90936440882511,-17.2659595630313,-324.405592601799)) ;
#26977 = CARTESIAN_POINT('Ctrl Pts',(8.09026389142239,-17.6675202552011,-324.416282278911)) ;
#26978 = CARTESIAN_POINT('Ctrl Pts',(7.62101385343965,-17.8749486244568,-324.422234049938)) ;
#26979 = CARTESIAN_POINT('Ctrl Pts',(6.98270746560611,-18.1273976659743,-324.430329249737)) ;
#26980 = CARTESIAN_POINT('Ctrl Pts',(6.82045926039131,-18.1890649852683,-324.432387472011)) ;
#26981 = CARTESIAN_POINT('Ctrl Pts',(6.53570661518215,-18.2929479900004,-324.436015219369)) ;
#26982 = CARTESIAN_POINT('Ctrl Pts',(6.41356558710243,-18.3361278220489,-324.437576227114)) ;
#26983 = CARTESIAN_POINT('Ctrl Pts',(6.22280664554407,-18.4014265205564,-324.440027704807)) ;
#26984 = CARTESIAN_POINT('Ctrl Pts',(6.15448198543807,-18.4243906822909,-324.440908439457)) ;
#26985 = CARTESIAN_POINT('Ctrl Pts',(6.02773974167217,-18.4662055210767,-324.44254842077)) ;
#26986 = CARTESIAN_POINT('Ctrl Pts',(5.96935757792709,-18.4851606113572,-324.44330632624)) ;
#26987 = CARTESIAN_POINT('Ctrl Pts',(5.807253738359,-18.5369432406899,-324.445416578835)) ;
#26988 = CARTESIAN_POINT('Ctrl Pts',(5.70334466969332,-18.5691766166284,-324.446775865346)) ;
#26989 = CARTESIAN_POINT('Ctrl Pts',(5.37440883403443,-18.6681935412559,-324.451093619567)) ;
#26990 = CARTESIAN_POINT('Ctrl Pts',(5.14843963413857,-18.7317721913582,-324.454081327165)) ;
#26991 = CARTESIAN_POINT('Ctrl Pts',(4.30396942894941,-18.9529366247887,-324.465262939739)) ;
#26992 = CARTESIAN_POINT('Ctrl Pts',(3.67897035963435,-19.0841069828959,-324.473557659298)) ;
#26993 = CARTESIAN_POINT('Ctrl Pts',(2.70140624977385,-19.2394556179909,-324.48621266116)) ;
#26994 = CARTESIAN_POINT('Ctrl Pts',(2.35272785827551,-19.2851995261928,-324.490667728301)) ;
#26995 = CARTESIAN_POINT('Ctrl Pts',(1.84945245054677,-19.3373726449075,-324.496994520506)) ;
#26996 = CARTESIAN_POINT('Ctrl Pts',(1.69572065494551,-19.3514595502254,-324.498913515799)) ;
#26997 = CARTESIAN_POINT('Ctrl Pts',(1.43018252699412,-19.3726030450014,-324.502204605072)) ;
#26998 = CARTESIAN_POINT('Ctrl Pts',(1.31845301135227,-19.380527662859,-324.503582218661)) ;
#26999 = CARTESIAN_POINT('Ctrl Pts',(1.06468201517957,-19.3963221607867,-324.506695370624)) ;
#27000 = CARTESIAN_POINT('Ctrl Pts',(0.922610002033545,-19.403598944801,-324.508426999435)) ;
#27001 = CARTESIAN_POINT('Ctrl Pts',(0.520324503775809,-19.419775305685,-324.513300715947)) ;
#27002 = CARTESIAN_POINT('Ctrl Pts',(0.259993944107991,-19.4250048653043,
-324.516419438809)) ;
#27003 = CARTESIAN_POINT('Ctrl Pts',(-0.000363249083133038,-19.4249999966036,
-324.51951242736)) ;
#27004 = CARTESIAN_POINT('Origin',(0.,0.,-328.125)) ;
#27005 = CARTESIAN_POINT('',(0.000472547777405694,-19.4249999942522,-326.231461493639)) ;
#27006 = CARTESIAN_POINT('',(0.000483615249731608,-19.4249999937201,-326.018849107561)) ;
#27007 = CARTESIAN_POINT('',(-2.37887640734373E-15,-19.425,-328.125)) ;
#27008 = CARTESIAN_POINT('Ctrl Pts',(0.000472547765765496,-19.4249999942522,
-326.231461493639)) ;
#27009 = CARTESIAN_POINT('Ctrl Pts',(0.396084841908866,-19.4249903702777,
-326.226835776913)) ;
#27010 = CARTESIAN_POINT('Ctrl Pts',(0.791603743676953,-19.4128951015776,
-326.222193988934)) ;
#27011 = CARTESIAN_POINT('Ctrl Pts',(1.30529304516484,-19.3814603553559,-326.216022043007)) ;
#27012 = CARTESIAN_POINT('Ctrl Pts',(1.42404097536059,-19.3730973950539,-326.214585139653)) ;
#27013 = CARTESIAN_POINT('Ctrl Pts',(1.60563597321444,-19.3586296944345,-326.212367709118)) ;
#27014 = CARTESIAN_POINT('Ctrl Pts',(1.66854271952288,-19.3533091668245,-326.211595873353)) ;
#27015 = CARTESIAN_POINT('Ctrl Pts',(1.80073618527897,-19.3414791852382,-326.209965196664)) ;
#27016 = CARTESIAN_POINT('Ctrl Pts',(1.87001606900058,-19.3349038723957,-326.209105486689)) ;
#27017 = CARTESIAN_POINT('Ctrl Pts',(2.05563583516961,-19.3162798234963,-326.206789770731)) ;
#27018 = CARTESIAN_POINT('Ctrl Pts',(2.17190470149032,-19.303552388465,-326.205326281727)) ;
#27019 = CARTESIAN_POINT('Ctrl Pts',(2.36736283260079,-19.2803681766676,-326.202848152535)) ;
#27020 = CARTESIAN_POINT('Ctrl Pts',(2.44661547478579,-19.270471621426,-326.201838380587)) ;
#27021 = CARTESIAN_POINT('Ctrl Pts',(2.65612601446928,-19.2429960065884,-326.199157691651)) ;
#27022 = CARTESIAN_POINT('Ctrl Pts',(2.7862703524327,-19.2245831732981,-326.197480955458)) ;
#27023 = CARTESIAN_POINT('Ctrl Pts',(3.47989406675427,-19.1192578192112,-326.188498333768)) ;
#27024 = CARTESIAN_POINT('Ctrl Pts',(4.03952898542165,-19.0088897385276,-326.18109671263)) ;
#27025 = CARTESIAN_POINT('Ctrl Pts',(4.89285894758898,-18.8012095801006,-326.169831073617)) ;
#27026 = CARTESIAN_POINT('Ctrl Pts',(5.19044480333996,-18.7212401741557,-326.165904310168)) ;
#27027 = CARTESIAN_POINT('Ctrl Pts',(5.68339826004158,-18.5761123874569,-326.159423465814)) ;
#27028 = CARTESIAN_POINT('Ctrl Pts',(5.87985801859845,-18.5148653005826,-326.156846833119)) ;
#27029 = CARTESIAN_POINT('Ctrl Pts',(6.19995025965793,-18.4094666395598,-326.152660754872)) ;
#27030 = CARTESIAN_POINT('Ctrl Pts',(6.32417374400339,-18.3671628643641,-326.151039156393)) ;
#27031 = CARTESIAN_POINT('Ctrl Pts',(6.56937795113919,-18.2808770692902,-326.147843866928)) ;
#27032 = CARTESIAN_POINT('Ctrl Pts',(6.69036918367765,-18.2369447365749,-326.14626993091)) ;
#27033 = CARTESIAN_POINT('Ctrl Pts',(6.99019521860138,-18.1246915156906,-326.142375203866)) ;
#27034 = CARTESIAN_POINT('Ctrl Pts',(7.16847366040169,-18.0549233526264,-326.140064455599)) ;
#27035 = CARTESIAN_POINT('Ctrl Pts',(7.55793724072128,-17.8958312096743,-326.13502141511)) ;
#27036 = CARTESIAN_POINT('Ctrl Pts',(7.76863118091874,-17.8053800803884,-326.132296549346)) ;
#27037 = CARTESIAN_POINT('Ctrl Pts',(8.47703854575547,-17.4862917638369,-326.123119856379)) ;
#27038 = CARTESIAN_POINT('Ctrl Pts',(8.96666650135865,-17.2403443607228,-326.116758422149)) ;
#27039 = CARTESIAN_POINT('Ctrl Pts',(9.77294345290514,-16.7916895589981,-326.105953059719)) ;
#27040 = CARTESIAN_POINT('Ctrl Pts',(10.0952915702622,-16.5998900229452,-326.101537009417)) ;
#27041 = CARTESIAN_POINT('Ctrl Pts',(10.4963999569461,-16.3452205632584,-326.095814785557)) ;
#27042 = CARTESIAN_POINT('Ctrl Pts',(10.5804994655467,-16.2909078426628,-326.094601904215)) ;
#27043 = CARTESIAN_POINT('Ctrl Pts',(10.7199208244748,-16.199332416763,-326.092566255682)) ;
#27044 = CARTESIAN_POINT('Ctrl Pts',(10.775477402656,-16.1624305098516,-326.091748366406)) ;
#27045 = CARTESIAN_POINT('Ctrl Pts',(10.895887921769,-16.0815543700598,-326.089960233181)) ;
#27046 = CARTESIAN_POINT('Ctrl Pts',(10.9606679288801,-16.0374724658583,-326.088988573305)) ;
#27047 = CARTESIAN_POINT('Ctrl Pts',(11.1598032586344,-15.9001934843546,-326.085974014216)) ;
#27048 = CARTESIAN_POINT('Ctrl Pts',(11.2932497849952,-15.8056910877373,-326.083914737489)) ;
#27049 = CARTESIAN_POINT('Ctrl Pts',(11.5299474163125,-15.6335415553318,-326.080202611092)) ;
#27050 = CARTESIAN_POINT('Ctrl Pts',(11.6336473610395,-15.5565278264689,-326.078555329287)) ;
#27051 = CARTESIAN_POINT('Ctrl Pts',(12.1746904051219,-15.1462816011811,-326.069864348592)) ;
#27052 = CARTESIAN_POINT('Ctrl Pts',(12.5985073981272,-14.7956258755794,-326.062729072707)) ;
#27053 = CARTESIAN_POINT('Ctrl Pts',(13.3244840162353,-14.1411318903667,-326.050178730053)) ;
#27054 = CARTESIAN_POINT('Ctrl Pts',(13.6325491130252,-13.844388457096,-326.044735417857)) ;
#27055 = CARTESIAN_POINT('Ctrl Pts',(14.0433691453359,-13.4216468675579,-326.03735055532)) ;
#27056 = CARTESIAN_POINT('Ctrl Pts',(14.1547135357055,-13.3041687607106,-326.03533511821)) ;
#27057 = CARTESIAN_POINT('Ctrl Pts',(14.349286739696,-13.093669057971,-326.031788505995)) ;
#27058 = CARTESIAN_POINT('Ctrl Pts',(14.4331115795398,-13.0012110788826,-326.030252171891)) ;
#27059 = CARTESIAN_POINT('Ctrl Pts',(14.6093078536236,-12.8030640630554,-326.027004305764)) ;
#27060 = CARTESIAN_POINT('Ctrl Pts',(14.7014365272681,-12.697168560939,-326.025294917591)) ;
#27061 = CARTESIAN_POINT('Ctrl Pts',(14.9591472116259,-12.3943825371397,-326.020479082189)) ;
#27062 = CARTESIAN_POINT('Ctrl Pts',(15.1219770626562,-12.1951881428237,-326.017395530525)) ;
#27063 = CARTESIAN_POINT('Ctrl Pts',(15.4996929057522,-11.7139166756847,-326.010122851828)) ;
#27064 = CARTESIAN_POINT('Ctrl Pts',(15.710906538774,-11.4290743394916,-326.005958671032)) ;
#27065 = CARTESIAN_POINT('Ctrl Pts',(16.2506144402162,-10.6579707793137,-325.994949217009)) ;
#27066 = CARTESIAN_POINT('Ctrl Pts',(16.565074473972,-10.1623380600414,-325.988145466328)) ;
#27067 = CARTESIAN_POINT('Ctrl Pts',(16.9312463594053,-9.52292352911861,-325.97935700466)) ;
#27068 = CARTESIAN_POINT('Ctrl Pts',(17.0043591495648,-9.39174880526528,-325.977552902012)) ;
#27069 = CARTESIAN_POINT('Ctrl Pts',(17.1121698836036,-9.19293436211056,-325.974808053192)) ;
#27070 = CARTESIAN_POINT('Ctrl Pts',(17.1480039276312,-9.12591702736912,-325.973881030145)) ;
#27071 = CARTESIAN_POINT('Ctrl Pts',(17.2149267948511,-8.99897094887938,-325.972120194062)) ;
#27072 = CARTESIAN_POINT('Ctrl Pts',(17.2460982151123,-8.93908714618695,-325.971287412036)) ;
#27073 = CARTESIAN_POINT('Ctrl Pts',(17.3251656313346,-8.78523672972515,-325.969143362188)) ;
#27074 = CARTESIAN_POINT('Ctrl Pts',(17.3726096636444,-8.6910403278129,-325.967826443599)) ;
#27075 = CARTESIAN_POINT('Ctrl Pts',(17.6397247722339,-8.14977651512699,-325.960245303503)) ;
#27076 = CARTESIAN_POINT('Ctrl Pts',(17.8429019095926,-7.6947772836951,-325.953823127078)) ;
#27077 = CARTESIAN_POINT('Ctrl Pts',(18.271838173851,-6.62556919956201,-325.938960369494)) ;
#27078 = CARTESIAN_POINT('Ctrl Pts',(18.4845107431424,-6.00675500020633,-325.930534180472)) ;
#27079 = CARTESIAN_POINT('Ctrl Pts',(18.7171504889706,-5.19938532732032,-325.91996710361)) ;
#27080 = CARTESIAN_POINT('Ctrl Pts',(18.7661536168004,-5.01964229726913,-325.917639830639)) ;
#27081 = CARTESIAN_POINT('Ctrl Pts',(18.844099693531,-4.7166255067859,-325.913759664277)) ;
#27082 = CARTESIAN_POINT('Ctrl Pts',(18.8744365109715,-4.59372353040788,-325.912197700383)) ;
#27083 = CARTESIAN_POINT('Ctrl Pts',(18.9339734996157,-4.34197246584523,-325.909021890631)) ;
#27084 = CARTESIAN_POINT('Ctrl Pts',(18.9630648768828,-4.21310430783586,-325.907408837553)) ;
#27085 = CARTESIAN_POINT('Ctrl Pts',(19.0351365151872,-3.87796280650687,-325.903245028846)) ;
#27086 = CARTESIAN_POINT('Ctrl Pts',(19.0760793072788,-3.67126901026545,-325.900707673654)) ;
#27087 = CARTESIAN_POINT('Ctrl Pts',(19.1386435201803,-3.32604734238882,-325.896513726673)) ;
#27088 = CARTESIAN_POINT('Ctrl Pts',(19.1621423368513,-3.1878782644296,-325.894846770509)) ;
#27089 = CARTESIAN_POINT('Ctrl Pts',(19.2536930146786,-2.61193452786711,-325.887939074793)) ;
#27090 = CARTESIAN_POINT('Ctrl Pts',(19.3082536480854,-2.17215058894986,-325.882765514894)) ;
#27091 = CARTESIAN_POINT('Ctrl Pts',(19.3533723314318,-1.66781714160012,-325.876851656223)) ;
#27092 = CARTESIAN_POINT('Ctrl Pts',(19.3587062438886,-1.60472028063411,-325.87611204624)) ;
#27093 = CARTESIAN_POINT('Ctrl Pts',(19.3723718487853,-1.43306916054423,-325.874099860656)) ;
#27094 = CARTESIAN_POINT('Ctrl Pts',(19.3800995802141,-1.32446914582103,-325.872826668675)) ;
#27095 = CARTESIAN_POINT('Ctrl Pts',(19.4092960029773,-0.85891238884552,-325.8673607595)) ;
#27096 = CARTESIAN_POINT('Ctrl Pts',(19.4218184782115,-0.501465522976049,
-325.863145504404)) ;
#27097 = CARTESIAN_POINT('Ctrl Pts',(19.425209268976,-0.0436874878296498,
-325.857632172223)) ;
#27098 = CARTESIAN_POINT('Ctrl Pts',(19.4251762054148,0.0565074280901048,
-325.856418319449)) ;
#27099 = CARTESIAN_POINT('Ctrl Pts',(19.4238298594906,0.223401737647895,-325.854381558668)) ;
#27100 = CARTESIAN_POINT('Ctrl Pts',(19.4229481584071,0.290102726359439,-325.853563541254)) ;
#27101 = CARTESIAN_POINT('Ctrl Pts',(19.4202844115637,0.435099498364049,-325.851775790253)) ;
#27102 = CARTESIAN_POINT('Ctrl Pts',(19.4183724160824,0.513391555499843,-325.850804647716)) ;
#27103 = CARTESIAN_POINT('Ctrl Pts',(19.4110137382568,0.754870814786239,-325.847793590315)) ;
#27104 = CARTESIAN_POINT('Ctrl Pts',(19.4039829861281,0.918002409764678,-325.845737350085)) ;
#27105 = CARTESIAN_POINT('Ctrl Pts',(19.3648500244098,1.62009465194668,-325.836818990162)) ;
#27106 = CARTESIAN_POINT('Ctrl Pts',(19.312342056374,2.1576763271493,-325.829822673471)) ;
#27107 = CARTESIAN_POINT('Ctrl Pts',(19.1617932126091,3.23337699561174,-325.815823072259)) ;
#27108 = CARTESIAN_POINT('Ctrl Pts',(19.0632889334125,3.77095004986145,-325.808827641273)) ;
#27109 = CARTESIAN_POINT('Ctrl Pts',(18.907937506103,4.45471909157949,-325.800029815056)) ;
#27110 = CARTESIAN_POINT('Ctrl Pts',(18.8718103689917,4.60536604461547,-325.798097191525)) ;
#27111 = CARTESIAN_POINT('Ctrl Pts',(18.8029470312267,4.87809162635995,-325.794609299792)) ;
#27112 = CARTESIAN_POINT('Ctrl Pts',(18.7708140035024,5.00031365710854,-325.793050178972)) ;
#27113 = CARTESIAN_POINT('Ctrl Pts',(18.7025662023517,5.24996989065656,-325.789873234782)) ;
#27114 = CARTESIAN_POINT('Ctrl Pts',(18.6663360928169,5.37736583577967,-325.788256275946)) ;
#27115 = CARTESIAN_POINT('Ctrl Pts',(18.5685715019384,5.70823636677896,-325.784066213437)) ;
#27116 = CARTESIAN_POINT('Ctrl Pts',(18.5049948939301,5.91108908958802,-325.781506853459)) ;
#27117 = CARTESIAN_POINT('Ctrl Pts',(18.3543613027813,6.36544245985224,-325.775786320851)) ;
#27118 = CARTESIAN_POINT('Ctrl Pts',(18.2654393628329,6.61628005150345,-325.772636693414)) ;
#27119 = CARTESIAN_POINT('Ctrl Pts',(18.0175211818165,7.27248974960846,-325.764384178665)) ;
#27120 = CARTESIAN_POINT('Ctrl Pts',(17.8500010577672,7.67447971423041,-325.759317554533)) ;
#27121 = CARTESIAN_POINT('Ctrl Pts',(17.6271365894711,8.16240710837583,-325.753041881376)) ;
#27122 = CARTESIAN_POINT('Ctrl Pts',(17.5844409502142,8.25398513474412,-325.75185826426)) ;
#27123 = CARTESIAN_POINT('Ctrl Pts',(17.4074493418963,8.62600809272875,-325.747020643377)) ;
#27124 = CARTESIAN_POINT('Ctrl Pts',(17.2671436068629,8.9035419401335,-325.743343976852)) ;
#27125 = CARTESIAN_POINT('Ctrl Pts',(17.0738027308345,9.26420771263443,-325.738413194164)) ;
#27126 = CARTESIAN_POINT('Ctrl Pts',(17.0267117592125,9.35047436581089,-325.737221999383)) ;
#27127 = CARTESIAN_POINT('Ctrl Pts',(16.946686515366,9.49446455000255,-325.735211040179)) ;
#27128 = CARTESIAN_POINT('Ctrl Pts',(16.914107029944,9.55238317534052,-325.734395871269)) ;
#27129 = CARTESIAN_POINT('Ctrl Pts',(16.8419967647843,9.67905259429694,-325.732598532699)) ;
#27130 = CARTESIAN_POINT('Ctrl Pts',(16.8023409570405,9.74773063283268,-325.731614785599)) ;
#27131 = CARTESIAN_POINT('Ctrl Pts',(16.6768041268439,9.96209968189783,-325.728517438262)) ;
#27132 = CARTESIAN_POINT('Ctrl Pts',(16.5894404450087,10.1069130560024,-325.726386204364)) ;
#27133 = CARTESIAN_POINT('Ctrl Pts',(16.2221460244764,10.6981418528673,-325.717551998203)) ;
#27134 = CARTESIAN_POINT('Ctrl Pts',(15.9259992493394,11.1342179038783,-325.710725819506)) ;
#27135 = CARTESIAN_POINT('Ctrl Pts',(15.2832966131833,12.0023991109174,-325.696802487383)) ;
#27136 = CARTESIAN_POINT('Ctrl Pts',(14.9352524282809,12.4328185922866,-325.689716562144)) ;
#27137 = CARTESIAN_POINT('Ctrl Pts',(14.4675281589715,12.9632147058041,-325.680845568925)) ;
#27138 = CARTESIAN_POINT('Ctrl Pts',(14.3643777437455,13.0774217130603,-325.678926059348)) ;
#27139 = CARTESIAN_POINT('Ctrl Pts',(14.1742228968212,13.2829945039999,-325.675454156428)) ;
#27140 = CARTESIAN_POINT('Ctrl Pts',(14.0876646352958,13.3747614144889,-325.67389803525)) ;
#27141 = CARTESIAN_POINT('Ctrl Pts',(13.9081467453182,13.5614055301608,-325.670719658124)) ;
#27142 = CARTESIAN_POINT('Ctrl Pts',(13.8150954490209,13.6561855447752,-325.669098345074)) ;
#27143 = CARTESIAN_POINT('Ctrl Pts',(13.5691389656526,13.9016246344569,-325.664879067421)) ;
#27144 = CARTESIAN_POINT('Ctrl Pts',(13.4146956986639,14.0507166817985,-325.662295232026)) ;
#27145 = CARTESIAN_POINT('Ctrl Pts',(13.1525768129787,14.2954916124292,-325.658010403642)) ;
#27146 = CARTESIAN_POINT('Ctrl Pts',(13.0462510346838,14.3925915406517,-325.656298880989)) ;
#27147 = CARTESIAN_POINT('Ctrl Pts',(12.5928614539457,14.7974879823851,-325.64910351462)) ;
#27148 = CARTESIAN_POINT('Ctrl Pts',(12.2359100273527,15.093982786436,-325.643692749335)) ;
#27149 = CARTESIAN_POINT('Ctrl Pts',(11.7488876920241,15.4698792771196,-325.636506148707)) ;
#27150 = CARTESIAN_POINT('Ctrl Pts',(11.6280110639731,15.5609410229762,-325.634737342497)) ;
#27151 = CARTESIAN_POINT('Ctrl Pts',(11.2273698264863,15.8554867178555,-325.628908145165)) ;
#27152 = CARTESIAN_POINT('Ctrl Pts',(10.9432335434142,16.0529103544129,-325.62482770151)) ;
#27153 = CARTESIAN_POINT('Ctrl Pts',(10.5700809031297,16.297671054631,-325.619453391335)) ;
#27154 = CARTESIAN_POINT('Ctrl Pts',(10.4857585903689,16.3520506007277,-325.618237862659)) ;
#27155 = CARTESIAN_POINT('Ctrl Pts',(10.3446639730459,16.4415025061108,-325.61619918184)) ;
#27156 = CARTESIAN_POINT('Ctrl Pts',(10.2881254175035,16.4769400307424,-325.615380942167)) ;
#27157 = CARTESIAN_POINT('Ctrl Pts',(10.1648936269429,16.553298307062,-325.61359384479)) ;
#27158 = CARTESIAN_POINT('Ctrl Pts',(10.0981336076106,16.5941087411156,-325.612623590125)) ;
#27159 = CARTESIAN_POINT('Ctrl Pts',(9.89165476917093,16.7186218925867,-325.609618534667)) ;
#27160 = CARTESIAN_POINT('Ctrl Pts',(9.75112850969913,16.8009715404932,-325.607567497704)) ;
#27161 = CARTESIAN_POINT('Ctrl Pts',(9.497987099999,16.9450687574504,-325.603873416864)) ;
#27162 = CARTESIAN_POINT('Ctrl Pts',(9.38576360586516,17.0074852824696,-325.602235946072)) ;
#27163 = CARTESIAN_POINT('Ctrl Pts',(8.79556612168375,17.3281208697744,-325.593639521415)) ;
#27164 = CARTESIAN_POINT('Ctrl Pts',(8.30753342520917,17.5673175379234,-325.586590346927)) ;
#27165 = CARTESIAN_POINT('Ctrl Pts',(7.42357290732393,17.9554843794327,-325.574190601969)) ;
#27166 = CARTESIAN_POINT('Ctrl Pts',(7.03159627399173,18.1125787616569,-325.568813203361)) ;
#27167 = CARTESIAN_POINT('Ctrl Pts',(6.4916775198293,18.3087940989341,-325.561609130395)) ;
#27168 = CARTESIAN_POINT('Ctrl Pts',(6.34793587494923,18.3591265748238,-325.55971002771)) ;
#27169 = CARTESIAN_POINT('Ctrl Pts',(6.08440513016666,18.4479393103549,-325.556262926084)) ;
#27170 = CARTESIAN_POINT('Ctrl Pts',(5.96480560268138,18.4869560706288,-325.554711392624)) ;
#27171 = CARTESIAN_POINT('Ctrl Pts',(5.71758288809553,18.5649582856223,-325.551530298572)) ;
#27172 = CARTESIAN_POINT('Ctrl Pts',(5.58991992884497,18.6037959963842,-325.549901806679)) ;
#27173 = CARTESIAN_POINT('Ctrl Pts',(5.25258801267257,18.7026335507579,-325.545634444311)) ;
#27174 = CARTESIAN_POINT('Ctrl Pts',(5.04229121569352,18.7604232916986,-325.543010345816)) ;
#27175 = CARTESIAN_POINT('Ctrl Pts',(4.68834397027207,18.8513068070034,-325.538646339078)) ;
#27176 = CARTESIAN_POINT('Ctrl Pts',(4.54520968921524,18.8863285593903,-325.536895765584)) ;
#27177 = CARTESIAN_POINT('Ctrl Pts',(3.93124955800609,19.0291669760619,-325.529438420388)) ;
#27178 = CARTESIAN_POINT('Ctrl Pts',(3.45688959178512,19.1210311832898,-325.523810351705)) ;
#27179 = CARTESIAN_POINT('Ctrl Pts',(2.84212074088501,19.2164598907093,-325.516540622699)) ;
#27180 = CARTESIAN_POINT('Ctrl Pts',(2.70441595484694,19.2363228128021,-325.514913420452)) ;
#27181 = CARTESIAN_POINT('Ctrl Pts',(2.23751401919986,19.2985573881291,-325.509387988822)) ;
#27182 = CARTESIAN_POINT('Ctrl Pts',(1.90744899709749,19.3339707156132,-325.50546887953)) ;
#27183 = CARTESIAN_POINT('Ctrl Pts',(1.4778991003224,19.368950763298,-325.500277049071)) ;
#27184 = CARTESIAN_POINT('Ctrl Pts',(1.37909821824477,19.3762361538079,-325.499076535612)) ;
#27185 = CARTESIAN_POINT('Ctrl Pts',(1.21383665341167,19.3871518028391,-325.497055001474)) ;
#27186 = CARTESIAN_POINT('Ctrl Pts',(1.14740522044847,19.391196861357,-325.49623869752)) ;
#27187 = CARTESIAN_POINT('Ctrl Pts',(1.00219016441312,19.3992902683791,-325.494445476449)) ;
#27188 = CARTESIAN_POINT('Ctrl Pts',(0.923400190141356,19.4032002543485,-325.49346705268)) ;
#27189 = CARTESIAN_POINT('Ctrl Pts',(0.678114941577363,19.4138752214988,-325.490406399665)) ;
#27190 = CARTESIAN_POINT('Ctrl Pts',(0.511555090690949,19.4189778883406,-325.488307099043)) ;
#27191 = CARTESIAN_POINT('Ctrl Pts',(0.212096983529731,19.4242965252181,-325.484506877959)) ;
#27192 = CARTESIAN_POINT('Ctrl Pts',(0.0792228208986704,19.4252929018594,
-325.482811492848)) ;
#27193 = CARTESIAN_POINT('Ctrl Pts',(-0.637144776103283,19.4233143195477,
-325.473637808661)) ;
#27194 = CARTESIAN_POINT('Ctrl Pts',(-1.22026982434284,19.3954127480834,-325.466061074104)) ;
#27195 = CARTESIAN_POINT('Ctrl Pts',(-1.8645501317094,19.3354110137535,-325.457766339239)) ;
#27196 = CARTESIAN_POINT('Ctrl Pts',(-1.92781786674355,19.3292054813668,-325.456952503665)) ;
#27197 = CARTESIAN_POINT('Ctrl Pts',(-2.32890427390012,19.287876622844,-325.451798510013)) ;
#27198 = CARTESIAN_POINT('Ctrl Pts',(-2.66578387154997,19.2442089192046,-325.447494783036)) ;
#27199 = CARTESIAN_POINT('Ctrl Pts',(-3.15653004257167,19.1674623850162,-325.441280217299)) ;
#27200 = CARTESIAN_POINT('Ctrl Pts',(-3.31141454551974,19.1413121282674,-325.43932667505)) ;
#27201 = CARTESIAN_POINT('Ctrl Pts',(-3.58810845795464,19.0911370094629,-325.435850996478)) ;
#27202 = CARTESIAN_POINT('Ctrl Pts',(-3.71003689988122,19.0678174122861,-325.43432436018)) ;
#27203 = CARTESIAN_POINT('Ctrl Pts',(-3.97399378550779,19.0147063014837,-325.431029628515)) ;
#27204 = CARTESIAN_POINT('Ctrl Pts',(-4.11592894129979,18.9844887042316,-325.429264437186)) ;
#27205 = CARTESIAN_POINT('Ctrl Pts',(-4.53672429806264,18.8899616471011,-325.424047724228)) ;
#27206 = CARTESIAN_POINT('Ctrl Pts',(-4.81451647953566,18.8210772781552,-325.420626047351)) ;
#27207 = CARTESIAN_POINT('Ctrl Pts',(-5.30638877774985,18.687504440139,-325.414584514576)) ;
#27208 = CARTESIAN_POINT('Ctrl Pts',(-5.52106502101552,18.6252094011296,-325.411953423699)) ;
#27209 = CARTESIAN_POINT('Ctrl Pts',(-6.13783686938827,18.4346329357197,-325.404383996537)) ;
#27210 = CARTESIAN_POINT('Ctrl Pts',(-6.53688761140747,18.2969350700254,-325.39947589223)) ;
#27211 = CARTESIAN_POINT('Ctrl Pts',(-7.24928254297333,18.0248304259889,-325.390533864692)) ;
#27212 = CARTESIAN_POINT('Ctrl Pts',(-7.5641781448081,17.8949662547641,-325.386514902835)) ;
#27213 = CARTESIAN_POINT('Ctrl Pts',(-7.96648494652901,17.716536066583,-325.381213741478)) ;
#27214 = CARTESIAN_POINT('Ctrl Pts',(-8.05716260927202,17.6754819807262,-325.380007668473)) ;
#27215 = CARTESIAN_POINT('Ctrl Pts',(-8.20799421657633,17.6057914821919,-325.377979800514)) ;
#27216 = CARTESIAN_POINT('Ctrl Pts',(-8.26832362945437,17.5775392800325,-325.377162794693)) ;
#27217 = CARTESIAN_POINT('Ctrl Pts',(-8.3995556877948,17.5152583247555,-325.375371912301)) ;
#27218 = CARTESIAN_POINT('Ctrl Pts',(-8.4703992682553,17.4811082643757,-325.3743965703)) ;
#27219 = CARTESIAN_POINT('Ctrl Pts',(-8.68941199258846,17.3738895157889,-325.371356990998)) ;
#27220 = CARTESIAN_POINT('Ctrl Pts',(-8.83685765693119,17.2993602276784,-325.369276001264)) ;
#27221 = CARTESIAN_POINT('Ctrl Pts',(-9.09963580621888,17.1622976041766,-325.365516174525)) ;
#27222 = CARTESIAN_POINT('Ctrl Pts',(-9.21531970046943,17.1004594566374,-325.363842889233)) ;
#27223 = CARTESIAN_POINT('Ctrl Pts',(-9.82830009622013,16.7647677095671,-325.354895062352)) ;
#27224 = CARTESIAN_POINT('Ctrl Pts',(-10.3140384817978,16.470383436115,-325.347525279057)) ;
#27225 = CARTESIAN_POINT('Ctrl Pts',(-11.0542380440815,15.9761800330096,-325.336107181016)) ;
#27226 = CARTESIAN_POINT('Ctrl Pts',(-11.3177954555445,15.7905672429973,-325.331999949366)) ;
#27227 = CARTESIAN_POINT('Ctrl Pts',(-11.7373448421941,15.4791933200159,-325.325415713842)) ;
#27228 = CARTESIAN_POINT('Ctrl Pts',(-11.896223738703,15.3574265659992,-325.322910934181)) ;
#27229 = CARTESIAN_POINT('Ctrl Pts',(-12.1451388796296,15.1604740551693,-325.318969897457)) ;
#27230 = CARTESIAN_POINT('Ctrl Pts',(-12.236424730392,15.0868910594503,-325.31752086666)) ;
#27231 = CARTESIAN_POINT('Ctrl Pts',(-12.4254476052965,14.9316807689751,-325.314512367915)) ;
#27232 = CARTESIAN_POINT('Ctrl Pts',(-12.5230595077615,14.8499097436134,-325.312954199042)) ;
#27233 = CARTESIAN_POINT('Ctrl Pts',(-12.7590220875803,14.6482589309166,-325.309175259915)) ;
#27234 = CARTESIAN_POINT('Ctrl Pts',(-12.8964958303719,14.5273717434908,-325.306963164984)) ;
#27235 = CARTESIAN_POINT('Ctrl Pts',(-13.4421571901979,14.0336954113039,-325.298130765579)) ;
#27236 = CARTESIAN_POINT('Ctrl Pts',(-13.8360567781492,13.6455022312483,-325.291642829936)) ;
#27237 = CARTESIAN_POINT('Ctrl Pts',(-14.6185895700435,12.8055355763361,-325.278228551828)) ;
#27238 = CARTESIAN_POINT('Ctrl Pts',(-15.0040829844115,12.3516149349621,-325.271314446436)) ;
#27239 = CARTESIAN_POINT('Ctrl Pts',(-15.4360989494827,11.7927870380293,-325.262829499861)) ;
#27240 = CARTESIAN_POINT('Ctrl Pts',(-15.5033179036917,11.7042774585965,-325.261486037796)) ;
#27241 = CARTESIAN_POINT('Ctrl Pts',(-15.6067066728022,11.5656883451552,-325.259379337861)) ;
#27242 = CARTESIAN_POINT('Ctrl Pts',(-15.6434034935567,11.5160048280485,-325.258623482972)) ;
#27243 = CARTESIAN_POINT('Ctrl Pts',(-15.7220145385164,11.4085048652786,-325.256985800007)) ;
#27244 = CARTESIAN_POINT('Ctrl Pts',(-15.7638481627917,11.3506306210139,-325.256102767062)) ;
#27245 = CARTESIAN_POINT('Ctrl Pts',(-15.8787043670023,11.1898744114611,-325.253647794848)) ;
#27246 = CARTESIAN_POINT('Ctrl Pts',(-15.9510451857132,11.0865097812202,-325.25206682712)) ;
#27247 = CARTESIAN_POINT('Ctrl Pts',(-16.1169345638572,10.8444925506724,-325.248366336661)) ;
#27248 = CARTESIAN_POINT('Ctrl Pts',(-16.2097095479583,10.7053217920047,-325.246239300687)) ;
#27249 = CARTESIAN_POINT('Ctrl Pts',(-16.5578352597424,10.168199205621,-325.238057219706)) ;
#27250 = CARTESIAN_POINT('Ctrl Pts',(-16.8004225966218,9.76217108044045,-325.231932129668)) ;
#27251 = CARTESIAN_POINT('Ctrl Pts',(-17.05376759195,9.30067275081635,-325.225152231068)) ;
#27252 = CARTESIAN_POINT('Ctrl Pts',(-17.0793873382062,9.25354153018789,-325.224461827909)) ;
#27253 = CARTESIAN_POINT('Ctrl Pts',(-17.3158714098972,8.81416703960838,-325.218045252925)) ;
#27254 = CARTESIAN_POINT('Ctrl Pts',(-17.5133843011955,8.41488653451556,-325.212362892978)) ;
#27255 = CARTESIAN_POINT('Ctrl Pts',(-17.7691101723148,7.84983667910317,-325.204576985564)) ;
#27256 = CARTESIAN_POINT('Ctrl Pts',(-17.8390652671148,7.68953592407484,-325.202395545304)) ;
#27257 = CARTESIAN_POINT('Ctrl Pts',(-17.9557145367167,7.41207392937469,-325.198667163691)) ;
#27258 = CARTESIAN_POINT('Ctrl Pts',(-18.0034499688762,7.29536248076059,-325.197113083154)) ;
#27259 = CARTESIAN_POINT('Ctrl Pts',(-18.1002543879553,7.05194135329516,-325.193900773564)) ;
#27260 = CARTESIAN_POINT('Ctrl Pts',(-18.1491371029069,6.92516485281814,-325.19224390582)) ;
#27261 = CARTESIAN_POINT('Ctrl Pts',(-18.2777432755427,6.58090986513966,-325.187786481361)) ;
#27262 = CARTESIAN_POINT('Ctrl Pts',(-18.354913570991,6.36250123483369,-325.185003342196)) ;
#27263 = CARTESIAN_POINT('Ctrl Pts',(-18.4790809710085,5.99000174850145,-325.18032220449)) ;
#27264 = CARTESIAN_POINT('Ctrl Pts',(-18.5281008393189,5.83661150313104,-325.178413081954)) ;
#27265 = CARTESIAN_POINT('Ctrl Pts',(-18.742259423375,5.13657637620256,-325.169770903708)) ;
#27266 = CARTESIAN_POINT('Ctrl Pts',(-18.8851511305252,4.58342352960965,-325.163145314514)) ;
#27267 = CARTESIAN_POINT('Ctrl Pts',(-19.0746222314727,3.68881403487805,-325.152423939428)) ;
#27268 = CARTESIAN_POINT('Ctrl Pts',(-19.1368553128876,3.35101924194614,-325.148372066186)) ;
#27269 = CARTESIAN_POINT('Ctrl Pts',(-19.2055552960972,2.91328104766467,-325.143035004805)) ;
#27270 = CARTESIAN_POINT('Ctrl Pts',(-19.2202516871079,2.81469105580526,-325.141827260868)) ;
#27271 = CARTESIAN_POINT('Ctrl Pts',(-19.2435055375327,2.65001130961778,-325.139797485778)) ;
#27272 = CARTESIAN_POINT('Ctrl Pts',(-19.2524829186465,2.58398273798356,-325.138980265536)) ;
#27273 = CARTESIAN_POINT('Ctrl Pts',(-19.27130514207,2.43999934238564,-325.137190069394)) ;
#27274 = CARTESIAN_POINT('Ctrl Pts',(-19.2810170891532,2.36202850462239,-325.136215640312)) ;
#27275 = CARTESIAN_POINT('Ctrl Pts',(-19.3096311085158,2.12035971438911,-325.13318228033)) ;
#27276 = CARTESIAN_POINT('Ctrl Pts',(-19.3269234399747,1.95647874094133,-325.131106690573)) ;
#27277 = CARTESIAN_POINT('Ctrl Pts',(-19.3541858703878,1.66228433565311,-325.127358746894)) ;
#27278 = CARTESIAN_POINT('Ctrl Pts',(-19.3649300274119,1.53205251272656,-325.125691949031)) ;
#27279 = CARTESIAN_POINT('Ctrl Pts',(-19.4149988140806,0.84001055586709,-325.116809074575)) ;
#27280 = CARTESIAN_POINT('Ctrl Pts',(-19.4311909363592,0.276797040068225,
-325.109498680027)) ;
#27281 = CARTESIAN_POINT('Ctrl Pts',(-19.417744045745,-0.63538152314059,-325.097792450297)) ;
#27282 = CARTESIAN_POINT('Ctrl Pts',(-19.4031896511467,-0.9842386427811,-325.093345099064)) ;
#27283 = CARTESIAN_POINT('Ctrl Pts',(-19.3662102197858,-1.52204406103101,
-325.086561579064)) ;
#27284 = CARTESIAN_POINT('Ctrl Pts',(-19.3503984453435,-1.71137271484999,
-325.084187167638)) ;
#27285 = CARTESIAN_POINT('Ctrl Pts',(-19.3204967723043,-2.01554111185302,
-325.080395597961)) ;
#27286 = CARTESIAN_POINT('Ctrl Pts',(-19.30815376008,-2.13053981822835,-325.078967390448)) ;
#27287 = CARTESIAN_POINT('Ctrl Pts',(-19.2798857624754,-2.37344517915201,
-325.075961609207)) ;
#27288 = CARTESIAN_POINT('Ctrl Pts',(-19.263713242992,-2.50131748802154,-325.074385718642)) ;
#27289 = CARTESIAN_POINT('Ctrl Pts',(-19.2202248084203,-2.81968337948499,
-325.070477084289)) ;
#27290 = CARTESIAN_POINT('Ctrl Pts',(-19.1913485108284,-3.0099499233247,-325.068154550253)) ;
#27291 = CARTESIAN_POINT('Ctrl Pts',(-19.1216056445185,-3.42755952841807,
-325.06308005832)) ;
#27292 = CARTESIAN_POINT('Ctrl Pts',(-19.0795015650774,-3.65466646762184,
-325.060335697121)) ;
#27293 = CARTESIAN_POINT('Ctrl Pts',(-18.9220424391497,-4.42689012892456,
-325.051029120634)) ;
#27294 = CARTESIAN_POINT('Ctrl Pts',(-18.7872913964923,-4.96776889548514,
-325.044560511481)) ;
#27295 = CARTESIAN_POINT('Ctrl Pts',(-18.5271474023991,-5.84858564806015,
-325.033800285075)) ;
#27296 = CARTESIAN_POINT('Ctrl Pts',(-18.4151707174467,-6.19214269991828,
-325.029542713167)) ;
#27297 = CARTESIAN_POINT('Ctrl Pts',(-18.2599377107106,-6.62686704863102,
-325.023983596761)) ;
#27298 = CARTESIAN_POINT('Ctrl Pts',(-18.2254648371978,-6.72109540982123,
-325.022768069526)) ;
#27299 = CARTESIAN_POINT('Ctrl Pts',(-18.1668533760571,-6.87753704346685,
-325.020729390357)) ;
#27300 = CARTESIAN_POINT('Ctrl Pts',(-18.1431214584966,-6.93990065656124,
-325.019911150876)) ;
#27301 = CARTESIAN_POINT('Ctrl Pts',(-18.0908635771359,-7.0751256054184,-325.01812405294)) ;
#27302 = CARTESIAN_POINT('Ctrl Pts',(-18.0622178125445,-7.14793921145577,
-325.017153797515)) ;
#27303 = CARTESIAN_POINT('Ctrl Pts',(-17.9725909710944,-7.3717790226332,-325.014148736918)) ;
#27304 = CARTESIAN_POINT('Ctrl Pts',(-17.9101498348287,-7.52221276780784,
-325.012097695501)) ;
#27305 = CARTESIAN_POINT('Ctrl Pts',(-17.795109040592,-7.78981440631045,-325.008403604915)) ;
#27306 = CARTESIAN_POINT('Ctrl Pts',(-17.743225215228,-7.90727975761271,-325.006766128828)) ;
#27307 = CARTESIAN_POINT('Ctrl Pts',(-17.4657653127215,-8.51896719920325,
-324.998169653473)) ;
#27308 = CARTESIAN_POINT('Ctrl Pts',(-17.2206938810605,-9.00408036202466,
-324.991120432854)) ;
#27309 = CARTESIAN_POINT('Ctrl Pts',(-16.7496251075442,-9.84677095407904,
-324.978720865924)) ;
#27310 = CARTESIAN_POINT('Ctrl Pts',(-16.5316800765929,-10.2084472304841,
-324.973343686081)) ;
#27311 = CARTESIAN_POINT('Ctrl Pts',(-16.2193087154888,-10.6905493119142,
-324.966139763965)) ;
#27312 = CARTESIAN_POINT('Ctrl Pts',(-16.1349930409324,-10.8173850561086,
-324.964240601602)) ;
#27313 = CARTESIAN_POINT('Ctrl Pts',(-15.9783236758234,-11.0471545362745,
-324.960793427597)) ;
#27314 = CARTESIAN_POINT('Ctrl Pts',(-15.9064448121643,-11.1504019803719,
-324.959241880871)) ;
#27315 = CARTESIAN_POINT('Ctrl Pts',(-15.7562692224957,-11.3617080546284,
-324.956060795673)) ;
#27316 = CARTESIAN_POINT('Ctrl Pts',(-15.6778517224656,-11.469672844314,-324.954432325524)) ;
#27317 = CARTESIAN_POINT('Ctrl Pts',(-15.4683656838477,-11.7519292506606,
-324.950165108696)) ;
#27318 = CARTESIAN_POINT('Ctrl Pts',(-15.335463792758,-11.9248366246883,-324.947541132036)) ;
#27319 = CARTESIAN_POINT('Ctrl Pts',(-15.1079328779118,-12.2107615919193,
-324.943177365538)) ;
#27320 = CARTESIAN_POINT('Ctrl Pts',(-15.0148781504649,-12.3250058288699,
-324.941426910848)) ;
#27321 = CARTESIAN_POINT('Ctrl Pts',(-14.611293800828,-12.8091356031988,-324.9339703778)) ;
#27322 = CARTESIAN_POINT('Ctrl Pts',(-14.2883282720562,-13.1684295531974,
-324.928342984642)) ;
#27323 = CARTESIAN_POINT('Ctrl Pts',(-13.8527552853799,-13.6180861125026,
-324.921027695776)) ;
#27324 = CARTESIAN_POINT('Ctrl Pts',(-13.7520685835165,-13.7197561208005,
-324.919354151233)) ;
#27325 = CARTESIAN_POINT('Ctrl Pts',(-13.4169969565866,-14.050705232608,-324.913828681741)) ;
#27326 = CARTESIAN_POINT('Ctrl Pts',(-13.1779305257114,-14.2751627317519,
-324.909956315435)) ;
#27327 = CARTESIAN_POINT('Ctrl Pts',(-12.8593247697737,-14.5594718658922,
-324.904812259717)) ;
#27328 = CARTESIAN_POINT('Ctrl Pts',(-12.7848467594902,-14.6249153107428,
-324.90361084194)) ;
#27329 = CARTESIAN_POINT('Ctrl Pts',(-12.6595332055423,-14.7333388885969,
-324.901588278773)) ;
#27330 = CARTESIAN_POINT('Ctrl Pts',(-12.608971834638,-14.7766330762512,-324.900771861881)) ;
#27331 = CARTESIAN_POINT('Ctrl Pts',(-12.5088695028484,-14.8614598149172,
-324.899154115393)) ;
#27332 = CARTESIAN_POINT('Ctrl Pts',(-12.4593418784281,-14.9030065427896,
-324.898353179809)) ;
#27333 = CARTESIAN_POINT('Ctrl Pts',(-12.3470059019273,-14.9962892609332,
-324.896536301882)) ;
#27334 = CARTESIAN_POINT('Ctrl Pts',(-12.2840780040508,-15.0478793824886,
-324.895518366136)) ;
#27335 = CARTESIAN_POINT('Ctrl Pts',(-12.1163758174103,-15.1836135178141,
-324.892807247386)) ;
#27336 = CARTESIAN_POINT('Ctrl Pts',(-12.0110494255584,-15.2670682854659,
-324.89110623763)) ;
#27337 = CARTESIAN_POINT('Ctrl Pts',(-11.6600185560434,-15.5393244653469,
-324.885453775664)) ;
#27338 = CARTESIAN_POINT('Ctrl Pts',(-11.4106628089186,-15.7233397051941,
-324.881465738513)) ;
#27339 = CARTESIAN_POINT('Ctrl Pts',(-10.5698958691711,-16.3132563050286,
-324.868220810446)) ;
#27340 = CARTESIAN_POINT('Ctrl Pts',(-9.96041182877992,-16.6923705271283,
-324.858960304287)) ;
#27341 = CARTESIAN_POINT('Ctrl Pts',(-9.17625143333914,-17.1218664623924,
-324.847726790361)) ;
#27342 = CARTESIAN_POINT('Ctrl Pts',(-9.019988594336,-17.2047001547047,-324.845519004315)) ;
#27343 = CARTESIAN_POINT('Ctrl Pts',(-8.75156815941257,-17.3423254858162,
-324.8417794228)) ;
#27344 = CARTESIAN_POINT('Ctrl Pts',(-8.63997384254361,-17.3981910137934,
-324.840240006221)) ;
#27345 = CARTESIAN_POINT('Ctrl Pts',(-8.42416522002516,-17.5036391147451,
-324.837291916696)) ;
#27346 = CARTESIAN_POINT('Ctrl Pts',(-8.32003210973969,-17.553375961431,-324.835882181701)) ;
#27347 = CARTESIAN_POINT('Ctrl Pts',(-8.07790275567883,-17.6663849333925,
-324.832632938715)) ;
#27348 = CARTESIAN_POINT('Ctrl Pts',(-7.93959560311288,-17.7289732156982,
-324.830798283569)) ;
#27349 = CARTESIAN_POINT('Ctrl Pts',(-7.24756956185587,-18.0324142997913,
-324.821717435721)) ;
#27350 = CARTESIAN_POINT('Ctrl Pts',(-6.68356404261919,-18.2489781452747,
-324.814640938176)) ;
#27351 = CARTESIAN_POINT('Ctrl Pts',(-5.58364637795645,-18.6134748534662,
-324.80110584276)) ;
#27352 = CARTESIAN_POINT('Ctrl Pts',(-5.04966680747359,-18.7653780770332,
-324.794647447349)) ;
#27353 = CARTESIAN_POINT('Ctrl Pts',(-4.39902852307145,-18.9206810315247,
-324.786617109329)) ;
#27354 = CARTESIAN_POINT('Ctrl Pts',(-4.2879057954522,-18.9461733993227,-324.785239714493)) ;
#27355 = CARTESIAN_POINT('Ctrl Pts',(-4.1157701721843,-18.9840705876446,-324.783092952287)) ;
#27356 = CARTESIAN_POINT('Ctrl Pts',(-4.0549111575994,-18.997162832384,-324.782331435344)) ;
#27357 = CARTESIAN_POINT('Ctrl Pts',(-3.93487736158078,-19.022381915437,-324.780823641292)) ;
#27358 = CARTESIAN_POINT('Ctrl Pts',(-3.87570685362606,-19.0345257351029,
-324.780077582616)) ;
#27359 = CARTESIAN_POINT('Ctrl Pts',(-3.74585696339403,-19.0605448135223,
-324.778434988017)) ;
#27360 = CARTESIAN_POINT('Ctrl Pts',(-3.67515509241211,-19.074303342726,-324.777537136675)) ;
#27361 = CARTESIAN_POINT('Ctrl Pts',(-3.49718704242215,-19.1079095529508,
-324.775269776329)) ;
#27362 = CARTESIAN_POINT('Ctrl Pts',(-3.38982717854915,-19.1272474849493,
-324.77389531636)) ;
#27363 = CARTESIAN_POINT('Ctrl Pts',(-3.06832164573027,-19.1823659712464,
-324.769764870065)) ;
#27364 = CARTESIAN_POINT('Ctrl Pts',(-2.85373323831447,-19.2154617008725,
-324.766989080645)) ;
#27365 = CARTESIAN_POINT('Ctrl Pts',(-1.76429229245401,-19.3648326843405,
-324.752866134105)) ;
#27366 = CARTESIAN_POINT('Ctrl Pts',(-0.882788452479083,-19.4249883427977,
-324.741391833281)) ;
#27367 = CARTESIAN_POINT('Ctrl Pts',(-0.000256543979532398,-19.4249999983059,
-324.730314803639)) ;
#27368 = CARTESIAN_POINT('Ctrl Pts',(-0.000363249083131095,-19.4249999966036,
-324.51951242736)) ;
#27369 = CARTESIAN_POINT('Ctrl Pts',(-0.368607332582545,-19.4249931104092,
-324.523887089415)) ;
#27370 = CARTESIAN_POINT('Ctrl Pts',(-0.73677704384083,-19.4145148993854,
-324.528207924419)) ;
#27371 = CARTESIAN_POINT('Ctrl Pts',(-1.74422720388531,-19.3571425948576,
-324.540005485921)) ;
#27372 = CARTESIAN_POINT('Ctrl Pts',(-2.38183084770121,-19.2890687619575,
-324.547434282136)) ;
#27373 = CARTESIAN_POINT('Ctrl Pts',(-3.1193991887729,-19.1731886686412,-324.556413841303)) ;
#27374 = CARTESIAN_POINT('Ctrl Pts',(-3.2237642527278,-19.155917075924,-324.557693900277)) ;
#27375 = CARTESIAN_POINT('Ctrl Pts',(-3.39389086251675,-19.126332764801,-324.559799404865)) ;
#27376 = CARTESIAN_POINT('Ctrl Pts',(-3.45973917404293,-19.1145312543628,
-324.560619007596)) ;
#27377 = CARTESIAN_POINT('Ctrl Pts',(-3.59984144819257,-19.0886740650673,
-324.56237375461)) ;
#27378 = CARTESIAN_POINT('Ctrl Pts',(-3.67407688585795,-19.0745247655761,
-324.563309926414)) ;
#27379 = CARTESIAN_POINT('Ctrl Pts',(-3.89330097014754,-19.0314133133711,
-324.566091477331)) ;
#27380 = CARTESIAN_POINT('Ctrl Pts',(-4.03804352861184,-19.0012286312902,
-324.567949935994)) ;
#27381 = CARTESIAN_POINT('Ctrl Pts',(-4.38714467628392,-18.9242577974208,
-324.572474247856)) ;
#27382 = CARTESIAN_POINT('Ctrl Pts',(-4.59111793609637,-18.8758101150869,
-324.575152592198)) ;
#27383 = CARTESIAN_POINT('Ctrl Pts',(-5.63482349233041,-18.6099907333345,
-324.58897734174)) ;
#27384 = CARTESIAN_POINT('Ctrl Pts',(-6.46010429753605,-18.3398489056761,
-324.600261335798)) ;
#27385 = CARTESIAN_POINT('Ctrl Pts',(-7.43744471109511,-17.9457457261627,
-324.613514878287)) ;
#27386 = CARTESIAN_POINT('Ctrl Pts',(-7.60931543644837,-17.8735472763722,
-324.615843637309)) ;
#27387 = CARTESIAN_POINT('Ctrl Pts',(-7.89612842799482,-17.7481776540722,
-324.61972551927)) ;
#27388 = CARTESIAN_POINT('Ctrl Pts',(-8.01163789221662,-17.6963361328111,
-324.621287731253)) ;
#27389 = CARTESIAN_POINT('Ctrl Pts',(-8.24659723913017,-17.5881125713985,
-324.62446345231)) ;
#27390 = CARTESIAN_POINT('Ctrl Pts',(-8.3659955044135,-17.5316339547681,-324.626076174751)) ;
#27391 = CARTESIAN_POINT('Ctrl Pts',(-8.67419904665552,-17.3819797981122,
-324.630237757478)) ;
#27392 = CARTESIAN_POINT('Ctrl Pts',(-8.86208210442236,-17.286944547256,-324.632773246298)) ;
#27393 = CARTESIAN_POINT('Ctrl Pts',(-9.17226337590775,-17.1236622363684,
-324.636963555373)) ;
#27394 = CARTESIAN_POINT('Ctrl Pts',(-9.29543490974306,-17.0571132877477,
-324.638628733178)) ;
#27395 = CARTESIAN_POINT('Ctrl Pts',(-9.80463915371254,-16.7748391550134,
-324.645525181517)) ;
#27396 = CARTESIAN_POINT('Ctrl Pts',(-10.1839681700064,-16.5472949560962,
-324.650689497295)) ;
#27397 = CARTESIAN_POINT('Ctrl Pts',(-10.625255237654,-16.2616585880031,-324.656828940282)) ;
#27398 = CARTESIAN_POINT('Ctrl Pts',(-10.6950173349779,-16.2158623915263,
-324.657803659373)) ;
#27399 = CARTESIAN_POINT('Ctrl Pts',(-10.8248997979754,-16.129396684843,-324.659627526123)) ;
#27400 = CARTESIAN_POINT('Ctrl Pts',(-10.8850915333987,-16.0888369797221,
-324.660476480876)) ;
#27401 = CARTESIAN_POINT('Ctrl Pts',(-11.2550270070968,-15.8365327147582,
-324.665720257567)) ;
#27402 = CARTESIAN_POINT('Ctrl Pts',(-11.5588086445539,-15.6161884836158,
-324.670138444608)) ;
#27403 = CARTESIAN_POINT('Ctrl Pts',(-11.935321334371,-15.3260807985454,-324.675862941955)) ;
#27404 = CARTESIAN_POINT('Ctrl Pts',(-12.0141520293376,-15.2643636937481,
-324.677075863568)) ;
#27405 = CARTESIAN_POINT('Ctrl Pts',(-12.1446980500494,-15.1605205243333,
-324.679111558303)) ;
#27406 = CARTESIAN_POINT('Ctrl Pts',(-12.1966798830382,-15.118732524105,-324.679929452985)) ;
#27407 = CARTESIAN_POINT('Ctrl Pts',(-12.3092596274258,-15.0272715994966,
-324.681717570718)) ;
#27408 = CARTESIAN_POINT('Ctrl Pts',(-12.3697741618878,-14.9774981710467,
-324.682689209409)) ;
#27409 = CARTESIAN_POINT('Ctrl Pts',(-12.5556320198291,-14.8227346670844,
-324.685703624531)) ;
#27410 = CARTESIAN_POINT('Ctrl Pts',(-12.6799520714954,-14.7165272312688,
-324.687762776328)) ;
#27411 = CARTESIAN_POINT('Ctrl Pts',(-12.9000485408463,-14.5236377557519,
-324.691474628817)) ;
#27412 = CARTESIAN_POINT('Ctrl Pts',(-12.9963293755352,-14.4375458001215,
-324.693121761559)) ;
#27413 = CARTESIAN_POINT('Ctrl Pts',(-13.4978614919641,-13.9800056309785,
-324.701811295967)) ;
#27414 = CARTESIAN_POINT('Ctrl Pts',(-13.8880682228419,-13.59243849508,-324.708945253904)) ;
#27415 = CARTESIAN_POINT('Ctrl Pts',(-14.5520398094792,-12.8744752783496,
-324.721501728454)) ;
#27416 = CARTESIAN_POINT('Ctrl Pts',(-14.8322947178448,-12.5505781281214,
-324.726952310985)) ;
#27417 = CARTESIAN_POINT('Ctrl Pts',(-15.2033110505697,-12.0919849506846,
-324.734342000055)) ;
#27418 = CARTESIAN_POINT('Ctrl Pts',(-15.303432133127,-11.9650211866163,-324.736355277088)) ;
#27419 = CARTESIAN_POINT('Ctrl Pts',(-15.4779915321134,-11.7378862140117,
-324.739899488485)) ;
#27420 = CARTESIAN_POINT('Ctrl Pts',(-15.5530715046046,-11.6382198579215,
-324.741435557541)) ;
#27421 = CARTESIAN_POINT('Ctrl Pts',(-15.7106097808053,-11.4248453790538,
-324.744684270358)) ;
#27422 = CARTESIAN_POINT('Ctrl Pts',(-15.7928056676612,-11.3109522512111,
-324.746394754798)) ;
#27423 = CARTESIAN_POINT('Ctrl Pts',(-16.0223502412724,-10.9855076750169,
-324.751218228642)) ;
#27424 = CARTESIAN_POINT('Ctrl Pts',(-16.1667328223465,-10.7719003119683,
-324.754308198409)) ;
#27425 = CARTESIAN_POINT('Ctrl Pts',(-16.5001278919634,-10.2568491186854,
-324.761601200645)) ;
#27426 = CARTESIAN_POINT('Ctrl Pts',(-16.6851947927748,-9.95296184527758,
-324.765779071058)) ;
#27427 = CARTESIAN_POINT('Ctrl Pts',(-17.1546116698316,-9.13223553285217,
-324.776837972113)) ;
#27428 = CARTESIAN_POINT('Ctrl Pts',(-17.4239446690138,-8.60723973028282,
-324.783677291709)) ;
#27429 = CARTESIAN_POINT('Ctrl Pts',(-17.7300154118263,-7.9371759473243,-324.792468037807)) ;
#27430 = CARTESIAN_POINT('Ctrl Pts',(-17.7895377357261,-7.80285560307284,
-324.794233806537)) ;
#27431 = CARTESIAN_POINT('Ctrl Pts',(-17.8772934261257,-7.59859787440915,
-324.796932587157)) ;
#27432 = CARTESIAN_POINT('Ctrl Pts',(-17.9066527183147,-7.52914990606029,
-324.797852542709)) ;
#27433 = CARTESIAN_POINT('Ctrl Pts',(-17.9616335713812,-7.39695463453026,
-324.799609647532)) ;
#27434 = CARTESIAN_POINT('Ctrl Pts',(-17.9873324856987,-7.33424082155586,
-324.800445875654)) ;
#27435 = CARTESIAN_POINT('Ctrl Pts',(-18.0527738100199,-7.17212952202171,
-324.802613251178)) ;
#27436 = CARTESIAN_POINT('Ctrl Pts',(-18.0920237353459,-7.07253570007065,
-324.803950295831)) ;
#27437 = CARTESIAN_POINT('Ctrl Pts',(-18.3095247827385,-6.50698214795709,
-324.811563596741)) ;
#27438 = CARTESIAN_POINT('Ctrl Pts',(-18.4705961028508,-6.03461620884636,
-324.817996869729)) ;
#27439 = CARTESIAN_POINT('Ctrl Pts',(-18.7988848052937,-4.93492142458627,
-324.832803259053)) ;
#27440 = CARTESIAN_POINT('Ctrl Pts',(-18.9532062671738,-4.30435790939297,
-324.841161715128)) ;
#27441 = CARTESIAN_POINT('Ctrl Pts',(-19.110964143209,-3.48376084504112,-324.851671915868)) ;
#27442 = CARTESIAN_POINT('Ctrl Pts',(-19.1435912961154,-3.29976552958719,
-324.854006385731)) ;
#27443 = CARTESIAN_POINT('Ctrl Pts',(-19.1938751866936,-2.9902889221362,-324.85789486167)) ;
#27444 = CARTESIAN_POINT('Ctrl Pts',(-19.2129679622242,-2.8650540400479,-324.859458028139)) ;
#27445 = CARTESIAN_POINT('Ctrl Pts',(-19.2494470467824,-2.60899013884006,
-324.862633419556)) ;
#27446 = CARTESIAN_POINT('Ctrl Pts',(-19.2667278168091,-2.47815262636089,
-324.864244881386)) ;
#27447 = CARTESIAN_POINT('Ctrl Pts',(-19.3080403099529,-2.13875563626868,
-324.868397977124)) ;
#27448 = CARTESIAN_POINT('Ctrl Pts',(-19.3300267363531,-1.9299644699258,-324.870926349816)) ;
#27449 = CARTESIAN_POINT('Ctrl Pts',(-19.3609751410651,-1.58199320377107,
-324.875102796553)) ;
#27450 = CARTESIAN_POINT('Ctrl Pts',(-19.3718304014805,-1.44299960345173,
-324.876761201998)) ;
#27451 = CARTESIAN_POINT('Ctrl Pts',(-19.4106652614121,-0.86575818283232,
-324.883614974356)) ;
#27452 = CARTESIAN_POINT('Ctrl Pts',(-19.4252761978651,-0.426741381569603,
-324.888744235974)) ;
#27453 = CARTESIAN_POINT('Ctrl Pts',(-19.4249037842933,0.157013435474684,
-324.895562093413)) ;
#27454 = CARTESIAN_POINT('Ctrl Pts',(-19.4231964476866,0.301628892196292,
-324.897251231417)) ;
#27455 = CARTESIAN_POINT('Ctrl Pts',(-19.4116346715268,0.804816558384056,
-324.903142417549)) ;
#27456 = CARTESIAN_POINT('Ctrl Pts',(-19.3934636536477,1.16312371228953,-324.907360757565)) ;
#27457 = CARTESIAN_POINT('Ctrl Pts',(-19.356245472028,1.6370728455232,-324.913064801735)) ;
#27458 = CARTESIAN_POINT('Ctrl Pts',(-19.3460601909795,1.75334004201231,-324.914474164533)) ;
#27459 = CARTESIAN_POINT('Ctrl Pts',(-19.3287914436211,1.93193687836117,-324.916658834579)) ;
#27460 = CARTESIAN_POINT('Ctrl Pts',(-19.3224528243252,1.99433588287526,-324.917425843237)) ;
#27461 = CARTESIAN_POINT('Ctrl Pts',(-19.3083942515218,2.12636892063776,-324.919057622037)) ;
#27462 = CARTESIAN_POINT('Ctrl Pts',(-19.3005995602904,2.19599406817172,-324.919923355672)) ;
#27463 = CARTESIAN_POINT('Ctrl Pts',(-19.2785061742896,2.38412952436164,-324.922275428641)) ;
#27464 = CARTESIAN_POINT('Ctrl Pts',(-19.2634914820184,2.50255264880877,-324.923769647723)) ;
#27465 = CARTESIAN_POINT('Ctrl Pts',(-19.1926066687591,3.02313106842967,-324.930387438392)) ;
#27466 = CARTESIAN_POINT('Ctrl Pts',(-19.1252275133483,3.4236156079509,-324.935606281046)) ;
#27467 = CARTESIAN_POINT('Ctrl Pts',(-18.8999474976657,4.54629511324837,-324.950369269271)) ;
#27468 = CARTESIAN_POINT('Ctrl Pts',(-18.7133120267843,5.26201255935657,-324.959917939432)) ;
#27469 = CARTESIAN_POINT('Ctrl Pts',(-18.4318193692617,6.13434528246556,-324.971429891259)) ;
#27470 = CARTESIAN_POINT('Ctrl Pts',(-18.3749724260403,6.30258246921978,-324.973645623024)) ;
#27471 = CARTESIAN_POINT('Ctrl Pts',(-18.27369742355,6.58927962630996,-324.977413147375)) ;
#27472 = CARTESIAN_POINT('Ctrl Pts',(-18.2304042300151,6.70812829191659,-324.978972488328)) ;
#27473 = CARTESIAN_POINT('Ctrl Pts',(-18.1385320812043,6.95287617442221,-324.982178996623)) ;
#27474 = CARTESIAN_POINT('Ctrl Pts',(-18.0897957378861,7.07870916042882,-324.983824978575)) ;
#27475 = CARTESIAN_POINT('Ctrl Pts',(-17.9557823515233,7.41429496806485,-324.988209387055)) ;
#27476 = CARTESIAN_POINT('Ctrl Pts',(-17.8681424591935,7.62308172809699,-324.990931432654)) ;
#27477 = CARTESIAN_POINT('Ctrl Pts',(-17.7141100294958,7.97277698637304,-324.995489894093)) ;
#27478 = CARTESIAN_POINT('Ctrl Pts',(-17.6496364976262,8.11450544260688,-324.997337273074)) ;
#27479 = CARTESIAN_POINT('Ctrl Pts',(-17.3563169390301,8.73925376450783,-325.005491493212)) ;
#27480 = CARTESIAN_POINT('Ctrl Pts',(-17.1092963951651,9.21348309503388,-325.011703415862)) ;
#27481 = CARTESIAN_POINT('Ctrl Pts',(-16.6633549071506,9.9896606498155,-325.022180284475)) ;
#27482 = CARTESIAN_POINT('Ctrl Pts',(-16.4749992001847,10.2973354291511,-325.026421402697)) ;
#27483 = CARTESIAN_POINT('Ctrl Pts',(-16.2144236414078,10.6975112079814,-325.032150801032)) ;
#27484 = CARTESIAN_POINT('Ctrl Pts',(-16.1497774817049,10.7948583733239,-325.033561874647)) ;
#27485 = CARTESIAN_POINT('Ctrl Pts',(-16.0490756956369,10.9435703164506,-325.03574857723)) ;
#27486 = CARTESIAN_POINT('Ctrl Pts',(-16.013642925308,10.9953536643952,-325.03651588339)) ;
#27487 = CARTESIAN_POINT('Ctrl Pts',(-15.9381345061251,11.1045665171004,-325.038147572487)) ;
#27488 = CARTESIAN_POINT('Ctrl Pts',(-15.8979979536569,11.1619527910017,-325.039012912954)) ;
#27489 = CARTESIAN_POINT('Ctrl Pts',(-15.7886994689323,11.3164396223703,-325.041362625346)) ;
#27490 = CARTESIAN_POINT('Ctrl Pts',(-15.7189525725689,11.4131225615677,-325.042854851139)) ;
#27491 = CARTESIAN_POINT('Ctrl Pts',(-15.4197721690338,11.8199004576638,-325.049215118221)) ;
#27492 = CARTESIAN_POINT('Ctrl Pts',(-15.1820190343417,12.123766648707,-325.05416858626)) ;
#27493 = CARTESIAN_POINT('Ctrl Pts',(-14.4451991957954,13.0097868472777,-325.069020313278)) ;
#27494 = CARTESIAN_POINT('Ctrl Pts',(-13.9205544390007,13.569690764296,-325.078934043954)) ;
#27495 = CARTESIAN_POINT('Ctrl Pts',(-13.2374997315169,14.2172326559511,-325.090748781695)) ;
#27496 = CARTESIAN_POINT('Ctrl Pts',(-13.1091891076168,14.3356292015037,-325.092926245476)) ;
#27497 = CARTESIAN_POINT('Ctrl Pts',(-12.8855190659725,14.5365027320809,-325.096650100929)) ;
#27498 = CARTESIAN_POINT('Ctrl Pts',(-12.7909206778261,14.6198105850174,-325.098203584598)) ;
#27499 = CARTESIAN_POINT('Ctrl Pts',(-12.5925957493675,14.7910665270515,-325.101416648189)) ;
#27500 = CARTESIAN_POINT('Ctrl Pts',(-12.4887429276944,14.878858049614,-325.103074845725)) ;
#27501 = CARTESIAN_POINT('Ctrl Pts',(-12.2050376314705,15.1136238515859,-325.107541206289)) ;
#27502 = CARTESIAN_POINT('Ctrl Pts',(-12.0234570239237,15.2584747262203,-325.110331823123)) ;
#27503 = CARTESIAN_POINT('Ctrl Pts',(-11.7111393562844,15.4985800011832,-325.115028052145)) ;
#27504 = CARTESIAN_POINT('Ctrl Pts',(-11.5817308258968,15.5955210949443,-325.116944806609)) ;
#27505 = CARTESIAN_POINT('Ctrl Pts',(-10.9860200675328,16.0302691146094,-325.125650132465)) ;
#27506 = CARTESIAN_POINT('Ctrl Pts',(-10.5060515857835,16.3488545200602,-325.132329538069)) ;
#27507 = CARTESIAN_POINT('Ctrl Pts',(-9.88787461375091,16.720698555901,-325.140789654089)) ;
#27508 = CARTESIAN_POINT('Ctrl Pts',(-9.7622667993393,16.7943434364832,-325.142502173436)) ;
#27509 = CARTESIAN_POINT('Ctrl Pts',(-9.44690652593406,16.9745082384834,-325.146797016947)) ;
#27510 = CARTESIAN_POINT('Ctrl Pts',(-9.25616996445633,17.0792649177425,-325.149390325727)) ;
#27511 = CARTESIAN_POINT('Ctrl Pts',(-8.98662443584238,17.2214634400773,-325.153072967232)) ;
#27512 = CARTESIAN_POINT('Ctrl Pts',(-8.90926189738624,17.2616127342032,-325.154131972869)) ;
#27513 = CARTESIAN_POINT('Ctrl Pts',(-8.77314327357809,17.3310961686683,-325.156000933056)) ;
#27514 = CARTESIAN_POINT('Ctrl Pts',(-8.71450391206616,17.3606554848438,-325.15680801149)) ;
#27515 = CARTESIAN_POINT('Ctrl Pts',(-8.57869231175896,17.4282548065239,-325.158681898262)) ;
#27516 = CARTESIAN_POINT('Ctrl Pts',(-8.50141520428343,17.4660804669774,-325.159751370941)) ;
#27517 = CARTESIAN_POINT('Ctrl Pts',(-8.23098669893119,17.5962300917132,-325.16350179842)) ;
#27518 = CARTESIAN_POINT('Ctrl Pts',(-8.03656266261235,17.685873339037,-325.166211900098)) ;
#27519 = CARTESIAN_POINT('Ctrl Pts',(-7.49531398524474,17.924659014154,-325.173756756317)) ;
#27520 = CARTESIAN_POINT('Ctrl Pts',(-7.14556263465918,18.0669329663617,-325.178631325225)) ;
#27521 = CARTESIAN_POINT('Ctrl Pts',(-6.65250779134534,18.2509423844661,-325.185420995463)) ;
#27522 = CARTESIAN_POINT('Ctrl Pts',(-6.51253389172983,18.3013567847367,-325.187339703212)) ;
#27523 = CARTESIAN_POINT('Ctrl Pts',(-5.9095715038718,18.510732261236,-325.195555919158)) ;
#27524 = CARTESIAN_POINT('Ctrl Pts',(-5.44124290075414,18.653769653589,-325.201809566647)) ;
#27525 = CARTESIAN_POINT('Ctrl Pts',(-4.8188103906079,18.8184353860043,-325.209886926799)) ;
#27526 = CARTESIAN_POINT('Ctrl Pts',(-4.66914407922479,18.8561273227786,-325.211812143026)) ;
#27527 = CARTESIAN_POINT('Ctrl Pts',(-4.39626426216751,18.9214011917838,-325.215290999131)) ;
#27528 = CARTESIAN_POINT('Ctrl Pts',(-4.27320066601249,18.949573046387,-325.216848421088)) ;
#27529 = CARTESIAN_POINT('Ctrl Pts',(-4.02027991853283,19.0048828300569,-325.220026146259)) ;
#27530 = CARTESIAN_POINT('Ctrl Pts',(-3.8904017388695,19.0318941877486,-325.221645540904)) ;
#27531 = CARTESIAN_POINT('Ctrl Pts',(-3.55056662750564,19.0989471826183,-325.225851951702)) ;
#27532 = CARTESIAN_POINT('Ctrl Pts',(-3.34020749841544,19.1368576558235,-325.2284250089)) ;
#27533 = CARTESIAN_POINT('Ctrl Pts',(-2.98804172153173,19.1943404986764,-325.232688713624)) ;
#27534 = CARTESIAN_POINT('Ctrl Pts',(-2.84656752583494,19.2158308142655,-325.234389853303)) ;
#27535 = CARTESIAN_POINT('Ctrl Pts',(-2.2504064075521,19.2996610295794,-325.241517168713)) ;
#27536 = CARTESIAN_POINT('Ctrl Pts',(-1.79382180773071,19.3474403621072,-325.246871687205)) ;
#27537 = CARTESIAN_POINT('Ctrl Pts',(-0.868674254276153,19.4112193736203,
-325.25770378038)) ;
#27538 = CARTESIAN_POINT('Ctrl Pts',(-0.400362562262684,19.4265215652412,
-325.263178244891)) ;
#27539 = CARTESIAN_POINT('Ctrl Pts',(0.187025652032619,19.4244640529543,-325.270222623098)) ;
#27540 = CARTESIAN_POINT('Ctrl Pts',(0.306003078054853,19.4229540593874,-325.271658875818)) ;
#27541 = CARTESIAN_POINT('Ctrl Pts',(0.48806508791664,19.4189701519047,-325.273875531531)) ;
#27542 = CARTESIAN_POINT('Ctrl Pts',(0.551164070730255,19.4172816698578,-325.274647252462)) ;
#27543 = CARTESIAN_POINT('Ctrl Pts',(0.683820183459702,19.4130847446476,-325.276277947389)) ;
#27544 = CARTESIAN_POINT('Ctrl Pts',(0.753374275789827,19.4105099499722,-325.277137792633)) ;
#27545 = CARTESIAN_POINT('Ctrl Pts',(0.939823431378142,19.4026041952801,-325.279454329519)) ;
#27546 = CARTESIAN_POINT('Ctrl Pts',(1.0566866429843,19.3965907035092,-325.280918513096)) ;
#27547 = CARTESIAN_POINT('Ctrl Pts',(1.76202815745998,19.3539021846119,-325.28981532353)) ;
#27548 = CARTESIAN_POINT('Ctrl Pts',(2.34864076285009,19.2915048356768,-325.297455202503)) ;
#27549 = CARTESIAN_POINT('Ctrl Pts',(3.18749649349097,19.163443076039,-325.308396900876)) ;
#27550 = CARTESIAN_POINT('Ctrl Pts',(3.44268206259244,19.1192474967462,-325.311729299308)) ;
#27551 = CARTESIAN_POINT('Ctrl Pts',(4.04014302449614,19.0034235689134,-325.319513271679)) ;
#27552 = CARTESIAN_POINT('Ctrl Pts',(4.38151981789101,18.9276292228183,-325.323946111349)) ;
#27553 = CARTESIAN_POINT('Ctrl Pts',(4.87405700639025,18.8042335430064,-325.330300306474)) ;
#27554 = CARTESIAN_POINT('Ctrl Pts',(5.02697389711931,18.7639325402317,-325.332267429082)) ;
#27555 = CARTESIAN_POINT('Ctrl Pts',(5.2990908966547,18.6886513080914,-325.335757626753)) ;
#27556 = CARTESIAN_POINT('Ctrl Pts',(5.41847970892812,18.654386340405,-325.33728535688)) ;
#27557 = CARTESIAN_POINT('Ctrl Pts',(5.67589511557756,18.5778275766727,-325.340572153735)) ;
#27558 = CARTESIAN_POINT('Ctrl Pts',(5.81379556488206,18.5351353928778,-325.342328434714)) ;
#27559 = CARTESIAN_POINT('Ctrl Pts',(6.21907285743305,18.4046989119538,-325.347479281235)) ;
#27560 = CARTESIAN_POINT('Ctrl Pts',(6.48503361034648,18.3126772689196,-325.350845206379)) ;
#27561 = CARTESIAN_POINT('Ctrl Pts',(7.13392445866303,18.0722533307277,-325.359051446528)) ;
#27562 = CARTESIAN_POINT('Ctrl Pts',(7.51432768800239,17.917424438839,-325.363855706064)) ;
#27563 = CARTESIAN_POINT('Ctrl Pts',(8.39559008253239,17.5257345362505,-325.375120538798)) ;
#27564 = CARTESIAN_POINT('Ctrl Pts',(8.89179086982165,17.2792753108281,-325.381566145849)) ;
#27565 = CARTESIAN_POINT('Ctrl Pts',(9.47673183865562,16.9568630366151,-325.389584211315)) ;
#27566 = CARTESIAN_POINT('Ctrl Pts',(9.57619557678084,16.9008913553037,-325.39096304451)) ;
#27567 = CARTESIAN_POINT('Ctrl Pts',(9.72915810139678,16.8130302272867,-325.393111509246)) ;
#27568 = CARTESIAN_POINT('Ctrl Pts',(9.78300656109073,16.781754538799,-325.393873270373)) ;
#27569 = CARTESIAN_POINT('Ctrl Pts',(9.89761917857128,16.7144473439642,-325.395507171316)) ;
#27570 = CARTESIAN_POINT('Ctrl Pts',(9.95833904811313,16.6783422078526,-325.396380383355)) ;
#27571 = CARTESIAN_POINT('Ctrl Pts',(10.1236531178821,16.5788188393363,-325.398777090183)) ;
#27572 = CARTESIAN_POINT('Ctrl Pts',(10.2278473510381,16.514742657855,-325.400308957564)) ;
#27573 = CARTESIAN_POINT('Ctrl Pts',(10.4670981303155,16.3644782456107,-325.403869645579)) ;
#27574 = CARTESIAN_POINT('Ctrl Pts',(10.6017075145806,16.2775946991318,-325.405905253548)) ;
#27575 = CARTESIAN_POINT('Ctrl Pts',(11.0954299089653,15.950199345179,-325.413471488027)) ;
#27576 = CARTESIAN_POINT('Ctrl Pts',(11.4475610480983,15.6993875639636,-325.419063631053)) ;
#27577 = CARTESIAN_POINT('Ctrl Pts',(11.864998600235,15.3805427780386,-325.42583542734)) ;
#27578 = CARTESIAN_POINT('Ctrl Pts',(11.9385581588302,15.3235151654231,-325.427034444693)) ;
#27579 = CARTESIAN_POINT('Ctrl Pts',(12.3822719068559,14.9743882006204,-325.434298155488)) ;
#27580 = CARTESIAN_POINT('Ctrl Pts',(12.7421001938579,14.6694186779427,-325.440316871328)) ;
#27581 = CARTESIAN_POINT('Ctrl Pts',(13.2038260649252,14.2482679740031,-325.448155735435)) ;
#27582 = CARTESIAN_POINT('Ctrl Pts',(13.3159484470554,14.1435384558895,-325.450069266996)) ;
#27583 = CARTESIAN_POINT('Ctrl Pts',(13.5179038621064,13.9503687091569,-325.45353389443)) ;
#27584 = CARTESIAN_POINT('Ctrl Pts',(13.6081391772843,13.8623612753066,-325.455088661402)) ;
#27585 = CARTESIAN_POINT('Ctrl Pts',(13.7918132126998,13.6797003278597,-325.458267771821)) ;
#27586 = CARTESIAN_POINT('Ctrl Pts',(13.8851492632979,13.5849528061858,-325.459891136017)) ;
#27587 = CARTESIAN_POINT('Ctrl Pts',(14.1272444060979,13.3340948991893,-325.464124160004)) ;
#27588 = CARTESIAN_POINT('Ctrl Pts',(14.2743900060806,13.1764529164931,-325.466719507893)) ;
#27589 = CARTESIAN_POINT('Ctrl Pts',(14.5160062522204,12.908803066421,-325.471026932218)) ;
#27590 = CARTESIAN_POINT('Ctrl Pts',(14.6119246120961,12.8001286441634,-325.472749577824)) ;
#27591 = CARTESIAN_POINT('Ctrl Pts',(15.0131750363146,12.3351282602621,-325.480018573662)) ;
#27592 = CARTESIAN_POINT('Ctrl Pts',(15.3067589266248,11.9688740228255,-325.485490289447)) ;
#27593 = CARTESIAN_POINT('Ctrl Pts',(15.6612775639348,11.4921968623271,-325.492430264243)) ;
#27594 = CARTESIAN_POINT('Ctrl Pts',(15.7347966678068,11.3913290474519,-325.493889231992)) ;
#27595 = CARTESIAN_POINT('Ctrl Pts',(16.0188763503328,10.9935753474814,-325.499615163043)) ;
#27596 = CARTESIAN_POINT('Ctrl Pts',(16.222047524525,10.6915046346124,-325.503903694146)) ;
#27597 = CARTESIAN_POINT('Ctrl Pts',(16.4703263920015,10.2989839564173,-325.50949683315)) ;
#27598 = CARTESIAN_POINT('Ctrl Pts',(16.523381616473,10.2136468467653,-325.510714125339)) ;
#27599 = CARTESIAN_POINT('Ctrl Pts',(16.6105731091213,10.0709453947153,-325.512754828303)) ;
#27600 = CARTESIAN_POINT('Ctrl Pts',(16.645080146972,10.0138098177995,-325.513573303581)) ;
#27601 = CARTESIAN_POINT('Ctrl Pts',(16.7193601196066,9.8893747573778,-325.5153597214)) ;
#27602 = CARTESIAN_POINT('Ctrl Pts',(16.7590225866423,9.82201088478792,-325.516329048357)) ;
#27603 = CARTESIAN_POINT('Ctrl Pts',(16.8798520113859,9.61392794712047,-325.519327842514)) ;
#27604 = CARTESIAN_POINT('Ctrl Pts',(16.9596611716917,9.47242879616766,-325.521373453081)) ;
#27605 = CARTESIAN_POINT('Ctrl Pts',(17.0991234205372,9.21775271055658,-325.525055666434)) ;
#27606 = CARTESIAN_POINT('Ctrl Pts',(17.1594511820689,9.10495589591066,-325.526686692969)) ;
#27607 = CARTESIAN_POINT('Ctrl Pts',(17.4681559887362,8.51379302888635,-325.535221679839)) ;
#27608 = CARTESIAN_POINT('Ctrl Pts',(17.6976576210753,8.02583708176584,-325.542214977713)) ;
#27609 = CARTESIAN_POINT('Ctrl Pts',(18.0757390442214,7.12662492662806,-325.554745917007)) ;
#27610 = CARTESIAN_POINT('Ctrl Pts',(18.2313002038026,6.71869179542986,-325.560305374599)) ;
#27611 = CARTESIAN_POINT('Ctrl Pts',(18.4261308783734,6.15102633449882,-325.567826863017)) ;
#27612 = CARTESIAN_POINT('Ctrl Pts',(18.4773141747127,5.99552208808988,-325.569865970646)) ;
#27613 = CARTESIAN_POINT('Ctrl Pts',(18.5641060972116,5.72015891252125,-325.573438999226)) ;
#27614 = CARTESIAN_POINT('Ctrl Pts',(18.6005345804788,5.60056841232328,-325.574978346069)) ;
#27615 = CARTESIAN_POINT('Ctrl Pts',(18.6751297821451,5.34692228588037,-325.57821753599)) ;
#27616 = CARTESIAN_POINT('Ctrl Pts',(18.7130132387495,5.2127906059857,-325.57991539965)) ;
#27617 = CARTESIAN_POINT('Ctrl Pts',(18.8152065044151,4.83548292998529,-325.584651387391)) ;
#27618 = CARTESIAN_POINT('Ctrl Pts',(18.876241449477,4.59144857723551,-325.587667894214)) ;
#27619 = CARTESIAN_POINT('Ctrl Pts',(19.0090923937612,4.01274840202132,-325.594730464643)) ;
#27620 = CARTESIAN_POINT('Ctrl Pts',(19.0768366527529,3.6772336271874,-325.598753748592)) ;
#27621 = CARTESIAN_POINT('Ctrl Pts',(19.2500629795013,2.68480841869195,-325.61054389156)) ;
#27622 = CARTESIAN_POINT('Ctrl Pts',(19.3307073497453,2.0240721052377,-325.618240613138)) ;
#27623 = CARTESIAN_POINT('Ctrl Pts',(19.3854783679516,1.24398464233931,-325.62762311095)) ;
#27624 = CARTESIAN_POINT('Ctrl Pts',(19.3926083448609,1.12739117805713,-325.629033641919)) ;
#27625 = CARTESIAN_POINT('Ctrl Pts',(19.401950651708,0.948088526546092,-325.631219699773)) ;
#27626 = CARTESIAN_POINT('Ctrl Pts',(19.4049115071287,0.885420993089332,-325.631986911533)) ;
#27627 = CARTESIAN_POINT('Ctrl Pts',(19.4105351865448,0.752764370559301,-325.633618628765)) ;
#27628 = CARTESIAN_POINT('Ctrl Pts',(19.4131231744416,0.68277303308811,-325.634484093655)) ;
#27629 = CARTESIAN_POINT('Ctrl Pts',(19.419094737144,0.493566636258129,-325.636834553257)) ;
#27630 = CARTESIAN_POINT('Ctrl Pts',(19.4217590336872,0.374331950196478,-325.638327410027)) ;
#27631 = CARTESIAN_POINT('Ctrl Pts',(19.428644258307,-0.149949519781678,-325.644931770118)) ;
#27632 = CARTESIAN_POINT('Ctrl Pts',(19.4212930891236,-0.555046297710654,
-325.650138132174)) ;
#27633 = CARTESIAN_POINT('Ctrl Pts',(19.3646787539922,-1.69966175390807,-325.664913171771)) ;
#27634 = CARTESIAN_POINT('Ctrl Pts',(19.2857620517131,-2.43701128522958,-325.674486892313)) ;
#27635 = CARTESIAN_POINT('Ctrl Pts',(19.1360113345374,-3.34291954851933,-325.686018013787)) ;
#27636 = CARTESIAN_POINT('Ctrl Pts',(19.1047120465276,-3.51738804445568,-325.688229549931)) ;
#27637 = CARTESIAN_POINT('Ctrl Pts',(19.0470022281513,-3.81553630322163,-325.691992275192)) ;
#27638 = CARTESIAN_POINT('Ctrl Pts',(19.0217636568214,-3.93943125257594,-325.693550962383)) ;
#27639 = CARTESIAN_POINT('Ctrl Pts',(18.9670698464512,-4.19513100999603,-325.696758116407)) ;
#27640 = CARTESIAN_POINT('Ctrl Pts',(18.9374459906652,-4.32689289913894,-325.698405376862)) ;
#27641 = CARTESIAN_POINT('Ctrl Pts',(18.8543442335556,-4.67930230128461,-325.702798349683)) ;
#27642 = CARTESIAN_POINT('Ctrl Pts',(18.7983680964116,-4.89933910485499,-325.705527560862)) ;
#27643 = CARTESIAN_POINT('Ctrl Pts',(18.6973591209794,-5.26913867199483,-325.710100354237)) ;
#27644 = CARTESIAN_POINT('Ctrl Pts',(18.654351624084,-5.41943041233557,-325.711954919475)) ;
#27645 = CARTESIAN_POINT('Ctrl Pts',(18.45512619462,-6.08514566439696,-325.720163986161)) ;
#27646 = CARTESIAN_POINT('Ctrl Pts',(18.2793264852936,-6.59446007216371,-325.726422210917)) ;
#27647 = CARTESIAN_POINT('Ctrl Pts',(17.9527051869881,-7.42680484279685,-325.736888857779)) ;
#27648 = CARTESIAN_POINT('Ctrl Pts',(17.8137553333078,-7.75417136742226,-325.741071215078)) ;
#27649 = CARTESIAN_POINT('Ctrl Pts',(17.6174632413621,-8.18347001519694,-325.746735194471)) ;
#27650 = CARTESIAN_POINT('Ctrl Pts',(17.5680754081074,-8.28896368351932,-325.748141832945)) ;
#27651 = CARTESIAN_POINT('Ctrl Pts',(17.4906565081747,-8.45053185472246,-325.750323267103)) ;
#27652 = CARTESIAN_POINT('Ctrl Pts',(17.4632978043589,-8.50692561974942,-325.751089802715)) ;
#27653 = CARTESIAN_POINT('Ctrl Pts',(17.4047603248558,-8.62611490128409,-325.752721730465)) ;
#27654 = CARTESIAN_POINT('Ctrl Pts',(17.3735135753857,-8.68887600771602,-325.753588095619)) ;
#27655 = CARTESIAN_POINT('Ctrl Pts',(17.2880361791306,-8.85825822880064,-325.755943956954)) ;
#27656 = CARTESIAN_POINT('Ctrl Pts',(17.2331593446905,-8.96454977765163,-325.757441374456)) ;
#27657 = CARTESIAN_POINT('Ctrl Pts',(16.9866755808574,-9.43133850274607,-325.764090807529)) ;
#27658 = CARTESIAN_POINT('Ctrl Pts',(16.7847135299939,-9.7862497425443,-325.769339068751)) ;
#27659 = CARTESIAN_POINT('Ctrl Pts',(16.1885418630482,-10.7610938883815,-325.784072138248)) ;
#27660 = CARTESIAN_POINT('Ctrl Pts',(15.7701363047459,-11.3654229387726,-325.793560286702)) ;
#27661 = CARTESIAN_POINT('Ctrl Pts',(15.2088176358446,-12.0852934644555,-325.80502637145)) ;
#27662 = CARTESIAN_POINT('Ctrl Pts',(15.0971840980272,-12.2244625422872,-325.807252691013)) ;
#27663 = CARTESIAN_POINT('Ctrl Pts',(14.9030748808706,-12.4597357151092,-325.811032337506)) ;
#27664 = CARTESIAN_POINT('Ctrl Pts',(14.8215475466529,-12.5566071598604,-325.812593339994)) ;
#27665 = CARTESIAN_POINT('Ctrl Pts',(14.651362637607,-12.7548552668303,-325.815798294029)) ;
#27666 = CARTESIAN_POINT('Ctrl Pts',(14.562586080773,-12.8561209824293,-325.817441112519)) ;
#27667 = CARTESIAN_POINT('Ctrl Pts',(14.4698035249581,-12.9597619825596,-325.819129065824)) ;
#27668 = CARTESIAN_POINT('Ctrl Pts',(14.4668422771126,-12.9630675082959,-325.819182908441)) ;
#27669 = CARTESIAN_POINT('Ctrl Pts',(14.4608152749881,-12.9697905789233,-325.819292432702)) ;
#27670 = CARTESIAN_POINT('Ctrl Pts',(14.4577494413635,-12.9732080523367,-325.819348113678)) ;
#27671 = CARTESIAN_POINT('Ctrl Pts',(14.4514825751406,-12.9801887244908,-325.819461865476)) ;
#27672 = CARTESIAN_POINT('Ctrl Pts',(14.448281435609,-12.9837518268191,-325.8195199354)) ;
#27673 = CARTESIAN_POINT('Ctrl Pts',(14.4417095754615,-12.9910613475353,-325.819639079928)) ;
#27674 = CARTESIAN_POINT('Ctrl Pts',(14.4383387141463,-12.9948076389376,-325.819700153353)) ;
#27675 = CARTESIAN_POINT('Ctrl Pts',(14.4313880826089,-13.0025263546757,-325.819826005797)) ;
#27676 = CARTESIAN_POINT('Ctrl Pts',(14.4278081291634,-13.0064986134991,-325.819890783282)) ;
#27677 = CARTESIAN_POINT('Ctrl Pts',(14.4203935131201,-13.0147189242541,-325.820024857457)) ;
#27678 = CARTESIAN_POINT('Ctrl Pts',(14.4165586125585,-13.0189667608933,-325.82009415216)) ;
#27679 = CARTESIAN_POINT('Ctrl Pts',(14.4085799305906,-13.027796726638,-325.820238220004)) ;
#27680 = CARTESIAN_POINT('Ctrl Pts',(14.4044358392714,-13.0323785748856,-325.820312990563)) ;
#27681 = CARTESIAN_POINT('Ctrl Pts',(14.3957738308613,-13.0419464069701,-325.820469156361)) ;
#27682 = CARTESIAN_POINT('Ctrl Pts',(14.3912555075687,-13.0469320220301,-325.820550548223)) ;
#27683 = CARTESIAN_POINT('Ctrl Pts',(14.3817662435857,-13.0573917529893,-325.820721342493)) ;
#27684 = CARTESIAN_POINT('Ctrl Pts',(14.3767947657148,-13.0628653801797,-325.820810740447)) ;
#27685 = CARTESIAN_POINT('Ctrl Pts',(14.2640103450764,-13.1868993344541,-325.822836992038)) ;
#27686 = CARTESIAN_POINT('Ctrl Pts',(14.1547374110561,-13.3041239505955,-325.82476165103)) ;
#27687 = CARTESIAN_POINT('Ctrl Pts',(13.8544910749184,-13.6183320566801,-325.829952337115)) ;
#27688 = CARTESIAN_POINT('Ctrl Pts',(13.6607748072115,-13.8126435895157,-325.833196813771)) ;
#27689 = CARTESIAN_POINT('Ctrl Pts',(13.1895220767711,-14.2657304810727,-325.840881878341)) ;
#27690 = CARTESIAN_POINT('Ctrl Pts',(12.9083916190039,-14.5206055189928,-325.845302310798)) ;
#27691 = CARTESIAN_POINT('Ctrl Pts',(12.5720206005074,-14.8080688385666,-325.850474450753)) ;
#27692 = CARTESIAN_POINT('Ctrl Pts',(12.5238634319281,-14.8488197997022,-325.851212278184)) ;
#27693 = CARTESIAN_POINT('Ctrl Pts',(12.2054641656248,-15.1156008662701,-325.856075350132)) ;
#27694 = CARTESIAN_POINT('Ctrl Pts',(11.9293145861188,-15.3344774134465,-325.860220217427)) ;
#27695 = CARTESIAN_POINT('Ctrl Pts',(11.5543412503041,-15.6154197745484,-325.865842453247)) ;
#27696 = CARTESIAN_POINT('Ctrl Pts',(11.4606923136646,-15.6842809238087,-325.867246241772)) ;
#27697 = CARTESIAN_POINT('Ctrl Pts',(11.3156366418857,-15.7889491678306,-325.869424291835)) ;
#27698 = CARTESIAN_POINT('Ctrl Pts',(11.2646652580572,-15.8253551318289,-325.870190333527)) ;
#27699 = CARTESIAN_POINT('Ctrl Pts',(11.1748671158137,-15.8888391823217,-325.87154189618)) ;
#27700 = CARTESIAN_POINT('Ctrl Pts',(11.1361158001846,-15.9160230740663,-325.872125810804)) ;
#27701 = CARTESIAN_POINT('Ctrl Pts',(11.0242953808099,-15.9938563442287,-325.873812183941)) ;
#27702 = CARTESIAN_POINT('Ctrl Pts',(10.9509774343343,-16.0441460541718,-325.874919645981)) ;
#27703 = CARTESIAN_POINT('Ctrl Pts',(10.6701742449084,-16.2339309708988,-325.879163759012)) ;
#27704 = CARTESIAN_POINT('Ctrl Pts',(10.4603482909359,-16.3699189494769,-325.882340204739)) ;
#27705 = CARTESIAN_POINT('Ctrl Pts',(9.79546693794153,-16.7828234519928,-325.892355523447)) ;
#27706 = CARTESIAN_POINT('Ctrl Pts',(9.33161089234153,-17.0450982505494,-325.899265475006)) ;
#27707 = CARTESIAN_POINT('Ctrl Pts',(8.46310830199521,-17.4900789825837,-325.911804980233)) ;
#27708 = CARTESIAN_POINT('Ctrl Pts',(8.06185063370071,-17.6786207355001,-325.917452404765)) ;
#27709 = CARTESIAN_POINT('Ctrl Pts',(7.50356713705214,-17.9179817995941,-325.925065656562)) ;
#27710 = CARTESIAN_POINT('Ctrl Pts',(7.35182462698565,-17.9807749085239,-325.927111294524)) ;
#27711 = CARTESIAN_POINT('Ctrl Pts',(7.0831364085428,-18.0879917999438,-325.930691643099)) ;
#27712 = CARTESIAN_POINT('Ctrl Pts',(6.96652369054359,-18.1332241053185,-325.932231853424)) ;
#27713 = CARTESIAN_POINT('Ctrl Pts',(6.73160129575199,-18.2217462930249,-325.935307787692)) ;
#27714 = CARTESIAN_POINT('Ctrl Pts',(6.61329102871445,-18.2650178151972,-325.93684332686)) ;
#27715 = CARTESIAN_POINT('Ctrl Pts',(6.41931972932114,-18.3338303186149,-325.939339680997)) ;
#27716 = CARTESIAN_POINT('Ctrl Pts',(6.34390740606857,-18.3600609686849,-325.940305031052)) ;
#27717 = CARTESIAN_POINT('Ctrl Pts',(5.92267179432441,-18.5036741050653,-325.945669505806)) ;
#27718 = CARTESIAN_POINT('Ctrl Pts',(5.57375305682515,-18.6117509719516,-325.950007494172)) ;
#27719 = CARTESIAN_POINT('Ctrl Pts',(4.49543333633788,-18.9127131301077,-325.963188830535)) ;
#27720 = CARTESIAN_POINT('Ctrl Pts',(3.75767969512353,-19.073003814011,-325.971875202038)) ;
#27721 = CARTESIAN_POINT('Ctrl Pts',(2.85505859821545,-19.214699006034,-325.982755057587)) ;
#27722 = CARTESIAN_POINT('Ctrl Pts',(2.69733833914895,-19.2374734110603,-325.984666544533)) ;
#27723 = CARTESIAN_POINT('Ctrl Pts',(2.46144089807498,-19.2685783081648,-325.98755124297)) ;
#27724 = CARTESIAN_POINT('Ctrl Pts',(2.38346422449059,-19.2783790704129,-325.988508985337)) ;
#27725 = CARTESIAN_POINT('Ctrl Pts',(2.24174403935766,-19.2953186692742,-325.990258857179)) ;
#27726 = CARTESIAN_POINT('Ctrl Pts',(2.17802067853291,-19.302615490631,-325.991049179009)) ;
#27727 = CARTESIAN_POINT('Ctrl Pts',(2.0468631093184,-19.3169763041413,-325.992682559518)) ;
#27728 = CARTESIAN_POINT('Ctrl Pts',(1.97942570103222,-19.3240031050592,-325.993525983449)) ;
#27729 = CARTESIAN_POINT('Ctrl Pts',(1.81484186417456,-19.3402817152584,-325.995591989879)) ;
#27730 = CARTESIAN_POINT('Ctrl Pts',(1.71765986544026,-19.3491548231964,-325.996818349495)) ;
#27731 = CARTESIAN_POINT('Ctrl Pts',(1.08162212538613,-19.4023980696581,-326.004878017996)) ;
#27732 = CARTESIAN_POINT('Ctrl Pts',(0.541181276773599,-19.4249859516044,
-326.011875812873)) ;
#27733 = CARTESIAN_POINT('Ctrl Pts',(0.000504484077160222,-19.4249999934491,
-326.018849108403)) ;
#27734 = CARTESIAN_POINT('Origin',(0.,0.,-328.125)) ;
#27735 = CARTESIAN_POINT('',(-0.000502513484877063,-19.4249999935001,-327.731156847152)) ;
#27736 = CARTESIAN_POINT('',(-0.000462715177408183,-19.4249999944889,-327.51849135163)) ;
#27737 = CARTESIAN_POINT('',(-2.37887640734373E-15,-19.425,-328.125)) ;
#27738 = CARTESIAN_POINT('Ctrl Pts',(-0.000501968905967098,-19.4249999935142,
-327.73119906165)) ;
#27739 = CARTESIAN_POINT('Ctrl Pts',(0.566668136750594,-19.4250146499753,
-327.723882407847)) ;
#27740 = CARTESIAN_POINT('Ctrl Pts',(1.13356879912891,-19.4001890010975,-327.716592548354)) ;
#27741 = CARTESIAN_POINT('Ctrl Pts',(1.84523395830898,-19.3377199424505,-327.707595627717)) ;
#27742 = CARTESIAN_POINT('Ctrl Pts',(1.99174650924835,-19.3231790047744,-327.705751083962)) ;
#27743 = CARTESIAN_POINT('Ctrl Pts',(2.25516570455525,-19.2940076164169,-327.70244934237)) ;
#27744 = CARTESIAN_POINT('Ctrl Pts',(2.37213141584046,-19.2799765259975,-327.700988468624)) ;
#27745 = CARTESIAN_POINT('Ctrl Pts',(2.6003936402977,-19.2504857630597,-327.698147630888)) ;
#27746 = CARTESIAN_POINT('Ctrl Pts',(2.71169801284079,-19.2351226437466,-327.696767100085)) ;
#27747 = CARTESIAN_POINT('Ctrl Pts',(2.9687411230739,-19.1973680670589,-327.693589343242)) ;
#27748 = CARTESIAN_POINT('Ctrl Pts',(3.11437077429207,-19.1742811941801,-327.691796736925)) ;
#27749 = CARTESIAN_POINT('Ctrl Pts',(3.55675817356864,-19.0989759523275,-327.686371990605)) ;
#27750 = CARTESIAN_POINT('Ctrl Pts',(3.85257645060155,-19.0415090353982,-327.682773666884)) ;
#27751 = CARTESIAN_POINT('Ctrl Pts',(4.82290285328572,-18.8294710535858,-327.671016525914)) ;
#27752 = CARTESIAN_POINT('Ctrl Pts',(5.49049028565787,-18.6457471262594,-327.663017810499)) ;
#27753 = CARTESIAN_POINT('Ctrl Pts',(6.41461400812271,-18.3374760815901,-327.651556986669)) ;
#27754 = CARTESIAN_POINT('Ctrl Pts',(6.68040060684859,-18.2423284981641,-327.648211192618)) ;
#27755 = CARTESIAN_POINT('Ctrl Pts',(7.01872674118403,-18.1128269188619,-327.643841877151)) ;
#27756 = CARTESIAN_POINT('Ctrl Pts',(7.093257555339,-18.0837695543178,-327.642872347894)) ;
#27757 = CARTESIAN_POINT('Ctrl Pts',(7.2242356374264,-18.0317707596647,-327.64115457026)) ;
#27758 = CARTESIAN_POINT('Ctrl Pts',(7.28075849345368,-18.0090225451982,-327.640408661855)) ;
#27759 = CARTESIAN_POINT('Ctrl Pts',(7.3955320375174,-17.9622020747321,-327.638883819505)) ;
#27760 = CARTESIAN_POINT('Ctrl Pts',(7.45377443851947,-17.9381114975901,-327.63810468766)) ;
#27761 = CARTESIAN_POINT('Ctrl Pts',(7.6211400281547,-17.867928862847,-327.635851475496)) ;
#27762 = CARTESIAN_POINT('Ctrl Pts',(7.7299601166779,-17.8211215614828,-327.634368888616)) ;
#27763 = CARTESIAN_POINT('Ctrl Pts',(8.18918203480905,-17.6185966819481,-327.628048015504)) ;
#27764 = CARTESIAN_POINT('Ctrl Pts',(8.53536031698953,-17.453517549193,-327.62312499457)) ;
#27765 = CARTESIAN_POINT('Ctrl Pts',(9.33590965349982,-17.0422493520048,-327.611526415786)) ;
#27766 = CARTESIAN_POINT('Ctrl Pts',(9.78579654832614,-16.7879617468808,-327.60484362662)) ;
#27767 = CARTESIAN_POINT('Ctrl Pts',(10.4149830250614,-16.3984351314029,-327.595404233212)) ;
#27768 = CARTESIAN_POINT('Ctrl Pts',(10.602910950418,-16.2775558907902,-327.592571372946)) ;
#27769 = CARTESIAN_POINT('Ctrl Pts',(10.9350401002305,-16.055730636703,-327.587547080553)) ;
#27770 = CARTESIAN_POINT('Ctrl Pts',(11.0800337011288,-15.9560158430098,-327.585347413003)) ;
#27771 = CARTESIAN_POINT('Ctrl Pts',(11.3161706080924,-15.7888491355471,-327.581755525946)) ;
#27772 = CARTESIAN_POINT('Ctrl Pts',(11.4081136007697,-15.722544907361,-327.580354533691)) ;
#27773 = CARTESIAN_POINT('Ctrl Pts',(11.6006406115458,-15.5811270469345,-327.577415492209)) ;
#27774 = CARTESIAN_POINT('Ctrl Pts',(11.7010875480931,-15.5058354463931,-327.575878957593)) ;
#27775 = CARTESIAN_POINT('Ctrl Pts',(11.9434078426385,-15.3205048272493,-327.572163486772)) ;
#27776 = CARTESIAN_POINT('Ctrl Pts',(12.0844991050308,-15.2094622051041,-327.569992821382)) ;
#27777 = CARTESIAN_POINT('Ctrl Pts',(12.8551378581171,-14.5854550079223,-327.558083539922)) ;
#27778 = CARTESIAN_POINT('Ctrl Pts',(13.4535768455231,-14.0353601777939,-327.54867443968)) ;
#27779 = CARTESIAN_POINT('Ctrl Pts',(14.1895957964404,-13.2683451562877,-327.536222005879)) ;
#27780 = CARTESIAN_POINT('Ctrl Pts',(14.3598373262853,-13.0839093436941,-327.533269964119)) ;
#27781 = CARTESIAN_POINT('Ctrl Pts',(14.5799589030939,-12.8359618934182,-327.52932490935)) ;
#27782 = CARTESIAN_POINT('Ctrl Pts',(14.6330852422614,-12.7753644027369,-327.528362527469)) ;
#27783 = CARTESIAN_POINT('Ctrl Pts',(14.7628832766829,-12.6254409669097,-327.525983724717)) ;
#27784 = CARTESIAN_POINT('Ctrl Pts',(14.8391229738793,-12.5357453530125,-327.524562459972)) ;
#27785 = CARTESIAN_POINT('Ctrl Pts',(14.9592222454539,-12.391818190619,-327.522280367687)) ;
#27786 = CARTESIAN_POINT('Ctrl Pts',(15.003613266523,-12.338033765723,-327.521427232539)) ;
#27787 = CARTESIAN_POINT('Ctrl Pts',(15.0875519420893,-12.235210257274,-327.519794435575)) ;
#27788 = CARTESIAN_POINT('Ctrl Pts',(15.1271525341827,-12.1862155668352,-327.519015695774)) ;
#27789 = CARTESIAN_POINT('Ctrl Pts',(15.2404203624299,-12.0446753192894,-327.516765046904)) ;
#27790 = CARTESIAN_POINT('Ctrl Pts',(15.3134814938793,-11.9516484572463,-327.515284660065)) ;
#27791 = CARTESIAN_POINT('Ctrl Pts',(15.6181868016405,-11.5562937080068,-327.508998597108)) ;
#27792 = CARTESIAN_POINT('Ctrl Pts',(15.8417625852091,-11.2478549323534,-327.504109321328)) ;
#27793 = CARTESIAN_POINT('Ctrl Pts',(16.3738776064693,-10.4663977676742,-327.49192626063)) ;
#27794 = CARTESIAN_POINT('Ctrl Pts',(16.6711357885627,-9.9861195722908,-327.484621259946)) ;
#27795 = CARTESIAN_POINT('Ctrl Pts',(17.0142455631378,-9.3736318898535,-327.475688157411)) ;
#27796 = CARTESIAN_POINT('Ctrl Pts',(17.0801629081835,-9.25297584412378,-327.473945670853)) ;
#27797 = CARTESIAN_POINT('Ctrl Pts',(17.2425369969996,-8.94811567775496,-327.469588249399)) ;
#27798 = CARTESIAN_POINT('Ctrl Pts',(17.3373274873748,-8.76304353983245,-327.466984085452)) ;
#27799 = CARTESIAN_POINT('Ctrl Pts',(17.4872367995477,-8.45839791387403,-327.462765861239)) ;
#27800 = CARTESIAN_POINT('Ctrl Pts',(17.5441433330496,-8.33972307201492,-327.461139271792)) ;
#27801 = CARTESIAN_POINT('Ctrl Pts',(17.6535542601527,-8.10547701976162,-327.457960821823)) ;
#27802 = CARTESIAN_POINT('Ctrl Pts',(17.706140601229,-7.98995123845244,-327.456408436128)) ;
#27803 = CARTESIAN_POINT('Ctrl Pts',(17.8339515520026,-7.70170661881636,-327.452571530115)) ;
#27804 = CARTESIAN_POINT('Ctrl Pts',(17.9078030513009,-7.5283931105201,-327.450296706834)) ;
#27805 = CARTESIAN_POINT('Ctrl Pts',(18.1654080331232,-6.89860105018048,-327.442136301733)) ;
#27806 = CARTESIAN_POINT('Ctrl Pts',(18.3343220985767,-6.43625511553254,-327.436349081787)) ;
#27807 = CARTESIAN_POINT('Ctrl Pts',(18.6253515271782,-5.53480932736616,-327.425271254274)) ;
#27808 = CARTESIAN_POINT('Ctrl Pts',(18.7499342377481,-5.09684204644661,-327.419978412791)) ;
#27809 = CARTESIAN_POINT('Ctrl Pts',(18.8983832634481,-4.49541130894042,-327.412663834606)) ;
#27810 = CARTESIAN_POINT('Ctrl Pts',(18.9357254740428,-4.33542540780872,-327.41071328482)) ;
#27811 = CARTESIAN_POINT('Ctrl Pts',(18.9978026811942,-4.05334805885832,-327.407253258793)) ;
#27812 = CARTESIAN_POINT('Ctrl Pts',(19.0234010809841,-3.93145627492153,-327.405751266031)) ;
#27813 = CARTESIAN_POINT('Ctrl Pts',(19.0617662007668,-3.73961868242635,-327.403371383068)) ;
#27814 = CARTESIAN_POINT('Ctrl Pts',(19.0753241990219,-3.66983450157261,-327.402502345583)) ;
#27815 = CARTESIAN_POINT('Ctrl Pts',(19.0999833063529,-3.53908220189843,-327.400866636083)) ;
#27816 = CARTESIAN_POINT('Ctrl Pts',(19.1111763305201,-3.47813231291543,-327.400101136104)) ;
#27817 = CARTESIAN_POINT('Ctrl Pts',(19.1418411427795,-3.30653365463806,-327.397938504287)) ;
#27818 = CARTESIAN_POINT('Ctrl Pts',(19.1606449130957,-3.19576807749216,-327.39653386666)) ;
#27819 = CARTESIAN_POINT('Ctrl Pts',(19.286925947311,-2.41067886167694,-327.386531538265)) ;
#27820 = CARTESIAN_POINT('Ctrl Pts',(19.3597420745788,-1.73126322544248,-327.377651447447)) ;
#27821 = CARTESIAN_POINT('Ctrl Pts',(19.4148425161922,-0.712838622452622,
-327.364522424441)) ;
#27822 = CARTESIAN_POINT('Ctrl Pts',(19.42428891004,-0.375832155735956,-327.360204052552)) ;
#27823 = CARTESIAN_POINT('Ctrl Pts',(19.4251963094077,0.07903115954985,-327.354437981209)) ;
#27824 = CARTESIAN_POINT('Ctrl Pts',(19.4243600257351,0.196812623540111,-327.352950449001)) ;
#27825 = CARTESIAN_POINT('Ctrl Pts',(19.4194294443807,0.501231877525742,-327.349121166749)) ;
#27826 = CARTESIAN_POINT('Ctrl Pts',(19.4137158078641,0.687831393476101,-327.346788983854)) ;
#27827 = CARTESIAN_POINT('Ctrl Pts',(19.3995557331429,1.0021108076904,-327.342887386928)) ;
#27828 = CARTESIAN_POINT('Ctrl Pts',(19.3925358278598,1.12984199358938,-327.341309001475)) ;
#27829 = CARTESIAN_POINT('Ctrl Pts',(19.3767082182586,1.37382428624687,-327.338307730169)) ;
#27830 = CARTESIAN_POINT('Ctrl Pts',(19.368114647542,1.49008375024846,-327.336883527271)) ;
#27831 = CARTESIAN_POINT('Ctrl Pts',(19.3422757059462,1.80149214885456,-327.333083614171)) ;
#27832 = CARTESIAN_POINT('Ctrl Pts',(19.3231238091603,1.99646935095384,-327.330720241292)) ;
#27833 = CARTESIAN_POINT('Ctrl Pts',(19.2443915751077,2.69000067636812,-327.322359060484)) ;
#27834 = CARTESIAN_POINT('Ctrl Pts',(19.1684366109644,3.18649491617604,-327.316462024864)) ;
#27835 = CARTESIAN_POINT('Ctrl Pts',(18.9907444286586,4.10759646295215,-327.305496826173)) ;
#27836 = CARTESIAN_POINT('Ctrl Pts',(18.8937667770527,4.53280251966119,-327.300423520097)) ;
#27837 = CARTESIAN_POINT('Ctrl Pts',(18.7415271704949,5.10995809640824,-327.29337233588)) ;
#27838 = CARTESIAN_POINT('Ctrl Pts',(18.698559115876,5.26501655375615,-327.291461057915)) ;
#27839 = CARTESIAN_POINT('Ctrl Pts',(18.6194378857411,5.53734702931232,-327.288062545053)) ;
#27840 = CARTESIAN_POINT('Ctrl Pts',(18.5840905040147,5.65484388600805,-327.286582431093)) ;
#27841 = CARTESIAN_POINT('Ctrl Pts',(18.526618928557,5.83952199731724,-327.284229109465)) ;
#27842 = CARTESIAN_POINT('Ctrl Pts',(18.5052369211638,5.90693089168744,-327.283364435468)) ;
#27843 = CARTESIAN_POINT('Ctrl Pts',(18.4643518369039,6.03342418287602,-327.281729934414)) ;
#27844 = CARTESIAN_POINT('Ctrl Pts',(18.4449320547868,6.09253458020453,-327.280961215013)) ;
#27845 = CARTESIAN_POINT('Ctrl Pts',(18.389184867434,6.25950950045119,-327.278776868335)) ;
#27846 = CARTESIAN_POINT('Ctrl Pts',(18.3521929909856,6.36714941247892,-327.277353498364)) ;
#27847 = CARTESIAN_POINT('Ctrl Pts',(18.0883996877346,7.1133398326548,-327.267395163338)) ;
#27848 = CARTESIAN_POINT('Ctrl Pts',(17.8292663515923,7.73996567300107,-327.258584083656)) ;
#27849 = CARTESIAN_POINT('Ctrl Pts',(17.3704649851364,8.70340522876972,-327.24484673261)) ;
#27850 = CARTESIAN_POINT('Ctrl Pts',(17.1924720892921,9.0499293308566,-327.239860933761)) ;
#27851 = CARTESIAN_POINT('Ctrl Pts',(16.8974944480936,9.58404965050726,-327.232151044033)) ;
#27852 = CARTESIAN_POINT('Ctrl Pts',(16.7875221512588,9.77539905052449,-327.229383295466)) ;
#27853 = CARTESIAN_POINT('Ctrl Pts',(16.6056208213326,10.0797774255433,-327.224974057793)) ;
#27854 = CARTESIAN_POINT('Ctrl Pts',(16.5357416159832,10.1940082930281,-327.223317724807)) ;
#27855 = CARTESIAN_POINT('Ctrl Pts',(16.3980620560127,10.4139305993688,-327.220125541971)) ;
#27856 = CARTESIAN_POINT('Ctrl Pts',(16.3304069663555,10.519705227921,-327.218588690707)) ;
#27857 = CARTESIAN_POINT('Ctrl Pts',(16.1634276993092,10.775274057909,-327.214870678222)) ;
#27858 = CARTESIAN_POINT('Ctrl Pts',(16.0630408596398,10.9243601408166,-327.212697817307)) ;
#27859 = CARTESIAN_POINT('Ctrl Pts',(15.5488179095441,11.6656248629819,-327.201863019034)) ;
#27860 = CARTESIAN_POINT('Ctrl Pts',(15.1042417609244,12.2357845352804,-327.19345142729)) ;
#27861 = CARTESIAN_POINT('Ctrl Pts',(14.3554395815758,13.0929294497839,-327.180149104946)) ;
#27862 = CARTESIAN_POINT('Ctrl Pts',(14.0719557399637,13.3971454884869,-327.17527742804)) ;
#27863 = CARTESIAN_POINT('Ctrl Pts',(13.6940323823287,13.7774674517206,-327.168849297126)) ;
#27864 = CARTESIAN_POINT('Ctrl Pts',(13.6083412286594,13.8621131582323,-327.167395769415)) ;
#27865 = CARTESIAN_POINT('Ctrl Pts',(13.4714177347975,13.9948728942528,-327.165074674288)) ;
#27866 = CARTESIAN_POINT('Ctrl Pts',(13.4207019244223,14.0435153348156,-327.164215257509)) ;
#27867 = CARTESIAN_POINT('Ctrl Pts',(13.3178041141762,14.1411400028828,-327.162470919151)) ;
#27868 = CARTESIAN_POINT('Ctrl Pts',(13.265613128547,14.190111180402,-327.161585864764)) ;
#27869 = CARTESIAN_POINT('Ctrl Pts',(13.1200916214667,14.3251505712105,-327.159118846724)) ;
#27870 = CARTESIAN_POINT('Ctrl Pts',(13.0261862103204,14.4105938733694,-327.15752771661)) ;
#27871 = CARTESIAN_POINT('Ctrl Pts',(12.3337919302591,15.0282961089767,-327.145823757275)) ;
#27872 = CARTESIAN_POINT('Ctrl Pts',(11.7037292927899,15.5240082809409,-327.135359251772)) ;
#27873 = CARTESIAN_POINT('Ctrl Pts',(10.8293324702579,16.1283859429093,-327.121745459268)) ;
#27874 = CARTESIAN_POINT('Ctrl Pts',(10.6108042556443,16.2729870727067,-327.118409705786)) ;
#27875 = CARTESIAN_POINT('Ctrl Pts',(10.211730515983,16.5255985746628,-327.112449543477)) ;
#27876 = CARTESIAN_POINT('Ctrl Pts',(10.0322283665869,16.6351808706627,-327.109814984559)) ;
#27877 = CARTESIAN_POINT('Ctrl Pts',(9.73718496395107,16.8087860144633,-327.105561264456)) ;
#27878 = CARTESIAN_POINT('Ctrl Pts',(9.62270792342425,16.8745829749602,-327.103929154302)) ;
#27879 = CARTESIAN_POINT('Ctrl Pts',(9.39713888430339,17.0011894379518,-327.100748611605)) ;
#27880 = CARTESIAN_POINT('Ctrl Pts',(9.28610534312561,17.062089822802,-327.099199560947)) ;
#27881 = CARTESIAN_POINT('Ctrl Pts',(9.01001857262122,17.2100263064322,-327.0953874077)) ;
#27882 = CARTESIAN_POINT('Ctrl Pts',(8.84429162752622,17.2957782681095,-327.093133708241)) ;
#27883 = CARTESIAN_POINT('Ctrl Pts',(8.07672098442936,17.6790243274644,-327.082841772652)) ;
#27884 = CARTESIAN_POINT('Ctrl Pts',(7.46094337387107,17.9475805610331,-327.075011020913)) ;
#27885 = CARTESIAN_POINT('Ctrl Pts',(6.40336234459716,18.3449649055034,-327.061812816211)) ;
#27886 = CARTESIAN_POINT('Ctrl Pts',(5.9686501663427,18.4909707634193,-327.05645088225)) ;
#27887 = CARTESIAN_POINT('Ctrl Pts',(5.41733637926735,18.6546697616887,-327.049550617234)) ;
#27888 = CARTESIAN_POINT('Ctrl Pts',(5.30519381248115,18.6868712179656,-327.048141705936)) ;
#27889 = CARTESIAN_POINT('Ctrl Pts',(5.12576375440439,18.736648740995,-327.04587451163)) ;
#27890 = CARTESIAN_POINT('Ctrl Pts',(5.05866008843115,18.754877184836,-327.045023747396)) ;
#27891 = CARTESIAN_POINT('Ctrl Pts',(4.93039816095674,18.7889805768839,-327.043390971663)) ;
#27892 = CARTESIAN_POINT('Ctrl Pts',(4.8692575155475,18.8049181965821,-327.042609840406)) ;
#27893 = CARTESIAN_POINT('Ctrl Pts',(4.69241927466212,18.8500946156265,-327.040343583932)) ;
#27894 = CARTESIAN_POINT('Ctrl Pts',(4.57652868663224,18.8785659091093,-327.038849805177)) ;
#27895 = CARTESIAN_POINT('Ctrl Pts',(4.03386528017089,19.0065935692324,-327.031826728494)) ;
#27896 = CARTESIAN_POINT('Ctrl Pts',(3.6040647352598,19.092757385174,-327.026185436129)) ;
#27897 = CARTESIAN_POINT('Ctrl Pts',(2.69977606802398,19.2424183953177,-327.014363128814)) ;
#27898 = CARTESIAN_POINT('Ctrl Pts',(2.22510743500877,19.3030659437785,-327.00818508451)) ;
#27899 = CARTESIAN_POINT('Ctrl Pts',(1.60273133153192,19.3593221410527,-327.000221521302)) ;
#27900 = CARTESIAN_POINT('Ctrl Pts',(1.45663307614301,19.3708626969991,-326.998361523632)) ;
#27901 = CARTESIAN_POINT('Ctrl Pts',(1.09365063585451,19.3954055449964,-326.993766406868)) ;
#27902 = CARTESIAN_POINT('Ctrl Pts',(0.876652267063747,19.4064244261836,-326.991042526894)) ;
#27903 = CARTESIAN_POINT('Ctrl Pts',(0.526301933439306,19.4183263272582,-326.986684497529)) ;
#27904 = CARTESIAN_POINT('Ctrl Pts',(0.393046185891204,19.4214805262244,-326.985036138449)) ;
#27905 = CARTESIAN_POINT('Ctrl Pts',(0.133900628525554,19.4249463618657,-326.981848184261)) ;
#27906 = CARTESIAN_POINT('Ctrl Pts',(0.00801934370696578,19.4254062062541,
-326.980307710019)) ;
#27907 = CARTESIAN_POINT('Ctrl Pts',(-0.29967727195655,19.4235392795287,-326.976561024763)) ;
#27908 = CARTESIAN_POINT('Ctrl Pts',(-0.481472646147607,19.4198833373667,
-326.974363447667)) ;
#27909 = CARTESIAN_POINT('Ctrl Pts',(-1.36054938609427,19.3898532211094,-326.963803470521)) ;
#27910 = CARTESIAN_POINT('Ctrl Pts',(-2.05611948930114,19.3284731949937,-326.955670778402)) ;
#27911 = CARTESIAN_POINT('Ctrl Pts',(-3.17492987809722,19.1686571106704,-326.942465666141)) ;
#27912 = CARTESIAN_POINT('Ctrl Pts',(-3.60082334543987,19.0932360969512,-326.9374039252)) ;
#27913 = CARTESIAN_POINT('Ctrl Pts',(-4.14343126675036,18.9783441030285,-326.930756640686)) ;
#27914 = CARTESIAN_POINT('Ctrl Pts',(-4.2627777868619,18.9518941804842,-326.929281917382)) ;
#27915 = CARTESIAN_POINT('Ctrl Pts',(-4.45067349253324,18.908387522229,-326.926935135514)) ;
#27916 = CARTESIAN_POINT('Ctrl Pts',(-4.51939301248104,18.892080351677,-326.926071532549)) ;
#27917 = CARTESIAN_POINT('Ctrl Pts',(-4.64854275545965,18.8606880684438,-326.924437286712)) ;
#27918 = CARTESIAN_POINT('Ctrl Pts',(-4.70899235067138,18.8456863816356,-326.923667735333)) ;
#27919 = CARTESIAN_POINT('Ctrl Pts',(-4.88006651847555,18.802356657807,-326.921477815159)) ;
#27920 = CARTESIAN_POINT('Ctrl Pts',(-4.99051483571171,18.7733435149545,-326.920049642568)) ;
#27921 = CARTESIAN_POINT('Ctrl Pts',(-5.7529370018419,18.5658626955099,-326.910106871463)) ;
#27922 = CARTESIAN_POINT('Ctrl Pts',(-6.39546372125375,18.3544432212098,-326.901318015372)) ;
#27923 = CARTESIAN_POINT('Ctrl Pts',(-7.34166763172784,17.9873686779461,-326.888252264395)) ;
#27924 = CARTESIAN_POINT('Ctrl Pts',(-7.65441356199913,17.8565245566211,-326.883909308)) ;
#27925 = CARTESIAN_POINT('Ctrl Pts',(-8.1915833385204,17.6150809732716,-326.876442976331)) ;
#27926 = CARTESIAN_POINT('Ctrl Pts',(-8.41759162717479,17.5082057002107,-326.873299108966)) ;
#27927 = CARTESIAN_POINT('Ctrl Pts',(-8.76605840465014,17.3351145305557,-326.868452580306)) ;
#27928 = CARTESIAN_POINT('Ctrl Pts',(-8.88997410658565,17.2718944007576,-326.866729219479)) ;
#27929 = CARTESIAN_POINT('Ctrl Pts',(-9.12399785893963,17.1493128829453,-326.86347451004)) ;
#27930 = CARTESIAN_POINT('Ctrl Pts',(-9.23423253101261,17.0902082754343,-326.861941396621)) ;
#27931 = CARTESIAN_POINT('Ctrl Pts',(-9.48787302276198,16.951043123397,-326.858412961664)) ;
#27932 = CARTESIAN_POINT('Ctrl Pts',(-9.63084973462912,16.8702202403512,-326.856423364099)) ;
#27933 = CARTESIAN_POINT('Ctrl Pts',(-10.162122188545,16.5609435688433,-326.849022203673)) ;
#27934 = CARTESIAN_POINT('Ctrl Pts',(-10.5434578538209,16.320817290034,-326.843696532373)) ;
#27935 = CARTESIAN_POINT('Ctrl Pts',(-11.3519267139935,15.7715567210137,-326.832236401009)) ;
#27936 = CARTESIAN_POINT('Ctrl Pts',(-11.775525302441,15.4578537960369,-326.82612416709)) ;
#27937 = CARTESIAN_POINT('Ctrl Pts',(-12.2843381111514,15.0479785374472,-326.818420678904)) ;
#27938 = CARTESIAN_POINT('Ctrl Pts',(-12.382053782604,14.9676773405857,-326.816923540845)) ;
#27939 = CARTESIAN_POINT('Ctrl Pts',(-12.6025293359435,14.7828573367772,-326.813497737258)) ;
#27940 = CARTESIAN_POINT('Ctrl Pts',(-12.7247861741752,14.6777530087043,-326.811563663347)) ;
#27941 = CARTESIAN_POINT('Ctrl Pts',(-12.904199675055,14.5195844800975,-326.808663216711)) ;
#27942 = CARTESIAN_POINT('Ctrl Pts',(-12.9623681656831,14.4676782603659,-326.80771293425)) ;
#27943 = CARTESIAN_POINT('Ctrl Pts',(-13.0698023372714,14.37064213509,-326.805937712827)) ;
#27944 = CARTESIAN_POINT('Ctrl Pts',(-13.1191506046413,14.3256056027662,-326.805114154647)) ;
#27945 = CARTESIAN_POINT('Ctrl Pts',(-13.2424598566688,14.2118988028023,-326.803036529357)) ;
#27946 = CARTESIAN_POINT('Ctrl Pts',(-13.3161198213233,14.1429050587323,-326.801777513884)) ;
#27947 = CARTESIAN_POINT('Ctrl Pts',(-13.6549543331401,13.8205412138688,-326.795909510694)) ;
#27948 = CARTESIAN_POINT('Ctrl Pts',(-13.9134567498053,13.560267609566,-326.791214313394)) ;
#27949 = CARTESIAN_POINT('Ctrl Pts',(-14.5424124808288,12.8900716781056,-326.779384787836)) ;
#27950 = CARTESIAN_POINT('Ctrl Pts',(-14.9030403284675,12.4713711967374,-326.772228808609)) ;
#27951 = CARTESIAN_POINT('Ctrl Pts',(-15.3434734675197,11.9135857595116,-326.763155982997)) ;
#27952 = CARTESIAN_POINT('Ctrl Pts',(-15.4400888892474,11.788102428551,-326.761142650473)) ;
#27953 = CARTESIAN_POINT('Ctrl Pts',(-15.6726540307524,11.4782836689256,-326.756242728018)) ;
#27954 = CARTESIAN_POINT('Ctrl Pts',(-15.8068988190968,11.2926980988616,-326.753367898429)) ;
#27955 = CARTESIAN_POINT('Ctrl Pts',(-16.015239153861,10.9936834047738,-326.748833791124)) ;
#27956 = CARTESIAN_POINT('Ctrl Pts',(-16.0914839950993,10.8817784785254,-326.747158079275)) ;
#27957 = CARTESIAN_POINT('Ctrl Pts',(-16.2365621773585,10.6639870902589,-326.743937142684)) ;
#27958 = CARTESIAN_POINT('Ctrl Pts',(-16.3055452492576,10.5582084736741,-326.742390807946)) ;
#27959 = CARTESIAN_POINT('Ctrl Pts',(-16.4682946799596,10.3032489915601,-326.738705613038)) ;
#27960 = CARTESIAN_POINT('Ctrl Pts',(-16.5610723739536,10.1534502213144,-326.736574345426)) ;
#27961 = CARTESIAN_POINT('Ctrl Pts',(-16.8572969802614,9.6603017929765,-326.729661186565)) ;
#27962 = CARTESIAN_POINT('Ctrl Pts',(-17.052203211794,9.31194172876649,-326.724940363902)) ;
#27963 = CARTESIAN_POINT('Ctrl Pts',(-17.2905594545227,8.85330747705538,-326.71887407053)) ;
#27964 = CARTESIAN_POINT('Ctrl Pts',(-17.3439265464113,8.7482976343601,-326.717494783342)) ;
#27965 = CARTESIAN_POINT('Ctrl Pts',(-17.5996876258909,8.23349908479791,-326.710772015474)) ;
#27966 = CARTESIAN_POINT('Ctrl Pts',(-17.7885307113949,7.81714051266059,-326.705458145723)) ;
#27967 = CARTESIAN_POINT('Ctrl Pts',(-18.025168735461,7.24230687357798,-326.698118428772)) ;
#27968 = CARTESIAN_POINT('Ctrl Pts',(-18.0858882867292,7.08931319371667,-326.69616421045)) ;
#27969 = CARTESIAN_POINT('Ctrl Pts',(-18.1891865200064,6.81906693505941,-326.692698447572)) ;
#27970 = CARTESIAN_POINT('Ctrl Pts',(-18.2325939537131,6.70214128267492,-326.691194420762)) ;
#27971 = CARTESIAN_POINT('Ctrl Pts',(-18.298981964423,6.51789402633894,-326.688812068452)) ;
#27972 = CARTESIAN_POINT('Ctrl Pts',(-18.322723968599,6.4508503181709,-326.68794262554)) ;
#27973 = CARTESIAN_POINT('Ctrl Pts',(-18.366454838942,6.32517185745441,-326.686306792006)) ;
#27974 = CARTESIAN_POINT('Ctrl Pts',(-18.3865324702208,6.26656892454612,-326.685541579356)) ;
#27975 = CARTESIAN_POINT('Ctrl Pts',(-18.4421916635148,6.10153948923378,-326.683380897827)) ;
#27976 = CARTESIAN_POINT('Ctrl Pts',(-18.4771318030187,5.99489931297739,-326.681977944361)) ;
#27977 = CARTESIAN_POINT('Ctrl Pts',(-18.7188400377754,5.23499359142138,-326.671947710709)) ;
#27978 = CARTESIAN_POINT('Ctrl Pts',(-18.8918391067089,4.57149274900552,-326.66303595763)) ;
#27979 = CARTESIAN_POINT('Ctrl Pts',(-19.1071108013469,3.52117451989093,-326.649235247183)) ;
#27980 = CARTESIAN_POINT('Ctrl Pts',(-19.17346007678,3.13986988593855,-326.644282771375)) ;
#27981 = CARTESIAN_POINT('Ctrl Pts',(-19.2595432977273,2.53945717945131,-326.636619493037)) ;
#27982 = CARTESIAN_POINT('Ctrl Pts',(-19.2870214234965,2.32156319290734,-326.633865593921)) ;
#27983 = CARTESIAN_POINT('Ctrl Pts',(-19.3252768256865,1.9703246796273,-326.629472520394)) ;
#27984 = CARTESIAN_POINT('Ctrl Pts',(-19.338381624878,1.83725336342452,-326.627818703396)) ;
#27985 = CARTESIAN_POINT('Ctrl Pts',(-19.3611346243423,1.57888582739337,-326.624627892762)) ;
#27986 = CARTESIAN_POINT('Ctrl Pts',(-19.3709429700669,1.45361029722551,-326.623089935928)) ;
#27987 = CARTESIAN_POINT('Ctrl Pts',(-19.3899024665977,1.17698564934953,-326.61971326631)) ;
#27988 = CARTESIAN_POINT('Ctrl Pts',(-19.398498497408,1.02560665391087,-326.617878197434)) ;
#27989 = CARTESIAN_POINT('Ctrl Pts',(-19.4263394954064,0.407556900906628,
-326.61043281078)) ;
#27990 = CARTESIAN_POINT('Ctrl Pts',(-19.4305227354124,-0.0596354283450282,
-326.604917585577)) ;
#27991 = CARTESIAN_POINT('Ctrl Pts',(-19.415876213536,-0.599789694896713,
-326.598586530051)) ;
#27992 = CARTESIAN_POINT('Ctrl Pts',(-19.4134749361234,-0.673043627672304,
-326.597728795079)) ;
#27993 = CARTESIAN_POINT('Ctrl Pts',(-19.3932242648902,-1.19975974885412,
-326.591564750028)) ;
#27994 = CARTESIAN_POINT('Ctrl Pts',(-19.3599033722535,-1.65248637867189,
-326.586287793001)) ;
#27995 = CARTESIAN_POINT('Ctrl Pts',(-19.2929932086128,-2.26670402728339,
-326.578992214636)) ;
#27996 = CARTESIAN_POINT('Ctrl Pts',(-19.2731635458214,-2.42954747176551,
-326.577044446651)) ;
#27997 = CARTESIAN_POINT('Ctrl Pts',(-19.2346711467184,-2.71542456076907,
-326.573588771862)) ;
#27998 = CARTESIAN_POINT('Ctrl Pts',(-19.2168843428523,-2.83856667193748,
-326.572088322599)) ;
#27999 = CARTESIAN_POINT('Ctrl Pts',(-19.1870816040106,-3.03176093930503,
-326.569710313521)) ;
#28000 = CARTESIAN_POINT('Ctrl Pts',(-19.1758621423515,-3.10193261591537,
-326.568841583785)) ;
#28001 = CARTESIAN_POINT('Ctrl Pts',(-19.1541357999772,-3.23319485908132,
-326.5672059672)) ;
#28002 = CARTESIAN_POINT('Ctrl Pts',(-19.1437210631545,-3.29429978671307,
-326.566440247877)) ;
#28003 = CARTESIAN_POINT('Ctrl Pts',(-19.1135902942605,-3.46611249698711,
-326.56427612866)) ;
#28004 = CARTESIAN_POINT('Ctrl Pts',(-19.0932051836634,-3.5767003703445,-326.5628702068)) ;
#28005 = CARTESIAN_POINT('Ctrl Pts',(-18.9595464781687,-4.26806130310755,
-326.554012584145)) ;
#28006 = CARTESIAN_POINT('Ctrl Pts',(-18.8207455204067,-4.84358205999536,
-326.546346905662)) ;
#28007 = CARTESIAN_POINT('Ctrl Pts',(-18.5064327021914,-5.9270873115761,-326.531798750423)) ;
#28008 = CARTESIAN_POINT('Ctrl Pts',(-18.3356934673468,-6.43589647271904,
-326.524915232974)) ;
#28009 = CARTESIAN_POINT('Ctrl Pts',(-18.075896477473,-7.11541150258877,-326.515759403713)) ;
#28010 = CARTESIAN_POINT('Ctrl Pts',(-18.005051215075,-7.29282148572337,-326.513371627074)) ;
#28011 = CARTESIAN_POINT('Ctrl Pts',(-17.8821342853836,-7.58791463495438,
-326.50940558034)) ;
#28012 = CARTESIAN_POINT('Ctrl Pts',(-17.8314892425379,-7.70617716854931,
-326.507817639474)) ;
#28013 = CARTESIAN_POINT('Ctrl Pts',(-17.7267828129144,-7.94411981083961,
-326.504625409922)) ;
#28014 = CARTESIAN_POINT('Ctrl Pts',(-17.6726750713459,-8.06377233943118,
-326.503021548296)) ;
#28015 = CARTESIAN_POINT('Ctrl Pts',(-17.5304664418693,-8.36994135480655,
-326.498919776123)) ;
#28016 = CARTESIAN_POINT('Ctrl Pts',(-17.4406003563519,-8.55561986964524,
-326.496434466652)) ;
#28017 = CARTESIAN_POINT('Ctrl Pts',(-17.2097305422998,-9.01387604164141,
-326.49029689024)) ;
#28018 = CARTESIAN_POINT('Ctrl Pts',(-17.0651926203697,-9.28461027162568,
-326.486667890694)) ;
#28019 = CARTESIAN_POINT('Ctrl Pts',(-16.633843796164,-10.0484410616153,-326.476360866207)) ;
#28020 = CARTESIAN_POINT('Ctrl Pts',(-16.3316492366972,-10.5324811302658,
-326.469752002778)) ;
#28021 = CARTESIAN_POINT('Ctrl Pts',(-15.934135843127,-11.1108605326733,-326.46148319074)) ;
#28022 = CARTESIAN_POINT('Ctrl Pts',(-15.8585774678224,-11.218441402047,-326.459928161646)) ;
#28023 = CARTESIAN_POINT('Ctrl Pts',(-15.7353624836308,-11.3901436737998,
-326.457413081492)) ;
#28024 = CARTESIAN_POINT('Ctrl Pts',(-15.6883921876064,-11.4547525487921,
-326.456459008982)) ;
#28025 = CARTESIAN_POINT('Ctrl Pts',(-15.5716603185519,-11.6132554557697,
-326.454097302849)) ;
#28026 = CARTESIAN_POINT('Ctrl Pts',(-15.5014466314936,-11.7068125306977,
-326.452684849241)) ;
#28027 = CARTESIAN_POINT('Ctrl Pts',(-15.3881181419605,-11.855011100751,-326.450413385241)) ;
#28028 = CARTESIAN_POINT('Ctrl Pts',(-15.3455472122291,-11.9100650252527,
-326.449561943308)) ;
#28029 = CARTESIAN_POINT('Ctrl Pts',(-15.263796771605,-12.0146210261364,-326.447929174773)) ;
#28030 = CARTESIAN_POINT('Ctrl Pts',(-15.2246700122831,-12.0641631824353,
-326.447148740501)) ;
#28031 = CARTESIAN_POINT('Ctrl Pts',(-15.1110754485364,-12.2065634681421,
-326.444887025995)) ;
#28032 = CARTESIAN_POINT('Ctrl Pts',(-15.0359948066638,-12.2989289380986,
-326.443397143485)) ;
#28033 = CARTESIAN_POINT('Ctrl Pts',(-14.7079796367397,-12.6949654957752,
-326.436920168873)) ;
#28034 = CARTESIAN_POINT('Ctrl Pts',(-14.4466595437442,-12.9915680756276,
-326.431842963322)) ;
#28035 = CARTESIAN_POINT('Ctrl Pts',(-13.8293412900612,-13.6505591957493,
-326.420203443125)) ;
#28036 = CARTESIAN_POINT('Ctrl Pts',(-13.4678107290303,-14.0073738668294,
-326.413637108092)) ;
#28037 = CARTESIAN_POINT('Ctrl Pts',(-12.9289486446662,-14.4990364906767,
-326.404334248841)) ;
#28038 = CARTESIAN_POINT('Ctrl Pts',(-12.7626346650623,-14.645645388478,-326.401524013453)) ;
#28039 = CARTESIAN_POINT('Ctrl Pts',(-12.4515504324741,-14.9105482166596,
-326.396384851544)) ;
#28040 = CARTESIAN_POINT('Ctrl Pts',(-12.3075117723127,-15.029661021551,-326.394049827619)) ;
#28041 = CARTESIAN_POINT('Ctrl Pts',(-12.0620015696288,-15.2267894256519,
-326.390144942639)) ;
#28042 = CARTESIAN_POINT('Ctrl Pts',(-11.9614374063831,-15.3059143243124,
-326.388566074749)) ;
#28043 = CARTESIAN_POINT('Ctrl Pts',(-11.7553471741115,-15.4647965503637,
-326.385371662671)) ;
#28044 = CARTESIAN_POINT('Ctrl Pts',(-11.6497734566204,-15.5444812712713,
-326.383756759582)) ;
#28045 = CARTESIAN_POINT('Ctrl Pts',(-11.3732227603759,-15.7488157138312,
-326.379580508997)) ;
#28046 = CARTESIAN_POINT('Ctrl Pts',(-11.2010083494869,-15.8717612288388,
-326.37703272424)) ;
#28047 = CARTESIAN_POINT('Ctrl Pts',(-10.7850066413038,-16.1586054898234,
-326.370993066476)) ;
#28048 = CARTESIAN_POINT('Ctrl Pts',(-10.539442647618,-16.3198360496331,-326.367519784772)) ;
#28049 = CARTESIAN_POINT('Ctrl Pts',(-9.80464189680152,-16.7787818732795,
-326.357339156697)) ;
#28050 = CARTESIAN_POINT('Ctrl Pts',(-9.30579190813018,-17.0605028990844,
-326.350704330877)) ;
#28051 = CARTESIAN_POINT('Ctrl Pts',(-8.67779433068673,-17.3794090092136,
-326.342406119453)) ;
#28052 = CARTESIAN_POINT('Ctrl Pts',(-8.55975720793982,-17.437847586399,-326.340848218291)) ;
#28053 = CARTESIAN_POINT('Ctrl Pts',(-8.29193777083849,-17.5670667657182,
-326.337309469636)) ;
#28054 = CARTESIAN_POINT('Ctrl Pts',(-8.14182597524522,-17.6371408222875,
-326.335323272179)) ;
#28055 = CARTESIAN_POINT('Ctrl Pts',(-7.91908482008568,-17.7376694523077,
-326.332360689482)) ;
#28056 = CARTESIAN_POINT('Ctrl Pts',(-7.84713698323759,-17.7696162910916,
-326.331401390081)) ;
#28057 = CARTESIAN_POINT('Ctrl Pts',(-7.7139676181522,-17.8277806724376,-326.329619852116)) ;
#28058 = CARTESIAN_POINT('Ctrl Pts',(-7.6528017566646,-17.8541223630844,-326.328799125861)) ;
#28059 = CARTESIAN_POINT('Ctrl Pts',(-7.50001859569355,-17.9189905935569,
-326.326743670764)) ;
#28060 = CARTESIAN_POINT('Ctrl Pts',(-7.40823883802229,-17.9571295063478,
-326.32550422923)) ;
#28061 = CARTESIAN_POINT('Ctrl Pts',(-6.98812127312395,-18.127939537327,-326.319816112918)) ;
#28062 = CARTESIAN_POINT('Ctrl Pts',(-6.65648651980135,-18.2523208701311,
-326.315286610653)) ;
#28063 = CARTESIAN_POINT('Ctrl Pts',(-5.78858960379139,-18.5510283946736,
-326.303478920906)) ;
#28064 = CARTESIAN_POINT('Ctrl Pts',(-5.24780573871246,-18.7111988137845,
-326.2961721002)) ;
#28065 = CARTESIAN_POINT('Ctrl Pts',(-4.54557802093626,-18.8863428392721,
-326.286930803986)) ;
#28066 = CARTESIAN_POINT('Ctrl Pts',(-4.38986001658318,-18.923143356745,-326.284896188374)) ;
#28067 = CARTESIAN_POINT('Ctrl Pts',(-4.00862152712661,-19.0082815552744,
-326.27995443038)) ;
#28068 = CARTESIAN_POINT('Ctrl Pts',(-3.78266041922966,-19.0545347533834,
-326.277059112407)) ;
#28069 = CARTESIAN_POINT('Ctrl Pts',(-3.42252949552614,-19.1215932735807,
-326.272501140098)) ;
#28070 = CARTESIAN_POINT('Ctrl Pts',(-3.28887318854987,-19.1450346220235,
-326.270821740463)) ;
#28071 = CARTESIAN_POINT('Ctrl Pts',(-3.03049355255374,-19.1875650131771,
-326.26759848037)) ;
#28072 = CARTESIAN_POINT('Ctrl Pts',(-2.90580818969529,-19.206843080534,-326.266053456598)) ;
#28073 = CARTESIAN_POINT('Ctrl Pts',(-2.60736587899296,-19.2500137118308,
-326.262379239882)) ;
#28074 = CARTESIAN_POINT('Ctrl Pts',(-2.4334557366044,-19.2727703777324,-326.26025751371)) ;
#28075 = CARTESIAN_POINT('Ctrl Pts',(-1.5092198318398,-19.380999890506,-326.24907341693)) ;
#28076 = CARTESIAN_POINT('Ctrl Pts',(-0.754693881584735,-19.4250183650223,
-326.240291315249)) ;
#28077 = CARTESIAN_POINT('Ctrl Pts',(0.000472547765781872,-19.4249999942522,
-326.231461493639)) ;
#28078 = CARTESIAN_POINT('Ctrl Pts',(0.000504483642990022,-19.4249999934491,
-326.018849108409)) ;
#28079 = CARTESIAN_POINT('Ctrl Pts',(-0.417183116006538,-19.4250108411485,
-326.024236169794)) ;
#28080 = CARTESIAN_POINT('Ctrl Pts',(-0.834763081159949,-19.4115496475603,
-326.029607004352)) ;
#28081 = CARTESIAN_POINT('Ctrl Pts',(-1.46262225600774,-19.37101143102,-326.037594245163)) ;
#28082 = CARTESIAN_POINT('Ctrl Pts',(-1.67342392998112,-19.3539401746368,
-326.040261445561)) ;
#28083 = CARTESIAN_POINT('Ctrl Pts',(-2.00934202281247,-19.3212073505849,
-326.044484909349)) ;
#28084 = CARTESIAN_POINT('Ctrl Pts',(-2.1346572109552,-19.3077639173627,-326.046054557209)) ;
#28085 = CARTESIAN_POINT('Ctrl Pts',(-2.37660880868619,-19.2794237285403,
-326.049073501275)) ;
#28086 = CARTESIAN_POINT('Ctrl Pts',(-2.49325832363575,-19.2646856113831,
-326.050523746003)) ;
#28087 = CARTESIAN_POINT('Ctrl Pts',(-2.74063320141473,-19.2311464933607,
-326.053588413026)) ;
#28088 = CARTESIAN_POINT('Ctrl Pts',(-2.87131523223212,-19.2120695055519,
-326.055200957389)) ;
#28089 = CARTESIAN_POINT('Ctrl Pts',(-3.20971610912804,-19.1591397853971,
-326.059361341599)) ;
#28090 = CARTESIAN_POINT('Ctrl Pts',(-3.41709751942014,-19.1232413456134,
-326.061895825569)) ;
#28091 = CARTESIAN_POINT('Ctrl Pts',(-4.43296558334321,-18.9303382748923,
-326.074256759928)) ;
#28092 = CARTESIAN_POINT('Ctrl Pts',(-5.23148311653603,-18.7253964223069,
-326.083763950563)) ;
#28093 = CARTESIAN_POINT('Ctrl Pts',(-6.29996291227972,-18.3774637432828,
-326.096969733408)) ;
#28094 = CARTESIAN_POINT('Ctrl Pts',(-6.5831561979217,-18.2779309573443,-326.100522725282)) ;
#28095 = CARTESIAN_POINT('Ctrl Pts',(-6.93978497935403,-18.1432242064827,
-326.10511947458)) ;
#28096 = CARTESIAN_POINT('Ctrl Pts',(-7.015461151484,-18.1140968579063,-326.106102037768)) ;
#28097 = CARTESIAN_POINT('Ctrl Pts',(-7.14746080771023,-18.0623396353363,
-326.107830053798)) ;
#28098 = CARTESIAN_POINT('Ctrl Pts',(-7.20386478530247,-18.039917994591,-326.108572992721)) ;
#28099 = CARTESIAN_POINT('Ctrl Pts',(-7.31830365745087,-17.9938040955344,
-326.110090444645)) ;
#28100 = CARTESIAN_POINT('Ctrl Pts',(-7.3763308009585,-17.9700945505292,-326.110865155662)) ;
#28101 = CARTESIAN_POINT('Ctrl Pts',(-7.54187651551435,-17.9015166082095,
-326.11308934351)) ;
#28102 = CARTESIAN_POINT('Ctrl Pts',(-7.64910749150483,-17.8559612671348,
-326.114547002543)) ;
#28103 = CARTESIAN_POINT('Ctrl Pts',(-8.08222157450199,-17.6673422943036,
-326.120494175031)) ;
#28104 = CARTESIAN_POINT('Ctrl Pts',(-8.40455377545699,-17.5162999629904,
-326.125056632679)) ;
#28105 = CARTESIAN_POINT('Ctrl Pts',(-9.20353286995009,-17.1147707058398,
-326.136572019043)) ;
#28106 = CARTESIAN_POINT('Ctrl Pts',(-9.67425787485637,-16.8531637977963,
-326.143542170827)) ;
#28107 = CARTESIAN_POINT('Ctrl Pts',(-10.3276486622673,-16.4536342705895,
-326.153316185075)) ;
#28108 = CARTESIAN_POINT('Ctrl Pts',(-10.5196878017921,-16.331520945544,-326.156202766444)) ;
#28109 = CARTESIAN_POINT('Ctrl Pts',(-10.8579377110256,-16.1079934731872,
-326.161304940683)) ;
#28110 = CARTESIAN_POINT('Ctrl Pts',(-11.0049842453181,-16.0078913964803,
-326.16352925462)) ;
#28111 = CARTESIAN_POINT('Ctrl Pts',(-11.2447509485099,-15.839804673661,-326.167165523729)) ;
#28112 = CARTESIAN_POINT('Ctrl Pts',(-11.3382791873913,-15.7729915076253,
-326.16858639451)) ;
#28113 = CARTESIAN_POINT('Ctrl Pts',(-11.5336552200955,-15.6307862109798,
-326.171559879923)) ;
#28114 = CARTESIAN_POINT('Ctrl Pts',(-11.6353694769942,-15.5552196221202,
-326.173111009631)) ;
#28115 = CARTESIAN_POINT('Ctrl Pts',(-11.8790195454502,-15.3704776120871,
-326.176835205948)) ;
#28116 = CARTESIAN_POINT('Ctrl Pts',(-12.0201993369405,-15.2603242237746,
-326.179000231612)) ;
#28117 = CARTESIAN_POINT('Ctrl Pts',(-12.7952140340315,-14.6382021115376,
-326.190937187967)) ;
#28118 = CARTESIAN_POINT('Ctrl Pts',(-13.3978713126674,-14.08870134432,-326.200376696002)) ;
#28119 = CARTESIAN_POINT('Ctrl Pts',(-14.1380236654869,-13.3232658099767,
-326.212850090392)) ;
#28120 = CARTESIAN_POINT('Ctrl Pts',(-14.3083214038202,-13.1402078870671,
-326.215790940702)) ;
#28121 = CARTESIAN_POINT('Ctrl Pts',(-14.5860165191591,-12.8299042025996,
-326.220745961123)) ;
#28122 = CARTESIAN_POINT('Ctrl Pts',(-14.6953966316696,-12.7044731268499,
-326.222741107501)) ;
#28123 = CARTESIAN_POINT('Ctrl Pts',(-14.8542065809904,-12.5175632287752,
-326.225714342843)) ;
#28124 = CARTESIAN_POINT('Ctrl Pts',(-14.9048954885932,-12.457163914408,-326.226675172374)) ;
#28125 = CARTESIAN_POINT('Ctrl Pts',(-14.9976940020526,-12.3452108249675,
-326.22845781827)) ;
#28126 = CARTESIAN_POINT('Ctrl Pts',(-15.0399089794738,-12.2937461152344,
-326.229278100201)) ;
#28127 = CARTESIAN_POINT('Ctrl Pts',(-15.1443370911326,-12.1650938045637,
-326.231329965454)) ;
#28128 = CARTESIAN_POINT('Ctrl Pts',(-15.2062253921845,-12.087645034796,-326.232566223194)) ;
#28129 = CARTESIAN_POINT('Ctrl Pts',(-15.4689639182021,-11.7536353174374,
-326.237895926575)) ;
#28130 = CARTESIAN_POINT('Ctrl Pts',(-15.6639343056643,-11.4925170967891,
-326.242057051588)) ;
#28131 = CARTESIAN_POINT('Ctrl Pts',(-15.8970461667046,-11.1633578027091,
-326.247240465853)) ;
#28132 = CARTESIAN_POINT('Ctrl Pts',(-15.9414691710518,-11.099828598737,-326.248238153613)) ;
#28133 = CARTESIAN_POINT('Ctrl Pts',(-16.0674169511324,-10.917395365414,-326.251093920234)) ;
#28134 = CARTESIAN_POINT('Ctrl Pts',(-16.1479998992553,-10.7978473915341,
-326.252954143089)) ;
#28135 = CARTESIAN_POINT('Ctrl Pts',(-16.5318296622806,-10.2145132881092,
-326.26196337989)) ;
#28136 = CARTESIAN_POINT('Ctrl Pts',(-16.81646896069,-9.73879091162881,-326.269097377645)) ;
#28137 = CARTESIAN_POINT('Ctrl Pts',(-17.1841508641447,-9.05996996571856,
-326.278848902605)) ;
#28138 = CARTESIAN_POINT('Ctrl Pts',(-17.284690113923,-8.86665577359058,-326.281580700346)) ;
#28139 = CARTESIAN_POINT('Ctrl Pts',(-17.4415088068861,-8.55232081375976,
-326.285947973971)) ;
#28140 = CARTESIAN_POINT('Ctrl Pts',(-17.499830257207,-8.43234023204501,-326.28759777327)) ;
#28141 = CARTESIAN_POINT('Ctrl Pts',(-17.6107478825292,-8.19804942612475,
-326.290786465122)) ;
#28142 = CARTESIAN_POINT('Ctrl Pts',(-17.6634784320572,-8.08381006107575,
-326.292326259148)) ;
#28143 = CARTESIAN_POINT('Ctrl Pts',(-17.7776100228906,-7.83009752777707,
-326.295713865107)) ;
#28144 = CARTESIAN_POINT('Ctrl Pts',(-17.8384872601975,-7.69039776402468,
-326.297557938864)) ;
#28145 = CARTESIAN_POINT('Ctrl Pts',(-18.0831141308431,-7.11049522523312,
-326.305131029254)) ;
#28146 = CARTESIAN_POINT('Ctrl Pts',(-18.2522623338474,-6.66431392536628,
-326.310760411905)) ;
#28147 = CARTESIAN_POINT('Ctrl Pts',(-18.564810536716,-5.73835461150738,-326.322206576312)) ;
#28148 = CARTESIAN_POINT('Ctrl Pts',(-18.706434490215,-5.25834682397881,-326.328014663097)) ;
#28149 = CARTESIAN_POINT('Ctrl Pts',(-18.8715498810197,-4.60702642197433,
-326.335940856829)) ;
#28150 = CARTESIAN_POINT('Ctrl Pts',(-18.9115221644071,-4.44009196565381,
-326.337976839763)) ;
#28151 = CARTESIAN_POINT('Ctrl Pts',(-18.9775461497973,-4.14727444332013,
-326.341570055708)) ;
#28152 = CARTESIAN_POINT('Ctrl Pts',(-19.0045705749389,-4.0216216084666,-326.343118989666)) ;
#28153 = CARTESIAN_POINT('Ctrl Pts',(-19.0447612838984,-3.8252920324257,-326.345555829049)) ;
#28154 = CARTESIAN_POINT('Ctrl Pts',(-19.0587856063218,-3.75479462686017,
-326.346434182434)) ;
#28155 = CARTESIAN_POINT('Ctrl Pts',(-19.0840812370409,-3.62384459931966,
-326.34807318371)) ;
#28156 = CARTESIAN_POINT('Ctrl Pts',(-19.0954573907817,-3.56341316168039,
-326.348832524501)) ;
#28157 = CARTESIAN_POINT('Ctrl Pts',(-19.1262882817015,-3.39524764038206,
-326.350952824574)) ;
#28158 = CARTESIAN_POINT('Ctrl Pts',(-19.1451194963724,-3.2874016173381,-326.35232083144)) ;
#28159 = CARTESIAN_POINT('Ctrl Pts',(-19.2617534728501,-2.58442001629184,
-326.361278917417)) ;
#28160 = CARTESIAN_POINT('Ctrl Pts',(-19.3327054174368,-1.98516349694068,
-326.369094774385)) ;
#28161 = CARTESIAN_POINT('Ctrl Pts',(-19.4135551854647,-0.852942967973674,
-326.383731202071)) ;
#28162 = CARTESIAN_POINT('Ctrl Pts',(-19.4296324368513,-0.320971838339124,
-326.390555701397)) ;
#28163 = CARTESIAN_POINT('Ctrl Pts',(-19.4217853942311,0.40143836211972,-326.399647433405)) ;
#28164 = CARTESIAN_POINT('Ctrl Pts',(-19.4169157293098,0.591848276379656,
-326.402028042702)) ;
#28165 = CARTESIAN_POINT('Ctrl Pts',(-19.4040704711969,0.91060412856428,-326.405985768708)) ;
#28166 = CARTESIAN_POINT('Ctrl Pts',(-19.3976192930046,1.03899785641799,-326.407572465259)) ;
#28167 = CARTESIAN_POINT('Ctrl Pts',(-19.3819955857502,1.29851752842469,-326.410764897464)) ;
#28168 = CARTESIAN_POINT('Ctrl Pts',(-19.3727656510467,1.42963342915828,-326.412370177779)) ;
#28169 = CARTESIAN_POINT('Ctrl Pts',(-19.3455785415224,1.76693127132444,-326.416481552516)) ;
#28170 = CARTESIAN_POINT('Ctrl Pts',(-19.3256557537582,1.97293819067365,-326.418974923173)) ;
#28171 = CARTESIAN_POINT('Ctrl Pts',(-19.2682214071699,2.48181069053854,-326.425099669427)) ;
#28172 = CARTESIAN_POINT('Ctrl Pts',(-19.2268575651396,2.78418553543426,-326.428708397974)) ;
#28173 = CARTESIAN_POINT('Ctrl Pts',(-19.0877464440495,3.64886263065718,-326.438998951925)) ;
#28174 = CARTESIAN_POINT('Ctrl Pts',(-18.9723227875187,4.20799586502152,-326.445611176658)) ;
#28175 = CARTESIAN_POINT('Ctrl Pts',(-18.8002227631502,4.88871551045755,-326.453883795848)) ;
#28176 = CARTESIAN_POINT('Ctrl Pts',(-18.7666992383657,5.01586631932116,-326.45543919765)) ;
#28177 = CARTESIAN_POINT('Ctrl Pts',(-18.7107365703249,5.2197073280047,-326.457954813923)) ;
#28178 = CARTESIAN_POINT('Ctrl Pts',(-18.6891107449705,5.29661657489869,-326.458909047071)) ;
#28179 = CARTESIAN_POINT('Ctrl Pts',(-18.6346501320464,5.48581126088675,-326.461271084028)) ;
#28180 = CARTESIAN_POINT('Ctrl Pts',(-18.601274289553,5.59793760944688,-326.462683708287)) ;
#28181 = CARTESIAN_POINT('Ctrl Pts',(-18.5464308537617,5.77627657972418,-326.464955378113)) ;
#28182 = CARTESIAN_POINT('Ctrl Pts',(-18.5256166996999,5.84268726129053,-326.465806852828)) ;
#28183 = CARTESIAN_POINT('Ctrl Pts',(-18.4852433312548,5.96911961220802,-326.467439621567)) ;
#28184 = CARTESIAN_POINT('Ctrl Pts',(-18.4657475535596,6.0291605748689,-326.468220022683)) ;
#28185 = CARTESIAN_POINT('Ctrl Pts',(-18.4086522976568,6.20212141369821,-326.470481520566)) ;
#28186 = CARTESIAN_POINT('Ctrl Pts',(-18.3703073048129,6.31479207182117,-326.471971217166)) ;
#28187 = CARTESIAN_POINT('Ctrl Pts',(-18.1757514643359,6.86969049614925,-326.479377466814)) ;
#28188 = CARTESIAN_POINT('Ctrl Pts',(-18.0045956924264,7.30651227905421,-326.485423242565)) ;
#28189 = CARTESIAN_POINT('Ctrl Pts',(-17.6351801819628,8.15728368714465,-326.497389157054)) ;
#28190 = CARTESIAN_POINT('Ctrl Pts',(-17.4377276249001,8.57126092051048,-326.503305230595)) ;
#28191 = CARTESIAN_POINT('Ctrl Pts',(-17.1597128363458,9.1046874695533,-326.510966440903)) ;
#28192 = CARTESIAN_POINT('Ctrl Pts',(-17.0922149949562,9.23077814535845,-326.512780626114)) ;
#28193 = CARTESIAN_POINT('Ctrl Pts',(-16.9204235871593,9.54335050121665,-326.517283503009)) ;
#28194 = CARTESIAN_POINT('Ctrl Pts',(-16.8144340916416,9.72887863851595,-326.519961131176)) ;
#28195 = CARTESIAN_POINT('Ctrl Pts',(-16.6377193158365,10.0266900924194,-326.524265151485)) ;
#28196 = CARTESIAN_POINT('Ctrl Pts',(-16.5688664539945,10.1400632507185,-326.525905095414)) ;
#28197 = CARTESIAN_POINT('Ctrl Pts',(-16.4322203865016,10.359956460082,-326.529088993722)) ;
#28198 = CARTESIAN_POINT('Ctrl Pts',(-16.3645390768141,10.4665383741401,-326.530633694216)) ;
#28199 = CARTESIAN_POINT('Ctrl Pts',(-16.211803027728,10.7019576948073,-326.534049881169)) ;
#28200 = CARTESIAN_POINT('Ctrl Pts',(-16.1262417074583,10.8304563333017,-326.535917383032)) ;
#28201 = CARTESIAN_POINT('Ctrl Pts',(-15.7603824333162,11.3659661551318,-326.543717928671)) ;
#28202 = CARTESIAN_POINT('Ctrl Pts',(-15.4661370481975,11.76322435966,-326.549543464933)) ;
#28203 = CARTESIAN_POINT('Ctrl Pts',(-15.0656645521474,12.2628599185116,-326.557038305064)) ;
#28204 = CARTESIAN_POINT('Ctrl Pts',(-14.9729816596672,12.3758556071624,-326.558745437124)) ;
#28205 = CARTESIAN_POINT('Ctrl Pts',(-14.6373134279127,12.7757996065916,-326.564843734692)) ;
#28206 = CARTESIAN_POINT('Ctrl Pts',(-14.3872834467677,13.0567252514564,-326.569230499365)) ;
#28207 = CARTESIAN_POINT('Ctrl Pts',(-13.9826765814699,13.4855851310261,-326.57620740386)) ;
#28208 = CARTESIAN_POINT('Ctrl Pts',(-13.8335419401867,13.6385251329558,-326.578755097916)) ;
#28209 = CARTESIAN_POINT('Ctrl Pts',(-13.6208870077426,13.8495289998455,-326.582377559289)) ;
#28210 = CARTESIAN_POINT('Ctrl Pts',(-13.5594570123582,13.909677994085,-326.583422830523)) ;
#28211 = CARTESIAN_POINT('Ctrl Pts',(-13.450403557329,14.015048400752,-326.585278427793)) ;
#28212 = CARTESIAN_POINT('Ctrl Pts',(-13.4029464126472,14.0604397147933,-326.586086058009)) ;
#28213 = CARTESIAN_POINT('Ctrl Pts',(-13.2919196433035,14.1655605502076,-326.587975791306)) ;
#28214 = CARTESIAN_POINT('Ctrl Pts',(-13.2281762027638,14.2251041411655,-326.589060738497)) ;
#28215 = CARTESIAN_POINT('Ctrl Pts',(-13.0036928778213,14.4319832617551,-326.592878049277)) ;
#28216 = CARTESIAN_POINT('Ctrl Pts',(-12.8408753597593,14.5770397896641,-326.595640351685)) ;
#28217 = CARTESIAN_POINT('Ctrl Pts',(-12.4854226354363,14.8831404312769,-326.601626730429)) ;
#28218 = CARTESIAN_POINT('Ctrl Pts',(-12.2920368979304,15.0432535110859,-326.604856772879)) ;
#28219 = CARTESIAN_POINT('Ctrl Pts',(-11.8013888222586,15.4337042188982,-326.612940931139)) ;
#28220 = CARTESIAN_POINT('Ctrl Pts',(-11.5004388587213,15.6592436124706,-326.617800394264)) ;
#28221 = CARTESIAN_POINT('Ctrl Pts',(-10.9654012677338,16.0364659855446,-326.626196764321)) ;
#28222 = CARTESIAN_POINT('Ctrl Pts',(-10.7342407951735,16.1921073743383,-326.629749773492)) ;
#28223 = CARTESIAN_POINT('Ctrl Pts',(-10.3152103388906,16.4613245202135,-326.636042206763)) ;
#28224 = CARTESIAN_POINT('Ctrl Pts',(-10.1286121238894,16.5767905815426,-326.638793725256)) ;
#28225 = CARTESIAN_POINT('Ctrl Pts',(-9.8252477072782,16.75747601166,-326.643184020207)) ;
#28226 = CARTESIAN_POINT('Ctrl Pts',(-9.70969460043107,16.824693923377,-326.64483740475)) ;
#28227 = CARTESIAN_POINT('Ctrl Pts',(-9.48417967702382,16.9527801429671,-326.648027983342)) ;
#28228 = CARTESIAN_POINT('Ctrl Pts',(-9.37430274110752,17.0137846138908,-326.649566133985)) ;
#28229 = CARTESIAN_POINT('Ctrl Pts',(-9.13050497006459,17.1460641694138,-326.652943963231)) ;
#28230 = CARTESIAN_POINT('Ctrl Pts',(-8.99632546631366,17.2168454048308,-326.654779987933)) ;
#28231 = CARTESIAN_POINT('Ctrl Pts',(-8.13862720077039,17.6565264678724,-326.666378870111)) ;
#28232 = CARTESIAN_POINT('Ctrl Pts',(-7.3934038179297,17.9813169280277,-326.675802315083)) ;
#28233 = CARTESIAN_POINT('Ctrl Pts',(-6.37883472138951,18.3497280544541,-326.688435679527)) ;
#28234 = CARTESIAN_POINT('Ctrl Pts',(-6.12576988629633,18.4357531722914,-326.691575097347)) ;
#28235 = CARTESIAN_POINT('Ctrl Pts',(-5.70534778763784,18.5690558471199,-326.69681806525)) ;
#28236 = CARTESIAN_POINT('Ctrl Pts',(-5.53898708887837,18.6193568710062,-326.698899779634)) ;
#28237 = CARTESIAN_POINT('Ctrl Pts',(-5.29502102269627,18.6895636533388,-326.701975830538)) ;
#28238 = CARTESIAN_POINT('Ctrl Pts',(-5.21793177330242,18.7112325935651,-326.702951187957)) ;
#28239 = CARTESIAN_POINT('Ctrl Pts',(-5.07678876141961,18.7499662566094,-326.704744824141)) ;
#28240 = CARTESIAN_POINT('Ctrl Pts',(-5.01277756209331,18.7671809239495,-326.705561360914)) ;
#28241 = CARTESIAN_POINT('Ctrl Pts',(-4.8549728558136,18.8087547158566,-326.707581380328)) ;
#28242 = CARTESIAN_POINT('Ctrl Pts',(-4.76108285627282,18.8327402517897,-326.708789196085)) ;
#28243 = CARTESIAN_POINT('Ctrl Pts',(-4.37929532780558,18.9272357411706,-326.71371914427)) ;
#28244 = CARTESIAN_POINT('Ctrl Pts',(-4.08998137092024,18.9918543633728,-326.717497169695)) ;
#28245 = CARTESIAN_POINT('Ctrl Pts',(-3.38409270725106,19.1326370003252,-326.726733920288)) ;
#28246 = CARTESIAN_POINT('Ctrl Pts',(-2.96628603633385,19.2018496334634,-326.732215253516)) ;
#28247 = CARTESIAN_POINT('Ctrl Pts',(-2.21547069081826,19.3011358853055,-326.741962961426)) ;
#28248 = CARTESIAN_POINT('Ctrl Pts',(-1.88331468709704,19.3363720294197,-326.746240436351)) ;
#28249 = CARTESIAN_POINT('Ctrl Pts',(-1.43374050038611,19.3723698468136,-326.751956792317)) ;
#28250 = CARTESIAN_POINT('Ctrl Pts',(-1.31698350369383,19.3806573621626,-326.753434844355)) ;
#28251 = CARTESIAN_POINT('Ctrl Pts',(-1.01465236074945,19.3993724137168,-326.757244160989)) ;
#28252 = CARTESIAN_POINT('Ctrl Pts',(-0.828990618031794,19.4081927073741,
-326.759565907703)) ;
#28253 = CARTESIAN_POINT('Ctrl Pts',(-0.51551396487016,19.4185787284142,-326.76345543232)) ;
#28254 = CARTESIAN_POINT('Ctrl Pts',(-0.387758458352586,19.4215498328149,
-326.765032051854)) ;
#28255 = CARTESIAN_POINT('Ctrl Pts',(-0.127468386899953,19.4250338491352,
-326.768227283868)) ;
#28256 = CARTESIAN_POINT('Ctrl Pts',(0.00506085209851253,19.4254514149154,
-326.76984519909)) ;
#28257 = CARTESIAN_POINT('Ctrl Pts',(0.350604160773705,19.4230039272076,-326.774041681859)) ;
#28258 = CARTESIAN_POINT('Ctrl Pts',(0.563585213194563,19.4179910585613,-326.776606421316)) ;
#28259 = CARTESIAN_POINT('Ctrl Pts',(1.06641434098791,19.3978762912909,-326.782620081931)) ;
#28260 = CARTESIAN_POINT('Ctrl Pts',(1.35609168051833,19.379779665416,-326.786051630194)) ;
#28261 = CARTESIAN_POINT('Ctrl Pts',(2.21643349375359,19.3066478154842,-326.796198434957)) ;
#28262 = CARTESIAN_POINT('Ctrl Pts',(2.78518184728668,19.2328361847249,-326.802840276206)) ;
#28263 = CARTESIAN_POINT('Ctrl Pts',(3.47963108027146,19.1112573385091,-326.811146429254)) ;
#28264 = CARTESIAN_POINT('Ctrl Pts',(3.60919668228023,19.0872127030689,-326.812705103974)) ;
#28265 = CARTESIAN_POINT('Ctrl Pts',(3.90112088561237,19.0299590408481,-326.816245283378)) ;
#28266 = CARTESIAN_POINT('Ctrl Pts',(4.06331934401819,18.9959869714271,-326.818232137123)) ;
#28267 = CARTESIAN_POINT('Ctrl Pts',(4.30190850520698,18.9428193966634,-326.821195501288)) ;
#28268 = CARTESIAN_POINT('Ctrl Pts',(4.37864916820153,18.9252280018726,-326.822154913167)) ;
#28269 = CARTESIAN_POINT('Ctrl Pts',(4.52009965707808,18.8918966459503,-326.823936532402)) ;
#28270 = CARTESIAN_POINT('Ctrl Pts',(4.58483943251127,18.8762895488931,-326.824757225824)) ;
#28271 = CARTESIAN_POINT('Ctrl Pts',(4.74597797907024,18.8365652969513,-326.826812416131)) ;
#28272 = CARTESIAN_POINT('Ctrl Pts',(4.84227431934409,18.8120407861977,-326.828051622884)) ;
#28273 = CARTESIAN_POINT('Ctrl Pts',(5.28051954548772,18.6968416508085,-326.833734939378)) ;
#28274 = CARTESIAN_POINT('Ctrl Pts',(5.62013976179984,18.597575180194,-326.838259710248)) ;
#28275 = CARTESIAN_POINT('Ctrl Pts',(6.14449427084479,18.4286374120117,-326.845346542195)) ;
#28276 = CARTESIAN_POINT('Ctrl Pts',(6.33119880152189,18.3653316989743,-326.847890471851)) ;
#28277 = CARTESIAN_POINT('Ctrl Pts',(6.92267888964475,18.1546874135974,-326.85599113061)) ;
#28278 = CARTESIAN_POINT('Ctrl Pts',(7.32353232626315,17.9967228539168,-326.861541019357)) ;
#28279 = CARTESIAN_POINT('Ctrl Pts',(7.84525898845189,17.7708054413704,-326.868775756652)) ;
#28280 = CARTESIAN_POINT('Ctrl Pts',(7.97112910764784,17.7147033684803,-326.870522373045)) ;
#28281 = CARTESIAN_POINT('Ctrl Pts',(8.28569430994319,17.5704656939094,-326.874888209231)) ;
#28282 = CARTESIAN_POINT('Ctrl Pts',(8.4735890077257,17.4806259738571,-326.877496640646)) ;
#28283 = CARTESIAN_POINT('Ctrl Pts',(8.77786350279586,17.3290817468366,-326.88171984838)) ;
#28284 = CARTESIAN_POINT('Ctrl Pts',(8.89512423676782,17.2691843099321,-326.883347212538)) ;
#28285 = CARTESIAN_POINT('Ctrl Pts',(9.12417182708066,17.1492336120069,-326.886525942127)) ;
#28286 = CARTESIAN_POINT('Ctrl Pts',(9.23599725188932,17.0892679720819,-326.888077845917)) ;
#28287 = CARTESIAN_POINT('Ctrl Pts',(9.51213956912431,16.93768628315,-326.891911194318)) ;
#28288 = CARTESIAN_POINT('Ctrl Pts',(9.67572832927351,16.8447706204523,-326.894182984249)) ;
#28289 = CARTESIAN_POINT('Ctrl Pts',(10.1432975643564,16.5701402892212,-326.900686451099)) ;
#28290 = CARTESIAN_POINT('Ctrl Pts',(10.4436919697828,16.3824703078355,-326.904876303068)) ;
#28291 = CARTESIAN_POINT('Ctrl Pts',(10.9263956157162,16.0622287328839,-326.911679817405)) ;
#28292 = CARTESIAN_POINT('Ctrl Pts',(11.1118249508326,15.9345115816321,-326.914311551687)) ;
#28293 = CARTESIAN_POINT('Ctrl Pts',(11.6138873146571,15.5756825500852,-326.921519803855)) ;
#28294 = CARTESIAN_POINT('Ctrl Pts',(11.9258103246577,15.3381652355206,-326.926089391126)) ;
#28295 = CARTESIAN_POINT('Ctrl Pts',(12.3138570314817,15.0236849062668,-326.931996915015)) ;
#28296 = CARTESIAN_POINT('Ctrl Pts',(12.396817733595,14.9553031799335,-326.933273495691)) ;
#28297 = CARTESIAN_POINT('Ctrl Pts',(12.532230505283,14.84178597579,-326.935382983852)) ;
#28298 = CARTESIAN_POINT('Ctrl Pts',(12.5850166949285,14.7970526513474,-326.936211844289)) ;
#28299 = CARTESIAN_POINT('Ctrl Pts',(12.7176539612149,14.6834268770724,-326.9383125494)) ;
#28300 = CARTESIAN_POINT('Ctrl Pts',(12.797185043915,14.614164431753,-326.939588802726)) ;
#28301 = CARTESIAN_POINT('Ctrl Pts',(12.9266949756125,14.4995082511701,-326.941697952982)) ;
#28302 = CARTESIAN_POINT('Ctrl Pts',(12.9770082687524,14.4544954571736,-326.942525138341)) ;
#28303 = CARTESIAN_POINT('Ctrl Pts',(13.0834603998713,14.3582542350868,-326.944292938768)) ;
#28304 = CARTESIAN_POINT('Ctrl Pts',(13.1395352190539,14.3069568714883,-326.945234554135)) ;
#28305 = CARTESIAN_POINT('Ctrl Pts',(13.3055221977264,14.1533126592461,-326.948050956018)) ;
#28306 = CARTESIAN_POINT('Ctrl Pts',(13.4145499204461,14.0500188790203,-326.949939293338)) ;
#28307 = CARTESIAN_POINT('Ctrl Pts',(13.9435881772821,13.5370315320262,-326.959268730439)) ;
#28308 = CARTESIAN_POINT('Ctrl Pts',(14.3460860275177,13.1097173707736,-326.966881115572)) ;
#28309 = CARTESIAN_POINT('Ctrl Pts',(15.0479269879425,12.2935089164111,-326.980748229276)) ;
#28310 = CARTESIAN_POINT('Ctrl Pts',(15.3530730676705,11.910231643154,-326.98701626338)) ;
#28311 = CARTESIAN_POINT('Ctrl Pts',(15.7530244135387,11.3669272550445,-326.995499113101)) ;
#28312 = CARTESIAN_POINT('Ctrl Pts',(15.8605087765957,11.2164644559859,-326.997808573495)) ;
#28313 = CARTESIAN_POINT('Ctrl Pts',(16.0385270504444,10.9595877914989,-327.001683897558)) ;
#28314 = CARTESIAN_POINT('Ctrl Pts',(16.1101897736959,10.8539716239569,-327.003258450649)) ;
#28315 = CARTESIAN_POINT('Ctrl Pts',(16.2542690027723,10.6370575408265,-327.006454546226)) ;
#28316 = CARTESIAN_POINT('Ctrl Pts',(16.3265956981309,10.5257079052748,-327.008075338598)) ;
#28317 = CARTESIAN_POINT('Ctrl Pts',(16.5127144504539,10.2326367289967,-327.01229112414)) ;
#28318 = CARTESIAN_POINT('Ctrl Pts',(16.6246495012352,10.0497573166538,-327.014872034383)) ;
#28319 = CARTESIAN_POINT('Ctrl Pts',(16.8792194207854,9.61794509212463,-327.020861112411)) ;
#28320 = CARTESIAN_POINT('Ctrl Pts',(17.0194127028395,9.36763084537578,-327.024253050164)) ;
#28321 = CARTESIAN_POINT('Ctrl Pts',(17.4232517264209,8.60756629500385,-327.034367776071)) ;
#28322 = CARTESIAN_POINT('Ctrl Pts',(17.6699057975651,8.08914863716062,-327.04101630178)) ;
#28323 = CARTESIAN_POINT('Ctrl Pts',(17.9445618546604,7.43913342215355,-327.049330020752)) ;
#28324 = CARTESIAN_POINT('Ctrl Pts',(17.9946379332251,7.31717239310941,-327.050889431504)) ;
#28325 = CARTESIAN_POINT('Ctrl Pts',(18.1048650624446,7.04073603725965,-327.054430972021)) ;
#28326 = CARTESIAN_POINT('Ctrl Pts',(18.164288078721,6.88598150726406,-327.056418449987)) ;
#28327 = CARTESIAN_POINT('Ctrl Pts',(18.249005064677,6.65662369761279,-327.059382557331)) ;
#28328 = CARTESIAN_POINT('Ctrl Pts',(18.2758377904471,6.58259659547528,-327.06034207608)) ;
#28329 = CARTESIAN_POINT('Ctrl Pts',(18.3245314776524,6.44566564471362,-327.062123772411)) ;
#28330 = CARTESIAN_POINT('Ctrl Pts',(18.346520441426,6.38280871839717,-327.06294443451)) ;
#28331 = CARTESIAN_POINT('Ctrl Pts',(18.400509248801,6.22589391674672,-327.064999372723)) ;
#28332 = CARTESIAN_POINT('Ctrl Pts',(18.4321115094623,6.13170130891736,-327.066238356017)) ;
#28333 = CARTESIAN_POINT('Ctrl Pts',(18.5725357075435,5.70226046808324,-327.071905136891)) ;
#28334 = CARTESIAN_POINT('Ctrl Pts',(18.6729431250667,5.36433138867651,-327.07641297421)) ;
#28335 = CARTESIAN_POINT('Ctrl Pts',(18.7798106867995,4.96518130934419,-327.081728324813)) ;
#28336 = CARTESIAN_POINT('Ctrl Pts',(18.7952455618037,4.90643038635758,-327.082510498498)) ;
#28337 = CARTESIAN_POINT('Ctrl Pts',(18.8309155779598,4.76801832205315,-327.084352213789)) ;
#28338 = CARTESIAN_POINT('Ctrl Pts',(18.8509212114941,4.68829923311079,-327.085412165662)) ;
#28339 = CARTESIAN_POINT('Ctrl Pts',(18.981086972907,4.15530448543709,-327.092489940947)) ;
#28340 = CARTESIAN_POINT('Ctrl Pts',(19.0753950898941,3.69831333694448,-327.098511001347)) ;
#28341 = CARTESIAN_POINT('Ctrl Pts',(19.1772426807593,3.09594157992855,-327.106293653917)) ;
#28342 = CARTESIAN_POINT('Ctrl Pts',(19.1997348651637,2.9532477496082,-327.108126448232)) ;
#28343 = CARTESIAN_POINT('Ctrl Pts',(19.2517566517433,2.5974544506631,-327.112666858757)) ;
#28344 = CARTESIAN_POINT('Ctrl Pts',(19.2793417520502,2.38409010747144,-327.115363339038)) ;
#28345 = CARTESIAN_POINT('Ctrl Pts',(19.3182263570742,2.03823918787935,-327.11968937501)) ;
#28346 = CARTESIAN_POINT('Ctrl Pts',(19.3317196393601,1.9060179465516,-327.121332749321)) ;
#28347 = CARTESIAN_POINT('Ctrl Pts',(19.3553685856004,1.64809952955765,-327.124518247665)) ;
#28348 = CARTESIAN_POINT('Ctrl Pts',(19.3656592611102,1.52242128688295,-327.126061172561)) ;
#28349 = CARTESIAN_POINT('Ctrl Pts',(19.3857736734706,1.2433887798575,-327.129467113427)) ;
#28350 = CARTESIAN_POINT('Ctrl Pts',(19.3950028745052,1.0900000722004,-327.131326233167)) ;
#28351 = CARTESIAN_POINT('Ctrl Pts',(19.4203187599284,0.565515471158907,-327.137642767645)) ;
#28352 = CARTESIAN_POINT('Ctrl Pts',(19.4275815287433,0.194075331456793,-327.142045639433)) ;
#28353 = CARTESIAN_POINT('Ctrl Pts',(19.4188878079119,-0.758129904308238,
-327.15324050368)) ;
#28354 = CARTESIAN_POINT('Ctrl Pts',(19.3875395894411,-1.33838394875235,-327.159968867587)) ;
#28355 = CARTESIAN_POINT('Ctrl Pts',(19.3171599756559,-2.04830057614149,-327.168372876977)) ;
#28356 = CARTESIAN_POINT('Ctrl Pts',(19.3027289955938,-2.18010505419259,-327.169941003362)) ;
#28357 = CARTESIAN_POINT('Ctrl Pts',(19.2671475067596,-2.47696154579646,-327.17349864906)) ;
#28358 = CARTESIAN_POINT('Ctrl Pts',(19.2452233374695,-2.64191030987806,-327.175493506102)) ;
#28359 = CARTESIAN_POINT('Ctrl Pts',(19.2097909069459,-2.88457535717359,-327.178466397096)) ;
#28360 = CARTESIAN_POINT('Ctrl Pts',(19.1979242139874,-2.96252384513382,-327.179427177242)) ;
#28361 = CARTESIAN_POINT('Ctrl Pts',(19.1751646178104,-3.10614193384714,-327.181209787227)) ;
#28362 = CARTESIAN_POINT('Ctrl Pts',(19.1644081246981,-3.17183180952745,-327.182030083349)) ;
#28363 = CARTESIAN_POINT('Ctrl Pts',(19.1367901629798,-3.33522368853037,-327.184082063747)) ;
#28364 = CARTESIAN_POINT('Ctrl Pts',(19.1195179375013,-3.43285429249027,-327.185318423672)) ;
#28365 = CARTESIAN_POINT('Ctrl Pts',(19.0420080899544,-3.85223339227551,-327.190667176932)) ;
#28366 = CARTESIAN_POINT('Ctrl Pts',(18.9743904370142,-4.17256288354558,-327.194847928542)) ;
#28367 = CARTESIAN_POINT('Ctrl Pts',(18.8810942157753,-4.56516289976145,-327.200034068147)) ;
#28368 = CARTESIAN_POINT('Ctrl Pts',(18.8630413877299,-4.63919181395662,-327.201014766755)) ;
#28369 = CARTESIAN_POINT('Ctrl Pts',(18.8102783724116,-4.85015547072424,-327.203816128341)) ;
#28370 = CARTESIAN_POINT('Ctrl Pts',(18.774509391943,-4.98682039187714,-327.205638843419)) ;
#28371 = CARTESIAN_POINT('Ctrl Pts',(18.6225570124736,-5.54257367454252,-327.213072340069)) ;
#28372 = CARTESIAN_POINT('Ctrl Pts',(18.4938059199857,-5.95809502764049,-327.218676949637)) ;
#28373 = CARTESIAN_POINT('Ctrl Pts',(18.2837437210495,-6.5633596971502,-327.226830804255)) ;
#28374 = CARTESIAN_POINT('Ctrl Pts',(18.2131849662172,-6.75669065016525,-327.229434306104)) ;
#28375 = CARTESIAN_POINT('Ctrl Pts',(18.0761830509373,-7.11432543246064,-327.234243838602)) ;
#28376 = CARTESIAN_POINT('Ctrl Pts',(18.01053751618,-7.27891190774359,-327.236454622286)) ;
#28377 = CARTESIAN_POINT('Ctrl Pts',(17.894209358965,-7.55935713985805,-327.240216487136)) ;
#28378 = CARTESIAN_POINT('Ctrl Pts',(17.8446303598341,-7.67566129532896,-327.241775057365)) ;
#28379 = CARTESIAN_POINT('Ctrl Pts',(17.7397433524522,-7.91519891632897,-327.244982329021)) ;
#28380 = CARTESIAN_POINT('Ctrl Pts',(17.6842782326749,-8.03835627128352,-327.246629820291)) ;
#28381 = CARTESIAN_POINT('Ctrl Pts',(17.5321069189807,-8.36704509027079,-327.251024339532)) ;
#28382 = CARTESIAN_POINT('Ctrl Pts',(17.4330726928829,-8.57147556109847,-327.253754844565)) ;
#28383 = CARTESIAN_POINT('Ctrl Pts',(17.2497861146696,-8.93349964869672,-327.258595143417)) ;
#28384 = CARTESIAN_POINT('Ctrl Pts',(17.166901407133,-9.09175632912777,-327.260712814534)) ;
#28385 = CARTESIAN_POINT('Ctrl Pts',(16.775653698174,-9.81435804617473,-327.270408558365)) ;
#28386 = CARTESIAN_POINT('Ctrl Pts',(16.4415688540731,-10.3643134021324,-327.27784875193)) ;
#28387 = CARTESIAN_POINT('Ctrl Pts',(15.9258105210219,-11.1254458842784,-327.288670960781)) ;
#28388 = CARTESIAN_POINT('Ctrl Pts',(15.7659326777758,-11.350874551876,-327.291948587657)) ;
#28389 = CARTESIAN_POINT('Ctrl Pts',(15.5458449519907,-11.6475745995569,-327.296406047861)) ;
#28390 = CARTESIAN_POINT('Ctrl Pts',(15.4898527694988,-11.7219345873691,-327.297535615674)) ;
#28391 = CARTESIAN_POINT('Ctrl Pts',(15.3933077424548,-11.8482507200985,-327.299478208889)) ;
#28392 = CARTESIAN_POINT('Ctrl Pts',(15.3530210190997,-11.9004081428921,-327.300287437464)) ;
#28393 = CARTESIAN_POINT('Ctrl Pts',(15.2616897803332,-12.0174148975402,-327.302119351405)) ;
#28394 = CARTESIAN_POINT('Ctrl Pts',(15.2104959819746,-12.0821458247054,-327.303144145037)) ;
#28395 = CARTESIAN_POINT('Ctrl Pts',(15.0404706456332,-12.2943374273616,-327.306538184947)) ;
#28396 = CARTESIAN_POINT('Ctrl Pts',(14.9198952264532,-12.4403864989065,-327.308929938267)) ;
#28397 = CARTESIAN_POINT('Ctrl Pts',(14.2348467673596,-13.2458759318782,-327.322382459771)) ;
#28398 = CARTESIAN_POINT('Ctrl Pts',(13.6288001022259,-13.8686665222032,-327.333731456611)) ;
#28399 = CARTESIAN_POINT('Ctrl Pts',(12.7848484682549,-14.6270071331188,-327.34813954358)) ;
#28400 = CARTESIAN_POINT('Ctrl Pts',(12.5829148230552,-14.8010791164603,-327.351496854248)) ;
#28401 = CARTESIAN_POINT('Ctrl Pts',(12.2680753927485,-15.0613776135139,-327.356589441689)) ;
#28402 = CARTESIAN_POINT('Ctrl Pts',(12.1577003724024,-15.1506135579832,-327.358349082568)) ;
#28403 = CARTESIAN_POINT('Ctrl Pts',(11.9486771657956,-15.3158494025382,-327.361633720247)) ;
#28404 = CARTESIAN_POINT('Ctrl Pts',(11.8502568530145,-15.3921259577127,-327.36316094445)) ;
#28405 = CARTESIAN_POINT('Ctrl Pts',(11.6243782033614,-15.5637330852144,-327.366622955208)) ;
#28406 = CARTESIAN_POINT('Ctrl Pts',(11.4964678627484,-15.6584540404362,-327.368552761204)) ;
#28407 = CARTESIAN_POINT('Ctrl Pts',(11.047361194786,-15.9825595979927,-327.375227595896)) ;
#28408 = CARTESIAN_POINT('Ctrl Pts',(10.7203492351549,-16.2037191385582,-327.379909129434)) ;
#28409 = CARTESIAN_POINT('Ctrl Pts',(9.89504163043827,-16.7259519144703,-327.391391715019)) ;
#28410 = CARTESIAN_POINT('Ctrl Pts',(9.38952089888908,-17.0148820705078,-327.398133363672)) ;
#28411 = CARTESIAN_POINT('Ctrl Pts',(8.75373157925027,-17.3412923698082,-327.406552383494)) ;
#28412 = CARTESIAN_POINT('Ctrl Pts',(8.63505115936703,-17.4006933494354,-327.408121946701)) ;
#28413 = CARTESIAN_POINT('Ctrl Pts',(8.36612745928314,-17.5318640565301,-327.411682245256)) ;
#28414 = CARTESIAN_POINT('Ctrl Pts',(8.21555138894398,-17.6029276310768,-327.413678316559)) ;
#28415 = CARTESIAN_POINT('Ctrl Pts',(7.99233402880609,-17.704785827853,-327.41665265265)) ;
#28416 = CARTESIAN_POINT('Ctrl Pts',(7.92038876206054,-17.7370878747095,-327.417613640019)) ;
#28417 = CARTESIAN_POINT('Ctrl Pts',(7.78736326845427,-17.7958430136533,-327.41939640075)) ;
#28418 = CARTESIAN_POINT('Ctrl Pts',(7.72634007583802,-17.822421952097,-327.420216637401)) ;
#28419 = CARTESIAN_POINT('Ctrl Pts',(7.57411262774205,-17.8877965671262,-327.42226813498)) ;
#28420 = CARTESIAN_POINT('Ctrl Pts',(7.48274582578998,-17.9262088293292,-327.423504066407)) ;
#28421 = CARTESIAN_POINT('Ctrl Pts',(7.09120926126737,-18.0873029356201,-327.42881389943)) ;
#28422 = CARTESIAN_POINT('Ctrl Pts',(6.78828727432972,-18.2031571831574,-327.43295479199)) ;
#28423 = CARTESIAN_POINT('Ctrl Pts',(6.34418467701447,-18.360378763321,-327.43900869954)) ;
#28424 = CARTESIAN_POINT('Ctrl Pts',(6.20520995065933,-18.4078123901962,-327.440900955598)) ;
#28425 = CARTESIAN_POINT('Ctrl Pts',(5.60697026383333,-18.6044534814421,-327.449022699918)) ;
#28426 = CARTESIAN_POINT('Ctrl Pts',(5.14276569758894,-18.7380833411738,-327.455260464921)) ;
#28427 = CARTESIAN_POINT('Ctrl Pts',(4.53106214377643,-18.8897275630234,-327.46329263949)) ;
#28428 = CARTESIAN_POINT('Ctrl Pts',(4.3876606325768,-18.9235505598868,-327.465162792236)) ;
#28429 = CARTESIAN_POINT('Ctrl Pts',(4.03109937961599,-19.0033789474859,-327.469778282066)) ;
#28430 = CARTESIAN_POINT('Ctrl Pts',(3.81752330056982,-19.0474326280615,-327.472512342319)) ;
#28431 = CARTESIAN_POINT('Ctrl Pts',(3.47213376834506,-19.11263237607,-327.47688225734)) ;
#28432 = CARTESIAN_POINT('Ctrl Pts',(3.34076527546002,-19.1360318948384,-327.478532468078)) ;
#28433 = CARTESIAN_POINT('Ctrl Pts',(3.08509292417461,-19.178859526517,-327.481721372759)) ;
#28434 = CARTESIAN_POINT('Ctrl Pts',(2.96082076117948,-19.1984372165268,-327.483260974537)) ;
#28435 = CARTESIAN_POINT('Ctrl Pts',(2.68569648657068,-19.2390450797176,-327.486647442526)) ;
#28436 = CARTESIAN_POINT('Ctrl Pts',(2.53476941735258,-19.25951103426,-327.488490580372)) ;
#28437 = CARTESIAN_POINT('Ctrl Pts',(1.59268795407757,-19.3759929441759,-327.499912650502)) ;
#28438 = CARTESIAN_POINT('Ctrl Pts',(0.796488855829417,-19.425018978354,-327.509167151829)) ;
#28439 = CARTESIAN_POINT('Ctrl Pts',(-0.000462715166402311,-19.4249999944889,
-327.51849135163)) ;
#28440 = CARTESIAN_POINT('Origin',(0.,0.,-328.125)) ;
#28441 = CARTESIAN_POINT('',(0.000354632730933767,-19.4249999967628,-329.231156838445)) ;
#28442 = CARTESIAN_POINT('',(0.000234857373855835,-19.4249998715866,-329.01970498129)) ;
#28443 = CARTESIAN_POINT('',(-2.37887640734373E-15,-19.425,-328.125)) ;
#28444 = CARTESIAN_POINT('Ctrl Pts',(0.000354632730933767,-19.4249999967628,
-329.231156838445)) ;
#28445 = CARTESIAN_POINT('Ctrl Pts',(0.415569471354703,-19.4249924163884,
-329.226055010052)) ;
#28446 = CARTESIAN_POINT('Ctrl Pts',(0.83072768051785,-19.4116674955667,-329.220953181658)) ;
#28447 = CARTESIAN_POINT('Ctrl Pts',(1.2449867673168,-19.3850621084691,-329.215851353265)) ;
#28448 = CARTESIAN_POINT('Ctrl Pts',(1.65937670872291,-19.3584483173617,-329.210747913325)) ;
#28449 = CARTESIAN_POINT('Ctrl Pts',(2.07286675400417,-19.3185456871708,-329.205644473386)) ;
#28450 = CARTESIAN_POINT('Ctrl Pts',(2.48461808999774,-19.2654431027904,-329.200541033446)) ;
#28451 = CARTESIAN_POINT('Ctrl Pts',(2.84751853597314,-19.2186407007835,-329.19604307444)) ;
#28452 = CARTESIAN_POINT('Ctrl Pts',(3.20906834148811,-19.1615854409615,-329.191545115434)) ;
#28453 = CARTESIAN_POINT('Ctrl Pts',(3.56869801950147,-19.094371407449,-329.187047156428)) ;
#28454 = CARTESIAN_POINT('Ctrl Pts',(3.96544946344926,-19.0202193936415,-329.182084908205)) ;
#28455 = CARTESIAN_POINT('Ctrl Pts',(4.359941694972,-18.9336874237587,-329.177122659982)) ;
#28456 = CARTESIAN_POINT('Ctrl Pts',(4.7513935665189,-18.8349378596279,-329.17216041176)) ;
#28457 = CARTESIAN_POINT('Ctrl Pts',(5.1425489128499,-18.7362630983986,-329.167201922445)) ;
#28458 = CARTESIAN_POINT('Ctrl Pts',(5.53066827328683,-18.6253893036814,-329.162243433131)) ;
#28459 = CARTESIAN_POINT('Ctrl Pts',(5.91498411383876,-18.5025292307034,-329.157284943817)) ;
#28460 = CARTESIAN_POINT('Ctrl Pts',(6.29925871129465,-18.3796823425314,-329.152326986626)) ;
#28461 = CARTESIAN_POINT('Ctrl Pts',(6.6797303781206,-18.2448518175426,-329.147369029435)) ;
#28462 = CARTESIAN_POINT('Ctrl Pts',(7.05564710108361,-18.0983001683852,-329.142411072244)) ;
#28463 = CARTESIAN_POINT('Ctrl Pts',(7.43154097862795,-17.9517574255455,-329.137453416361)) ;
#28464 = CARTESIAN_POINT('Ctrl Pts',(7.8028802442326,-17.7934950677717,-329.132495760477)) ;
#28465 = CARTESIAN_POINT('Ctrl Pts',(8.16893166101332,-17.6238242307875,-329.127538104594)) ;
#28466 = CARTESIAN_POINT('Ctrl Pts',(8.53555551838824,-17.4538880581968,-329.122572695801)) ;
#28467 = CARTESIAN_POINT('Ctrl Pts',(8.8968747532441,-17.2725077847233,-329.117607287009)) ;
#28468 = CARTESIAN_POINT('Ctrl Pts',(9.25217472367527,-17.0800435562262,-329.112641878216)) ;
#28469 = CARTESIAN_POINT('Ctrl Pts',(9.60695632518435,-16.8878601255984,-329.107683713763)) ;
#28470 = CARTESIAN_POINT('Ctrl Pts',(9.95573601117668,-16.6846251848545,-329.10272554931)) ;
#28471 = CARTESIAN_POINT('Ctrl Pts',(10.2978273866379,-16.4707430346967,-329.097767384856)) ;
#28472 = CARTESIAN_POINT('Ctrl Pts',(10.6406685030812,-16.2563921319634,-329.092798353894)) ;
#28473 = CARTESIAN_POINT('Ctrl Pts',(10.9767917494116,-16.031347413386,-329.087829322931)) ;
#28474 = CARTESIAN_POINT('Ctrl Pts',(11.3055345829969,-15.7960600401702,-329.082860291969)) ;
#28475 = CARTESIAN_POINT('Ctrl Pts',(11.6342774165822,-15.5607726669543,-329.077891261006)) ;
#28476 = CARTESIAN_POINT('Ctrl Pts',(11.9556396463903,-15.3152427840079,-329.072922230044)) ;
#28477 = CARTESIAN_POINT('Ctrl Pts',(12.2689900757296,-15.0599637290948,-329.067953199082)) ;
#28478 = CARTESIAN_POINT('Ctrl Pts',(12.5819127809508,-14.8050331307286,-329.062990950859)) ;
#28479 = CARTESIAN_POINT('Ctrl Pts',(12.8869287333671,-14.5403121997181,-329.058028702636)) ;
#28480 = CARTESIAN_POINT('Ctrl Pts',(13.1834296627393,-14.2663172307223,-329.053066454413)) ;
#28481 = CARTESIAN_POINT('Ctrl Pts',(13.4797059923366,-13.9925298132121,-329.048107965099)) ;
#28482 = CARTESIAN_POINT('Ctrl Pts',(13.7674800198178,-13.7094825637859,-329.043149475785)) ;
#28483 = CARTESIAN_POINT('Ctrl Pts',(14.0461795388355,-13.4177295159352,-329.03819098647)) ;
#28484 = CARTESIAN_POINT('Ctrl Pts',(14.3248491490381,-13.1260077777474,-329.033233029279)) ;
#28485 = CARTESIAN_POINT('Ctrl Pts',(14.5944460319504,-12.825582278749,-329.028275072088)) ;
#28486 = CARTESIAN_POINT('Ctrl Pts',(14.8544354156144,-12.5170433203429,-329.023317114897)) ;
#28487 = CARTESIAN_POINT('Ctrl Pts',(15.1144089990605,-12.2085231126362,-329.018359459014)) ;
#28488 = CARTESIAN_POINT('Ctrl Pts',(15.3647760967842,-11.8918906120237,-329.013401803131)) ;
#28489 = CARTESIAN_POINT('Ctrl Pts',(15.6050416873464,-11.5677698341635,-329.008444147248)) ;
#28490 = CARTESIAN_POINT('Ctrl Pts',(15.8456830114029,-11.2431421879156,-329.003478738455)) ;
#28491 = CARTESIAN_POINT('Ctrl Pts',(16.0761910565558,-10.9110030089518,-328.998513329663)) ;
#28492 = CARTESIAN_POINT('Ctrl Pts',(16.2961105777967,-10.5720104538457,-328.99354792087)) ;
#28493 = CARTESIAN_POINT('Ctrl Pts',(16.5157092449555,-10.2335124757761,-328.988589756417)) ;
#28494 = CARTESIAN_POINT('Ctrl Pts',(16.7247501452136,-9.88818131222814,-328.983631591964)) ;
#28495 = CARTESIAN_POINT('Ctrl Pts',(16.9228239627251,-9.53670037940891,-328.97867342751)) ;
#28496 = CARTESIAN_POINT('Ctrl Pts',(17.1213318866479,-9.18444912707794,-328.973704396548)) ;
#28497 = CARTESIAN_POINT('Ctrl Pts',(17.308824473051,-8.82602132105644,-328.968735365586)) ;
#28498 = CARTESIAN_POINT('Ctrl Pts',(17.4849357707604,-8.46213011554323,-328.963766334623)) ;
#28499 = CARTESIAN_POINT('Ctrl Pts',(17.6610470684698,-8.09823891003003,-328.958797303661)) ;
#28500 = CARTESIAN_POINT('Ctrl Pts',(17.8257769790622,-7.72888452366728,-328.953828272698)) ;
#28501 = CARTESIAN_POINT('Ctrl Pts',(17.9788072554305,-7.35480215043743,-328.948859241736)) ;
#28502 = CARTESIAN_POINT('Ctrl Pts',(18.1316286450887,-6.98123040058307,-328.943896993513)) ;
#28503 = CARTESIAN_POINT('Ctrl Pts',(18.2728229536204,-6.60284426211896,-328.938934745291)) ;
#28504 = CARTESIAN_POINT('Ctrl Pts',(18.4021030494348,-6.22038811956168,-328.933972497068)) ;
#28505 = CARTESIAN_POINT('Ctrl Pts',(18.5312852154367,-5.83822168794605,-328.929014007754)) ;
#28506 = CARTESIAN_POINT('Ctrl Pts',(18.6485711358642,-5.45199164099182,-328.924055518439)) ;
#28507 = CARTESIAN_POINT('Ctrl Pts',(18.7537234030452,-5.06245824892152,-328.919097029125)) ;
#28508 = CARTESIAN_POINT('Ctrl Pts',(18.8588643857443,-4.67296665987346,-328.914139071934)) ;
#28509 = CARTESIAN_POINT('Ctrl Pts',(18.9518742541405,-4.28017266283976,-328.909181114743)) ;
#28510 = CARTESIAN_POINT('Ctrl Pts',(19.0325658242294,-3.88485046641099,-328.904223157552)) ;
#28511 = CARTESIAN_POINT('Ctrl Pts',(19.1132524904863,-3.48955229471847,-328.899265501669)) ;
#28512 = CARTESIAN_POINT('Ctrl Pts',(19.181622306525,-3.09172646307406,-328.894307845786)) ;
#28513 = CARTESIAN_POINT('Ctrl Pts',(19.2375391241372,-2.69215776790513,-328.889350189903)) ;
#28514 = CARTESIAN_POINT('Ctrl Pts',(19.2935433859028,-2.29196421696319,-328.88438478111)) ;
#28515 = CARTESIAN_POINT('Ctrl Pts',(19.3370556235782,-1.89002258157972,-328.879419372317)) ;
#28516 = CARTESIAN_POINT('Ctrl Pts',(19.36799095163,-1.48712860828419,-328.874453963525)) ;
#28517 = CARTESIAN_POINT('Ctrl Pts',(19.3988811462339,-1.08482244172293,-328.869495799072)) ;
#28518 = CARTESIAN_POINT('Ctrl Pts',(19.417231099536,-0.681566952346034,-328.864537634618)) ;
#28519 = CARTESIAN_POINT('Ctrl Pts',(19.4230083425457,-0.278158094259134,
-328.859579470165)) ;
#28520 = CARTESIAN_POINT('Ctrl Pts',(19.4287982471895,0.12613489063155,-328.854610439203)) ;
#28521 = CARTESIAN_POINT('Ctrl Pts',(19.4219602533177,0.530581678137673,-328.84964140824)) ;
#28522 = CARTESIAN_POINT('Ctrl Pts',(19.4025141990856,0.934380947087321,-328.844672377278)) ;
#28523 = CARTESIAN_POINT('Ctrl Pts',(19.3830681448536,1.33818021603692,-328.839703346316)) ;
#28524 = CARTESIAN_POINT('Ctrl Pts',(19.3510140484364,1.74133172734594,-328.834734315353)) ;
#28525 = CARTESIAN_POINT('Ctrl Pts',(19.306424182672,2.14303762886651,-328.829765284391)) ;
#28526 = CARTESIAN_POINT('Ctrl Pts',(19.2618951821857,2.54419520082795,-328.824803036168)) ;
#28527 = CARTESIAN_POINT('Ctrl Pts',(19.2048527866065,2.94401774602782,-328.819840787945)) ;
#28528 = CARTESIAN_POINT('Ctrl Pts',(19.1354009891766,3.3417142282694,-328.814878539723)) ;
#28529 = CARTESIAN_POINT('Ctrl Pts',(19.0660018015586,3.73910945499445,-328.809920050408)) ;
#28530 = CARTESIAN_POINT('Ctrl Pts',(18.9842120460907,4.13438160453245,-328.804961561094)) ;
#28531 = CARTESIAN_POINT('Ctrl Pts',(18.8901869801266,4.52674948012969,-328.80000307178)) ;
#28532 = CARTESIAN_POINT('Ctrl Pts',(18.7961720045218,4.91907524852091,-328.795045114589)) ;
#28533 = CARTESIAN_POINT('Ctrl Pts',(18.6899243962863,5.30849713474285,-328.790087157398)) ;
#28534 = CARTESIAN_POINT('Ctrl Pts',(18.5716501840751,5.69424573059011,-328.785129200207)) ;
#28535 = CARTESIAN_POINT('Ctrl Pts',(18.4533831596888,6.07997088351307,-328.780171544324)) ;
#28536 = CARTESIAN_POINT('Ctrl Pts',(18.3230910610183,6.46202296516201,-328.77521388844)) ;
#28537 = CARTESIAN_POINT('Ctrl Pts',(18.1810297981968,6.83964768661962,-328.770256232557)) ;
#28538 = CARTESIAN_POINT('Ctrl Pts',(18.0387463763287,7.2178629473024,-328.765290823765)) ;
#28539 = CARTESIAN_POINT('Ctrl Pts',(17.884657022939,7.59163676160008,-328.760325414972)) ;
#28540 = CARTESIAN_POINT('Ctrl Pts',(17.719067902185,7.96022975031234,-328.755360006179)) ;
#28541 = CARTESIAN_POINT('Ctrl Pts',(17.5537203695582,8.32828497609991,-328.750401841726)) ;
#28542 = CARTESIAN_POINT('Ctrl Pts',(17.3769067115698,8.69117427168043,-328.745443677273)) ;
#28543 = CARTESIAN_POINT('Ctrl Pts',(17.1889792201584,9.04818315292986,-328.74048551282)) ;
#28544 = CARTESIAN_POINT('Ctrl Pts',(17.0006398594255,9.40597446896082,-328.735516481857)) ;
#28545 = CARTESIAN_POINT('Ctrl Pts',(16.8011379953144,9.75785934829109,-328.730547450895)) ;
#28546 = CARTESIAN_POINT('Ctrl Pts',(16.5908744199071,10.1031436188382,-328.725578419933)) ;
#28547 = CARTESIAN_POINT('Ctrl Pts',(16.3806108444999,10.4484278893853,-328.72060938897)) ;
#28548 = CARTESIAN_POINT('Ctrl Pts',(16.1595856881402,10.7871113498981,-328.715640358008)) ;
#28549 = CARTESIAN_POINT('Ctrl Pts',(15.9282441276453,11.118527960577,-328.710671327045)) ;
#28550 = CARTESIAN_POINT('Ctrl Pts',(15.6972183489589,11.4494921867537,-328.705709078823)) ;
#28551 = CARTESIAN_POINT('Ctrl Pts',(15.4558429079907,11.7732973736191,-328.7007468306)) ;
#28552 = CARTESIAN_POINT('Ctrl Pts',(15.2045875752387,12.0892986424729,-328.695784582377)) ;
#28553 = CARTESIAN_POINT('Ctrl Pts',(14.953522568673,12.4050605400237,-328.690826093063)) ;
#28554 = CARTESIAN_POINT('Ctrl Pts',(14.6925927805345,12.7130301521005,-328.685867603749)) ;
#28555 = CARTESIAN_POINT('Ctrl Pts',(14.4223082903802,13.0125957663039,-328.680909114434)) ;
#28556 = CARTESIAN_POINT('Ctrl Pts',(14.1520528059764,13.3121292324346,-328.675951157244)) ;
#28557 = CARTESIAN_POINT('Ctrl Pts',(13.8724447836342,13.6032603258739,-328.670993200053)) ;
#28558 = CARTESIAN_POINT('Ctrl Pts',(13.584033246719,13.8854119763165,-328.666035242862)) ;
#28559 = CARTESIAN_POINT('Ctrl Pts',(13.295639237308,14.1675464796841,-328.661077586978)) ;
#28560 = CARTESIAN_POINT('Ctrl Pts',(12.998442951767,14.4407024642955,-328.656119931095)) ;
#28561 = CARTESIAN_POINT('Ctrl Pts',(12.6930299823837,14.7043400010442,-328.651162275212)) ;
#28562 = CARTESIAN_POINT('Ctrl Pts',(12.3871394003657,14.9683898209346,-328.646196866419)) ;
#28563 = CARTESIAN_POINT('Ctrl Pts',(12.0730065872004,15.2228912330626,-328.641231457627)) ;
#28564 = CARTESIAN_POINT('Ctrl Pts',(11.7512541315046,15.4673414437258,-328.636266048834)) ;
#28565 = CARTESIAN_POINT('Ctrl Pts',(11.4299711002049,15.7114350109803,-328.631307884381)) ;
#28566 = CARTESIAN_POINT('Ctrl Pts',(11.1010908420707,15.9455065519856,-328.626349719928)) ;
#28567 = CARTESIAN_POINT('Ctrl Pts',(10.765264541436,16.1690972027786,-328.621391555475)) ;
#28568 = CARTESIAN_POINT('Ctrl Pts',(10.428702230603,16.3931778836821,-328.616422524512)) ;
#28569 = CARTESIAN_POINT('Ctrl Pts',(10.0851635885213,16.6067315384875,-328.61145349355)) ;
#28570 = CARTESIAN_POINT('Ctrl Pts',(9.73533267111695,16.8093403434722,-328.606484462588)) ;
#28571 = CARTESIAN_POINT('Ctrl Pts',(9.38550175371263,17.011949148457,-328.601515431625)) ;
#28572 = CARTESIAN_POINT('Ctrl Pts',(9.0293787717279,17.2036129892565,-328.596546400663)) ;
#28573 = CARTESIAN_POINT('Ctrl Pts',(8.66767329742823,17.383959980656,-328.5915773697)) ;
#28574 = CARTESIAN_POINT('Ctrl Pts',(8.30646155200444,17.5640607979618,-328.586615121478)) ;
#28575 = CARTESIAN_POINT('Ctrl Pts',(7.93958653014361,17.7329235258746,-328.581652873255)) ;
#28576 = CARTESIAN_POINT('Ctrl Pts',(7.56776927654216,17.8902066275665,-328.576690625032)) ;
#28577 = CARTESIAN_POINT('Ctrl Pts',(7.19623367491283,18.0473705871386,-328.571732135718)) ;
#28578 = CARTESIAN_POINT('Ctrl Pts',(6.81976354496309,18.1929723644495,-328.566773646404)) ;
#28579 = CARTESIAN_POINT('Ctrl Pts',(6.43909946036323,18.3267188317917,-328.561815157089)) ;
#28580 = CARTESIAN_POINT('Ctrl Pts',(6.05847622696971,18.4604509460475,-328.556857199898)) ;
#28581 = CARTESIAN_POINT('Ctrl Pts',(5.67366016173786,18.5823302128011,-328.551899242707)) ;
#28582 = CARTESIAN_POINT('Ctrl Pts',(5.28540946239075,18.6921125562327,-328.546941285516)) ;
#28583 = CARTESIAN_POINT('Ctrl Pts',(4.89718235802834,18.8018882279113,-328.541983629633)) ;
#28584 = CARTESIAN_POINT('Ctrl Pts',(4.50552126488381,18.8995683803713,-328.53702597375)) ;
#28585 = CARTESIAN_POINT('Ctrl Pts',(4.11119872364413,18.9849590480124,-328.532068317867)) ;
#28586 = CARTESIAN_POINT('Ctrl Pts',(3.71625953069999,19.0704832517698,-328.527102909074)) ;
#28587 = CARTESIAN_POINT('Ctrl Pts',(3.31865078938638,19.1436794396047,-328.522137500281)) ;
#28588 = CARTESIAN_POINT('Ctrl Pts',(2.91915976144519,19.2044039555296,-328.517172091488)) ;
#28589 = CARTESIAN_POINT('Ctrl Pts',(2.52025157547297,19.2650398767327,-328.512213927035)) ;
#28590 = CARTESIAN_POINT('Ctrl Pts',(2.11946682860372,19.3132404698375,-328.507255762582)) ;
#28591 = CARTESIAN_POINT('Ctrl Pts',(1.7175968762395,19.3489143357123,-328.502297598129)) ;
#28592 = CARTESIAN_POINT('Ctrl Pts',(1.31484616979748,19.3846663858421,-328.497328567166)) ;
#28593 = CARTESIAN_POINT('Ctrl Pts',(0.911005732975615,19.4078367046179,-328.492359536204)) ;
#28594 = CARTESIAN_POINT('Ctrl Pts',(0.506876152011263,19.4183856580953,-328.487390505242)) ;
#28595 = CARTESIAN_POINT('Ctrl Pts',(0.102746571046912,19.4289346115727,-328.482421474279)) ;
#28596 = CARTESIAN_POINT('Ctrl Pts',(-0.301671914286292,19.426862200149,-328.477452443317)) ;
#28597 = CARTESIAN_POINT('Ctrl Pts',(-0.705578289224847,19.4121813374431,
-328.472483412354)) ;
#28598 = CARTESIAN_POINT('Ctrl Pts',(-1.10893333095202,19.3975205141515,-328.467521164131)) ;
#28599 = CARTESIAN_POINT('Ctrl Pts',(-1.51188488185458,19.3702817519047,-328.462558915909)) ;
#28600 = CARTESIAN_POINT('Ctrl Pts',(-1.91363637230772,19.3305101028033,-328.457596667686)) ;
#28601 = CARTESIAN_POINT('Ctrl Pts',(-2.31508353557163,19.2907685807692,-328.452638178372)) ;
#28602 = CARTESIAN_POINT('Ctrl Pts',(-2.715332219408,19.2385131754269,-328.447679689057)) ;
#28603 = CARTESIAN_POINT('Ctrl Pts',(-3.11359186534508,19.1738407914548,-328.442721199743)) ;
#28604 = CARTESIAN_POINT('Ctrl Pts',(-3.51180877179723,19.1091753478404,-328.437763242552)) ;
#28605 = CARTESIAN_POINT('Ctrl Pts',(-3.90803683248095,19.0320956251393,-328.432805285361)) ;
#28606 = CARTESIAN_POINT('Ctrl Pts',(-4.30149348035884,18.9427500336786,-328.42784732817)) ;
#28607 = CARTESIAN_POINT('Ctrl Pts',(-4.69492621687323,18.8534098719773,-328.422889672287)) ;
#28608 = CARTESIAN_POINT('Ctrl Pts',(-5.08558764565361,18.7518053832431,-328.417932016403)) ;
#28609 = CARTESIAN_POINT('Ctrl Pts',(-5.47270657864753,18.6381358430512,-328.41297436052)) ;
#28610 = CARTESIAN_POINT('Ctrl Pts',(-5.86043089815883,18.5242885435165,-328.408008951728)) ;
#28611 = CARTESIAN_POINT('Ctrl Pts',(-6.24460140074579,18.3983384818859,-328.403043542935)) ;
#28612 = CARTESIAN_POINT('Ctrl Pts',(-6.62445804072266,18.2605361549628,-328.398078134142)) ;
#28613 = CARTESIAN_POINT('Ctrl Pts',(-7.00376048454349,18.1229348763086,-328.393119969689)) ;
#28614 = CARTESIAN_POINT('Ctrl Pts',(-7.37876142559328,17.9735159862364,-328.388161805236)) ;
#28615 = CARTESIAN_POINT('Ctrl Pts',(-7.74872222438242,17.8125778283033,-328.383203640783)) ;
#28616 = CARTESIAN_POINT('Ctrl Pts',(-8.11949384388696,17.6512869519395,-328.37823460982)) ;
#28617 = CARTESIAN_POINT('Ctrl Pts',(-8.48520297924535,17.4784263421979,-328.373265578858)) ;
#28618 = CARTESIAN_POINT('Ctrl Pts',(-8.84512765083664,17.2943442153903,-328.368296547895)) ;
#28619 = CARTESIAN_POINT('Ctrl Pts',(-9.20505232242797,17.1102620885828,-328.363327516933)) ;
#28620 = CARTESIAN_POINT('Ctrl Pts',(-9.55919231989017,16.9149585597718,-328.358358485971)) ;
#28621 = CARTESIAN_POINT('Ctrl Pts',(-9.90685042733949,16.7088281938119,-328.353389455008)) ;
#28622 = CARTESIAN_POINT('Ctrl Pts',(-10.2540339806029,16.5029791963169,-328.348427206785)) ;
#28623 = CARTESIAN_POINT('Ctrl Pts',(-10.5948456236609,16.2862781891673,-328.343464958563)) ;
#28624 = CARTESIAN_POINT('Ctrl Pts',(-10.9286074198686,16.0591458322787,-328.33850271034)) ;
#28625 = CARTESIAN_POINT('Ctrl Pts',(-11.2621163911543,15.8321855283963,-328.333544221026)) ;
#28626 = CARTESIAN_POINT('Ctrl Pts',(-11.5885859956914,15.5948098059353,-328.328585731711)) ;
#28627 = CARTESIAN_POINT('Ctrl Pts',(-11.9073683829411,15.3474819821668,-328.323627242397)) ;
#28628 = CARTESIAN_POINT('Ctrl Pts',(-12.2261165598585,15.1001807005392,-328.318669285206)) ;
#28629 = CARTESIAN_POINT('Ctrl Pts',(-12.5371789797316,14.8429295962303,-328.313711328015)) ;
#28630 = CARTESIAN_POINT('Ctrl Pts',(-12.8399394510907,14.5762333918034,-328.308753370824)) ;
#28631 = CARTESIAN_POINT('Ctrl Pts',(-13.1426815229238,14.309553395185,-328.303795714941)) ;
#28632 = CARTESIAN_POINT('Ctrl Pts',(-13.4371224761093,14.0334296020142,-328.298838059058)) ;
#28633 = CARTESIAN_POINT('Ctrl Pts',(-13.7226804465684,13.7484059571053,-328.293880403175)) ;
#28634 = CARTESIAN_POINT('Ctrl Pts',(-14.0086849799063,13.4629365849096,-328.288914994382)) ;
#28635 = CARTESIAN_POINT('Ctrl Pts',(-14.2857785474108,13.1685396624901,-328.283949585589)) ;
#28636 = CARTESIAN_POINT('Ctrl Pts',(-14.5534135749228,12.8657987827128,-328.278984176797)) ;
#28637 = CARTESIAN_POINT('Ctrl Pts',(-14.8206581332742,12.5634995901775,-328.274026012344)) ;
#28638 = CARTESIAN_POINT('Ctrl Pts',(-15.078471584423,12.252880957598,-328.26906784789)) ;
#28639 = CARTESIAN_POINT('Ctrl Pts',(-15.3263480426619,11.9345582522017,-328.264109683437)) ;
#28640 = CARTESIAN_POINT('Ctrl Pts',(-15.5747677567474,11.615537898178,-328.259140652475)) ;
#28641 = CARTESIAN_POINT('Ctrl Pts',(-15.8132067149351,11.2887798450214,-328.254171621513)) ;
#28642 = CARTESIAN_POINT('Ctrl Pts',(-16.0411975213713,10.9549352841699,-328.24920259055)) ;
#28643 = CARTESIAN_POINT('Ctrl Pts',(-16.2691883278076,10.6210907233183,-328.244233559588)) ;
#28644 = CARTESIAN_POINT('Ctrl Pts',(-16.4867308528162,10.2801598564539,-328.239264528625)) ;
#28645 = CARTESIAN_POINT('Ctrl Pts',(-16.6934016205675,9.93282272742416,-328.234295497663)) ;
#28646 = CARTESIAN_POINT('Ctrl Pts',(-16.8997902822045,9.58595971444351,-328.22933324944)) ;
#28647 = CARTESIAN_POINT('Ctrl Pts',(-17.0953917198708,9.23261571757025,-328.224371001217)) ;
#28648 = CARTESIAN_POINT('Ctrl Pts',(-17.2798118719054,8.87348447181585,-328.219408752995)) ;
#28649 = CARTESIAN_POINT('Ctrl Pts',(-17.4640923254751,8.51462526836899,-328.21445026368)) ;
#28650 = CARTESIAN_POINT('Ctrl Pts',(-17.6372083181478,8.14998779171401,-328.209491774366)) ;
#28651 = CARTESIAN_POINT('Ctrl Pts',(-17.7988126160577,7.78028884158328,-328.204533285052)) ;
#28652 = CARTESIAN_POINT('Ctrl Pts',(-17.9603995713005,7.41062956592835,-328.199575327861)) ;
#28653 = CARTESIAN_POINT('Ctrl Pts',(-18.1104772042123,7.03591011910896,-328.19461737067)) ;
#28654 = CARTESIAN_POINT('Ctrl Pts',(-18.2487458909687,6.65686851356201,-328.189659413479)) ;
#28655 = CARTESIAN_POINT('Ctrl Pts',(-18.3870061747845,6.27784994333961,-328.184701757596)) ;
#28656 = CARTESIAN_POINT('Ctrl Pts',(-18.5134588648321,5.89450996205973,-328.179744101712)) ;
#28657 = CARTESIAN_POINT('Ctrl Pts',(-18.6278532460382,5.50760460128204,-328.174786445829)) ;
#28658 = CARTESIAN_POINT('Ctrl Pts',(-18.7424265201119,5.12009418797716,-328.169821037037)) ;
#28659 = CARTESIAN_POINT('Ctrl Pts',(-18.8449036609417,4.72900746014064,-328.164855628244)) ;
#28660 = CARTESIAN_POINT('Ctrl Pts',(-18.9350830330146,4.33511886028998,-328.159890219451)) ;
#28661 = CARTESIAN_POINT('Ctrl Pts',(-19.0251308368694,3.94180492868166,-328.154932054998)) ;
#28662 = CARTESIAN_POINT('Ctrl Pts',(-19.1029166911701,3.54569752989965,-328.149973890545)) ;
#28663 = CARTESIAN_POINT('Ctrl Pts',(-19.1682907698617,3.14757906366712,-328.145015726092)) ;
#28664 = CARTESIAN_POINT('Ctrl Pts',(-19.2338081249689,2.74858806526303,-328.140046695129)) ;
#28665 = CARTESIAN_POINT('Ctrl Pts',(-19.2868591872791,2.34757740845687,-328.135077664167)) ;
#28666 = CARTESIAN_POINT('Ctrl Pts',(-19.3273450689611,1.94534253675375,-328.130108633204)) ;
#28667 = CARTESIAN_POINT('Ctrl Pts',(-19.3678309506432,1.54310766505063,-328.125139602242)) ;
#28668 = CARTESIAN_POINT('Ctrl Pts',(-19.3957516343142,1.1396488175936,-328.120170571279)) ;
#28669 = CARTESIAN_POINT('Ctrl Pts',(-19.4110606032759,0.735765761604836,
-328.115201540317)) ;
#28670 = CARTESIAN_POINT('Ctrl Pts',(-19.4263486754567,0.332434006996665,
-328.110239292094)) ;
#28671 = CARTESIAN_POINT('Ctrl Pts',(-19.4290635153354,-0.0714280142283438,
-328.105277043872)) ;
#28672 = CARTESIAN_POINT('Ctrl Pts',(-19.419190985827,-0.47502258470058,-328.100314795649)) ;
#28673 = CARTESIAN_POINT('Ctrl Pts',(-19.4093259347704,-0.878311431849071,
-328.095356306334)) ;
#28674 = CARTESIAN_POINT('Ctrl Pts',(-19.3868925827909,-1.28133299581268,
-328.09039781702)) ;
#28675 = CARTESIAN_POINT('Ctrl Pts',(-19.3519289483619,-1.68329170898924,
-328.085439327706)) ;
#28676 = CARTESIAN_POINT('Ctrl Pts',(-19.3169690660775,-2.08520728571259,
-328.080481370515)) ;
#28677 = CARTESIAN_POINT('Ctrl Pts',(-19.2694816077016,-2.48606000308133,
-328.075523413324)) ;
#28678 = CARTESIAN_POINT('Ctrl Pts',(-19.2095565481291,-2.88505844381516,
-328.070565456133)) ;
#28679 = CARTESIAN_POINT('Ctrl Pts',(-19.1496351303553,-3.28403263639661,
-328.06560780025)) ;
#28680 = CARTESIAN_POINT('Ctrl Pts',(-19.0772776566582,-3.68115254280761,
-328.060650144366)) ;
#28681 = CARTESIAN_POINT('Ctrl Pts',(-18.9926256709009,-4.07563432180022,
-328.055692488483)) ;
#28682 = CARTESIAN_POINT('Ctrl Pts',(-18.9078413041969,-4.47073300151744,
-328.05072707969)) ;
#28683 = CARTESIAN_POINT('Ctrl Pts',(-18.8107239791508,-4.86318506006524,
-328.045761670898)) ;
#28684 = CARTESIAN_POINT('Ctrl Pts',(-18.701467146049,-5.25221396986548,-328.040796262105)) ;
#28685 = CARTESIAN_POINT('Ctrl Pts',(-18.5923697144437,-5.64067530152309,
-328.035838097652)) ;
#28686 = CARTESIAN_POINT('Ctrl Pts',(-18.4711682497348,-6.02572324068312,
-328.030879933199)) ;
#28687 = CARTESIAN_POINT('Ctrl Pts',(-18.3381055045038,-6.40659905922707,
-328.025921768746)) ;
#28688 = CARTESIAN_POINT('Ctrl Pts',(-18.204751133699,-6.7883096202745,-328.020952737783)) ;
#28689 = CARTESIAN_POINT('Ctrl Pts',(-18.0594834991421,-7.16582952231242,
-328.015983706821)) ;
#28690 = CARTESIAN_POINT('Ctrl Pts',(-17.9025963241962,-7.53841295319364,
-328.011014675858)) ;
#28691 = CARTESIAN_POINT('Ctrl Pts',(-17.7457091492502,-7.9109963840749,-328.006045644896)) ;
#28692 = CARTESIAN_POINT('Ctrl Pts',(-17.5772025330628,-8.27864312548473,
-328.001076613934)) ;
#28693 = CARTESIAN_POINT('Ctrl Pts',(-17.3974182561651,-8.64062862412527,
-327.996107582971)) ;
#28694 = CARTESIAN_POINT('Ctrl Pts',(-17.2178793852547,-9.00212001165545,
-327.991145334748)) ;
#28695 = CARTESIAN_POINT('Ctrl Pts',(-17.027045905362,-9.35806169999152,-327.986183086526)) ;
#28696 = CARTESIAN_POINT('Ctrl Pts',(-16.8252870497874,-9.70774642706828,
-327.981220838303)) ;
#28697 = CARTESIAN_POINT('Ctrl Pts',(-16.6236810267648,-10.0571662675849,
-327.976262348989)) ;
#28698 = CARTESIAN_POINT('Ctrl Pts',(-16.4111662924579,-10.4003384168076,
-327.971303859674)) ;
#28699 = CARTESIAN_POINT('Ctrl Pts',(-16.1881568509599,-10.7365824529372,
-327.96634537036)) ;
#28700 = CARTESIAN_POINT('Ctrl Pts',(-15.9651713418614,-11.0727904048252,
-327.961387413169)) ;
#28701 = CARTESIAN_POINT('Ctrl Pts',(-15.7316935062015,-11.4020715308846,
-327.956429455978)) ;
#28702 = CARTESIAN_POINT('Ctrl Pts',(-15.4881809868841,-11.7237739110545,
-327.951471498787)) ;
#28703 = CARTESIAN_POINT('Ctrl Pts',(-15.2446832664427,-12.0454567405514,
-327.946513842904)) ;
#28704 = CARTESIAN_POINT('Ctrl Pts',(-14.9911522238549,-12.3595615550819,
-327.941556187021)) ;
#28705 = CARTESIAN_POINT('Ctrl Pts',(-14.728087161658,-12.6654677591712,-327.936598531138)) ;
#28706 = CARTESIAN_POINT('Ctrl Pts',(-14.4646107115677,-12.9718523472307,
-327.931633122345)) ;
#28707 = CARTESIAN_POINT('Ctrl Pts',(-14.1915705447016,-13.2700124726014,
-327.926667713552)) ;
#28708 = CARTESIAN_POINT('Ctrl Pts',(-13.9095080450804,-13.5593587954535,
-327.92170230476)) ;
#28709 = CARTESIAN_POINT('Ctrl Pts',(-13.6278570637449,-13.8482829732034,
-327.916744140307)) ;
#28710 = CARTESIAN_POINT('Ctrl Pts',(-13.3372102336003,-14.1284188877619,
-327.911785975854)) ;
#28711 = CARTESIAN_POINT('Ctrl Pts',(-13.0381437167325,-14.3992164169384,
-327.9068278114)) ;
#28712 = CARTESIAN_POINT('Ctrl Pts',(-12.7384217538598,-14.6706074366885,
-327.901858780438)) ;
#28713 = CARTESIAN_POINT('Ctrl Pts',(-12.4302433255165,-14.9326189219133,
-327.896889749476)) ;
#28714 = CARTESIAN_POINT('Ctrl Pts',(-12.1142231733798,-15.1847364779751,
-327.891920718513)) ;
#28715 = CARTESIAN_POINT('Ctrl Pts',(-11.798203021243,-15.4368540340369,-327.886951687551)) ;
#28716 = CARTESIAN_POINT('Ctrl Pts',(-11.4743413368243,-15.6790775166619,
-327.881982656588)) ;
#28717 = CARTESIAN_POINT('Ctrl Pts',(-11.1432848914274,-15.910934190942,-327.877013625626)) ;
#28718 = CARTESIAN_POINT('Ctrl Pts',(-10.8126803389072,-16.1424743802812,
-327.872051377403)) ;
#28719 = CARTESIAN_POINT('Ctrl Pts',(-10.4748127774727,-16.3637376024259,
-327.86708912918)) ;
#28720 = CARTESIAN_POINT('Ctrl Pts',(-10.1303448129449,-16.5742794404716,
-327.862126880958)) ;
#28721 = CARTESIAN_POINT('Ctrl Pts',(-9.78613778327344,-16.7846617928469,
-327.857168391643)) ;
#28722 = CARTESIAN_POINT('Ctrl Pts',(-9.43534054901703,-16.9843388740011,
-327.852209902329)) ;
#28723 = CARTESIAN_POINT('Ctrl Pts',(-9.07864218947691,-17.1729112556797,
-327.847251413015)) ;
#28724 = CARTESIAN_POINT('Ctrl Pts',(-8.72198210924533,-17.3614634005946,
-327.842293455824)) ;
#28725 = CARTESIAN_POINT('Ctrl Pts',(-8.35942237837064,-17.5389131153692,
-327.837335498633)) ;
#28726 = CARTESIAN_POINT('Ctrl Pts',(-7.99167676071931,-17.7049068778172,
-327.832377541442)) ;
#28727 = CARTESIAN_POINT('Ctrl Pts',(-7.62395349190861,-17.8708905524002,
-327.827419885559)) ;
#28728 = CARTESIAN_POINT('Ctrl Pts',(-7.25104518221184,-18.0254195678817,
-327.822462229676)) ;
#28729 = CARTESIAN_POINT('Ctrl Pts',(-6.87368719156906,-18.1681878400808,
-327.817504573792)) ;
#28730 = CARTESIAN_POINT('Ctrl Pts',(-6.49573907881945,-18.3111793769667,
-327.812539165)) ;
#28731 = CARTESIAN_POINT('Ctrl Pts',(-6.11332757553556,-18.442373261119,-327.807573756207)) ;
#28732 = CARTESIAN_POINT('Ctrl Pts',(-5.72721004115265,-18.5615109876465,
-327.802608347414)) ;
#28733 = CARTESIAN_POINT('Ctrl Pts',(-5.34165583732873,-18.6804748968357,
-327.797650182961)) ;
#28734 = CARTESIAN_POINT('Ctrl Pts',(-4.95240664008152,-18.7874177457839,
-327.792692018508)) ;
#28735 = CARTESIAN_POINT('Ctrl Pts',(-4.5602315857874,-18.8821321064118,-327.787733854055)) ;
#28736 = CARTESIAN_POINT('Ctrl Pts',(-4.16719702513717,-18.9770540467776,
-327.782764823093)) ;
#28737 = CARTESIAN_POINT('Ctrl Pts',(-3.77122399772105,-19.0596937687268,
-327.77779579213)) ;
#28738 = CARTESIAN_POINT('Ctrl Pts',(-3.37309842482874,-19.1298936749899,
-327.772826761168)) ;
#28739 = CARTESIAN_POINT('Ctrl Pts',(-2.97497285193639,-19.200093581253,-327.767857730205)) ;
#28740 = CARTESIAN_POINT('Ctrl Pts',(-2.57469497076363,-19.2578536367626,
-327.762888699243)) ;
#28741 = CARTESIAN_POINT('Ctrl Pts',(-2.17305889770295,-19.3030681506105,
-327.757919668281)) ;
#28742 = CARTESIAN_POINT('Ctrl Pts',(-1.74947978310094,-19.3507529205489,
-327.752679158584)) ;
#28743 = CARTESIAN_POINT('Ctrl Pts',(-1.32431853671982,-19.3844924495454,
-327.747438648887)) ;
#28744 = CARTESIAN_POINT('Ctrl Pts',(-0.898462567284284,-19.4042106259232,
-327.74219813919)) ;
#28745 = CARTESIAN_POINT('Ctrl Pts',(-0.599382236252206,-19.4180587791526,
-327.738517708511)) ;
#28746 = CARTESIAN_POINT('Ctrl Pts',(-0.299959377809275,-19.4249922467247,
-327.734837277831)) ;
#28747 = CARTESIAN_POINT('Ctrl Pts',(-0.000502513484877063,-19.4249999935001,
-327.731156847152)) ;
#28748 = CARTESIAN_POINT('Ctrl Pts',(-0.000462715166386019,-19.4249999944889,
-327.51849135163)) ;
#28749 = CARTESIAN_POINT('Ctrl Pts',(-0.0875504618603551,-19.4249979200065,
-327.51951026367)) ;
#28750 = CARTESIAN_POINT('Ctrl Pts',(-0.174637192315756,-19.4244101871887,
-327.52053032404)) ;
#28751 = CARTESIAN_POINT('Ctrl Pts',(-0.583156222337328,-19.4189056271317,
-327.525325080606)) ;
#28752 = CARTESIAN_POINT('Ctrl Pts',(-0.904437827676747,-19.4065957419375,
-327.529123355872)) ;
#28753 = CARTESIAN_POINT('Ctrl Pts',(-1.32409120042041,-19.3800725791597,
-327.534188979659)) ;
#28754 = CARTESIAN_POINT('Ctrl Pts',(-1.42286835371274,-19.3730709050083,
-327.535388970211)) ;
#28755 = CARTESIAN_POINT('Ctrl Pts',(-1.58793135333655,-19.3601014380791,
-327.537409909657)) ;
#28756 = CARTESIAN_POINT('Ctrl Pts',(-1.6542478829034,-19.3545477246516,-327.538226148633)) ;
#28757 = CARTESIAN_POINT('Ctrl Pts',(-1.79913386337507,-19.3416640706631,
-327.540019594531)) ;
#28758 = CARTESIAN_POINT('Ctrl Pts',(-1.87768966295884,-19.3341959540435,
-327.540998312023)) ;
#28759 = CARTESIAN_POINT('Ctrl Pts',(-2.12211761287909,-19.3094550235214,
-327.544060979465)) ;
#28760 = CARTESIAN_POINT('Ctrl Pts',(-2.28781417049907,-19.2905246853991,
-327.546162031428)) ;
#28761 = CARTESIAN_POINT('Ctrl Pts',(-2.58521889389346,-19.252661306604,-327.549966124065)) ;
#28762 = CARTESIAN_POINT('Ctrl Pts',(-2.71701549882846,-19.2345041746206,
-327.551663631084)) ;
#28763 = CARTESIAN_POINT('Ctrl Pts',(-3.42733183246168,-19.1292000703169,
-327.56085938714)) ;
#28764 = CARTESIAN_POINT('Ctrl Pts',(-4.0018774113232,-19.0173046861576,-327.568456382094)) ;
#28765 = CARTESIAN_POINT('Ctrl Pts',(-4.62835111285505,-18.8656442881826,
-327.57671843398)) ;
#28766 = CARTESIAN_POINT('Ctrl Pts',(-4.68614198174414,-18.8513724105741,
-327.577480494774)) ;
#28767 = CARTESIAN_POINT('Ctrl Pts',(-5.07470334456549,-18.7535171625303,
-327.582602852089)) ;
#28768 = CARTESIAN_POINT('Ctrl Pts',(-5.40328839243028,-18.6614976730265,
-327.586926368301)) ;
#28769 = CARTESIAN_POINT('Ctrl Pts',(-5.87956901118637,-18.5144816882297,
-327.593163028833)) ;
#28770 = CARTESIAN_POINT('Ctrl Pts',(-6.02928939306963,-18.4662674476857,
-327.595119327925)) ;
#28771 = CARTESIAN_POINT('Ctrl Pts',(-6.2961097124211,-18.3767527186552,-327.598597946213)) ;
#28772 = CARTESIAN_POINT('Ctrl Pts',(-6.41343041863843,-18.3361377695898,
-327.600124796865)) ;
#28773 = CARTESIAN_POINT('Ctrl Pts',(-6.66687158684052,-18.2456696257398,
-327.603417875488)) ;
#28774 = CARTESIAN_POINT('Ctrl Pts',(-6.80283974071304,-18.1954117398044,
-327.605181223814)) ;
#28775 = CARTESIAN_POINT('Ctrl Pts',(-7.20459842630199,-18.041776869807,-327.610384246399)) ;
#28776 = CARTESIAN_POINT('Ctrl Pts',(-7.46868901250923,-17.9340635660464,
-327.613794328311)) ;
#28777 = CARTESIAN_POINT('Ctrl Pts',(-8.11569024270686,-17.653403611891,-327.622154760609)) ;
#28778 = CARTESIAN_POINT('Ctrl Pts',(-8.49554402994306,-17.4737751879205,
-327.627066974282)) ;
#28779 = CARTESIAN_POINT('Ctrl Pts',(-9.34594352841898,-17.0373419898732,
-327.638231163116)) ;
#28780 = CARTESIAN_POINT('Ctrl Pts',(-9.8122858686368,-16.7730952776925,-327.644472418995)) ;
#28781 = CARTESIAN_POINT('Ctrl Pts',(-10.365208327018,-16.4288294310756,-327.652289173024)) ;
#28782 = CARTESIAN_POINT('Ctrl Pts',(-10.4627640056774,-16.3668735390041,
-327.653684986233)) ;
#28783 = CARTESIAN_POINT('Ctrl Pts',(-10.6122358801313,-16.2700640243478,
-327.655853571851)) ;
#28784 = CARTESIAN_POINT('Ctrl Pts',(-10.6645464568458,-16.2358240502541,
-327.656618236636)) ;
#28785 = CARTESIAN_POINT('Ctrl Pts',(-10.7753323086322,-16.1625425629803,
-327.658250832286)) ;
#28786 = CARTESIAN_POINT('Ctrl Pts',(-10.8337627389026,-16.1234349118448,
-327.65911977435)) ;
#28787 = CARTESIAN_POINT('Ctrl Pts',(-10.9918688591171,-16.0163665552893,
-327.66149105469)) ;
#28788 = CARTESIAN_POINT('Ctrl Pts',(-11.0911258067423,-15.9477931678159,
-327.663001483979)) ;
#28789 = CARTESIAN_POINT('Ctrl Pts',(-11.9249176232268,-15.3602043433064,
-327.675853058101)) ;
#28790 = CARTESIAN_POINT('Ctrl Pts',(-12.6232290523684,-14.7916745942156,
-327.687641646055)) ;
#28791 = CARTESIAN_POINT('Ctrl Pts',(-13.5081919684354,-13.9627164337976,
-327.703106522724)) ;
#28792 = CARTESIAN_POINT('Ctrl Pts',(-13.7315400811651,-13.7431258503417,
-327.70706605129)) ;
#28793 = CARTESIAN_POINT('Ctrl Pts',(-14.0545557157477,-13.4098055655803,
-327.712865575638)) ;
#28794 = CARTESIAN_POINT('Ctrl Pts',(-14.1583619135899,-13.3001582577333,
-327.71474125546)) ;
#28795 = CARTESIAN_POINT('Ctrl Pts',(-14.3450195712004,-13.098335572006,-327.718135884983)) ;
#28796 = CARTESIAN_POINT('Ctrl Pts',(-14.4282873802844,-13.0065562149735,
-327.719658442122)) ;
#28797 = CARTESIAN_POINT('Ctrl Pts',(-14.6105714554529,-12.8017345403403,
-327.723010527185)) ;
#28798 = CARTESIAN_POINT('Ctrl Pts',(-14.7091657556736,-12.6883272478202,
-327.72483636482)) ;
#28799 = CARTESIAN_POINT('Ctrl Pts',(-15.0140380604009,-12.3293207168525,
-327.730526010657)) ;
#28800 = CARTESIAN_POINT('Ctrl Pts',(-15.215555652452,-12.0797497909713,-327.734350565174)) ;
#28801 = CARTESIAN_POINT('Ctrl Pts',(-15.7283613059349,-11.4114586055765,
-327.744305891026)) ;
#28802 = CARTESIAN_POINT('Ctrl Pts',(-16.0291217978085,-10.9849893599266,
-327.750372355706)) ;
#28803 = CARTESIAN_POINT('Ctrl Pts',(-16.3415791284692,-10.5017291097709,
-327.757104294624)) ;
#28804 = CARTESIAN_POINT('Ctrl Pts',(-16.37061864433,-10.4564032012761,-327.75773442795)) ;
#28805 = CARTESIAN_POINT('Ctrl Pts',(-16.5913556505341,-10.1086955206593,
-327.76256029579)) ;
#28806 = CARTESIAN_POINT('Ctrl Pts',(-16.7748483169206,-9.80118718528197,
-327.76678046217)) ;
#28807 = CARTESIAN_POINT('Ctrl Pts',(-16.9986916894915,-9.4013376396414,-327.772299194441)) ;
#28808 = CARTESIAN_POINT('Ctrl Pts',(-17.0469687853949,-9.31351296554688,
-327.773513332704)) ;
#28809 = CARTESIAN_POINT('Ctrl Pts',(-17.1262458260637,-9.16661219314292,
-327.775550420558)) ;
#28810 = CARTESIAN_POINT('Ctrl Pts',(-17.1576249752709,-9.10774288237239,
-327.776368475831)) ;
#28811 = CARTESIAN_POINT('Ctrl Pts',(-17.2251759874745,-8.97942473321593,
-327.778156115374)) ;
#28812 = CARTESIAN_POINT('Ctrl Pts',(-17.2612323543557,-8.90991660608215,
-327.779127106549)) ;
#28813 = CARTESIAN_POINT('Ctrl Pts',(-17.3711421197179,-8.69486533267194,
-327.782137139557)) ;
#28814 = CARTESIAN_POINT('Ctrl Pts',(-17.4435822327408,-8.5486080997419,-327.784192491514)) ;
#28815 = CARTESIAN_POINT('Ctrl Pts',(-17.5698800013233,-8.28532031359845,
-327.78789601854)) ;
#28816 = CARTESIAN_POINT('Ctrl Pts',(-17.6244329586573,-8.16863383910826,
-327.789538623193)) ;
#28817 = CARTESIAN_POINT('Ctrl Pts',(-17.9044144906519,-7.55390159856788,
-327.798184370866)) ;
#28818 = CARTESIAN_POINT('Ctrl Pts',(-18.1099043209476,-7.04704576123368,
-327.805278442457)) ;
#28819 = CARTESIAN_POINT('Ctrl Pts',(-18.4299567344089,-6.15072336292275,
-327.817500569215)) ;
#28820 = CARTESIAN_POINT('Ctrl Pts',(-18.5542060066141,-5.76507969884636,
-327.822660738808)) ;
#28821 = CARTESIAN_POINT('Ctrl Pts',(-18.7145393192184,-5.2083602612631,-327.829932752344)) ;
#28822 = CARTESIAN_POINT('Ctrl Pts',(-18.7605150291436,-5.04024548104869,
-327.832106367436)) ;
#28823 = CARTESIAN_POINT('Ctrl Pts',(-18.8358229250807,-4.74955547962341,
-327.835825844672)) ;
#28824 = CARTESIAN_POINT('Ctrl Pts',(-18.8662359727767,-4.62727163535486,
-327.837378753196)) ;
#28825 = CARTESIAN_POINT('Ctrl Pts',(-18.9270179645635,-4.37231494533072,
-327.840592562787)) ;
#28826 = CARTESIAN_POINT('Ctrl Pts',(-18.9571867050428,-4.23960131407512,
-327.842252060928)) ;
#28827 = CARTESIAN_POINT('Ctrl Pts',(-19.0351914873101,-3.87896180438932,
-327.846727166939)) ;
#28828 = CARTESIAN_POINT('Ctrl Pts',(-19.0803273789256,-3.6504749029966,-327.849525102332)) ;
#28829 = CARTESIAN_POINT('Ctrl Pts',(-19.1499347249954,-3.26143779399589,
-327.854236118045)) ;
#28830 = CARTESIAN_POINT('Ctrl Pts',(-19.1765211977967,-3.10129187239817,
-327.856160358225)) ;
#28831 = CARTESIAN_POINT('Ctrl Pts',(-19.2889847794236,-2.36700151958446,
-327.864928287907)) ;
#28832 = CARTESIAN_POINT('Ctrl Pts',(-19.3511044448623,-1.7895211434636,-327.871661108941)) ;
#28833 = CARTESIAN_POINT('Ctrl Pts',(-19.4079322895241,-0.879091330808883,
-327.882361781228)) ;
#28834 = CARTESIAN_POINT('Ctrl Pts',(-19.4201130868161,-0.547580203657073,
-327.886278288567)) ;
#28835 = CARTESIAN_POINT('Ctrl Pts',(-19.4249011936842,-0.116852268629662,
-327.891467491982)) ;
#28836 = CARTESIAN_POINT('Ctrl Pts',(-19.4252445233405,-0.0177765970544005,
-327.892668090084)) ;
#28837 = CARTESIAN_POINT('Ctrl Pts',(-19.4245513318986,0.147851710666956,
-327.894689720622)) ;
#28838 = CARTESIAN_POINT('Ctrl Pts',(-19.4239307403101,0.214404239399394,
-327.895506035233)) ;
#28839 = CARTESIAN_POINT('Ctrl Pts',(-19.4218272108245,0.35982669676706,-327.89729922046)) ;
#28840 = CARTESIAN_POINT('Ctrl Pts',(-19.4202058603158,0.438693265072396,
-327.8982775971)) ;
#28841 = CARTESIAN_POINT('Ctrl Pts',(-19.4136651284702,0.684097918810671,
-327.901337926387)) ;
#28842 = CARTESIAN_POINT('Ctrl Pts',(-19.4070835133104,0.850583940071773,
-327.903436945489)) ;
#28843 = CARTESIAN_POINT('Ctrl Pts',(-19.3914059212147,1.14963039464501,-327.90723654428)) ;
#28844 = CARTESIAN_POINT('Ctrl Pts',(-19.3830900955522,1.2822214869906,-327.908931588346)) ;
#28845 = CARTESIAN_POINT('Ctrl Pts',(-19.3309370403932,1.99641590309156,-327.918101731131)) ;
#28846 = CARTESIAN_POINT('Ctrl Pts',(-19.2622820041996,2.57590698486401,-327.925675215487)) ;
#28847 = CARTESIAN_POINT('Ctrl Pts',(-19.1652868113706,3.1658521879522,-327.933339322707)) ;
#28848 = CARTESIAN_POINT('Ctrl Pts',(-19.1628992368409,3.18027223312467,-327.933526634876)) ;
#28849 = CARTESIAN_POINT('Ctrl Pts',(-19.098528555165,3.5663423417311,-327.938540941272)) ;
#28850 = CARTESIAN_POINT('Ctrl Pts',(-19.0257614235174,3.93611408048295,-327.943325971691)) ;
#28851 = CARTESIAN_POINT('Ctrl Pts',(-18.9068865748296,4.45934928392815,-327.950045265111)) ;
#28852 = CARTESIAN_POINT('Ctrl Pts',(-18.8695657925242,4.61472023953373,-327.952034233729)) ;
#28853 = CARTESIAN_POINT('Ctrl Pts',(-18.7997437351827,4.89037625064205,-327.955551545897)) ;
#28854 = CARTESIAN_POINT('Ctrl Pts',(-18.7679941210356,5.01084235446707,-327.957084751049)) ;
#28855 = CARTESIAN_POINT('Ctrl Pts',(-18.6976984268474,5.26751694916318,-327.960343658998)) ;
#28856 = CARTESIAN_POINT('Ctrl Pts',(-18.6588178232343,5.40362644688988,-327.962067022582)) ;
#28857 = CARTESIAN_POINT('Ctrl Pts',(-18.5430858897196,5.79261963843345,-327.966980871184)) ;
#28858 = CARTESIAN_POINT('Ctrl Pts',(-18.4625565609238,6.0443760799163,-327.97014684446)) ;
#28859 = CARTESIAN_POINT('Ctrl Pts',(-18.2569675181771,6.64460576565063,-327.977683463269)) ;
#28860 = CARTESIAN_POINT('Ctrl Pts',(-18.1270341365808,6.99130049699873,-327.982026272134)) ;
#28861 = CARTESIAN_POINT('Ctrl Pts',(-17.7477311490485,7.92156516897305,-327.993770961313)) ;
#28862 = CARTESIAN_POINT('Ctrl Pts',(-17.4795500406759,8.49696888257827,-328.001127490372)) ;
#28863 = CARTESIAN_POINT('Ctrl Pts',(-17.1336482373289,9.15315474311764,-328.01004562201)) ;
#28864 = CARTESIAN_POINT('Ctrl Pts',(-17.0828147637338,9.24767989134375,-328.011343940473)) ;
#28865 = CARTESIAN_POINT('Ctrl Pts',(-16.9989057045247,9.40065632672372,-328.013470902948)) ;
#28866 = CARTESIAN_POINT('Ctrl Pts',(-16.9663057094028,9.45936599930026,-328.014293460279)) ;
#28867 = CARTESIAN_POINT('Ctrl Pts',(-16.8966524543524,9.58328680956738,-328.016043998878)) ;
#28868 = CARTESIAN_POINT('Ctrl Pts',(-16.859524680645,9.64845468258854,-328.016972904328)) ;
#28869 = CARTESIAN_POINT('Ctrl Pts',(-16.7496263004419,9.83878059205885,-328.019708390291)) ;
#28870 = CARTESIAN_POINT('Ctrl Pts',(-16.6758328624322,9.9633419585146,-328.021527439188)) ;
#28871 = CARTESIAN_POINT('Ctrl Pts',(-16.5445552142952,10.1793903807148,-328.024725469698)) ;
#28872 = CARTESIAN_POINT('Ctrl Pts',(-16.4876872576234,10.2712445509051,-328.026098922453)) ;
#28873 = CARTESIAN_POINT('Ctrl Pts',(-16.2192340189682,10.6968803446237,-328.032520083794)) ;
#28874 = CARTESIAN_POINT('Ctrl Pts',(-15.9982606271777,11.0246296024608,-328.037626670119)) ;
#28875 = CARTESIAN_POINT('Ctrl Pts',(-15.6316426828024,11.5341421044106,-328.045723772713)) ;
#28876 = CARTESIAN_POINT('Ctrl Pts',(-15.4924631778218,11.720421146313,-328.048719860984)) ;
#28877 = CARTESIAN_POINT('Ctrl Pts',(-15.1672884594444,12.1397220107385,-328.055525761193)) ;
#28878 = CARTESIAN_POINT('Ctrl Pts',(-14.9792051310224,12.3710510408541,-328.05932550012)) ;
#28879 = CARTESIAN_POINT('Ctrl Pts',(-14.6498080327277,12.7576551792302,-328.065734463548)) ;
#28880 = CARTESIAN_POINT('Ctrl Pts',(-14.5111651439612,12.9151355954244,-328.068362699002)) ;
#28881 = CARTESIAN_POINT('Ctrl Pts',(-14.2812164998254,13.1679493546265,-328.072609034282)) ;
#28882 = CARTESIAN_POINT('Ctrl Pts',(-14.1914423413766,13.264652247545,-328.07423999536)) ;
#28883 = CARTESIAN_POINT('Ctrl Pts',(-14.0125298009809,13.4534777319322,-328.077438316816)) ;
#28884 = CARTESIAN_POINT('Ctrl Pts',(-13.9234509162741,13.5456476087286,-328.079006086041)) ;
#28885 = CARTESIAN_POINT('Ctrl Pts',(-13.7013245503481,13.7709752873562,-328.082856378434)) ;
#28886 = CARTESIAN_POINT('Ctrl Pts',(-13.5672413571309,13.9030937889803,-328.085129388247)) ;
#28887 = CARTESIAN_POINT('Ctrl Pts',(-13.0595226335151,14.3890329128252,-328.09355805165)) ;
#28888 = CARTESIAN_POINT('Ctrl Pts',(-12.6737954045668,14.7299121166464,-328.099603966987)) ;
#28889 = CARTESIAN_POINT('Ctrl Pts',(-11.7867392338451,15.4531636738416,-328.112983197014)) ;
#28890 = CARTESIAN_POINT('Ctrl Pts',(-11.2794137507289,15.8272647355028,-328.120289609384)) ;
#28891 = CARTESIAN_POINT('Ctrl Pts',(-10.6656083675607,16.2353594966201,-328.129151822134)) ;
#28892 = CARTESIAN_POINT('Ctrl Pts',(-10.5759153109872,16.2939287810693,-328.130447720425)) ;
#28893 = CARTESIAN_POINT('Ctrl Pts',(-10.4292427979209,16.3879841520384,-328.132571832571)) ;
#28894 = CARTESIAN_POINT('Ctrl Pts',(-10.3725556956901,16.4239221337203,-328.133393992149)) ;
#28895 = CARTESIAN_POINT('Ctrl Pts',(-10.2520694051062,16.4994343591286,-328.135145056372)) ;
#28896 = CARTESIAN_POINT('Ctrl Pts',(-10.1882248457873,16.5389339357645,-328.136074898614)) ;
#28897 = CARTESIAN_POINT('Ctrl Pts',(-10.0002597944637,16.6537234020935,-328.138816294909)) ;
#28898 = CARTESIAN_POINT('Ctrl Pts',(-9.87552249824322,16.7279931369871,-328.140640395017)) ;
#28899 = CARTESIAN_POINT('Ctrl Pts',(-9.57340816236359,16.9033177640869,-328.145059377197)) ;
#28900 = CARTESIAN_POINT('Ctrl Pts',(-9.39524773944961,17.0029884141334,-328.147666048256)) ;
#28901 = CARTESIAN_POINT('Ctrl Pts',(-8.52006113134286,17.4746495162777,-328.160421872988)) ;
#28902 = CARTESIAN_POINT('Ctrl Pts',(-7.80234867035075,17.8066892439386,-328.170699647395)) ;
#28903 = CARTESIAN_POINT('Ctrl Pts',(-6.85126365716647,18.1781231647068,-328.183617118768)) ;
#28904 = CARTESIAN_POINT('Ctrl Pts',(-6.63462999414935,18.2583038811386,-328.186516920105)) ;
#28905 = CARTESIAN_POINT('Ctrl Pts',(-6.28848315555995,18.3794459665695,-328.1910801135)) ;
#28906 = CARTESIAN_POINT('Ctrl Pts',(-6.15988186663016,18.422945201186,-328.192760319243)) ;
#28907 = CARTESIAN_POINT('Ctrl Pts',(-5.91092959732751,18.5042548426715,-328.195984095111)) ;
#28908 = CARTESIAN_POINT('Ctrl Pts',(-5.79064542670328,18.5422480184539,-328.197528840129)) ;
#28909 = CARTESIAN_POINT('Ctrl Pts',(-5.50241931714543,18.6302094831768,-328.201200700974)) ;
#28910 = CARTESIAN_POINT('Ctrl Pts',(-5.33415456343649,18.6790823903147,-328.203320377013)) ;
#28911 = CARTESIAN_POINT('Ctrl Pts',(-4.58304801967351,18.8862660988725,-328.212685189116)) ;
#28912 = CARTESIAN_POINT('Ctrl Pts',(-3.99367099082209,19.019620657785,-328.219763796531)) ;
#28913 = CARTESIAN_POINT('Ctrl Pts',(-2.85075675345324,19.2227449147989,-328.233323400113)) ;
#28914 = CARTESIAN_POINT('Ctrl Pts',(-2.29853727687148,19.2965659824724,-328.239804063995)) ;
#28915 = CARTESIAN_POINT('Ctrl Pts',(-1.63054495472792,19.3567793016164,-328.247856128942)) ;
#28916 = CARTESIAN_POINT('Ctrl Pts',(-1.51708922322488,19.3660017043853,-328.249231402219)) ;
#28917 = CARTESIAN_POINT('Ctrl Pts',(-1.34150149314783,19.3787220968429,-328.251375654006)) ;
#28918 = CARTESIAN_POINT('Ctrl Pts',(-1.27942264897695,19.3829196468775,-328.25213681154)) ;
#28919 = CARTESIAN_POINT('Ctrl Pts',(-1.14674808015745,19.3912504637301,-328.253771028205)) ;
#28920 = CARTESIAN_POINT('Ctrl Pts',(-1.07614779048985,19.3952966365952,-328.254645172534)) ;
#28921 = CARTESIAN_POINT('Ctrl Pts',(-0.883008938816952,19.405307810807,-328.257047413063)) ;
#28922 = CARTESIAN_POINT('Ctrl Pts',(-0.760433538934665,19.4104975923624,
-328.258583943438)) ;
#28923 = CARTESIAN_POINT('Ctrl Pts',(-0.4770327765349,19.419808040223,-328.262157836714)) ;
#28924 = CARTESIAN_POINT('Ctrl Pts',(-0.316188912043937,19.4230926747799,
-328.264202054021)) ;
#28925 = CARTESIAN_POINT('Ctrl Pts',(0.280529308760709,19.4278642091606,-328.271824201158)) ;
#28926 = CARTESIAN_POINT('Ctrl Pts',(0.716375330055747,19.4166786717865,-328.277464415724)) ;
#28927 = CARTESIAN_POINT('Ctrl Pts',(1.64383212011842,19.3616040490396,-328.289441166289)) ;
#28928 = CARTESIAN_POINT('Ctrl Pts',(2.13489813713932,19.3136249209026,-328.29576586133)) ;
#28929 = CARTESIAN_POINT('Ctrl Pts',(2.82210247795921,19.219950462699,-328.304506387869)) ;
#28930 = CARTESIAN_POINT('Ctrl Pts',(3.02016925046345,19.1898237634445,-328.30701335451)) ;
#28931 = CARTESIAN_POINT('Ctrl Pts',(3.333389318249,19.1372122844123,-328.310956903586)) ;
#28932 = CARTESIAN_POINT('Ctrl Pts',(3.44886565933088,19.1167388450256,-328.312406289383)) ;
#28933 = CARTESIAN_POINT('Ctrl Pts',(3.68929967144744,19.0718615017091,-328.315414889356)) ;
#28934 = CARTESIAN_POINT('Ctrl Pts',(3.81421716603853,19.0472722631414,-328.316972810427)) ;
#28935 = CARTESIAN_POINT('Ctrl Pts',(4.11800216615945,18.984365731484,-328.32074986184)) ;
#28936 = CARTESIAN_POINT('Ctrl Pts',(4.29658764890146,18.9447464691426,-328.32296033885)) ;
#28937 = CARTESIAN_POINT('Ctrl Pts',(4.58592423128139,18.8762553098497,-328.326529341337)) ;
#28938 = CARTESIAN_POINT('Ctrl Pts',(4.69702643109369,18.8489166350012,-328.327896851862)) ;
#28939 = CARTESIAN_POINT('Ctrl Pts',(5.1207545749154,18.7406717029069,-328.333104256076)) ;
#28940 = CARTESIAN_POINT('Ctrl Pts',(5.43158704647897,18.6529559552165,-328.336906449447)) ;
#28941 = CARTESIAN_POINT('Ctrl Pts',(6.14384608956865,18.432644884267,-328.345640440425)) ;
#28942 = CARTESIAN_POINT('Ctrl Pts',(6.54342013044681,18.2946138186444,-328.350555108372)) ;
#28943 = CARTESIAN_POINT('Ctrl Pts',(7.23126063713109,18.0315821955327,-328.359201022238)) ;
#28944 = CARTESIAN_POINT('Ctrl Pts',(7.52158930831235,17.9124197234087,-328.362910550602)) ;
#28945 = CARTESIAN_POINT('Ctrl Pts',(7.89913067769083,17.7466636248394,-328.36787842997)) ;
#28946 = CARTESIAN_POINT('Ctrl Pts',(7.98905554481765,17.7063640180782,-328.369072698009)) ;
#28947 = CARTESIAN_POINT('Ctrl Pts',(8.13913274411021,17.6377312460158,-328.371087138981)) ;
#28948 = CARTESIAN_POINT('Ctrl Pts',(8.19945329742817,17.6097703268403,-328.371902676444)) ;
#28949 = CARTESIAN_POINT('Ctrl Pts',(8.3312808262468,17.5478389503597,-328.373698629495)) ;
#28950 = CARTESIAN_POINT('Ctrl Pts',(8.40272592842685,17.5137400056105,-328.374680598938)) ;
#28951 = CARTESIAN_POINT('Ctrl Pts',(8.62538791531918,17.4057929420576,-328.377765650427)) ;
#28952 = CARTESIAN_POINT('Ctrl Pts',(8.77585474530485,17.3304159778611,-328.379886176734)) ;
#28953 = CARTESIAN_POINT('Ctrl Pts',(9.39414740862465,17.0105625191951,-328.388720696626)) ;
#28954 = CARTESIAN_POINT('Ctrl Pts',(9.85289134556037,16.7490230926985,-328.395558970818)) ;
#28955 = CARTESIAN_POINT('Ctrl Pts',(10.76960464394,16.1756760325585,-328.409496001678)) ;
#28956 = CARTESIAN_POINT('Ctrl Pts',(11.2260433501576,15.8623085791451,-328.416583652633)) ;
#28957 = CARTESIAN_POINT('Ctrl Pts',(11.791563928678,15.4374009301672,-328.425457193509)) ;
#28958 = CARTESIAN_POINT('Ctrl Pts',(11.9135446029793,15.3434605758474,-328.427377568888)) ;
#28959 = CARTESIAN_POINT('Ctrl Pts',(12.133428209973,15.1699196223859,-328.430850526408)) ;
#28960 = CARTESIAN_POINT('Ctrl Pts',(12.2316969456628,15.0907962465439,-328.432406844608)) ;
#28961 = CARTESIAN_POINT('Ctrl Pts',(12.4318045921049,14.9264360691077,-328.435585120368)) ;
#28962 = CARTESIAN_POINT('Ctrl Pts',(12.5335542943512,14.8411009008113,-328.437206140261)) ;
#28963 = CARTESIAN_POINT('Ctrl Pts',(12.7973574017057,14.6152072555017,-328.441423451381)) ;
#28964 = CARTESIAN_POINT('Ctrl Pts',(12.9579716186118,14.4729959349308,-328.444005639473)) ;
#28965 = CARTESIAN_POINT('Ctrl Pts',(13.2223035620439,14.2310226751055,-328.448287237365)) ;
#28966 = CARTESIAN_POINT('Ctrl Pts',(13.3273273051481,14.1327161162044,-328.44999717113)) ;
#28967 = CARTESIAN_POINT('Ctrl Pts',(13.7658223450253,13.7130317652644,-328.457182081507)) ;
#28968 = CARTESIAN_POINT('Ctrl Pts',(14.0888366531669,13.3809486644664,-328.462584199108)) ;
#28969 = CARTESIAN_POINT('Ctrl Pts',(14.523415987501,12.9009691178902,-328.470147717985)) ;
#28970 = CARTESIAN_POINT('Ctrl Pts',(14.6452069443666,12.7625440109993,-328.472302774086)) ;
#28971 = CARTESIAN_POINT('Ctrl Pts',(14.9711996524403,12.3812153556524,-328.478191645861)) ;
#28972 = CARTESIAN_POINT('Ctrl Pts',(15.1714492825501,12.1350087990501,-328.481941903477)) ;
#28973 = CARTESIAN_POINT('Ctrl Pts',(15.4260241849358,11.8058529949963,-328.486955100602)) ;
#28974 = CARTESIAN_POINT('Ctrl Pts',(15.4858737690684,11.7272375546989,-328.488152480239)) ;
#28975 = CARTESIAN_POINT('Ctrl Pts',(15.5850091957751,11.5949358864183,-328.490170452266)) ;
#28976 = CARTESIAN_POINT('Ctrl Pts',(15.6246237566944,11.5414982698249,-328.490986368716)) ;
#28977 = CARTESIAN_POINT('Ctrl Pts',(15.7106981854784,11.4241337739055,-328.492780946795)) ;
#28978 = CARTESIAN_POINT('Ctrl Pts',(15.757043910693,11.3601248732004,-328.493761138643)) ;
#28979 = CARTESIAN_POINT('Ctrl Pts',(15.900373890429,11.1596046514029,-328.496833937232)) ;
#28980 = CARTESIAN_POINT('Ctrl Pts',(15.9959843169556,11.0221210032187,-328.498943800484)) ;
#28981 = CARTESIAN_POINT('Ctrl Pts',(16.164805327881,10.7725397598502,-328.502767393576)) ;
#28982 = CARTESIAN_POINT('Ctrl Pts',(16.2386574684142,10.6608886935786,-328.504475598661)) ;
#28983 = CARTESIAN_POINT('Ctrl Pts',(16.6333256709286,10.0506046527205,-328.513783709302)) ;
#28984 = CARTESIAN_POINT('Ctrl Pts',(16.9323376134122,9.53824519432217,-328.521483935989)) ;
#28985 = CARTESIAN_POINT('Ctrl Pts',(17.3837203324637,8.67647524791353,-328.533948471815)) ;
#28986 = CARTESIAN_POINT('Ctrl Pts',(17.5500836194091,8.33483781685596,-328.538773630745)) ;
#28987 = CARTESIAN_POINT('Ctrl Pts',(17.7719648702282,7.84304581583767,-328.545529756818)) ;
#28988 = CARTESIAN_POINT('Ctrl Pts',(17.8358122197019,7.69674642814802,-328.547516604124)) ;
#28989 = CARTESIAN_POINT('Ctrl Pts',(17.9462605208759,7.43490911529878,-328.551031579928)) ;
#28990 = CARTESIAN_POINT('Ctrl Pts',(17.9935668112125,7.31967852391603,-328.552564546232)) ;
#28991 = CARTESIAN_POINT('Ctrl Pts',(18.0922940469317,7.07245259582448,-328.55582440529)) ;
#28992 = CARTESIAN_POINT('Ctrl Pts',(18.1433861041146,6.94033359033269,-328.557548942601)) ;
#28993 = CARTESIAN_POINT('Ctrl Pts',(18.2858621492871,6.55957604548678,-328.562471087437)) ;
#28994 = CARTESIAN_POINT('Ctrl Pts',(18.3736114261812,6.30961139634169,-328.565644044003)) ;
#28995 = CARTESIAN_POINT('Ctrl Pts',(18.5178237990721,5.87025085931974,-328.571136712812)) ;
#28996 = CARTESIAN_POINT('Ctrl Pts',(18.5765599670062,5.68164265930143,-328.57346801455)) ;
#28997 = CARTESIAN_POINT('Ctrl Pts',(18.7390434990264,5.13041083008669,-328.580222060576)) ;
#28998 = CARTESIAN_POINT('Ctrl Pts',(18.835119323012,4.76562133162026,-328.584616196779)) ;
#28999 = CARTESIAN_POINT('Ctrl Pts',(18.9457287663866,4.28980037581498,-328.590326853063)) ;
#29000 = CARTESIAN_POINT('Ctrl Pts',(18.9700097425174,4.18111900222879,-328.591629958322)) ;
#29001 = CARTESIAN_POINT('Ctrl Pts',(19.0635272449003,3.74494300758538,-328.596862228875)) ;
#29002 = CARTESIAN_POINT('Ctrl Pts',(19.1252279979171,3.4158925936385,-328.600814090908)) ;
#29003 = CARTESIAN_POINT('Ctrl Pts',(19.1941138378297,2.98771015971316,-328.606038789843)) ;
#29004 = CARTESIAN_POINT('Ctrl Pts',(19.2090854597564,2.88988819503593,-328.607238022498)) ;
#29005 = CARTESIAN_POINT('Ctrl Pts',(19.2328726949179,2.72610719882213,-328.609258100138)) ;
#29006 = CARTESIAN_POINT('Ctrl Pts',(19.2420980601437,2.66020954257854,-328.610074245071)) ;
#29007 = CARTESIAN_POINT('Ctrl Pts',(19.2615277079114,2.5160300716269,-328.611868017614)) ;
#29008 = CARTESIAN_POINT('Ctrl Pts',(19.2715937206496,2.43773099606517,-328.612847161481)) ;
#29009 = CARTESIAN_POINT('Ctrl Pts',(19.3014619344503,2.19364304700804,-328.615912755867)) ;
#29010 = CARTESIAN_POINT('Ctrl Pts',(19.3196040811624,2.02765890125357,-328.618016352966)) ;
#29011 = CARTESIAN_POINT('Ctrl Pts',(19.3483756561692,1.72879927397616,-328.621826074587)) ;
#29012 = CARTESIAN_POINT('Ctrl Pts',(19.3597815846282,1.59600889892476,-328.623526667964)) ;
#29013 = CARTESIAN_POINT('Ctrl Pts',(19.4140560922293,0.877480454101865,-328.6327546531)) ;
#29014 = CARTESIAN_POINT('Ctrl Pts',(19.4317102667252,0.290144060602212,-328.640381243504)) ;
#29015 = CARTESIAN_POINT('Ctrl Pts',(19.4211375599041,-0.401067422563322,
-328.649241150573)) ;
#29016 = CARTESIAN_POINT('Ctrl Pts',(19.4187121536292,-0.505032187418889,
-328.650571014867)) ;
#29017 = CARTESIAN_POINT('Ctrl Pts',(19.4056527125555,-0.92139738290081,-328.655883612525)) ;
#29018 = CARTESIAN_POINT('Ctrl Pts',(19.3883137091128,-1.23354064513692,-328.65983549798)) ;
#29019 = CARTESIAN_POINT('Ctrl Pts',(19.3514473338134,-1.69554727671923,-328.665626386004)) ;
#29020 = CARTESIAN_POINT('Ctrl Pts',(19.3376922992548,-1.84581990003371,-328.667500912717)) ;
#29021 = CARTESIAN_POINT('Ctrl Pts',(19.3094549899377,-2.11918124803914,-328.670894375396)) ;
#29022 = CARTESIAN_POINT('Ctrl Pts',(19.2955429734247,-2.24232080165343,-328.672416905486)) ;
#29023 = CARTESIAN_POINT('Ctrl Pts',(19.2621451709096,-2.51455673009521,-328.675770019596)) ;
#29024 = CARTESIAN_POINT('Ctrl Pts',(19.2421045967728,-2.66357708739031,-328.677596900015)) ;
#29025 = CARTESIAN_POINT('Ctrl Pts',(19.1738103485886,-3.13031787574574,-328.683295116365)) ;
#29026 = CARTESIAN_POINT('Ctrl Pts',(19.1194015183647,-3.4470827487168,-328.687127015382)) ;
#29027 = CARTESIAN_POINT('Ctrl Pts',(18.9557263236737,-4.27613439621117,-328.697113591652)) ;
#29028 = CARTESIAN_POINT('Ctrl Pts',(18.833557101158,-4.78560473702088,-328.703203357151)) ;
#29029 = CARTESIAN_POINT('Ctrl Pts',(18.6640288810854,-5.38464725988825,-328.710486763052)) ;
#29030 = CARTESIAN_POINT('Ctrl Pts',(18.6363803460844,-5.47957368540066,-328.711644876675)) ;
#29031 = CARTESIAN_POINT('Ctrl Pts',(18.5180095844289,-5.87471748854718,-328.716487795794)) ;
#29032 = CARTESIAN_POINT('Ctrl Pts',(18.42074832925,-6.17292594519729,-328.720195441116)) ;
#29033 = CARTESIAN_POINT('Ctrl Pts',(18.2835001178679,-6.56155134176968,-328.725161207465)) ;
#29034 = CARTESIAN_POINT('Ctrl Pts',(18.2499836720626,-6.65420382184506,-328.726355312801)) ;
#29035 = CARTESIAN_POINT('Ctrl Pts',(18.1926729738228,-6.80894229425044,-328.728369569298)) ;
#29036 = CARTESIAN_POINT('Ctrl Pts',(18.1692622368004,-6.87116837787449,-328.729185087108)) ;
#29037 = CARTESIAN_POINT('Ctrl Pts',(18.1172739931451,-7.00723028406511,-328.730981112833)) ;
#29038 = CARTESIAN_POINT('Ctrl Pts',(18.0885636643284,-7.0810138918785,-328.731963175847)) ;
#29039 = CARTESIAN_POINT('Ctrl Pts',(17.9974044190267,-7.31111438525707,-328.735048873475)) ;
#29040 = CARTESIAN_POINT('Ctrl Pts',(17.9333742789148,-7.46679624694865,-328.737169962277)) ;
#29041 = CARTESIAN_POINT('Ctrl Pts',(17.6602429619318,-8.1070962461664,-328.746004464597)) ;
#29042 = CARTESIAN_POINT('Ctrl Pts',(17.4334571860961,-8.58392458218402,-328.752842102091)) ;
#29043 = CARTESIAN_POINT('Ctrl Pts',(16.9296851257332,-9.54057833566551,-328.766778429147)) ;
#29044 = CARTESIAN_POINT('Ctrl Pts',(16.6510266556395,-10.0189913769374,-328.773866006283)) ;
#29045 = CARTESIAN_POINT('Ctrl Pts',(16.2692257675936,-10.6144533087036,-328.782739423047)) ;
#29046 = CARTESIAN_POINT('Ctrl Pts',(16.1845908557538,-10.7430603199628,-328.784659746744)) ;
#29047 = CARTESIAN_POINT('Ctrl Pts',(16.027834385079,-10.9752023296477,-328.788132641318)) ;
#29048 = CARTESIAN_POINT('Ctrl Pts',(15.9562157940351,-11.0790666951431,-328.789688947763)) ;
#29049 = CARTESIAN_POINT('Ctrl Pts',(15.8071453887112,-11.2908110515374,-328.792867229578)) ;
#29050 = CARTESIAN_POINT('Ctrl Pts',(15.72958882447,-11.3986093454665,-328.794488266968)) ;
#29051 = CARTESIAN_POINT('Ctrl Pts',(15.5238717078849,-11.6784438335292,-328.798705695407)) ;
#29052 = CARTESIAN_POINT('Ctrl Pts',(15.3939559513521,-11.8491672094131,-328.801287981765)) ;
#29053 = CARTESIAN_POINT('Ctrl Pts',(15.1722379539842,-12.130726098726,-328.805569772342)) ;
#29054 = CARTESIAN_POINT('Ctrl Pts',(15.0819840011969,-12.2427561788938,-328.807279800864)) ;
#29055 = CARTESIAN_POINT('Ctrl Pts',(14.6959333734352,-12.7112032986595,-328.81446533437)) ;
#29056 = CARTESIAN_POINT('Ctrl Pts',(14.3886831821545,-13.0579839052764,-328.819867967277)) ;
#29057 = CARTESIAN_POINT('Ctrl Pts',(13.9436264774696,-13.5254997984984,-328.827408064073)) ;
#29058 = CARTESIAN_POINT('Ctrl Pts',(13.8160675971733,-13.655773147065,-328.829539140338)) ;
#29059 = CARTESIAN_POINT('Ctrl Pts',(13.4602783048246,-14.0090448654444,-328.835424021284)) ;
#29060 = CARTESIAN_POINT('Ctrl Pts',(13.2283584410324,-14.2282452255454,-328.839194564661)) ;
#29061 = CARTESIAN_POINT('Ctrl Pts',(12.9176113072446,-14.507781568872,-328.844230048485)) ;
#29062 = CARTESIAN_POINT('Ctrl Pts',(12.8435729370392,-14.5733675623781,-328.845428677288)) ;
#29063 = CARTESIAN_POINT('Ctrl Pts',(12.7188985370547,-14.6821208166604,-328.847448068536)) ;
#29064 = CARTESIAN_POINT('Ctrl Pts',(12.6685357819987,-14.7255985555529,-328.848264138786)) ;
#29065 = CARTESIAN_POINT('Ctrl Pts',(12.5757823455232,-14.8048437851223,-328.849768335297)) ;
#29066 = CARTESIAN_POINT('Ctrl Pts',(12.5334600553495,-14.84069001554,-328.850455045954)) ;
#29067 = CARTESIAN_POINT('Ctrl Pts',(12.4316346643341,-14.9261880734865,-328.852107476155)) ;
#29068 = CARTESIAN_POINT('Ctrl Pts',(12.3719868276337,-14.9756660202979,-328.853075637098)) ;
#29069 = CARTESIAN_POINT('Ctrl Pts',(12.2162677354234,-15.1032698640578,-328.85560185962)) ;
#29070 = CARTESIAN_POINT('Ctrl Pts',(12.1197427333562,-15.1808364061166,-328.857166498434)) ;
#29071 = CARTESIAN_POINT('Ctrl Pts',(11.8114886010359,-15.4237324353542,-328.862150817487)) ;
#29072 = CARTESIAN_POINT('Ctrl Pts',(11.5970685372586,-15.5855954733917,-328.865599291756)) ;
#29073 = CARTESIAN_POINT('Ctrl Pts',(10.7605296986841,-16.1902643483047,-328.878893990631)) ;
#29074 = CARTESIAN_POINT('Ctrl Pts',(10.1158588581006,-16.6006948005297,-328.888781954592)) ;
#29075 = CARTESIAN_POINT('Ctrl Pts',(9.28707959837534,-17.0620924036585,-328.900715462584)) ;
#29076 = CARTESIAN_POINT('Ctrl Pts',(9.12417581604499,-17.1497597792226,-328.90302732312)) ;
#29077 = CARTESIAN_POINT('Ctrl Pts',(8.84806662081084,-17.2933013052925,-328.906888340963)) ;
#29078 = CARTESIAN_POINT('Ctrl Pts',(8.73552390719892,-17.3504229077495,-328.908446363769)) ;
#29079 = CARTESIAN_POINT('Ctrl Pts',(8.52207399768947,-17.4561571665108,-328.911372094351)) ;
#29080 = CARTESIAN_POINT('Ctrl Pts',(8.4212874200101,-17.5050017557113,-328.91274142855)) ;
#29081 = CARTESIAN_POINT('Ctrl Pts',(8.15565048331308,-17.6309132893874,-328.916319601425)) ;
#29082 = CARTESIAN_POINT('Ctrl Pts',(7.99012972785903,-17.7065401840973,-328.918518181041)) ;
#29083 = CARTESIAN_POINT('Ctrl Pts',(7.62523327087576,-17.8671037649761,-328.923302711856)) ;
#29084 = CARTESIAN_POINT('Ctrl Pts',(7.42544924867052,-17.9510524211035,-328.92588214141)) ;
#29085 = CARTESIAN_POINT('Ctrl Pts',(6.77554638210064,-18.2114333173945,-328.934164740703)) ;
#29086 = CARTESIAN_POINT('Ctrl Pts',(6.32023468587314,-18.3744106309521,-328.939797666943)) ;
#29087 = CARTESIAN_POINT('Ctrl Pts',(5.74812072314533,-18.5554125739758,-328.946809590416)) ;
#29088 = CARTESIAN_POINT('Ctrl Pts',(5.63660815978807,-18.5895905301772,-328.94817351863)) ;
#29089 = CARTESIAN_POINT('Ctrl Pts',(5.18622949860399,-18.7232038781322,-328.953679466404)) ;
#29090 = CARTESIAN_POINT('Ctrl Pts',(4.84498893126302,-18.8143939847388,-328.957843935287)) ;
#29091 = CARTESIAN_POINT('Ctrl Pts',(4.40480269374701,-18.9192549998506,-328.963294756656)) ;
#29092 = CARTESIAN_POINT('Ctrl Pts',(4.30797659548703,-18.9415372695713,-328.964498680015)) ;
#29093 = CARTESIAN_POINT('Ctrl Pts',(4.14597519600303,-18.9775116705646,-328.966524096919)) ;
#29094 = CARTESIAN_POINT('Ctrl Pts',(4.08089272225523,-18.9916132577066,-328.967340829337)) ;
#29095 = CARTESIAN_POINT('Ctrl Pts',(3.9550880828026,-19.0181951301683,-328.968926127317)) ;
#29096 = CARTESIAN_POINT('Ctrl Pts',(3.8943763013049,-19.0307199276687,-328.969693982674)) ;
#29097 = CARTESIAN_POINT('Ctrl Pts',(3.75509229619976,-19.0587596925301,-328.971461176781)) ;
#29098 = CARTESIAN_POINT('Ctrl Pts',(3.67648199704405,-19.0740797753528,-328.972462628536)) ;
#29099 = CARTESIAN_POINT('Ctrl Pts',(3.46917677656013,-19.1131515870996,-328.97511228646)) ;
#29100 = CARTESIAN_POINT('Ctrl Pts',(3.34033273678266,-19.1360896799641,-328.976767895768)) ;
#29101 = CARTESIAN_POINT('Ctrl Pts',(2.91965497893381,-19.2066047663371,-328.98219205468)) ;
#29102 = CARTESIAN_POINT('Ctrl Pts',(2.62696522986092,-19.2488208781446,-328.98599446048)) ;
#29103 = CARTESIAN_POINT('Ctrl Pts',(1.75320651242472,-19.3545466566369,-328.997340702496)) ;
#29104 = CARTESIAN_POINT('Ctrl Pts',(1.1701118523581,-19.3985321784804,-329.004897823376)) ;
#29105 = CARTESIAN_POINT('Ctrl Pts',(0.390749323107679,-19.4220510608801,
-329.014795385046)) ;
#29106 = CARTESIAN_POINT('Ctrl Pts',(0.195497788728379,-19.4249976374814,
-329.017259094025)) ;
#29107 = CARTESIAN_POINT('Ctrl Pts',(0.000234885055415066,-19.4249999985799,
-329.01970520092)) ;
#29108 = CARTESIAN_POINT('Origin',(0.,0.,-328.125)) ;
#29109 = CARTESIAN_POINT('',(-0.000119142683527153,-19.4253123583886,-330.73193689292)) ;
#29110 = CARTESIAN_POINT('',(5.03575626882774E-5,-19.4249999999347,-330.517882160562)) ;
#29111 = CARTESIAN_POINT('',(-2.37887640734373E-15,-19.425,-328.125)) ;
#29112 = CARTESIAN_POINT('Ctrl Pts',(-0.000108465306112585,-19.4254057326986,
-330.731859656045)) ;
#29113 = CARTESIAN_POINT('Ctrl Pts',(0.402674651299642,-19.4253741486293,
-330.726849257756)) ;
#29114 = CARTESIAN_POINT('Ctrl Pts',(0.805509665086475,-19.4127567695453,
-330.721745417837)) ;
#29115 = CARTESIAN_POINT('Ctrl Pts',(1.20759860177362,-19.3876107506117,-330.716618925219)) ;
#29116 = CARTESIAN_POINT('Ctrl Pts',(1.60962475126056,-19.3624686582923,-330.711493233116)) ;
#29117 = CARTESIAN_POINT('Ctrl Pts',(2.01090509352846,-19.3248020034305,-330.706345044419)) ;
#29118 = CARTESIAN_POINT('Ctrl Pts',(2.41065213885928,-19.2747078749785,-330.701224744958)) ;
#29119 = CARTESIAN_POINT('Ctrl Pts',(2.81035664497823,-19.2246190773094,-330.696104990376)) ;
#29120 = CARTESIAN_POINT('Ctrl Pts',(3.20852822676042,-19.1621055444608,-330.69101320624)) ;
#29121 = CARTESIAN_POINT('Ctrl Pts',(3.60438911586109,-19.0873023567467,-330.685977631048)) ;
#29122 = CARTESIAN_POINT('Ctrl Pts',(4.00022756142526,-19.0125034100378,-330.680942341351)) ;
#29123 = CARTESIAN_POINT('Ctrl Pts',(4.39375352994971,-18.9254076404805,-330.675968388971)) ;
#29124 = CARTESIAN_POINT('Ctrl Pts',(4.78420335923599,-18.8262087064853,-330.671048234656)) ;
#29125 = CARTESIAN_POINT('Ctrl Pts',(5.17469155317068,-18.7270000254446,-330.666127596899)) ;
#29126 = CARTESIAN_POINT('Ctrl Pts',(5.56209903036803,-18.6156685406528,-330.66127095472)) ;
#29127 = CARTESIAN_POINT('Ctrl Pts',(5.94566583029117,-18.4924280199309,-330.656457881628)) ;
#29128 = CARTESIAN_POINT('Ctrl Pts',(6.3292385142747,-18.3691856086525,-330.651644734702)) ;
#29129 = CARTESIAN_POINT('Ctrl Pts',(6.70897049216514,-18.2340336797976,-330.646875082202)) ;
#29130 = CARTESIAN_POINT('Ctrl Pts',(7.08410902033399,-18.0872198197287,-330.642108681419)) ;
#29131 = CARTESIAN_POINT('Ctrl Pts',(7.45932563463387,-17.9403753999454,-330.637341288495)) ;
#29132 = CARTESIAN_POINT('Ctrl Pts',(7.82994684780494,-17.7818640425076,-330.632577014357)) ;
#29133 = CARTESIAN_POINT('Ctrl Pts',(8.19522780036955,-17.6119735047545,-330.627754785151)) ;
#29134 = CARTESIAN_POINT('Ctrl Pts',(8.46600107051254,-17.4860380675224,-330.624180192054)) ;
#29135 = CARTESIAN_POINT('Ctrl Pts',(8.73384009414484,-17.3538507208123,-330.620573300167)) ;
#29136 = CARTESIAN_POINT('Ctrl Pts',(8.99844474090565,-17.2155437140451,-330.616902657059)) ;
#29137 = CARTESIAN_POINT('Ctrl Pts',(9.35615722376798,-17.0285698895354,-330.611940405353)) ;
#29138 = CARTESIAN_POINT('Ctrl Pts',(9.70805425730376,-16.8303596312534,-330.60686136969)) ;
#29139 = CARTESIAN_POINT('Ctrl Pts',(10.0534516520941,-16.6213392975729,-330.601742006995)) ;
#29140 = CARTESIAN_POINT('Ctrl Pts',(10.398587407984,-16.4124772970214,-330.596626522223)) ;
#29141 = CARTESIAN_POINT('Ctrl Pts',(10.7372334913246,-16.1928217428675,-330.591470937802)) ;
#29142 = CARTESIAN_POINT('Ctrl Pts',(11.068735856015,-15.962828706399,-330.586331682058)) ;
#29143 = CARTESIAN_POINT('Ctrl Pts',(11.40020264532,-15.7328603517783,-330.581192977835)) ;
#29144 = CARTESIAN_POINT('Ctrl Pts',(11.724527346361,-15.492556809596,-330.576070702434)) ;
#29145 = CARTESIAN_POINT('Ctrl Pts',(12.0410830588788,-15.2424030075675,-330.570999388913)) ;
#29146 = CARTESIAN_POINT('Ctrl Pts',(12.3576195334984,-14.9922644080237,-330.565928383588)) ;
#29147 = CARTESIAN_POINT('Ctrl Pts',(12.6663880271718,-14.7322767624914,-330.560908380111)) ;
#29148 = CARTESIAN_POINT('Ctrl Pts',(12.9667874752304,-14.4629532264957,-330.555950911202)) ;
#29149 = CARTESIAN_POINT('Ctrl Pts',(13.2676566956521,-14.1932085154454,-330.550985689675)) ;
#29150 = CARTESIAN_POINT('Ctrl Pts',(13.5601306894737,-13.9140986506533,-330.546083196941)) ;
#29151 = CARTESIAN_POINT('Ctrl Pts',(13.8436307850831,-13.6261678064441,-330.541231609387)) ;
#29152 = CARTESIAN_POINT('Ctrl Pts',(14.1267172650108,-13.3386570422077,-330.536387100111)) ;
#29153 = CARTESIAN_POINT('Ctrl Pts',(14.4008559908154,-13.0423509503839,-330.531593280308)) ;
#29154 = CARTESIAN_POINT('Ctrl Pts',(14.6654959701515,-12.7378206348702,-330.526815586168)) ;
#29155 = CARTESIAN_POINT('Ctrl Pts',(14.9307159449308,-12.4326228986753,-330.522027421045)) ;
#29156 = CARTESIAN_POINT('Ctrl Pts',(15.186395394976,-12.1191647291519,-330.517255339955)) ;
#29157 = CARTESIAN_POINT('Ctrl Pts',(15.4320058807281,-11.7980519082937,-330.512442964679)) ;
#29158 = CARTESIAN_POINT('Ctrl Pts',(15.6776163664798,-11.4769390874361,-330.507630589403)) ;
#29159 = CARTESIAN_POINT('Ctrl Pts',(15.9131577290167,-11.1481714825423,-330.502777734163)) ;
#29160 = CARTESIAN_POINT('Ctrl Pts',(16.1381295772808,-10.8123876582478,-330.497808699713)) ;
#29161 = CARTESIAN_POINT('Ctrl Pts',(16.3627943384096,-10.477062179713,-330.492846448007)) ;
#29162 = CARTESIAN_POINT('Ctrl Pts',(16.5769766019597,-10.1346519189442,-330.487767412344)) ;
#29163 = CARTESIAN_POINT('Ctrl Pts',(16.7802795418121,-9.78585860641153,-330.482648049649)) ;
#29164 = CARTESIAN_POINT('Ctrl Pts',(16.983428479467,-9.43732950519144,-330.477532564877)) ;
#29165 = CARTESIAN_POINT('Ctrl Pts',(17.1757147494581,-9.08242709239955,-330.472376980456)) ;
#29166 = CARTESIAN_POINT('Ctrl Pts',(17.3567822107624,-8.72186476897166,-330.467237724712)) ;
#29167 = CARTESIAN_POINT('Ctrl Pts',(17.5378302406982,-8.36134113951656,-330.462099020489)) ;
#29168 = CARTESIAN_POINT('Ctrl Pts',(17.707661991502,-7.99515883449741,-330.456976745088)) ;
#29169 = CARTESIAN_POINT('Ctrl Pts',(17.8659589653153,-7.62404360727233,-330.451905431567)) ;
#29170 = CARTESIAN_POINT('Ctrl Pts',(18.0242463190186,-7.25295093366409,-330.446834426242)) ;
#29171 = CARTESIAN_POINT('Ctrl Pts',(18.1710003612529,-6.8769259217238,-330.441814422765)) ;
#29172 = CARTESIAN_POINT('Ctrl Pts',(18.3059387860068,-6.49670675208336,-330.436856953856)) ;
#29173 = CARTESIAN_POINT('Ctrl Pts',(18.44108823093,-6.11589298595449,-330.431891732329)) ;
#29174 = CARTESIAN_POINT('Ctrl Pts',(18.5643850678305,-5.73087189082319,-330.426989239595)) ;
#29175 = CARTESIAN_POINT('Ctrl Pts',(18.6755814948354,-5.3423981724351,-330.422137652041)) ;
#29176 = CARTESIAN_POINT('Ctrl Pts',(18.786615690552,-4.95449122218408,-330.417293142765)) ;
#29177 = CARTESIAN_POINT('Ctrl Pts',(18.8855847067103,-4.56314166631443,-330.412499322962)) ;
#29178 = CARTESIAN_POINT('Ctrl Pts',(18.9722779311626,-4.16911461576395,-330.407721628822)) ;
#29179 = CARTESIAN_POINT('Ctrl Pts',(19.0591611559129,-3.77422399995261,-330.402933463699)) ;
#29180 = CARTESIAN_POINT('Ctrl Pts',(19.1337145786862,-3.37664408047978,-330.398161382609)) ;
#29181 = CARTESIAN_POINT('Ctrl Pts',(19.1957639824324,-2.97715963031415,-330.393349007333)) ;
#29182 = CARTESIAN_POINT('Ctrl Pts',(19.2578133861786,-2.57767518014851,-330.388536632057)) ;
#29183 = CARTESIAN_POINT('Ctrl Pts',(19.3073585678561,-2.17628615879326,-330.383683776818)) ;
#29184 = CARTESIAN_POINT('Ctrl Pts',(19.3442656246268,-1.77379270750654,-330.378714742367)) ;
#29185 = CARTESIAN_POINT('Ctrl Pts',(19.3811223031729,-1.37184866078595,-330.373752490662)) ;
#29186 = CARTESIAN_POINT('Ctrl Pts',(19.4053844665361,-0.968698346227976,
-330.368673454999)) ;
#29187 = CARTESIAN_POINT('Ctrl Pts',(19.4170393753042,-0.565147824828563,
-330.363554092304)) ;
#29188 = CARTESIAN_POINT('Ctrl Pts',(19.4286854554663,-0.161902993386298,
-330.358438607532)) ;
#29189 = CARTESIAN_POINT('Ctrl Pts',(19.4277435671211,0.241741460408317,-330.353283023111)) ;
#29190 = CARTESIAN_POINT('Ctrl Pts',(19.4142422810442,0.644988692133317,-330.348143767366)) ;
#29191 = CARTESIAN_POINT('Ctrl Pts',(19.4007424438665,1.04819264912468,-330.343005063144)) ;
#29192 = CARTESIAN_POINT('Ctrl Pts',(19.3746860211204,1.45099950969481,-330.337882787743)) ;
#29193 = CARTESIAN_POINT('Ctrl Pts',(19.3361405488261,1.85261959181327,-330.332811474221)) ;
#29194 = CARTESIAN_POINT('Ctrl Pts',(19.2975974190382,2.25421526645776,-330.327740468897)) ;
#29195 = CARTESIAN_POINT('Ctrl Pts',(19.2465668059578,2.6546243510754,-330.32272046542)) ;
#29196 = CARTESIAN_POINT('Ctrl Pts',(19.1831539722185,3.0530635659536,-330.31776299651)) ;
#29197 = CARTESIAN_POINT('Ctrl Pts',(19.1196419718631,3.45212587029724,-330.312797774984)) ;
#29198 = CARTESIAN_POINT('Ctrl Pts',(19.0437089669166,3.8492121738211,-330.30789528225)) ;
#29199 = CARTESIAN_POINT('Ctrl Pts',(18.9554984251055,4.24354119325974,-330.303043694696)) ;
#29200 = CARTESIAN_POINT('Ctrl Pts',(18.8674165790657,4.63729490189939,-330.29819918542)) ;
#29201 = CARTESIAN_POINT('Ctrl Pts',(18.7670929256151,5.02829938473267,-330.293405365617)) ;
#29202 = CARTESIAN_POINT('Ctrl Pts',(18.6547085679444,5.41578201386611,-330.288627671477)) ;
#29203 = CARTESIAN_POINT('Ctrl Pts',(18.5420779042709,5.80411386525304,-330.283839506354)) ;
#29204 = CARTESIAN_POINT('Ctrl Pts',(18.4173334587013,6.18890839291264,-330.279067425264)) ;
#29205 = CARTESIAN_POINT('Ctrl Pts',(18.2806977008023,6.56939311546342,-330.274255049988)) ;
#29206 = CARTESIAN_POINT('Ctrl Pts',(18.1440619429034,6.94987783801368,-330.269442674711)) ;
#29207 = CARTESIAN_POINT('Ctrl Pts',(17.9955346750036,7.32605269387698,-330.264589819473)) ;
#29208 = CARTESIAN_POINT('Ctrl Pts',(17.8353811203026,7.69715099363916,-330.259620785022)) ;
#29209 = CARTESIAN_POINT('Ctrl Pts',(17.6754461756045,8.06774274329367,-330.254658533316)) ;
#29210 = CARTESIAN_POINT('Ctrl Pts',(17.5038745173134,8.43336822759492,-330.249579497653)) ;
#29211 = CARTESIAN_POINT('Ctrl Pts',(17.3210405978621,8.79331352638083,-330.244460134959)) ;
#29212 = CARTESIAN_POINT('Ctrl Pts',(17.138345175303,9.15298616621259,-330.239344650187)) ;
#29213 = CARTESIAN_POINT('Ctrl Pts',(16.9444047068852,9.50698733420804,-330.234189065765)) ;
#29214 = CARTESIAN_POINT('Ctrl Pts',(16.7396255112679,9.85463096734606,-330.229049810021)) ;
#29215 = CARTESIAN_POINT('Ctrl Pts',(16.5348682916581,10.2022372928901,-330.223911105798)) ;
#29216 = CARTESIAN_POINT('Ctrl Pts',(16.3192747541773,10.5434875393202,-330.218788830397)) ;
#29217 = CARTESIAN_POINT('Ctrl Pts',(16.0932820073231,10.8777205750419,-330.213717516876)) ;
#29218 = CARTESIAN_POINT('Ctrl Pts',(15.8673029946267,11.2119332985663,-330.208646511551)) ;
#29219 = CARTESIAN_POINT('Ctrl Pts',(15.6309260577843,11.5391297261789,-330.203626508074)) ;
#29220 = CARTESIAN_POINT('Ctrl Pts',(15.3846183710913,11.8586723976787,-330.198669039165)) ;
#29221 = CARTESIAN_POINT('Ctrl Pts',(15.1379255021176,12.1787147782076,-330.193703817638)) ;
#29222 = CARTESIAN_POINT('Ctrl Pts',(14.8812707592671,12.4910794635653,-330.188801324904)) ;
#29223 = CARTESIAN_POINT('Ctrl Pts',(14.6151539106746,12.7951490249379,-330.18394973735)) ;
#29224 = CARTESIAN_POINT('Ctrl Pts',(14.3494253162779,13.0987749605738,-330.179105228074)) ;
#29225 = CARTESIAN_POINT('Ctrl Pts',(14.0742621359218,13.3941299422748,-330.174311408271)) ;
#29226 = CARTESIAN_POINT('Ctrl Pts',(13.7901930455831,13.6806221474832,-330.169533714131)) ;
#29227 = CARTESIAN_POINT('Ctrl Pts',(13.5055013781947,13.9677422403357,-330.164745549008)) ;
#29228 = CARTESIAN_POINT('Ctrl Pts',(13.2118645930312,14.2459605783631,-330.159973467918)) ;
#29229 = CARTESIAN_POINT('Ctrl Pts',(12.909847620977,14.5147052583501,-330.155161092642)) ;
#29230 = CARTESIAN_POINT('Ctrl Pts',(12.6078306489231,14.7834499383368,-330.150348717366)) ;
#29231 = CARTESIAN_POINT('Ctrl Pts',(12.2974333458584,15.0427208116386,-330.145495862126)) ;
#29232 = CARTESIAN_POINT('Ctrl Pts',(11.9792554148419,15.2919715155149,-330.140526827676)) ;
#29233 = CARTESIAN_POINT('Ctrl Pts',(11.6615117974963,15.5408819915575,-330.13556457597)) ;
#29234 = CARTESIAN_POINT('Ctrl Pts',(11.3359256303457,15.7798641592174,-330.130485540307)) ;
#29235 = CARTESIAN_POINT('Ctrl Pts',(11.0031672876764,16.0084702518838,-330.125366177613)) ;
#29236 = CARTESIAN_POINT('Ctrl Pts',(10.6706610098141,16.2369031751859,-330.120250692841)) ;
#29237 = CARTESIAN_POINT('Ctrl Pts',(10.3309935048472,16.4549759114473,-330.11509510842)) ;
#29238 = CARTESIAN_POINT('Ctrl Pts',(9.98484980217588,16.6622804017955,-330.109955852675)) ;
#29239 = CARTESIAN_POINT('Ctrl Pts',(9.63874324613229,16.8695626451329,-330.104817148452)) ;
#29240 = CARTESIAN_POINT('Ctrl Pts',(9.28616191162137,17.0660790735682,-330.099694873052)) ;
#29241 = CARTESIAN_POINT('Ctrl Pts',(8.9278059376802,17.251458251842,-330.09462355953)) ;
#29242 = CARTESIAN_POINT('Ctrl Pts',(8.56947174194395,17.4368261641511,-330.089552554205)) ;
#29243 = CARTESIAN_POINT('Ctrl Pts',(8.20536359771144,17.6110582444914,-330.084532550729)) ;
#29244 = CARTESIAN_POINT('Ctrl Pts',(7.83619672068672,17.7738182283462,-330.079575081819)) ;
#29245 = CARTESIAN_POINT('Ctrl Pts',(7.46645253103106,17.9368327404384,-330.074609860293)) ;
#29246 = CARTESIAN_POINT('Ctrl Pts',(7.09163373071272,18.0883392439755,-330.069707367559)) ;
#29247 = CARTESIAN_POINT('Ctrl Pts',(6.71247457351918,18.2280346582659,-330.064855780004)) ;
#29248 = CARTESIAN_POINT('Ctrl Pts',(6.33386859488192,18.367526262346,-330.060011270729)) ;
#29249 = CARTESIAN_POINT('Ctrl Pts',(5.95093486173872,18.4952411677311,-330.055217450926)) ;
#29250 = CARTESIAN_POINT('Ctrl Pts',(5.56442076202264,18.6109126095375,-330.050439756786)) ;
#29251 = CARTESIAN_POINT('Ctrl Pts',(5.17705956272058,18.72683756145,-330.045651591662)) ;
#29252 = CARTESIAN_POINT('Ctrl Pts',(4.78610221554313,18.830666063824,-330.040879510572)) ;
#29253 = CARTESIAN_POINT('Ctrl Pts',(4.39231841500205,18.9221661887551,-330.036067135296)) ;
#29254 = CARTESIAN_POINT('Ctrl Pts',(3.9985346144603,19.0136663136863,-330.03125476002)) ;
#29255 = CARTESIAN_POINT('Ctrl Pts',(3.60192430511406,19.0928378616947,-330.026401904781)) ;
#29256 = CARTESIAN_POINT('Ctrl Pts',(3.20327549673131,19.1594879685595,-330.021432870331)) ;
#29257 = CARTESIAN_POINT('Ctrl Pts',(2.80517084496984,19.2260470978615,-330.016470618625)) ;
#29258 = CARTESIAN_POINT('Ctrl Pts',(2.40492937024616,19.2801358269128,-330.011391582962)) ;
#29259 = CARTESIAN_POINT('Ctrl Pts',(2.00335396996647,19.3216816824276,-330.006272220267)) ;
#29260 = CARTESIAN_POINT('Ctrl Pts',(1.6020827634881,19.3631960669117,-330.001156735495)) ;
#29261 = CARTESIAN_POINT('Ctrl Pts',(1.19947964438572,19.3921867675156,-329.996001151074)) ;
#29262 = CARTESIAN_POINT('Ctrl Pts',(0.796341381989622,19.4086231908243,-329.990861895329)) ;
#29263 = CARTESIAN_POINT('Ctrl Pts',(0.393246382627672,19.4250578502481,-329.985723191107)) ;
#29264 = CARTESIAN_POINT('Ctrl Pts',(-0.0103836768102819,19.4289410461147,
-329.980600915706)) ;
#29265 = CARTESIAN_POINT('Ctrl Pts',(-0.413756280420004,19.4202815740748,
-329.975529602185)) ;
#29266 = CARTESIAN_POINT('Ctrl Pts',(-0.817104370046287,19.4116226282931,
-329.97045859686)) ;
#29267 = CARTESIAN_POINT('Ctrl Pts',(-1.22019507561338,19.3904225905207,-329.965438593383)) ;
#29268 = CARTESIAN_POINT('Ctrl Pts',(-1.6222394685035,19.3567283538937,-329.960481124473)) ;
#29269 = CARTESIAN_POINT('Ctrl Pts',(-2.02491258872684,19.3229814253553,-329.955515902947)) ;
#29270 = CARTESIAN_POINT('Ctrl Pts',(-2.42653615787623,19.2767011661808,-329.950613410213)) ;
#29271 = CARTESIAN_POINT('Ctrl Pts',(-2.82632040539988,19.2179727174615,-329.945761822659)) ;
#29272 = CARTESIAN_POINT('Ctrl Pts',(-3.22552138315938,19.1593299512789,-329.940917313383)) ;
#29273 = CARTESIAN_POINT('Ctrl Pts',(-3.62288842607095,19.0882752241637,-329.93612349358)) ;
#29274 = CARTESIAN_POINT('Ctrl Pts',(-4.01763760448166,19.0049318508567,-329.93134579944)) ;
#29275 = CARTESIAN_POINT('Ctrl Pts',(-4.4132519307991,18.9214058189177,-329.926557634317)) ;
#29276 = CARTESIAN_POINT('Ctrl Pts',(-4.80623690085269,18.8255370621331,-329.921785553227)) ;
#29277 = CARTESIAN_POINT('Ctrl Pts',(-5.19580566380469,18.7174901586082,-329.916973177951)) ;
#29278 = CARTESIAN_POINT('Ctrl Pts',(-5.58537442675735,18.609443255083,-329.912160802675)) ;
#29279 = CARTESIAN_POINT('Ctrl Pts',(-5.97152693585674,18.4892180031243,-329.907307947436)) ;
#29280 = CARTESIAN_POINT('Ctrl Pts',(-6.35347894613258,18.3570220462464,-329.902338912985)) ;
#29281 = CARTESIAN_POINT('Ctrl Pts',(-6.73490959095979,18.2250065371801,-329.897376661279)) ;
#29282 = CARTESIAN_POINT('Ctrl Pts',(-7.11225049723722,18.0810181030995,-329.892297625616)) ;
#29283 = CARTESIAN_POINT('Ctrl Pts',(-7.48476194469701,17.9253772288684,-329.887178262922)) ;
#29284 = CARTESIAN_POINT('Ctrl Pts',(-7.85699121433129,17.7698542527684,-329.88206277815)) ;
#29285 = CARTESIAN_POINT('Ctrl Pts',(-8.22439843833507,17.6026966505424,-329.876907193728)) ;
#29286 = CARTESIAN_POINT('Ctrl Pts',(-8.58626931403335,17.424258751148,-329.871767937984)) ;
#29287 = CARTESIAN_POINT('Ctrl Pts',(-8.948101355329,17.24584000093,-329.866629233761)) ;
#29288 = CARTESIAN_POINT('Ctrl Pts',(-9.30439832140479,17.0561434641823,-329.86150695836)) ;
#29289 = CARTESIAN_POINT('Ctrl Pts',(-9.6544684893318,16.8555560235912,-329.856435644839)) ;
#29290 = CARTESIAN_POINT('Ctrl Pts',(-10.0045173826051,16.6549807732087,-329.851364639514)) ;
#29291 = CARTESIAN_POINT('Ctrl Pts',(-10.3483402947084,16.4435159685035,-329.846344636037)) ;
#29292 = CARTESIAN_POINT('Ctrl Pts',(-10.6852668795819,16.2215802304122,-329.841387167128)) ;
#29293 = CARTESIAN_POINT('Ctrl Pts',(-11.0227203588905,15.9992974235214,-329.836421945601)) ;
#29294 = CARTESIAN_POINT('Ctrl Pts',(-11.3532559456396,15.7665108698316,-329.831519452867)) ;
#29295 = CARTESIAN_POINT('Ctrl Pts',(-11.6762208531975,15.5236731797096,-329.826667865313)) ;
#29296 = CARTESIAN_POINT('Ctrl Pts',(-11.998714567437,15.2811897803923,-329.821823356038)) ;
#29297 = CARTESIAN_POINT('Ctrl Pts',(-12.3136596654231,15.0286844808624,-329.817029536234)) ;
#29298 = CARTESIAN_POINT('Ctrl Pts',(-12.6204267527925,14.7666406184365,-329.812251842094)) ;
#29299 = CARTESIAN_POINT('Ctrl Pts',(-12.9278661630434,14.5040224503178,-329.807463676971)) ;
#29300 = CARTESIAN_POINT('Ctrl Pts',(-13.2270915988808,14.2318237292235,-329.802691595881)) ;
#29301 = CARTESIAN_POINT('Ctrl Pts',(-13.517490842168,13.9505654245815,-329.797879220605)) ;
#29302 = CARTESIAN_POINT('Ctrl Pts',(-13.8078900854546,13.66930711994,-329.793066845329)) ;
#29303 = CARTESIAN_POINT('Ctrl Pts',(-14.0894629986418,13.3789890770053,-329.78821399009)) ;
#29304 = CARTESIAN_POINT('Ctrl Pts',(-14.3616202554224,13.0801688354689,-329.783244955639)) ;
#29305 = CARTESIAN_POINT('Ctrl Pts',(-14.6334060168663,12.7817564843102,-329.778282703933)) ;
#29306 = CARTESIAN_POINT('Ctrl Pts',(-14.895872321534,12.4747869945993,-329.773203668271)) ;
#29307 = CARTESIAN_POINT('Ctrl Pts',(-15.1485229275982,12.1598956935516,-329.768084305576)) ;
#29308 = CARTESIAN_POINT('Ctrl Pts',(-15.4009821505541,11.8452429230061,-329.762968820804)) ;
#29309 = CARTESIAN_POINT('Ctrl Pts',(-15.6436407073037,11.5226804374807,-329.757813236383)) ;
#29310 = CARTESIAN_POINT('Ctrl Pts',(-15.876040867779,11.1928611232644,-329.752673980638)) ;
#29311 = CARTESIAN_POINT('Ctrl Pts',(-16.1084160880843,10.8630772038162,-329.747535276416)) ;
#29312 = CARTESIAN_POINT('Ctrl Pts',(-16.3305352311991,10.5260380512659,-329.742413001015)) ;
#29313 = CARTESIAN_POINT('Ctrl Pts',(-16.5419759694787,10.1824143355649,-329.737341687493)) ;
#29314 = CARTESIAN_POINT('Ctrl Pts',(-16.7534038579647,9.83881150275446,-329.732270682169)) ;
#29315 = CARTESIAN_POINT('Ctrl Pts',(-16.9541547046722,9.48862490098346,-329.727250678692)) ;
#29316 = CARTESIAN_POINT('Ctrl Pts',(-17.1438401379526,9.13254284325703,-329.722293209782)) ;
#29317 = CARTESIAN_POINT('Ctrl Pts',(-17.3338222061812,8.77590393527117,-329.717327988256)) ;
#29318 = CARTESIAN_POINT('Ctrl Pts',(-17.5127042251083,8.41335107430971,-329.712425495522)) ;
#29319 = CARTESIAN_POINT('Ctrl Pts',(-17.6801295038996,8.04559401961159,-329.707573907968)) ;
#29320 = CARTESIAN_POINT('Ctrl Pts',(-17.8473105156807,7.67837350824137,-329.702729398692)) ;
#29321 = CARTESIAN_POINT('Ctrl Pts',(-18.0030681487466,7.30596392084994,-329.697935578889)) ;
#29322 = CARTESIAN_POINT('Ctrl Pts',(-18.1470809542084,6.9290908074623,-329.693157884749)) ;
#29323 = CARTESIAN_POINT('Ctrl Pts',(-18.2914093838285,6.55139172405881,-329.688369719625)) ;
#29324 = CARTESIAN_POINT('Ctrl Pts',(-18.4239413159214,6.1692094479231,-329.683597638536)) ;
#29325 = CARTESIAN_POINT('Ctrl Pts',(-18.5443883886575,5.78329435739147,-329.678785263259)) ;
#29326 = CARTESIAN_POINT('Ctrl Pts',(-18.6648354613935,5.39737926686037,-329.673972887983)) ;
#29327 = CARTESIAN_POINT('Ctrl Pts',(-18.7731974799528,5.00773129185362,-329.669120032744)) ;
#29328 = CARTESIAN_POINT('Ctrl Pts',(-18.8692236805865,4.61512197209525,-329.664150998294)) ;
#29329 = CARTESIAN_POINT('Ctrl Pts',(-18.9651188052163,4.22304856504,-329.659188746588)) ;
#29330 = CARTESIAN_POINT('Ctrl Pts',(-19.0487363029649,3.82791954463094,-329.654109710925)) ;
#29331 = CARTESIAN_POINT('Ctrl Pts',(-19.1199443656912,3.43053022416198,-329.648990348231)) ;
#29332 = CARTESIAN_POINT('Ctrl Pts',(-19.1910984882332,3.03344192653243,-329.643874863459)) ;
#29333 = CARTESIAN_POINT('Ctrl Pts',(-19.2498621633251,2.63409675913522,-329.638719279037)) ;
#29334 = CARTESIAN_POINT('Ctrl Pts',(-19.2961458017985,2.23328702942527,-329.633580023292)) ;
#29335 = CARTESIAN_POINT('Ctrl Pts',(-19.3424244733139,1.83252031286454,-329.62844131907)) ;
#29336 = CARTESIAN_POINT('Ctrl Pts',(-19.3762259080336,1.43028932561657,-329.623319043669)) ;
#29337 = CARTESIAN_POINT('Ctrl Pts',(-19.3975001128118,1.02738505409656,-329.618247730148)) ;
#29338 = CARTESIAN_POINT('Ctrl Pts',(-19.4187730247023,0.624505268099502,
-329.613176724823)) ;
#29339 = CARTESIAN_POINT('Ctrl Pts',(-19.4275202835506,0.220952243111883,
-329.608156721346)) ;
#29340 = CARTESIAN_POINT('Ctrl Pts',(-19.4237301548154,-0.182483786957448,
-329.603199252437)) ;
#29341 = CARTESIAN_POINT('Ctrl Pts',(-19.4199340989795,-0.586550720641379,
-329.59823403091)) ;
#29342 = CARTESIAN_POINT('Ctrl Pts',(-19.4035613913778,-0.99050033152334,
-329.593331538176)) ;
#29343 = CARTESIAN_POINT('Ctrl Pts',(-19.3746383777031,-1.39353871001521,
-329.588479950622)) ;
#29344 = CARTESIAN_POINT('Ctrl Pts',(-19.3457575615872,-1.7959890710923,-329.583635441346)) ;
#29345 = CARTESIAN_POINT('Ctrl Pts',(-19.3043629677051,-2.19753088539806,
-329.578841621543)) ;
#29346 = CARTESIAN_POINT('Ctrl Pts',(-19.2505194434125,-2.59737323761063,
-329.574063927403)) ;
#29347 = CARTESIAN_POINT('Ctrl Pts',(-19.1965579135233,-2.99809190012976,
-329.56927576228)) ;
#29348 = CARTESIAN_POINT('Ctrl Pts',(-19.1300926713332,-3.39710365032791,
-329.56450368119)) ;
#29349 = CARTESIAN_POINT('Ctrl Pts',(-19.0512294973661,-3.79361160008601,
-329.559691305914)) ;
#29350 = CARTESIAN_POINT('Ctrl Pts',(-18.972366323399,-4.19011954984452,-329.554878930638)) ;
#29351 = CARTESIAN_POINT('Ctrl Pts',(-18.8811050130503,-4.58412366749528,
-329.550026075399)) ;
#29352 = CARTESIAN_POINT('Ctrl Pts',(-18.7775944869237,-4.97482647033875,
-329.545057040948)) ;
#29353 = CARTESIAN_POINT('Ctrl Pts',(-18.6742252529241,-5.36499596287974,
-329.540094789242)) ;
#29354 = CARTESIAN_POINT('Ctrl Pts',(-18.5586128019716,-5.7519747605986,-329.53501575358)) ;
#29355 = CARTESIAN_POINT('Ctrl Pts',(-18.4310218868634,-6.13500141580958,
-329.529896390885)) ;
#29356 = CARTESIAN_POINT('Ctrl Pts',(-18.3035276220115,-6.51773792791467,
-329.524780906113)) ;
#29357 = CARTESIAN_POINT('Ctrl Pts',(-18.1640732076723,-6.89652836939212,
-329.519625321692)) ;
#29358 = CARTESIAN_POINT('Ctrl Pts',(-18.0129590322685,-7.27063413065785,
-329.514486065947)) ;
#29359 = CARTESIAN_POINT('Ctrl Pts',(-17.8618610737785,-7.64469974452619,
-329.509347361725)) ;
#29360 = CARTESIAN_POINT('Ctrl Pts',(-17.6991059523496,-8.01408176160161,
-329.504225086323)) ;
#29361 = CARTESIAN_POINT('Ctrl Pts',(-17.5250281947923,-8.37806167604782,
-329.499153772802)) ;
#29362 = CARTESIAN_POINT('Ctrl Pts',(-17.3509610163828,-8.74201947050942,
-329.494082767477)) ;
#29363 = CARTESIAN_POINT('Ctrl Pts',(-17.165572608229,-9.10057587700563,-329.489062764001)) ;
#29364 = CARTESIAN_POINT('Ctrl Pts',(-16.9692307331029,-9.45303135434919,
-329.484105295091)) ;
#29365 = CARTESIAN_POINT('Ctrl Pts',(-16.7725818135176,-9.80603801060642,
-329.479140073565)) ;
#29366 = CARTESIAN_POINT('Ctrl Pts',(-16.5649451048215,-10.1529246648428,
-329.47423758083)) ;
#29367 = CARTESIAN_POINT('Ctrl Pts',(-16.3467235676692,-10.4930067666653,
-329.469385993276)) ;
#29368 = CARTESIAN_POINT('Ctrl Pts',(-16.1288204073066,-10.8325927018433,
-329.464541484001)) ;
#29369 = CARTESIAN_POINT('Ctrl Pts',(-15.9003632101785,-11.1653939189612,
-329.459747664198)) ;
#29370 = CARTESIAN_POINT('Ctrl Pts',(-15.6617873138256,-11.4907469171131,
-329.454969970058)) ;
#29371 = CARTESIAN_POINT('Ctrl Pts',(-15.4226885451021,-11.816812971764,-329.450181804934)) ;
#29372 = CARTESIAN_POINT('Ctrl Pts',(-15.1734265359729,-12.1353980561948,
-329.445409723845)) ;
#29373 = CARTESIAN_POINT('Ctrl Pts',(-14.9144754261016,-12.4458530080436,
-329.440597348569)) ;
#29374 = CARTESIAN_POINT('Ctrl Pts',(-14.6555243162303,-12.7563079598923,
-329.435784973292)) ;
#29375 = CARTESIAN_POINT('Ctrl Pts',(-14.3868839410984,-13.0586326534627,
-329.430932118053)) ;
#29376 = CARTESIAN_POINT('Ctrl Pts',(-14.109066607375,-13.3521980435425,-329.425963083603)) ;
#29377 = CARTESIAN_POINT('Ctrl Pts',(-13.8316284950075,-13.6453627161301,
-329.421000831897)) ;
#29378 = CARTESIAN_POINT('Ctrl Pts',(-13.5449657684854,-13.9298680937984,
-329.415921796234)) ;
#29379 = CARTESIAN_POINT('Ctrl Pts',(-13.2496752100234,-14.205172191667,-329.41080243354)) ;
#29380 = CARTESIAN_POINT('Ctrl Pts',(-12.9546083344793,-14.4802677463833,
-329.405686948768)) ;
#29381 = CARTESIAN_POINT('Ctrl Pts',(-12.6509268046961,-14.7461761153773,
-329.400531364346)) ;
#29382 = CARTESIAN_POINT('Ctrl Pts',(-12.3392477692486,-15.0023924175166,
-329.395392108602)) ;
#29383 = CARTESIAN_POINT('Ctrl Pts',(-12.0276021818338,-15.2585812236415,
-329.390253404379)) ;
#29384 = CARTESIAN_POINT('Ctrl Pts',(-11.7079608519094,-15.5050801572995,
-329.385131128978)) ;
#29385 = CARTESIAN_POINT('Ctrl Pts',(-11.3809612878261,-15.7414183236748,
-329.380059815457)) ;
#29386 = CARTESIAN_POINT('Ctrl Pts',(-11.0539815963396,-15.9777421271773,
-329.374988810132)) ;
#29387 = CARTESIAN_POINT('Ctrl Pts',(-10.7196445637678,-16.2039064638128,
-329.369968806655)) ;
#29388 = CARTESIAN_POINT('Ctrl Pts',(-10.3786078107617,-16.4194729930648,
-329.365011337746)) ;
#29389 = CARTESIAN_POINT('Ctrl Pts',(-10.0370377357319,-16.6353766307857,
-329.360046116219)) ;
#29390 = CARTESIAN_POINT('Ctrl Pts',(-9.68874692593803,-16.8406492921397,
-329.355143623485)) ;
#29391 = CARTESIAN_POINT('Ctrl Pts',(-9.33441673834071,-17.0348826399849,
-329.350292035931)) ;
#29392 = CARTESIAN_POINT('Ctrl Pts',(-8.98060350479251,-17.2288326088827,
-329.345447526656)) ;
#29393 = CARTESIAN_POINT('Ctrl Pts',(-8.62076844326921,-17.4117754128841,
-329.340653706852)) ;
#29394 = CARTESIAN_POINT('Ctrl Pts',(-8.25561127121673,-17.5833366889,-329.335876012712)) ;
#29395 = CARTESIAN_POINT('Ctrl Pts',(-7.88965380626628,-17.7552739653926,
-329.331087847589)) ;
#29396 = CARTESIAN_POINT('Ctrl Pts',(-7.5183507868964,-17.9157796444934,-329.326315766499)) ;
#29397 = CARTESIAN_POINT('Ctrl Pts',(-7.14242914390155,-18.064510518084,-329.321503391223)) ;
#29398 = CARTESIAN_POINT('Ctrl Pts',(-6.76650750090671,-18.2132413916746,
-329.316691015947)) ;
#29399 = CARTESIAN_POINT('Ctrl Pts',(-6.38596714995471,-18.3501972706682,
-329.311838160707)) ;
#29400 = CARTESIAN_POINT('Ctrl Pts',(-6.00155891284836,-18.4750708724202,
-329.306869126257)) ;
#29401 = CARTESIAN_POINT('Ctrl Pts',(-5.61714582334436,-18.5999460504558,
-329.301900029083)) ;
#29402 = CARTESIAN_POINT('Ctrl Pts',(-5.22876506703618,-18.7127705519045,
-329.296813838182)) ;
#29403 = CARTESIAN_POINT('Ctrl Pts',(-4.83720163750646,-18.8133536643378,
-329.291687298428)) ;
#29404 = CARTESIAN_POINT('Ctrl Pts',(-4.44269726062567,-18.9146922345483,
-329.286522254354)) ;
#29405 = CARTESIAN_POINT('Ctrl Pts',(-4.0449622374953,-19.0036049824047,-329.281316452944)) ;
#29406 = CARTESIAN_POINT('Ctrl Pts',(-3.64480127510044,-19.0799397939025,
-329.276127822886)) ;
#29407 = CARTESIAN_POINT('Ctrl Pts',(-3.24773361572114,-19.1556845260952,
-329.2709793017)) ;
#29408 = CARTESIAN_POINT('Ctrl Pts',(-2.84827736176992,-19.2190452047198,
-329.265847764364)) ;
#29409 = CARTESIAN_POINT('Ctrl Pts',(-2.44722057878536,-19.2699127853372,
-329.260767661831)) ;
#29410 = CARTESIAN_POINT('Ctrl Pts',(-2.04147722616975,-19.3213747816799,
-329.255628195498)) ;
#29411 = CARTESIAN_POINT('Ctrl Pts',(-1.63409567639069,-19.3600499784979,
-329.250541467613)) ;
#29412 = CARTESIAN_POINT('Ctrl Pts',(-1.2258943436162,-19.3858651114941,-329.245518998991)) ;
#29413 = CARTESIAN_POINT('Ctrl Pts',(-0.817693010841706,-19.4116802444903,
-329.240496530368)) ;
#29414 = CARTESIAN_POINT('Ctrl Pts',(-0.408671848873124,-19.4246353027172,
-329.235538311889)) ;
#29415 = CARTESIAN_POINT('Ctrl Pts',(0.00034766423293037,-19.4246965399752,
-329.230631277206)) ;
#29416 = CARTESIAN_POINT('Ctrl Pts',(0.000234860130568747,-19.4249999985802,
-329.019705201232)) ;
#29417 = CARTESIAN_POINT('Ctrl Pts',(-0.126046610261835,-19.4250015254004,
-329.021287160577)) ;
#29418 = CARTESIAN_POINT('Ctrl Pts',(-0.252325183923784,-19.4237716230069,
-329.022861695855)) ;
#29419 = CARTESIAN_POINT('Ctrl Pts',(-0.497313765973587,-19.4189960193607,
-329.025901815613)) ;
#29420 = CARTESIAN_POINT('Ctrl Pts',(-0.616021015960607,-19.415592845199,
-329.027368237702)) ;
#29421 = CARTESIAN_POINT('Ctrl Pts',(-0.860833286120161,-19.4063269595396,
-329.030379035671)) ;
#29422 = CARTESIAN_POINT('Ctrl Pts',(-0.986927450483557,-19.4003230453251,
-329.031922428832)) ;
#29423 = CARTESIAN_POINT('Ctrl Pts',(-1.29779130204551,-19.3824828132906,
-329.035710337357)) ;
#29424 = CARTESIAN_POINT('Ctrl Pts',(-1.48246744420815,-19.3692331466568,
-329.03794568431)) ;
#29425 = CARTESIAN_POINT('Ctrl Pts',(-2.16575504279031,-19.3103807931307,
-329.046170321658)) ;
#29426 = CARTESIAN_POINT('Ctrl Pts',(-2.66273693011824,-19.2481462644099,
-329.05205648756)) ;
#29427 = CARTESIAN_POINT('Ctrl Pts',(-3.77474229733379,-19.0649995822922,
-329.065233742579)) ;
#29428 = CARTESIAN_POINT('Ctrl Pts',(-4.38743975061462,-18.9333899647806,
-329.0724950833)) ;
#29429 = CARTESIAN_POINT('Ctrl Pts',(-5.08872671248827,-18.7468759528274,
-329.08120333217)) ;
#29430 = CARTESIAN_POINT('Ctrl Pts',(-5.18455191753345,-18.7206014573183,
-329.082402285589)) ;
#29431 = CARTESIAN_POINT('Ctrl Pts',(-5.33991150447989,-18.6767187633371,
-329.084363620134)) ;
#29432 = CARTESIAN_POINT('Ctrl Pts',(-5.39957052763507,-18.6595583213338,
-329.085120998125)) ;
#29433 = CARTESIAN_POINT('Ctrl Pts',(-5.52297683532595,-18.6234200838414,
-329.086697292404)) ;
#29434 = CARTESIAN_POINT('Ctrl Pts',(-5.586710808117,-18.6044003142872,-329.087516875054)) ;
#29435 = CARTESIAN_POINT('Ctrl Pts',(-5.74481467636614,-18.5563325740781,
-329.089563021076)) ;
#29436 = CARTESIAN_POINT('Ctrl Pts',(-5.83906310599182,-18.526891705618,-329.090794197824)) ;
#29437 = CARTESIAN_POINT('Ctrl Pts',(-6.23431758458721,-18.4001083704002,
-329.095999567488)) ;
#29438 = CARTESIAN_POINT('Ctrl Pts',(-6.53314649935522,-18.2961389348601,
-329.100037404475)) ;
#29439 = CARTESIAN_POINT('Ctrl Pts',(-7.22487132458085,-18.0363633532905,
-329.109529116724)) ;
#29440 = CARTESIAN_POINT('Ctrl Pts',(-7.61548811129174,-17.874940831897,-329.114999464136)) ;
#29441 = CARTESIAN_POINT('Ctrl Pts',(-8.29335589944453,-17.5685553684375,
-329.124567755624)) ;
#29442 = CARTESIAN_POINT('Ctrl Pts',(-8.58285359440435,-17.4289562096154,
-329.12867980861)) ;
#29443 = CARTESIAN_POINT('Ctrl Pts',(-9.02457781680675,-17.2022758719631,
-329.134968444941)) ;
#29444 = CARTESIAN_POINT('Ctrl Pts',(-9.17931211165127,-17.1202082120269,
-329.137174332155)) ;
#29445 = CARTESIAN_POINT('Ctrl Pts',(-9.4433807839012,-16.9755426773974,-329.140942054621)) ;
#29446 = CARTESIAN_POINT('Ctrl Pts',(-9.55325490127617,-16.9139531352362,
-329.1425107172)) ;
#29447 = CARTESIAN_POINT('Ctrl Pts',(-9.75414939261759,-16.7987603854043,
-329.145380519007)) ;
#29448 = CARTESIAN_POINT('Ctrl Pts',(-9.84534649879981,-16.7454750069123,
-329.146683920128)) ;
#29449 = CARTESIAN_POINT('Ctrl Pts',(-10.0448274114636,-16.6267277810303,
-329.149536571307)) ;
#29450 = CARTESIAN_POINT('Ctrl Pts',(-10.152915411835,-16.5609463231864,-329.151083340673)) ;
#29451 = CARTESIAN_POINT('Ctrl Pts',(-10.4189464164537,-16.3954586758336,
-329.154894109615)) ;
#29452 = CARTESIAN_POINT('Ctrl Pts',(-10.5761087717045,-16.2945215644385,
-329.157148679774)) ;
#29453 = CARTESIAN_POINT('Ctrl Pts',(-11.2217079366288,-15.8666114497986,
-329.166434849004)) ;
#29454 = CARTESIAN_POINT('Ctrl Pts',(-11.6966346693122,-15.5198204466108,
-329.173315766768)) ;
#29455 = CARTESIAN_POINT('Ctrl Pts',(-12.4536934339356,-14.9125006154747,
-329.184651691979)) ;
#29456 = CARTESIAN_POINT('Ctrl Pts',(-12.7451357523674,-14.6641968302286,
-329.189116228882)) ;
#29457 = CARTESIAN_POINT('Ctrl Pts',(-13.1408028699748,-14.3063841291079,
-329.195427485265)) ;
#29458 = CARTESIAN_POINT('Ctrl Pts',(-13.2513756455363,-14.2040265532576,
-329.197220005716)) ;
#29459 = CARTESIAN_POINT('Ctrl Pts',(-13.3642585895728,-14.097064969841,-329.19908573432)) ;
#29460 = CARTESIAN_POINT('Ctrl Pts',(-13.3677696945875,-14.0937355518455,
-329.199143802005)) ;
#29461 = CARTESIAN_POINT('Ctrl Pts',(-13.3737856463479,-14.0880266333443,
-329.199243357919)) ;
#29462 = CARTESIAN_POINT('Ctrl Pts',(-13.3762911025314,-14.0856477762512,
-329.199284838399)) ;
#29463 = CARTESIAN_POINT('Ctrl Pts',(-13.3838704089354,-14.0784476014184,
-329.19941037819)) ;
#29464 = CARTESIAN_POINT('Ctrl Pts',(-13.3889422878783,-14.0736242098798,
-329.199494462675)) ;
#29465 = CARTESIAN_POINT('Ctrl Pts',(-13.3984984242318,-14.0645264177258,
-329.199653035017)) ;
#29466 = CARTESIAN_POINT('Ctrl Pts',(-13.4029832460212,-14.0602526110279,
-329.199727515537)) ;
#29467 = CARTESIAN_POINT('Ctrl Pts',(-13.4114343038745,-14.0521914656687,
-329.199867979011)) ;
#29468 = CARTESIAN_POINT('Ctrl Pts',(-13.4154009821426,-14.048404591386,-329.199933956143)) ;
#29469 = CARTESIAN_POINT('Ctrl Pts',(-13.4228770996811,-14.0412613019108,
-329.200058395737)) ;
#29470 = CARTESIAN_POINT('Ctrl Pts',(-13.4263868850787,-14.0379052494973,
-329.200116853592)) ;
#29471 = CARTESIAN_POINT('Ctrl Pts',(-13.4330035202074,-14.0315736798233,
-329.200227129547)) ;
#29472 = CARTESIAN_POINT('Ctrl Pts',(-13.4361106407303,-14.0285984458985,
-329.200278944008)) ;
#29473 = CARTESIAN_POINT('Ctrl Pts',(-13.4419698702036,-14.0229841883633,
-329.200376709096)) ;
#29474 = CARTESIAN_POINT('Ctrl Pts',(-13.4447221910157,-14.0203453860793,
-329.200422656852)) ;
#29475 = CARTESIAN_POINT('Ctrl Pts',(-13.4499140189637,-14.0153647586434,
-329.200509374685)) ;
#29476 = CARTESIAN_POINT('Ctrl Pts',(-13.452353691896,-14.0130231065059,-329.200550142497)) ;
#29477 = CARTESIAN_POINT('Ctrl Pts',(-13.4569573188365,-14.008602133164,-329.200627105909)) ;
#29478 = CARTESIAN_POINT('Ctrl Pts',(-13.4591214026975,-14.0065229473171,
-329.200663299723)) ;
#29479 = CARTESIAN_POINT('Ctrl Pts',(-13.4632064246332,-14.0025963617682,
-329.200731648588)) ;
#29480 = CARTESIAN_POINT('Ctrl Pts',(-13.4651274645359,-14.0007490680566,
-329.20076380223)) ;
#29481 = CARTESIAN_POINT('Ctrl Pts',(-13.4687549837879,-13.9972593673283,
-329.200824540279)) ;
#29482 = CARTESIAN_POINT('Ctrl Pts',(-13.4704615430534,-13.9956170434423,
-329.200853123576)) ;
#29483 = CARTESIAN_POINT('Ctrl Pts',(-13.4736851815328,-13.9925136078305,
-329.200907133981)) ;
#29484 = CARTESIAN_POINT('Ctrl Pts',(-13.4752023235606,-13.9910525613866,
-329.200932560213)) ;
#29485 = CARTESIAN_POINT('Ctrl Pts',(-13.4780691361253,-13.9882908489626,
-329.200980619797)) ;
#29486 = CARTESIAN_POINT('Ctrl Pts',(-13.4794188561093,-13.986990234318,-329.201003252456)) ;
#29487 = CARTESIAN_POINT('Ctrl Pts',(-13.4819701456136,-13.9845310532327,
-329.201046044502)) ;
#29488 = CARTESIAN_POINT('Ctrl Pts',(-13.4831717541051,-13.983372527232,-329.201066203341)) ;
#29489 = CARTESIAN_POINT('Ctrl Pts',(-13.4854437931989,-13.9811813847254,
-329.201104329031)) ;
#29490 = CARTESIAN_POINT('Ctrl Pts',(-13.4865142545722,-13.9801488001144,
-329.201122295448)) ;
#29491 = CARTESIAN_POINT('Ctrl Pts',(-13.4885389211562,-13.9781953245404,
-329.201156284003)) ;
#29492 = CARTESIAN_POINT('Ctrl Pts',(-13.4894931506702,-13.9772744587981,
-329.201172305796)) ;
#29493 = CARTESIAN_POINT('Ctrl Pts',(-13.4912984845053,-13.9755318897551,
-329.201202623409)) ;
#29494 = CARTESIAN_POINT('Ctrl Pts',(-13.4921496081091,-13.9747102063683,
-329.201216918956)) ;
#29495 = CARTESIAN_POINT('Ctrl Pts',(-13.4937602971788,-13.9731549464448,
-329.201243976639)) ;
#29496 = CARTESIAN_POINT('Ctrl Pts',(-13.4945198778563,-13.972421385759,-329.201256738557)) ;
#29497 = CARTESIAN_POINT('Ctrl Pts',(-13.4959576813893,-13.9710326086315,
-329.201280898995)) ;
#29498 = CARTESIAN_POINT('Ctrl Pts',(-13.4966359163656,-13.9703774047219,
-329.201292297343)) ;
#29499 = CARTESIAN_POINT('Ctrl Pts',(-13.497920033498,-13.9691367120228,-329.201313880893)) ;
#29500 = CARTESIAN_POINT('Ctrl Pts',(-13.498525925335,-13.9685512331433,-329.201324065959)) ;
#29501 = CARTESIAN_POINT('Ctrl Pts',(-13.500890695743,-13.966265836113,-329.201363822469)) ;
#29502 = CARTESIAN_POINT('Ctrl Pts',(-13.5026492912326,-13.9645656252299,
-329.20139339796)) ;
#29503 = CARTESIAN_POINT('Ctrl Pts',(-13.5060934635385,-13.9612345390759,
-329.201451340562)) ;
#29504 = CARTESIAN_POINT('Ctrl Pts',(-13.5077790662557,-13.9596036905833,
-329.201479707301)) ;
#29505 = CARTESIAN_POINT('Ctrl Pts',(-13.5580221773944,-13.9109750292108,
-329.20232551594)) ;
#29506 = CARTESIAN_POINT('Ctrl Pts',(-13.6063343725602,-13.8637244835447,
-329.203146486416)) ;
#29507 = CARTESIAN_POINT('Ctrl Pts',(-13.6885866029149,-13.7824356404178,
-329.204558331305)) ;
#29508 = CARTESIAN_POINT('Ctrl Pts',(-13.7226486895035,-13.7485216772645,
-329.205147200894)) ;
#29509 = CARTESIAN_POINT('Ctrl Pts',(-13.8007238732929,-13.6702068058699,
-329.206507137861)) ;
#29510 = CARTESIAN_POINT('Ctrl Pts',(-13.8446491755584,-13.6257191640261,
-329.207279720744)) ;
#29511 = CARTESIAN_POINT('Ctrl Pts',(-13.9691498612876,-13.4984010264772,
-329.209489832114)) ;
#29512 = CARTESIAN_POINT('Ctrl Pts',(-14.049201894453,-13.4150625861286,-329.210935386781)) ;
#29513 = CARTESIAN_POINT('Ctrl Pts',(-14.4970275654825,-12.9404470026636,
-329.219148791015)) ;
#29514 = CARTESIAN_POINT('Ctrl Pts',(-14.8491956150212,-12.5347662675792,
-329.226090168281)) ;
#29515 = CARTESIAN_POINT('Ctrl Pts',(-15.5710466732553,-11.6300494945189,
-329.241021774506)) ;
#29516 = CARTESIAN_POINT('Ctrl Pts',(-15.9345359981257,-11.1268195428766,
-329.248994545562)) ;
#29517 = CARTESIAN_POINT('Ctrl Pts',(-16.3690329904371,-10.4602154831915,
-329.258984022886)) ;
#29518 = CARTESIAN_POINT('Ctrl Pts',(-16.4627545307046,-10.3120833194354,
-329.261170458734)) ;
#29519 = CARTESIAN_POINT('Ctrl Pts',(-16.6204567244288,-10.0551955165625,
-329.264904530834)) ;
#29520 = CARTESIAN_POINT('Ctrl Pts',(-16.6854062078596,-9.94704771943078,
-329.266459365622)) ;
#29521 = CARTESIAN_POINT('Ctrl Pts',(-16.818041072939,-9.72124178614683,-329.26967075392)) ;
#29522 = CARTESIAN_POINT('Ctrl Pts',(-16.8855560032346,-9.603491339979,-329.271325972388)) ;
#29523 = CARTESIAN_POINT('Ctrl Pts',(-17.0645445670757,-9.28359990869937,
-329.275772317734)) ;
#29524 = CARTESIAN_POINT('Ctrl Pts',(-17.1736582386741,-9.08016362778839,
-329.278546186021)) ;
#29525 = CARTESIAN_POINT('Ctrl Pts',(-17.6401858251183,-8.17184363294039,
-329.290721113284)) ;
#29526 = CARTESIAN_POINT('Ctrl Pts',(-17.9580128596447,-7.44747975160154,
-329.299846525682)) ;
#29527 = CARTESIAN_POINT('Ctrl Pts',(-18.3013067436693,-6.51417484900391,
-329.31153587164)) ;
#29528 = CARTESIAN_POINT('Ctrl Pts',(-18.3687573969846,-6.32147561813183,
-329.313948008058)) ;
#29529 = CARTESIAN_POINT('Ctrl Pts',(-18.4789553415451,-5.98998423307379,
-329.318117787057)) ;
#29530 = CARTESIAN_POINT('Ctrl Pts',(-18.5232067821707,-5.85171017963855,
-329.319863117471)) ;
#29531 = CARTESIAN_POINT('Ctrl Pts',(-18.5879842264298,-5.64119702708577,
-329.322537304368)) ;
#29532 = CARTESIAN_POINT('Ctrl Pts',(-18.6096482943204,-5.56931340865173,
-329.323453454193)) ;
#29533 = CARTESIAN_POINT('Ctrl Pts',(-18.6498895712344,-5.43293187960375,
-329.325198746452)) ;
#29534 = CARTESIAN_POINT('Ctrl Pts',(-18.668550258484,-5.36845983848395,-329.326026921109)) ;
#29535 = CARTESIAN_POINT('Ctrl Pts',(-18.7161239010457,-5.20084656551007,
-329.328187029729)) ;
#29536 = CARTESIAN_POINT('Ctrl Pts',(-18.744518528706,-5.09756058883894,-329.329524952954)) ;
#29537 = CARTESIAN_POINT('Ctrl Pts',(-18.9340199637367,-4.38524588410929,
-329.33878630526)) ;
#29538 = CARTESIAN_POINT('Ctrl Pts',(-19.0662705213906,-3.76892839954168,
-329.346958674151)) ;
#29539 = CARTESIAN_POINT('Ctrl Pts',(-19.2517110642867,-2.63951186555944,
-329.361711786254)) ;
#29540 = CARTESIAN_POINT('Ctrl Pts',(-19.3148732133948,-2.12863270367683,
-329.368306573883)) ;
#29541 = CARTESIAN_POINT('Ctrl Pts',(-19.3733345527792,-1.4282728158781,-329.377147957782)) ;
#29542 = CARTESIAN_POINT('Ctrl Pts',(-19.3862649088912,-1.24047892788992,
-329.379499989339)) ;
#29543 = CARTESIAN_POINT('Ctrl Pts',(-19.40340911906,-0.92453722504556,-329.383424571532)) ;
#29544 = CARTESIAN_POINT('Ctrl Pts',(-19.409087325017,-0.796482129985812,
-329.385006341726)) ;
#29545 = CARTESIAN_POINT('Ctrl Pts',(-19.4180377512594,-0.536511686249656,
-329.388199869549)) ;
#29546 = CARTESIAN_POINT('Ctrl Pts',(-19.4212340889775,-0.404600315161816,
-329.38981105662)) ;
#29547 = CARTESIAN_POINT('Ctrl Pts',(-19.4260311445044,-0.062887590516012,
-329.393962301736)) ;
#29548 = CARTESIAN_POINT('Ctrl Pts',(-19.4255773139515,0.146925479434508,
-329.396489122477)) ;
#29549 = CARTESIAN_POINT('Ctrl Pts',(-19.4162509773394,0.654743038639132,
-329.402561257111)) ;
#29550 = CARTESIAN_POINT('Ctrl Pts',(-19.4039167620585,0.952630647513047,
-329.406086443771)) ;
#29551 = CARTESIAN_POINT('Ctrl Pts',(-19.3479290612677,1.82079502743547,-329.416309169884)) ;
#29552 = CARTESIAN_POINT('Ctrl Pts',(-19.2859433831771,2.38956892535373,-329.422935304786)) ;
#29553 = CARTESIAN_POINT('Ctrl Pts',(-19.1789344061941,3.08487037432564,-329.431223676442)) ;
#29554 = CARTESIAN_POINT('Ctrl Pts',(-19.1575908769915,3.21475689959559,-329.432780617861)) ;
#29555 = CARTESIAN_POINT('Ctrl Pts',(-19.1064198175111,3.50752983442487,-329.436317591298)) ;
#29556 = CARTESIAN_POINT('Ctrl Pts',(-19.0758262616216,3.67027193388655,-329.438302974392)) ;
#29557 = CARTESIAN_POINT('Ctrl Pts',(-19.0276262464499,3.90976464252415,-329.441264587557)) ;
#29558 = CARTESIAN_POINT('Ctrl Pts',(-19.0116278932979,3.98683144371374,-329.442223747549)) ;
#29559 = CARTESIAN_POINT('Ctrl Pts',(-18.9812286249278,4.12892485006904,-329.444005185271)) ;
#29560 = CARTESIAN_POINT('Ctrl Pts',(-18.966960855422,4.19397858870562,-329.444825952714)) ;
#29561 = CARTESIAN_POINT('Ctrl Pts',(-18.9305629948807,4.35594904608031,-329.446881738122)) ;
#29562 = CARTESIAN_POINT('Ctrl Pts',(-18.9080229550369,4.45277164114303,-329.448121472296)) ;
#29563 = CARTESIAN_POINT('Ctrl Pts',(-18.8054594578311,4.87851523013988,-329.453614078224)) ;
#29564 = CARTESIAN_POINT('Ctrl Pts',(-18.7175892256608,5.20548451773665,-329.45794031994)) ;
#29565 = CARTESIAN_POINT('Ctrl Pts',(-18.4297523065071,6.17472227755628,-329.470940152228)) ;
#29566 = CARTESIAN_POINT('Ctrl Pts',(-18.2049283834514,6.809078681661,-329.479667819195)) ;
#29567 = CARTESIAN_POINT('Ctrl Pts',(-17.8442157184515,7.68034614028408,-329.491646923635)) ;
#29568 = CARTESIAN_POINT('Ctrl Pts',(-17.7355682358456,7.92801180864771,-329.495053692921)) ;
#29569 = CARTESIAN_POINT('Ctrl Pts',(-17.5617977989332,8.30266275922816,-329.500203035459)) ;
#29570 = CARTESIAN_POINT('Ctrl Pts',(-17.5003880386997,8.43133259866922,-329.501970857903)) ;
#29571 = CARTESIAN_POINT('Ctrl Pts',(-17.3827437547907,8.67100483424224,-329.505262622015)) ;
#29572 = CARTESIAN_POINT('Ctrl Pts',(-17.3268483205266,8.78216559878099,-329.506788892475)) ;
#29573 = CARTESIAN_POINT('Ctrl Pts',(-17.1974887996662,9.0333833386592,-329.510237900127)) ;
#29574 = CARTESIAN_POINT('Ctrl Pts',(-17.1233744423508,9.17309562559524,-329.51215580403)) ;
#29575 = CARTESIAN_POINT('Ctrl Pts',(-16.8696308244936,9.637631968042,-329.518536451193)) ;
#29576 = CARTESIAN_POINT('Ctrl Pts',(-16.6823992933428,9.95821011869755,-329.522944439844)) ;
#29577 = CARTESIAN_POINT('Ctrl Pts',(-16.4734472567714,10.2935286792378,-329.527595103698)) ;
#29578 = CARTESIAN_POINT('Ctrl Pts',(-16.4607590036743,10.3138067761155,-329.527876514739)) ;
#29579 = CARTESIAN_POINT('Ctrl Pts',(-16.1374153711969,10.8284511781678,-329.535023065582)) ;
#29580 = CARTESIAN_POINT('Ctrl Pts',(-15.8046657047995,11.3085839077288,-329.541786412174)) ;
#29581 = CARTESIAN_POINT('Ctrl Pts',(-15.3702417526816,11.878718769304,-329.550229940245)) ;
#29582 = CARTESIAN_POINT('Ctrl Pts',(-15.2886030453137,11.9836099739594,-329.551801842031)) ;
#29583 = CARTESIAN_POINT('Ctrl Pts',(-15.102183644944,12.2181197873783,-329.555366457079)) ;
#29584 = CARTESIAN_POINT('Ctrl Pts',(-14.9967983046114,12.3472443258574,-329.557364503377)) ;
#29585 = CARTESIAN_POINT('Ctrl Pts',(-14.8390991464197,12.5354690955653,-329.56034118974)) ;
#29586 = CARTESIAN_POINT('Ctrl Pts',(-14.7880658507319,12.5956324691032,-329.56130251395)) ;
#29587 = CARTESIAN_POINT('Ctrl Pts',(-14.693307992945,12.7059731822496,-329.563085520106)) ;
#29588 = CARTESIAN_POINT('Ctrl Pts',(-14.6496894294661,12.7562398013074,-329.563905660478)) ;
#29589 = CARTESIAN_POINT('Ctrl Pts',(-14.5405082472926,12.880763068274,-329.565956375087)) ;
#29590 = CARTESIAN_POINT('Ctrl Pts',(-14.4746343527734,12.9547442130536,-329.567191611471)) ;
#29591 = CARTESIAN_POINT('Ctrl Pts',(-14.1853759424155,13.2746415514943,-329.57260045997)) ;
#29592 = CARTESIAN_POINT('Ctrl Pts',(-13.9562694592616,13.5153076536035,-329.576844703964)) ;
#29593 = CARTESIAN_POINT('Ctrl Pts',(-13.6019245600803,13.8689084406734,-329.583279392369)) ;
#29594 = CARTESIAN_POINT('Ctrl Pts',(-13.4812035339259,13.9862834348667,-329.585450276993)) ;
#29595 = CARTESIAN_POINT('Ctrl Pts',(-13.0225004063363,14.4208154165743,-329.593601396861)) ;
#29596 = CARTESIAN_POINT('Ctrl Pts',(-12.6747284697147,14.7274129991098,-329.599582958634)) ;
#29597 = CARTESIAN_POINT('Ctrl Pts',(-12.2050356319801,15.1125259804316,-329.607319964546)) ;
#29598 = CARTESIAN_POINT('Ctrl Pts',(-12.0927366806281,15.2025345228885,-329.609145797043)) ;
#29599 = CARTESIAN_POINT('Ctrl Pts',(-11.8105346642878,15.4236162641598,-329.613672176451)) ;
#29600 = CARTESIAN_POINT('Ctrl Pts',(-11.6394402857428,15.5531378758439,-329.61636161435)) ;
#29601 = CARTESIAN_POINT('Ctrl Pts',(-11.3590349398232,15.758191124415,-329.620679426373)) ;
#29602 = CARTESIAN_POINT('Ctrl Pts',(-11.2510336382605,15.8354824494095,-329.622321519226)) ;
#29603 = CARTESIAN_POINT('Ctrl Pts',(-11.0389115975896,15.9840223492637,-329.625506410988)) ;
#29604 = CARTESIAN_POINT('Ctrl Pts',(-10.9348725019958,16.0553761442925,-329.627049990396)) ;
#29605 = CARTESIAN_POINT('Ctrl Pts',(-10.7023652046694,16.2115297441868,-329.630459720165)) ;
#29606 = CARTESIAN_POINT('Ctrl Pts',(-10.5735691368235,16.2958262574358,-329.632321941622)) ;
#29607 = CARTESIAN_POINT('Ctrl Pts',(-9.97721786341936,16.6760889606876,-329.64082948912)) ;
#29608 = CARTESIAN_POINT('Ctrl Pts',(-9.49815124838969,16.9535230515074,-329.647335031457)) ;
#29609 = CARTESIAN_POINT('Ctrl Pts',(-8.54061355179574,17.4547046982999,-329.659969082736)) ;
#29610 = CARTESIAN_POINT('Ctrl Pts',(-8.06356561379674,17.6801499752187,-329.666097009389)) ;
#29611 = CARTESIAN_POINT('Ctrl Pts',(-7.42263720389651,17.9516999052366,-329.674377280215)) ;
#29612 = CARTESIAN_POINT('Ctrl Pts',(-7.26648673273136,18.0154723211392,-329.676398810078)) ;
#29613 = CARTESIAN_POINT('Ctrl Pts',(-7.03579486704565,18.106200393726,-329.679403425369)) ;
#29614 = CARTESIAN_POINT('Ctrl Pts',(-6.96188722351389,18.1347464381203,-329.680368735014)) ;
#29615 = CARTESIAN_POINT('Ctrl Pts',(-6.82565549421285,18.1864089476938,-329.682154680872)) ;
#29616 = CARTESIAN_POINT('Ctrl Pts',(-6.7633835539294,18.2096591458001,-329.682973718172)) ;
#29617 = CARTESIAN_POINT('Ctrl Pts',(-6.60861307331499,18.2665416859719,-329.685015339672)) ;
#29618 = CARTESIAN_POINT('Ctrl Pts',(-6.51597598391044,18.2997914976492,-329.686242488885)) ;
#29619 = CARTESIAN_POINT('Ctrl Pts',(-6.12823723989252,18.4356433059545,-329.691394268673)) ;
#29620 = CARTESIAN_POINT('Ctrl Pts',(-5.8309351381501,18.531822104761,-329.695380968365)) ;
#29621 = CARTESIAN_POINT('Ctrl Pts',(-5.34904594947418,18.6749708733267,-329.70183735162)) ;
#29622 = CARTESIAN_POINT('Ctrl Pts',(-5.16586200375946,18.7264705537524,-329.704290569241)) ;
#29623 = CARTESIAN_POINT('Ctrl Pts',(-4.53445142570174,18.8940131010588,-329.712718020036)) ;
#29624 = CARTESIAN_POINT('Ctrl Pts',(-4.08284870326067,18.9967188896844,-329.718693126352)) ;
#29625 = CARTESIAN_POINT('Ctrl Pts',(-3.4867131694502,19.1100534330141,-329.726422667093)) ;
#29626 = CARTESIAN_POINT('Ctrl Pts',(-3.34512383873779,19.1353457638368,-329.728247357277)) ;
#29627 = CARTESIAN_POINT('Ctrl Pts',(-2.99171757097076,19.1944329162501,-329.732771433222)) ;
#29628 = CARTESIAN_POINT('Ctrl Pts',(-2.77959701936612,19.2262963058545,-329.735459714409)) ;
#29629 = CARTESIAN_POINT('Ctrl Pts',(-2.43536753442395,19.2721883275814,-329.739776175621)) ;
#29630 = CARTESIAN_POINT('Ctrl Pts',(-2.30356638045084,19.288386141651,-329.741418057993)) ;
#29631 = CARTESIAN_POINT('Ctrl Pts',(-2.04623715102699,19.3173356252656,-329.744602851125)) ;
#29632 = CARTESIAN_POINT('Ctrl Pts',(-1.92073036912962,19.3302182355755,-329.74614653903)) ;
#29633 = CARTESIAN_POINT('Ctrl Pts',(-1.64179812927608,19.3561057533673,-329.749556895494)) ;
#29634 = CARTESIAN_POINT('Ctrl Pts',(-1.48832548328144,19.3685110003754,-329.751419629746)) ;
#29635 = CARTESIAN_POINT('Ctrl Pts',(-0.782618687420034,19.4171160687365,
-329.759928377173)) ;
#29636 = CARTESIAN_POINT('Ctrl Pts',(-0.229142436903726,19.4315306616868,
-329.76643458717)) ;
#29637 = CARTESIAN_POINT('Ctrl Pts',(0.852082647786337,19.4134830869873,-329.779075691845)) ;
#29638 = CARTESIAN_POINT('Ctrl Pts',(1.37939265059248,19.3831536112505,-329.785209916209)) ;
#29639 = CARTESIAN_POINT('Ctrl Pts',(2.07217604052569,19.3148905002749,-329.7934914149)) ;
#29640 = CARTESIAN_POINT('Ctrl Pts',(2.2393213137948,19.2962262755618,-329.795507228865)) ;
#29641 = CARTESIAN_POINT('Ctrl Pts',(2.48473988405587,19.2655899701118,-329.798505049115)) ;
#29642 = CARTESIAN_POINT('Ctrl Pts',(2.56321622626901,19.2553060672706,-329.799469392061)) ;
#29643 = CARTESIAN_POINT('Ctrl Pts',(2.70749982302108,19.2355007898599,-329.801254618865)) ;
#29644 = CARTESIAN_POINT('Ctrl Pts',(2.77332511123636,19.2261206102772,-329.802073917687)) ;
#29645 = CARTESIAN_POINT('Ctrl Pts',(2.93661672440895,19.2019953161281,-329.804117716235)) ;
#29646 = CARTESIAN_POINT('Ctrl Pts',(3.03402137604771,19.1868459148034,-329.805346804255)) ;
#29647 = CARTESIAN_POINT('Ctrl Pts',(3.44139029456022,19.1203079232232,-329.810522829321)) ;
#29648 = CARTESIAN_POINT('Ctrl Pts',(3.75019931043715,19.0621443362934,-329.814532537657)) ;
#29649 = CARTESIAN_POINT('Ctrl Pts',(4.24142142460484,18.9572243412917,-329.820984351117)) ;
#29650 = CARTESIAN_POINT('Ctrl Pts',(4.42480165834261,18.9152621093813,-329.823409664787)) ;
#29651 = CARTESIAN_POINT('Ctrl Pts',(5.05736211567749,18.7608132273843,-329.831809789347)) ;
#29652 = CARTESIAN_POINT('Ctrl Pts',(5.50311082982857,18.6349348544389,-329.837785518647)) ;
#29653 = CARTESIAN_POINT('Ctrl Pts',(6.08087035233225,18.4492365463619,-329.845515779874)) ;
#29654 = CARTESIAN_POINT('Ctrl Pts',(6.21731269528264,18.4037044176976,-329.847340580353)) ;
#29655 = CARTESIAN_POINT('Ctrl Pts',(6.55593420055569,18.2865075806495,-329.85186487872)) ;
#29656 = CARTESIAN_POINT('Ctrl Pts',(6.75745590092216,18.2130014746607,-329.854553271605)) ;
#29657 = CARTESIAN_POINT('Ctrl Pts',(7.08169931576495,18.0886094871706,-329.85886986326)) ;
#29658 = CARTESIAN_POINT('Ctrl Pts',(7.20518863757643,18.0397759169091,-329.860511765958)) ;
#29659 = CARTESIAN_POINT('Ctrl Pts',(7.44500765626171,17.9420846866245,-329.863696568602)) ;
#29660 = CARTESIAN_POINT('Ctrl Pts',(7.56138131868501,17.8933522433812,-329.865240246017)) ;
#29661 = CARTESIAN_POINT('Ctrl Pts',(7.81870035685193,17.7826391310795,-329.86865054191)) ;
#29662 = CARTESIAN_POINT('Ctrl Pts',(7.95940031105361,17.7201093819379,-329.870513226602)) ;
#29663 = CARTESIAN_POINT('Ctrl Pts',(8.60234784879894,17.4251684223834,-329.879021872229)) ;
#29664 = CARTESIAN_POINT('Ctrl Pts',(9.09526374345616,17.1730329928343,-329.885528031184)) ;
#29665 = CARTESIAN_POINT('Ctrl Pts',(10.0360385137874,16.6399293712994,-329.898168508318)) ;
#29666 = CARTESIAN_POINT('Ctrl Pts',(10.4845341954365,16.3610469968299,-329.904302164253)) ;
#29667 = CARTESIAN_POINT('Ctrl Pts',(10.9883381970162,16.0185410370371,-329.911549411892)) ;
#29668 = CARTESIAN_POINT('Ctrl Pts',(11.0552776022657,15.9724159227267,-329.912520029171)) ;
#29669 = CARTESIAN_POINT('Ctrl Pts',(11.2190410091295,15.8580507939716,-329.914915749324)) ;
#29670 = CARTESIAN_POINT('Ctrl Pts',(11.3155340792936,15.7893427535045,-329.916345719318)) ;
#29671 = CARTESIAN_POINT('Ctrl Pts',(11.4679435376613,15.6787046432279,-329.918638322728)) ;
#29672 = CARTESIAN_POINT('Ctrl Pts',(11.5242725878605,15.6373479077846,-329.919493140801)) ;
#29673 = CARTESIAN_POINT('Ctrl Pts',(11.6308543099371,15.5582070236111,-329.921126028849)) ;
#29674 = CARTESIAN_POINT('Ctrl Pts',(11.6811490893172,15.5204811043532,-329.921903147994)) ;
#29675 = CARTESIAN_POINT('Ctrl Pts',(11.8249685551808,15.411507602585,-329.924143179281)) ;
#29676 = CARTESIAN_POINT('Ctrl Pts',(11.9180306606808,15.3396542668313,-329.925614450232)) ;
#29677 = CARTESIAN_POINT('Ctrl Pts',(12.530944631856,14.8574781905786,-329.935434095091)) ;
#29678 = CARTESIAN_POINT('Ctrl Pts',(13.0301727123745,14.4216445271644,-329.944041450593)) ;
#29679 = CARTESIAN_POINT('Ctrl Pts',(13.7527387155712,13.7226274193422,-329.956986459446)) ;
#29680 = CARTESIAN_POINT('Ctrl Pts',(13.9929517170713,13.4775972776863,-329.961383478991)) ;
#29681 = CARTESIAN_POINT('Ctrl Pts',(14.3980848492097,13.0418267506142,-329.968928244738)) ;
#29682 = CARTESIAN_POINT('Ctrl Pts',(14.5660147501345,12.8539996491689,-329.972097133833)) ;
#29683 = CARTESIAN_POINT('Ctrl Pts',(14.8211459938935,12.5572170883597,-329.976972598279)) ;
#29684 = CARTESIAN_POINT('Ctrl Pts',(14.9109068062645,12.4504991007317,-329.978700289798)) ;
#29685 = CARTESIAN_POINT('Ctrl Pts',(15.0789347481953,12.2463045845789,-329.98195841114)) ;
#29686 = CARTESIAN_POINT('Ctrl Pts',(15.1574252350588,12.1490209239088,-329.983490662288)) ;
#29687 = CARTESIAN_POINT('Ctrl Pts',(15.3364476016038,11.9226991496856,-329.987010323259)) ;
#29688 = CARTESIAN_POINT('Ctrl Pts',(15.4362995158311,11.7931351814819,-329.988992106712)) ;
#29689 = CARTESIAN_POINT('Ctrl Pts',(15.7877770424613,11.3249585053423,-329.996041309069)) ;
#29690 = CARTESIAN_POINT('Ctrl Pts',(16.0299939242519,10.979430084686,-330.00103525652)) ;
#29691 = CARTESIAN_POINT('Ctrl Pts',(16.5620966495462,10.1651854458793,-330.012452887739)) ;
#29692 = CARTESIAN_POINT('Ctrl Pts',(16.8436746087177,9.69147381567583,-330.018838674233)) ;
#29693 = CARTESIAN_POINT('Ctrl Pts',(17.1660121301032,9.09259953020383,-330.026854255297)) ;
#29694 = CARTESIAN_POINT('Ctrl Pts',(17.2261467234629,8.97815168514524,-330.028383985516)) ;
#29695 = CARTESIAN_POINT('Ctrl Pts',(17.3597854876978,8.71752495064118,-330.031870509975)) ;
#29696 = CARTESIAN_POINT('Ctrl Pts',(17.432594262541,8.5710005586371,-330.033832684312)) ;
#29697 = CARTESIAN_POINT('Ctrl Pts',(17.5375289033438,8.35295439600053,-330.036766648313)) ;
#29698 = CARTESIAN_POINT('Ctrl Pts',(17.5710869078076,8.28212967992373,-330.037721814283)) ;
#29699 = CARTESIAN_POINT('Ctrl Pts',(17.6324060024832,8.15066446374064,-330.039500411068)) ;
#29700 = CARTESIAN_POINT('Ctrl Pts',(17.6602851247482,8.09008046395288,-330.040322389622)) ;
#29701 = CARTESIAN_POINT('Ctrl Pts',(17.7292190593585,7.93822600730525,-330.042387788954)) ;
#29702 = CARTESIAN_POINT('Ctrl Pts',(17.7698815436645,7.84677962494043,-330.043636028261)) ;
#29703 = CARTESIAN_POINT('Ctrl Pts',(17.9587281726829,7.41308299936894,-330.049569896015)) ;
#29704 = CARTESIAN_POINT('Ctrl Pts',(18.0977421370436,7.0669261867291,-330.054345337509)) ;
#29705 = CARTESIAN_POINT('Ctrl Pts',(18.3726347461828,6.32099814188781,-330.064578500043)) ;
#29706 = CARTESIAN_POINT('Ctrl Pts',(18.5056218614875,5.92036189891185,-330.070039834706)) ;
#29707 = CARTESIAN_POINT('Ctrl Pts',(18.7078947623865,5.23732697135032,-330.079184498698)) ;
#29708 = CARTESIAN_POINT('Ctrl Pts',(18.7840839296965,4.95712735499223,-330.082890437858)) ;
#29709 = CARTESIAN_POINT('Ctrl Pts',(18.9082752036702,4.45630704415951,-330.089414286316)) ;
#29710 = CARTESIAN_POINT('Ctrl Pts',(18.9587659637942,4.23635893725976,-330.092245753194)) ;
#29711 = CARTESIAN_POINT('Ctrl Pts',(19.0332794884967,3.88369256885976,-330.096729320622)) ;
#29712 = CARTESIAN_POINT('Ctrl Pts',(19.059772072674,3.75151764677148,-330.098397204061)) ;
#29713 = CARTESIAN_POINT('Ctrl Pts',(19.108463893334,3.4947456211699,-330.101613405512)) ;
#29714 = CARTESIAN_POINT('Ctrl Pts',(19.1308255109528,3.37018614293166,-330.10316271848)) ;
#29715 = CARTESIAN_POINT('Ctrl Pts',(19.1817059851789,3.06992850458334,-330.106872330538)) ;
#29716 = CARTESIAN_POINT('Ctrl Pts',(19.2090302010524,2.89403945852976,-330.109024756651)) ;
#29717 = CARTESIAN_POINT('Ctrl Pts',(19.3370075946335,1.98834035795882,-330.120013319429)) ;
#29718 = CARTESIAN_POINT('Ctrl Pts',(19.3985007088822,1.25360707187879,-330.128586401666)) ;
#29719 = CARTESIAN_POINT('Ctrl Pts',(19.4289544576065,0.110147357720164,-330.141957838631)) ;
#29720 = CARTESIAN_POINT('Ctrl Pts',(19.4269948692778,-0.297107080162094,
-330.146731886919)) ;
#29721 = CARTESIAN_POINT('Ctrl Pts',(19.4079079471966,-0.823415874174811,
-330.153047216981)) ;
#29722 = CARTESIAN_POINT('Ctrl Pts',(19.4024753011762,-0.9427919776234,-330.154489529161)) ;
#29723 = CARTESIAN_POINT('Ctrl Pts',(19.3921094443329,-1.13209018345098,-330.1567970516)) ;
#29724 = CARTESIAN_POINT('Ctrl Pts',(19.3878986820907,-1.20204890547807,-330.157654271325)) ;
#29725 = CARTESIAN_POINT('Ctrl Pts',(19.3792037612119,-1.33454777108671,-330.159287389927)) ;
#29726 = CARTESIAN_POINT('Ctrl Pts',(19.3747952291614,-1.39709197583418,-330.160062297965)) ;
#29727 = CARTESIAN_POINT('Ctrl Pts',(19.361323142618,-1.57587588909988,-330.162287785291)) ;
#29728 = CARTESIAN_POINT('Ctrl Pts',(19.3515157696895,-1.69205673864896,-330.163746561227)) ;
#29729 = CARTESIAN_POINT('Ctrl Pts',(19.3074242499004,-2.1636785377513,-330.169709887209)) ;
#29730 = CARTESIAN_POINT('Ctrl Pts',(19.2643881515232,-2.51823040209902,-330.174287874772)) ;
#29731 = CARTESIAN_POINT('Ctrl Pts',(19.1321730462123,-3.40284075193063,-330.185806709429)) ;
#29732 = CARTESIAN_POINT('Ctrl Pts',(19.0307241587448,-3.93076461554458,-330.192764279617)) ;
#29733 = CARTESIAN_POINT('Ctrl Pts',(18.8717201503551,-4.60577697688609,-330.201614460744)) ;
#29734 = CARTESIAN_POINT('Ctrl Pts',(18.8340902751248,-4.75731505957141,-330.203598861156)) ;
#29735 = CARTESIAN_POINT('Ctrl Pts',(18.737317073765,-5.12786829685356,-330.208441729512)) ;
#29736 = CARTESIAN_POINT('Ctrl Pts',(18.6761561933707,-5.34633280887128,-330.211288527478)) ;
#29737 = CARTESIAN_POINT('Ctrl Pts',(18.5725122925584,-5.69303443887426,-330.215789968112)) ;
#29738 = CARTESIAN_POINT('Ctrl Pts',(18.5324939498157,-5.82198609062626,-330.217460622785)) ;
#29739 = CARTESIAN_POINT('Ctrl Pts',(18.4523984751142,-6.07088175785231,-330.220678468924)) ;
#29740 = CARTESIAN_POINT('Ctrl Pts',(18.4124880041225,-6.19087234153317,-330.222226696371)) ;
#29741 = CARTESIAN_POINT('Ctrl Pts',(18.3137968376767,-6.47818806682719,-330.225927486203)) ;
#29742 = CARTESIAN_POINT('Ctrl Pts',(18.2538907121145,-6.6451146895395,-330.228072277041)) ;
#29743 = CARTESIAN_POINT('Ctrl Pts',(17.9320982838824,-7.50457492864761,-330.239098476883)) ;
#29744 = CARTESIAN_POINT('Ctrl Pts',(17.6330591901992,-8.18254346902189,-330.24771337926)) ;
#29745 = CARTESIAN_POINT('Ctrl Pts',(17.1115484562098,-9.20270851882717,-330.261107227162)) ;
#29746 = CARTESIAN_POINT('Ctrl Pts',(16.9157906619508,-9.55776958613195,-330.265860643072)) ;
#29747 = CARTESIAN_POINT('Ctrl Pts',(16.6482306281246,-10.0090595496097,-330.272152113662)) ;
#29748 = CARTESIAN_POINT('Ctrl Pts',(16.58644851546,-10.1111117932829,-330.27359202634)) ;
#29749 = CARTESIAN_POINT('Ctrl Pts',(16.486904582115,-10.2721715620907,-330.275896646844)) ;
#29750 = CARTESIAN_POINT('Ctrl Pts',(16.4497568097972,-10.3315551681954,-330.276753398276)) ;
#29751 = CARTESIAN_POINT('Ctrl Pts',(16.3787324048448,-10.4437390382676,-330.278386462983)) ;
#29752 = CARTESIAN_POINT('Ctrl Pts',(16.3449196062418,-10.4965786494179,-330.279161793123)) ;
#29753 = CARTESIAN_POINT('Ctrl Pts',(16.2474314927806,-10.6473110342797,-330.281390062468)) ;
#29754 = CARTESIAN_POINT('Ctrl Pts',(16.1831286178432,-10.7447945746771,-330.282851229269)) ;
#29755 = CARTESIAN_POINT('Ctrl Pts',(15.7466166015083,-11.3937411615886,-330.292697711069)) ;
#29756 = CARTESIAN_POINT('Ctrl Pts',(15.347165847278,-11.9263478388706,-330.30134540886)) ;
#29757 = CARTESIAN_POINT('Ctrl Pts',(14.7020796762253,-12.7002587857508,-330.314317731273)) ;
#29758 = CARTESIAN_POINT('Ctrl Pts',(14.476074232971,-12.9572757744647,-330.318703156046)) ;
#29759 = CARTESIAN_POINT('Ctrl Pts',(14.0723804993433,-13.3926095285967,-330.326231120311)) ;
#29760 = CARTESIAN_POINT('Ctrl Pts',(13.897797527134,-13.5736917292507,-330.329394662299)) ;
#29761 = CARTESIAN_POINT('Ctrl Pts',(13.621083254794,-13.8497704134581,-330.334263945175)) ;
#29762 = CARTESIAN_POINT('Ctrl Pts',(13.5213625299281,-13.9471432537138,-330.335990712906)) ;
#29763 = CARTESIAN_POINT('Ctrl Pts',(13.3302232323978,-14.1298054449018,-330.339248102491)) ;
#29764 = CARTESIAN_POINT('Ctrl Pts',(13.2390122540193,-14.2153018934401,-330.340780533645)) ;
#29765 = CARTESIAN_POINT('Ctrl Pts',(13.0264656530984,-14.4107119350479,-330.344302045213)) ;
#29766 = CARTESIAN_POINT('Ctrl Pts',(12.9045530645632,-14.5199840286034,-330.346285478662)) ;
#29767 = CARTESIAN_POINT('Ctrl Pts',(12.450911539559,-14.9163632034542,-330.353539056599)) ;
#29768 = CARTESIAN_POINT('Ctrl Pts',(12.1108648617341,-15.1937501258125,-330.358728467319)) ;
#29769 = CARTESIAN_POINT('Ctrl Pts',(11.3341713003241,-15.7846695223877,-330.370176712069)) ;
#29770 = CARTESIAN_POINT('Ctrl Pts',(10.8933149469342,-16.0920762802304,-330.376406960397)) ;
#29771 = CARTESIAN_POINT('Ctrl Pts',(10.3325948795987,-16.449450337789,-330.384245305199)) ;
#29772 = CARTESIAN_POINT('Ctrl Pts',(10.2242296705161,-16.5170233686163,-330.385756720922)) ;
#29773 = CARTESIAN_POINT('Ctrl Pts',(9.97667259589361,-16.6680220954688,-330.389209164512)) ;
#29774 = CARTESIAN_POINT('Ctrl Pts',(9.83708585449466,-16.7507820238262,-330.391155589243)) ;
#29775 = CARTESIAN_POINT('Ctrl Pts',(9.62876909556282,-16.8707894540805,-330.394070773089)) ;
#29776 = CARTESIAN_POINT('Ctrl Pts',(9.56082467379982,-16.9093868202285,-330.395023208434)) ;
#29777 = CARTESIAN_POINT('Ctrl Pts',(9.43440719750226,-16.9801955876855,-330.396799904291)) ;
#29778 = CARTESIAN_POINT('Ctrl Pts',(9.37599753475988,-17.0125174961228,-330.397622752435)) ;
#29779 = CARTESIAN_POINT('Ctrl Pts',(9.22919724359832,-17.0927660989602,-330.399694922638)) ;
#29780 = CARTESIAN_POINT('Ctrl Pts',(9.14059896808375,-17.1403087819225,-330.400949135163)) ;
#29781 = CARTESIAN_POINT('Ctrl Pts',(8.72895003226867,-17.3571041041459,-330.406786052973)) ;
#29782 = CARTESIAN_POINT('Ctrl Pts',(8.40154287486246,-17.5179253327682,-330.411454153591)) ;
#29783 = CARTESIAN_POINT('Ctrl Pts',(7.95537784495177,-17.721693279478,-330.417766639287)) ;
#29784 = CARTESIAN_POINT('Ctrl Pts',(7.84044697423284,-17.7728399694747,-330.419388607912)) ;
#29785 = CARTESIAN_POINT('Ctrl Pts',(7.29560097256129,-18.0089944781337,-330.427048879598)) ;
#29786 = CARTESIAN_POINT('Ctrl Pts',(6.8595871410745,-18.1795418331174,-330.433090521909)) ;
#29787 = CARTESIAN_POINT('Ctrl Pts',(6.2812378385883,-18.3819918070808,-330.44089693956)) ;
#29788 = CARTESIAN_POINT('Ctrl Pts',(6.14410566080346,-18.4282809092375,-330.44273334278)) ;
#29789 = CARTESIAN_POINT('Ctrl Pts',(5.80161605941945,-18.5396407017903,-330.447281021887)) ;
#29790 = CARTESIAN_POINT('Ctrl Pts',(5.5956692156963,-18.6028361416602,-330.449981147973)) ;
#29791 = CARTESIAN_POINT('Ctrl Pts',(5.26097648977465,-18.6994766922756,-330.454311441326)) ;
#29792 = CARTESIAN_POINT('Ctrl Pts',(5.13286383151931,-18.7350476683488,-330.455955479026)) ;
#29793 = CARTESIAN_POINT('Ctrl Pts',(4.8825852219394,-18.8017786189703,-330.459141295461)) ;
#29794 = CARTESIAN_POINT('Ctrl Pts',(4.76046108048249,-18.8330700640084,-330.460683885563)) ;
#29795 = CARTESIAN_POINT('Ctrl Pts',(4.48895598576786,-18.8998272263996,-330.464087882715)) ;
#29796 = CARTESIAN_POINT('Ctrl Pts',(4.33944161609734,-18.934715249318,-330.465945410294)) ;
#29797 = CARTESIAN_POINT('Ctrl Pts',(3.72773599019687,-19.0698260660903,-330.473481372213)) ;
#29798 = CARTESIAN_POINT('Ctrl Pts',(3.2623712842438,-19.1549266967292,-330.479062504468)) ;
#29799 = CARTESIAN_POINT('Ctrl Pts',(2.29855048969756,-19.2950334940898,-330.490469943193)) ;
#29800 = CARTESIAN_POINT('Ctrl Pts',(1.8001337712822,-19.3478983106631,-330.496286567124)) ;
#29801 = CARTESIAN_POINT('Ctrl Pts',(1.12885643116695,-19.3929319654646,-330.504222820823)) ;
#29802 = CARTESIAN_POINT('Ctrl Pts',(0.957335222378236,-19.4021554525485,
-330.506260143751)) ;
#29803 = CARTESIAN_POINT('Ctrl Pts',(0.657234931424957,-19.4143040385478,
-330.50985544195)) ;
#29804 = CARTESIAN_POINT('Ctrl Pts',(0.528707000938554,-19.4182292675448,
-330.511405105086)) ;
#29805 = CARTESIAN_POINT('Ctrl Pts',(0.328274487591244,-19.4223589995926,
-330.51384282867)) ;
#29806 = CARTESIAN_POINT('Ctrl Pts',(0.25639159959772,-19.4234409047298,-330.514721326051)) ;
#29807 = CARTESIAN_POINT('Ctrl Pts',(0.123021396673552,-19.4247077517276,
-330.516360385086)) ;
#29808 = CARTESIAN_POINT('Ctrl Pts',(0.0615360145035663,-19.4249998405387,
-330.517119637573)) ;
#29809 = CARTESIAN_POINT('Ctrl Pts',(5.03575626769576E-5,-19.4249999999347,
-330.517882160562)) ;
#29810 = CARTESIAN_POINT('Origin',(0.,0.,-328.125)) ;
#29811 = CARTESIAN_POINT('',(-0.000189941651959998,-19.4249999990714,-332.23026054535)) ;
#29812 = CARTESIAN_POINT('',(-0.000307709618470118,-19.4249998857984,-332.019601644739)) ;
#29813 = CARTESIAN_POINT('',(-2.37887640734373E-15,-19.425,-328.125)) ;
#29814 = CARTESIAN_POINT('Ctrl Pts',(-0.000189941651381996,-19.4249999990714,
-332.23026054535)) ;
#29815 = CARTESIAN_POINT('Ctrl Pts',(0.145183061578013,-19.4250014205585,
-332.228446617012)) ;
#29816 = CARTESIAN_POINT('Ctrl Pts',(0.290551611289528,-19.4233709264318,
-332.22664282915)) ;
#29817 = CARTESIAN_POINT('Ctrl Pts',(0.559970945372767,-19.4173237550444,
-332.223318412199)) ;
#29818 = CARTESIAN_POINT('Ctrl Pts',(0.684024165112581,-19.4133495372617,
-332.221795018015)) ;
#29819 = CARTESIAN_POINT('Ctrl Pts',(0.964611173299925,-19.4016677163885,
-332.21836521505)) ;
#29820 = CARTESIAN_POINT('Ctrl Pts',(1.1211069864383,-19.3932540876237,-332.216463457601)) ;
#29821 = CARTESIAN_POINT('Ctrl Pts',(1.64778164968142,-19.3585422135905,-332.210096697832)) ;
#29822 = CARTESIAN_POINT('Ctrl Pts',(2.01730434183639,-19.3235303464314,-332.205686909149)) ;
#29823 = CARTESIAN_POINT('Ctrl Pts',(3.11839476728218,-19.1872732378065,-332.192621682752)) ;
#29824 = CARTESIAN_POINT('Ctrl Pts',(3.8454224700446,-19.0548828285682,-332.184113525765)) ;
#29825 = CARTESIAN_POINT('Ctrl Pts',(4.73247214919932,-18.8405063487433,-332.173265741295)) ;
#29826 = CARTESIAN_POINT('Ctrl Pts',(4.901243260989,-18.7973079573857,-332.171179181993)) ;
#29827 = CARTESIAN_POINT('Ctrl Pts',(5.14677633285928,-18.7309300718365,-332.168097389376)) ;
#29828 = CARTESIAN_POINT('Ctrl Pts',(5.22401227178006,-18.7095361711371,-332.167121233573)) ;
#29829 = CARTESIAN_POINT('Ctrl Pts',(5.3584339170233,-18.6714049008776,-332.165408952922)) ;
#29830 = CARTESIAN_POINT('Ctrl Pts',(5.4156790013102,-18.6548812901269,-332.164675401307)) ;
#29831 = CARTESIAN_POINT('Ctrl Pts',(5.56061613963103,-18.6123222825573,-332.162807406222)) ;
#29832 = CARTESIAN_POINT('Ctrl Pts',(5.64820188983442,-18.5859303771073,-332.161668718322)) ;
#29833 = CARTESIAN_POINT('Ctrl Pts',(5.98412901790217,-18.4821127610899,-332.157267863808)) ;
#29834 = CARTESIAN_POINT('Ctrl Pts',(6.2310918948355,-18.4003202570807,-332.153962142931)) ;
#29835 = CARTESIAN_POINT('Ctrl Pts',(7.00055523704415,-18.1282106884239,-332.143514486035)) ;
#29836 = CARTESIAN_POINT('Ctrl Pts',(7.51657217514077,-17.920405691037,-332.136297820485)) ;
#29837 = CARTESIAN_POINT('Ctrl Pts',(8.37952140627743,-17.5290481232115,-332.124134920143)) ;
#29838 = CARTESIAN_POINT('Ctrl Pts',(8.7311104163697,-17.3566016034502,-332.119149427255)) ;
#29839 = CARTESIAN_POINT('Ctrl Pts',(9.23199444589439,-17.0918559530118,-332.112037175361)) ;
#29840 = CARTESIAN_POINT('Ctrl Pts',(9.38562827163967,-17.0079758772757,-332.109853938412)) ;
#29841 = CARTESIAN_POINT('Ctrl Pts',(9.64797072652297,-16.8601064763324,-332.106123510751)) ;
#29842 = CARTESIAN_POINT('Ctrl Pts',(9.75722826446648,-16.7971136263695,-332.104569159518)) ;
#29843 = CARTESIAN_POINT('Ctrl Pts',(9.98286204189661,-16.6640792528831,-332.101357184621)) ;
#29844 = CARTESIAN_POINT('Ctrl Pts',(10.0991327673247,-16.593872040654,-332.099700912792)) ;
#29845 = CARTESIAN_POINT('Ctrl Pts',(10.4114274206998,-16.4008024436098,-332.095247491828)) ;
#29846 = CARTESIAN_POINT('Ctrl Pts',(10.6060085039264,-16.275648239215,-332.092467702735)) ;
#29847 = CARTESIAN_POINT('Ctrl Pts',(10.9319162620003,-16.057698045176,-332.087793320668)) ;
#29848 = CARTESIAN_POINT('Ctrl Pts',(11.0644105451957,-15.9666928017923,-332.08588761199)) ;
#29849 = CARTESIAN_POINT('Ctrl Pts',(11.6606826503562,-15.5461499688412,-332.077273464015)) ;
#29850 = CARTESIAN_POINT('Ctrl Pts',(12.1109744539353,-15.1979799924377,-332.070671742748)) ;
#29851 = CARTESIAN_POINT('Ctrl Pts',(12.8105859332824,-14.6061705364964,-332.059929377883)) ;
#29852 = CARTESIAN_POINT('Ctrl Pts',(13.0697697607249,-14.374715546004,-332.0558308824)) ;
#29853 = CARTESIAN_POINT('Ctrl Pts',(13.3947723799751,-14.0684232067241,-332.050451049101)) ;
#29854 = CARTESIAN_POINT('Ctrl Pts',(13.4664170002983,-13.9998597053941,-332.049249387131)) ;
#29855 = CARTESIAN_POINT('Ctrl Pts',(13.5852722199482,-13.8843593608555,-332.047226546011)) ;
#29856 = CARTESIAN_POINT('Ctrl Pts',(13.6327722284112,-13.8377229892832,-332.04641009854)) ;
#29857 = CARTESIAN_POINT('Ctrl Pts',(13.7360014314585,-13.7353232493974,-332.044617367667)) ;
#29858 = CARTESIAN_POINT('Ctrl Pts',(13.7916326485883,-13.6794630360962,-332.043639586189)) ;
#29859 = CARTESIAN_POINT('Ctrl Pts',(13.9635761062621,-13.5046967410677,-332.040583335402)) ;
#29860 = CARTESIAN_POINT('Ctrl Pts',(14.0787021108828,-13.384634416601,-332.038487861583)) ;
#29861 = CARTESIAN_POINT('Ctrl Pts',(14.2827527636636,-13.1662887475904,-332.034696095332)) ;
#29862 = CARTESIAN_POINT('Ctrl Pts',(14.3722406182465,-13.0685456517839,-332.033005341881)) ;
#29863 = CARTESIAN_POINT('Ctrl Pts',(14.8480758432325,-12.5380154714742,-332.023879596559)) ;
#29864 = CARTESIAN_POINT('Ctrl Pts',(15.2158886002915,-12.0890001132909,-332.016346844542)) ;
#29865 = CARTESIAN_POINT('Ctrl Pts',(15.7319625990933,-11.3980546067838,-332.005289862359)) ;
#29866 = CARTESIAN_POINT('Ctrl Pts',(15.8959224334734,-11.1682561957224,-332.001692856113)) ;
#29867 = CARTESIAN_POINT('Ctrl Pts',(16.1745491797759,-10.7591738876472,-331.995444926376)) ;
#29868 = CARTESIAN_POINT('Ctrl Pts',(16.2913865873953,-10.5814265199878,-331.992779600584)) ;
#29869 = CARTESIAN_POINT('Ctrl Pts',(16.4762155032514,-10.2899220178838,-331.988489948021)) ;
#29870 = CARTESIAN_POINT('Ctrl Pts',(16.5460032924671,-10.1773251665681,-331.986852242614)) ;
#29871 = CARTESIAN_POINT('Ctrl Pts',(16.680859824846,-9.95469134763043,-331.983651304628)) ;
#29872 = CARTESIAN_POINT('Ctrl Pts',(16.7460049393203,-9.84470837279573,-331.982087549643)) ;
#29873 = CARTESIAN_POINT('Ctrl Pts',(16.9033149498739,-9.57304552699521,-331.978266718079)) ;
#29874 = CARTESIAN_POINT('Ctrl Pts',(16.9942510935242,-9.41066877916073,-331.976018807149)) ;
#29875 = CARTESIAN_POINT('Ctrl Pts',(17.1386599867603,-9.14388914501315,-331.972379375948)) ;
#29876 = CARTESIAN_POINT('Ctrl Pts',(17.1935450362668,-9.04026459545534,-331.970978696809)) ;
#29877 = CARTESIAN_POINT('Ctrl Pts',(17.4015354542087,-8.63882632729048,-331.965598756246)) ;
#29878 = CARTESIAN_POINT('Ctrl Pts',(17.547868631977,-8.33756939353622,-331.961659792414)) ;
#29879 = CARTESIAN_POINT('Ctrl Pts',(17.9709482516761,-7.40603345718022,-331.949681911)) ;
#29880 = CARTESIAN_POINT('Ctrl Pts',(18.2220486622741,-6.76470604059831,-331.941725831355)) ;
#29881 = CARTESIAN_POINT('Ctrl Pts',(18.4736973084831,-6.00546341794311,-331.932118568671)) ;
#29882 = CARTESIAN_POINT('Ctrl Pts',(18.5078995812386,-5.89921487556642,-331.930769464782)) ;
#29883 = CARTESIAN_POINT('Ctrl Pts',(18.5596270560921,-5.73364573708061,-331.928656118261)) ;
#29884 = CARTESIAN_POINT('Ctrl Pts',(18.5777878853142,-5.67452616352374,-331.927899335838)) ;
#29885 = CARTESIAN_POINT('Ctrl Pts',(18.6162719118137,-5.54708267132632,-331.926262349003)) ;
#29886 = CARTESIAN_POINT('Ctrl Pts',(18.6365019847742,-5.47873158792611,-331.925380961635)) ;
#29887 = CARTESIAN_POINT('Ctrl Pts',(18.6913140242785,-5.28972202966955,-331.922935778102)) ;
#29888 = CARTESIAN_POINT('Ctrl Pts',(18.7251034368335,-5.16883742374057,-331.921363064997)) ;
#29889 = CARTESIAN_POINT('Ctrl Pts',(18.8008697492577,-4.88727913632979,-331.917686195177)) ;
#29890 = CARTESIAN_POINT('Ctrl Pts',(18.8419625989181,-4.72637768170358,-331.915574650318)) ;
#29891 = CARTESIAN_POINT('Ctrl Pts',(18.990419540356,-4.11235086217358,-331.907500506545)) ;
#29892 = CARTESIAN_POINT('Ctrl Pts',(19.0835410384605,-3.65594384115663,-331.901469366308)) ;
#29893 = CARTESIAN_POINT('Ctrl Pts',(19.2388388600166,-2.72511031791686,-331.889313621042)) ;
#29894 = CARTESIAN_POINT('Ctrl Pts',(19.3000738742438,-2.2508437299137,-331.883195438394)) ;
#29895 = CARTESIAN_POINT('Ctrl Pts',(19.3609659263224,-1.58717469476144,-331.874810973372)) ;
#29896 = CARTESIAN_POINT('Ctrl Pts',(19.3754500400912,-1.39930733366558,-331.872456557579)) ;
#29897 = CARTESIAN_POINT('Ctrl Pts',(19.3951138116733,-1.08457241748325,-331.868545031217)) ;
#29898 = CARTESIAN_POINT('Ctrl Pts',(19.4017868898804,-0.95781137292958,-331.866978509954)) ;
#29899 = CARTESIAN_POINT('Ctrl Pts',(19.4128469572975,-0.699512103697202,
-331.863804109812)) ;
#29900 = CARTESIAN_POINT('Ctrl Pts',(19.4171405487011,-0.567976352789986,
-331.862196913271)) ;
#29901 = CARTESIAN_POINT('Ctrl Pts',(19.4247674339681,-0.228580240947926,
-331.85807258392)) ;
#29902 = CARTESIAN_POINT('Ctrl Pts',(19.4261012774139,-0.0206916773786139,
-331.855568341005)) ;
#29903 = CARTESIAN_POINT('Ctrl Pts',(19.4216149522909,0.44486853013388,-331.850000704656)) ;
#29904 = CARTESIAN_POINT('Ctrl Pts',(19.4140040167574,0.70248393352843,-331.846947842104)) ;
#29905 = CARTESIAN_POINT('Ctrl Pts',(19.3639925052298,1.71333444094908,-331.835031566279)) ;
#29906 = CARTESIAN_POINT('Ctrl Pts',(19.2828551746358,2.46398241000536,-331.826344588909)) ;
#29907 = CARTESIAN_POINT('Ctrl Pts',(19.1319614578613,3.36512328443824,-331.815464527323)) ;
#29908 = CARTESIAN_POINT('Ctrl Pts',(19.1037202554312,3.52191371448126,-331.813553539969)) ;
#29909 = CARTESIAN_POINT('Ctrl Pts',(19.0586733397916,3.75549871709915,-331.810669442696)) ;
#29910 = CARTESIAN_POINT('Ctrl Pts',(19.0433249563059,3.83256763474922,-331.809711792714)) ;
#29911 = CARTESIAN_POINT('Ctrl Pts',(19.0140984886371,3.97481115013713,-331.807931437525)) ;
#29912 = CARTESIAN_POINT('Ctrl Pts',(19.0003519094621,4.04001142270088,-331.807110220716)) ;
#29913 = CARTESIAN_POINT('Ctrl Pts',(18.9652086770134,4.20254886742442,-331.805050840987)) ;
#29914 = CARTESIAN_POINT('Ctrl Pts',(18.943397910721,4.29979449540964,-331.803807923576)) ;
#29915 = CARTESIAN_POINT('Ctrl Pts',(18.8376944509196,4.75466334579143,-331.797950406501)) ;
#29916 = CARTESIAN_POINT('Ctrl Pts',(18.7444170238787,5.11002791269658,-331.793248596988)) ;
#29917 = CARTESIAN_POINT('Ctrl Pts',(18.4146725110056,6.23529479487276,-331.778157495301)) ;
#29918 = CARTESIAN_POINT('Ctrl Pts',(18.1403904340824,6.99323323157091,-331.767716400128)) ;
#29919 = CARTESIAN_POINT('Ctrl Pts',(17.7472338864107,7.89934219163304,-331.755301613081)) ;
#29920 = CARTESIAN_POINT('Ctrl Pts',(17.6722512209016,8.06569616394171,-331.753023343509)) ;
#29921 = CARTESIAN_POINT('Ctrl Pts',(17.5415549493129,8.34507912297241,-331.749199630797)) ;
#29922 = CARTESIAN_POINT('Ctrl Pts',(17.4870651022486,8.45866713891524,-331.747645723418)) ;
#29923 = CARTESIAN_POINT('Ctrl Pts',(17.3727364855567,8.69116621621547,-331.744466119297)) ;
#29924 = CARTESIAN_POINT('Ctrl Pts',(17.3127725646518,8.81000847761039,-331.742841425203)) ;
#29925 = CARTESIAN_POINT('Ctrl Pts',(17.1521909530555,9.12029281623065,-331.738599490998)) ;
#29926 = CARTESIAN_POINT('Ctrl Pts',(17.0495893622681,9.31068731832818,-331.735996681663)) ;
#29927 = CARTESIAN_POINT('Ctrl Pts',(16.8726434363274,9.62630346965445,-331.731674593841)) ;
#29928 = CARTESIAN_POINT('Ctrl Pts',(16.8000318651307,9.75247375823509,-331.72994472089)) ;
#29929 = CARTESIAN_POINT('Ctrl Pts',(16.4856041523759,10.2848911192371,-331.722627467802)) ;
#29930 = CARTESIAN_POINT('Ctrl Pts',(16.2304183255159,10.6830543810869,-331.717115752371)) ;
#29931 = CARTESIAN_POINT('Ctrl Pts',(15.7058696099165,11.4392567127996,-331.70636365177)) ;
#29932 = CARTESIAN_POINT('Ctrl Pts',(15.438145079093,11.7980764918677,-331.701126965723)) ;
#29933 = CARTESIAN_POINT('Ctrl Pts',(15.0839428810739,12.240074279329,-331.694334025471)) ;
#29934 = CARTESIAN_POINT('Ctrl Pts',(15.0087687247099,12.3321373860809,-331.692899320292)) ;
#29935 = CARTESIAN_POINT('Ctrl Pts',(14.8923993896484,12.4720105345549,-331.690684507595)) ;
#29936 = CARTESIAN_POINT('Ctrl Pts',(14.8518082039201,12.5203194614866,-331.689913059907)) ;
#29937 = CARTESIAN_POINT('Ctrl Pts',(14.7659324756137,12.6215177757053,-331.688282321056)) ;
#29938 = CARTESIAN_POINT('Ctrl Pts',(14.7205975219702,12.6743631557729,-331.687422153422)) ;
#29939 = CARTESIAN_POINT('Ctrl Pts',(14.5982276757477,12.8154631890887,-331.685103659509)) ;
#29940 = CARTESIAN_POINT('Ctrl Pts',(14.5206769381909,12.9032666104526,-331.683637820034)) ;
#29941 = CARTESIAN_POINT('Ctrl Pts',(14.3888086845939,13.0498741938686,-331.681155076116)) ;
#29942 = CARTESIAN_POINT('Ctrl Pts',(14.3349132574999,13.1090538835616,-331.680143046149)) ;
#29943 = CARTESIAN_POINT('Ctrl Pts',(14.1912763778585,13.2648288154611,-331.677454810346)) ;
#29944 = CARTESIAN_POINT('Ctrl Pts',(14.1009146274485,13.3608463562341,-331.675772751248)) ;
#29945 = CARTESIAN_POINT('Ctrl Pts',(13.6120280139532,13.8698482651593,-331.666736121505)) ;
#29946 = CARTESIAN_POINT('Ctrl Pts',(13.196325332094,14.265938335449,-331.659285049867)) ;
#29947 = CARTESIAN_POINT('Ctrl Pts',(12.5478290072065,14.8312041481034,-331.648251896928)) ;
#29948 = CARTESIAN_POINT('Ctrl Pts',(12.3278261885927,15.0145706293054,-331.644601329447)) ;
#29949 = CARTESIAN_POINT('Ctrl Pts',(11.9359971651274,15.3267300233875,-331.638275907073)) ;
#29950 = CARTESIAN_POINT('Ctrl Pts',(11.7659397493424,15.4576629404534,-331.635586056566)) ;
#29951 = CARTESIAN_POINT('Ctrl Pts',(11.4871858024061,15.6650191878181,-331.631267762876)) ;
#29952 = CARTESIAN_POINT('Ctrl Pts',(11.3798138182809,15.7431922217855,-331.629625595117)) ;
#29953 = CARTESIAN_POINT('Ctrl Pts',(11.1677215703687,15.8943041232146,-331.626422746484)) ;
#29954 = CARTESIAN_POINT('Ctrl Pts',(11.0630674282216,15.9673243770922,-331.62486146989)) ;
#29955 = CARTESIAN_POINT('Ctrl Pts',(10.8051447725305,16.143531442446,-331.621059083091)) ;
#29956 = CARTESIAN_POINT('Ctrl Pts',(10.6511088968725,16.245572947636,-331.618826922081)) ;
#29957 = CARTESIAN_POINT('Ctrl Pts',(10.3979809418721,16.408110407635,-331.615217155277)) ;
#29958 = CARTESIAN_POINT('Ctrl Pts',(10.2997611428721,16.469942782157,-331.613830463344)) ;
#29959 = CARTESIAN_POINT('Ctrl Pts',(9.44878637246384,16.9950679920014,-331.601928374943)) ;
#29960 = CARTESIAN_POINT('Ctrl Pts',(8.66577910616792,17.4073594147061,-331.591781831453)) ;
#29961 = CARTESIAN_POINT('Ctrl Pts',(7.67737204769751,17.8445326499902,-331.578978450184)) ;
#29962 = CARTESIAN_POINT('Ctrl Pts',(7.49611701379523,17.9214289758924,-331.576628211505)) ;
#29963 = CARTESIAN_POINT('Ctrl Pts',(7.23407970049879,18.0279257539974,-331.573208953416)) ;
#29964 = CARTESIAN_POINT('Ctrl Pts',(7.15422067673161,18.0597658508473,-331.572164032097)) ;
#29965 = CARTESIAN_POINT('Ctrl Pts',(7.01300957922743,18.1149836266799,-331.570309308251)) ;
#29966 = CARTESIAN_POINT('Ctrl Pts',(6.95174558882464,18.1385823152968,-331.569502199694)) ;
#29967 = CARTESIAN_POINT('Ctrl Pts',(6.8088222228855,18.1928054690851,-331.567613513103)) ;
#29968 = CARTESIAN_POINT('Ctrl Pts',(6.72707411148477,18.2231913991497,-331.566529087482)) ;
#29969 = CARTESIAN_POINT('Ctrl Pts',(6.43547579214956,18.3293495278886,-331.562649752165)) ;
#29970 = CARTESIAN_POINT('Ctrl Pts',(6.22452825124152,18.402055605892,-331.559823078078)) ;
#29971 = CARTESIAN_POINT('Ctrl Pts',(5.62542245516853,18.5970654761727,-331.5517811508)) ;
#29972 = CARTESIAN_POINT('Ctrl Pts',(5.23460710018778,18.7108286924396,-331.546520495896)) ;
#29973 = CARTESIAN_POINT('Ctrl Pts',(4.79050246733825,18.8250996604329,-331.540606014974)) ;
#29974 = CARTESIAN_POINT('Ctrl Pts',(4.74044574905439,18.8377669912263,-331.53994023261)) ;
#29975 = CARTESIAN_POINT('Ctrl Pts',(4.18408516602188,18.976201332403,-331.532551111083)) ;
#29976 = CARTESIAN_POINT('Ctrl Pts',(3.67296095157779,19.0817228347984,-331.525868754511)) ;
#29977 = CARTESIAN_POINT('Ctrl Pts',(2.9792747107328,19.1960265196259,-331.517033784981)) ;
#29978 = CARTESIAN_POINT('Ctrl Pts',(2.7999357611646,19.2230037148001,-331.514769780853)) ;
#29979 = CARTESIAN_POINT('Ctrl Pts',(2.49558946317666,19.2644357630188,-331.510962456308)) ;
#29980 = CARTESIAN_POINT('Ctrl Pts',(2.37077170894318,19.2801943348318,-331.509410846289)) ;
#29981 = CARTESIAN_POINT('Ctrl Pts',(2.11327886946166,19.3101651927803,-331.506229803252)) ;
#29982 = CARTESIAN_POINT('Ctrl Pts',(1.98059263133643,19.3242252170197,-331.504601436768)) ;
#29983 = CARTESIAN_POINT('Ctrl Pts',(1.6307434255086,19.3576556525071,-331.500334913811)) ;
#29984 = CARTESIAN_POINT('Ctrl Pts',(1.4133809057161,19.374738994857,-331.497711518008)) ;
#29985 = CARTESIAN_POINT('Ctrl Pts',(1.04876343398794,19.3972270022643,-331.493348896814)) ;
#29986 = CARTESIAN_POINT('Ctrl Pts',(0.901651694841911,19.4046217277171,-331.491599008477)) ;
#29987 = CARTESIAN_POINT('Ctrl Pts',(0.272172070881169,19.4290892764116,-331.48414634572)) ;
#29988 = CARTESIAN_POINT('Ctrl Pts',(-0.210657321659002,19.429853615345,-331.478522171617)) ;
#29989 = CARTESIAN_POINT('Ctrl Pts',(-0.857525756742793,19.4067610302219,
-331.47095862306)) ;
#29990 = CARTESIAN_POINT('Ctrl Pts',(-1.02195766698405,19.3987970398744,-331.4690330048)) ;
#29991 = CARTESIAN_POINT('Ctrl Pts',(-1.49472725504589,19.3698714114922,-331.46347056873)) ;
#29992 = CARTESIAN_POINT('Ctrl Pts',(-1.80269132314621,19.3436405902285,-331.459815864918)) ;
#29993 = CARTESIAN_POINT('Ctrl Pts',(-2.20740205846246,19.2994202455134,-331.454910134814)) ;
#29994 = CARTESIAN_POINT('Ctrl Pts',(-2.30482453628656,19.2880281387308,-331.453721268001)) ;
#29995 = CARTESIAN_POINT('Ctrl Pts',(-2.46807440058971,19.2676839918965,-331.451712942153)) ;
#29996 = CARTESIAN_POINT('Ctrl Pts',(-2.53394971701626,19.2591312498112,-331.450898048381)) ;
#29997 = CARTESIAN_POINT('Ctrl Pts',(-2.67847661660683,19.2396126294239,-331.449099641192)) ;
#29998 = CARTESIAN_POINT('Ctrl Pts',(-2.75710726738437,19.2285020376209,-331.448114532312)) ;
#29999 = CARTESIAN_POINT('Ctrl Pts',(-3.00360809940843,19.1921281142128,-331.4450077374)) ;
#30000 = CARTESIAN_POINT('Ctrl Pts',(-3.17121642209234,19.1651462142298,-331.442868271512)) ;
#30001 = CARTESIAN_POINT('Ctrl Pts',(-3.85795317980455,19.0453385594749,-331.434019652971)) ;
#30002 = CARTESIAN_POINT('Ctrl Pts',(-4.37355068944828,18.9335886096018,-331.427187546371)) ;
#30003 = CARTESIAN_POINT('Ctrl Pts',(-5.4183967982167,18.6621675421631,-331.413273094881)) ;
#30004 = CARTESIAN_POINT('Ctrl Pts',(-5.9466718113193,18.5006113154178,-331.40620172262)) ;
#30005 = CARTESIAN_POINT('Ctrl Pts',(-6.61235440309683,18.2655698793065,-331.397346078729)) ;
#30006 = CARTESIAN_POINT('Ctrl Pts',(-6.75674945712199,18.2126497420973,-331.395427932506)) ;
#30007 = CARTESIAN_POINT('Ctrl Pts',(-7.01839704791395,18.1132171273544,-331.391957689612)) ;
#30008 = CARTESIAN_POINT('Ctrl Pts',(-7.13585402567213,18.0672665115155,-331.390401878052)) ;
#30009 = CARTESIAN_POINT('Ctrl Pts',(-7.37610560545495,17.9705687875472,-331.387223338295)) ;
#30010 = CARTESIAN_POINT('Ctrl Pts',(-7.49884387351457,17.9196991344049,-331.38560156125)) ;
#30011 = CARTESIAN_POINT('Ctrl Pts',(-7.81869503445604,17.78327312194,-331.381379173044)) ;
#30012 = CARTESIAN_POINT('Ctrl Pts',(-8.01492718843297,17.695698272446,-331.378792732357)) ;
#30013 = CARTESIAN_POINT('Ctrl Pts',(-8.34035800174749,17.5439404947011,-331.374502793489)) ;
#30014 = CARTESIAN_POINT('Ctrl Pts',(-8.47036715907341,17.4815416918333,-331.372788756653)) ;
#30015 = CARTESIAN_POINT('Ctrl Pts',(-9.01669629313318,17.2118017302532,-331.365576814086)) ;
#30016 = CARTESIAN_POINT('Ctrl Pts',(-9.42619412550397,16.9909915989308,-331.360152335424)) ;
#30017 = CARTESIAN_POINT('Ctrl Pts',(-9.91875193730231,16.7021019026936,-331.353481819009)) ;
#30018 = CARTESIAN_POINT('Ctrl Pts',(-10.0096928089832,16.6477595437041,-331.352243746245)) ;
#30019 = CARTESIAN_POINT('Ctrl Pts',(-10.4054628321071,16.4068490190876,-331.346820433181)) ;
#30020 = CARTESIAN_POINT('Ctrl Pts',(-10.7055540384789,16.2126328265006,-331.342617157296)) ;
#30021 = CARTESIAN_POINT('Ctrl Pts',(-11.0962296247897,15.9442124902621,-331.336929884951)) ;
#30022 = CARTESIAN_POINT('Ctrl Pts',(-11.1917471523464,15.8773114676175,-331.335521660125)) ;
#30023 = CARTESIAN_POINT('Ctrl Pts',(-11.3376888021515,15.7731217355167,-331.333338341927)) ;
#30024 = CARTESIAN_POINT('Ctrl Pts',(-11.3885445195097,15.736442112944,-331.332571531048)) ;
#30025 = CARTESIAN_POINT('Ctrl Pts',(-11.4958613239839,15.6582473044546,-331.33093969124)) ;
#30026 = CARTESIAN_POINT('Ctrl Pts',(-11.5522771202698,15.6166715256386,-331.330073694845)) ;
#30027 = CARTESIAN_POINT('Ctrl Pts',(-11.7042590679014,15.5033937732473,-331.327720044719)) ;
#30028 = CARTESIAN_POINT('Ctrl Pts',(-11.7993906854033,15.4311139651934,-331.326224493936)) ;
#30029 = CARTESIAN_POINT('Ctrl Pts',(-12.2155905345387,15.1087913461664,-331.319593546571)) ;
#30030 = CARTESIAN_POINT('Ctrl Pts',(-12.5294219555271,14.8495728079125,-331.314362474225)) ;
#30031 = CARTESIAN_POINT('Ctrl Pts',(-13.3881918424572,14.0936272529455,-331.299611735002)) ;
#30032 = CARTESIAN_POINT('Ctrl Pts',(-13.9133341702555,13.5754613423282,-331.29008804216)) ;
#30033 = CARTESIAN_POINT('Ctrl Pts',(-14.5270836557819,12.8967483345373,-331.278595076019)) ;
#30034 = CARTESIAN_POINT('Ctrl Pts',(-14.6445931160055,12.7631567312836,-331.276375032726)) ;
#30035 = CARTESIAN_POINT('Ctrl Pts',(-14.8425103502254,12.5318204100332,-331.272602574181)) ;
#30036 = CARTESIAN_POINT('Ctrl Pts',(-14.9238283723514,12.4348696433832,-331.271042558816)) ;
#30037 = CARTESIAN_POINT('Ctrl Pts',(-15.0898236597302,12.2329892103144,-331.267836696898)) ;
#30038 = CARTESIAN_POINT('Ctrl Pts',(-15.1743674369943,12.1279584451394,-331.266192014314)) ;
#30039 = CARTESIAN_POINT('Ctrl Pts',(-15.3975558965813,11.8446984654067,-331.261816306679)) ;
#30040 = CARTESIAN_POINT('Ctrl Pts',(-15.5341979193056,11.6649176839494,-331.259101540744)) ;
#30041 = CARTESIAN_POINT('Ctrl Pts',(-15.8394661575855,11.248395114483,-331.252940539209)) ;
#30042 = CARTESIAN_POINT('Ctrl Pts',(-16.0059758350177,11.010168878258,-331.249509062683)) ;
#30043 = CARTESIAN_POINT('Ctrl Pts',(-16.4010222887596,10.41706236079,-331.241142833796)) ;
#30044 = CARTESIAN_POINT('Ctrl Pts',(-16.6234582152476,10.0582979240445,-331.236233557358)) ;
#30045 = CARTESIAN_POINT('Ctrl Pts',(-17.0157179024034,9.37702254855795,-331.227026665904)) ;
#30046 = CARTESIAN_POINT('Ctrl Pts',(-17.1884951408275,9.05642541069598,-331.222738703137)) ;
#30047 = CARTESIAN_POINT('Ctrl Pts',(-17.3989377270437,8.63819554004497,-331.217105491648)) ;
#30048 = CARTESIAN_POINT('Ctrl Pts',(-17.4449686597368,8.54485369300976,-331.215845680376)) ;
#30049 = CARTESIAN_POINT('Ctrl Pts',(-17.5192329167675,8.39115854581083,-331.213763833116)) ;
#30050 = CARTESIAN_POINT('Ctrl Pts',(-17.5479098209778,8.33102182555669,-331.212947371418)) ;
#30051 = CARTESIAN_POINT('Ctrl Pts',(-17.6087414185538,8.2017476411726,-331.21118726001)) ;
#30052 = CARTESIAN_POINT('Ctrl Pts',(-17.6407995088479,8.13256610083372,-331.210242462108)) ;
#30053 = CARTESIAN_POINT('Ctrl Pts',(-17.7353603690866,7.92531308687257,-331.207405543751)) ;
#30054 = CARTESIAN_POINT('Ctrl Pts',(-17.7966553838376,7.78669711603526,-331.205499591473)) ;
#30055 = CARTESIAN_POINT('Ctrl Pts',(-17.9418964534058,7.44756503803881,-331.20082801241)) ;
#30056 = CARTESIAN_POINT('Ctrl Pts',(-18.0241110520805,7.246329686057,-331.198048881185)) ;
#30057 = CARTESIAN_POINT('Ctrl Pts',(-18.4078383340327,6.26012471535239,-331.184457460101)) ;
#30058 = CARTESIAN_POINT('Ctrl Pts',(-18.6615438059373,5.45751492504185,-331.17352600709)) ;
#30059 = CARTESIAN_POINT('Ctrl Pts',(-18.9084208581279,4.4541305363446,-331.160518479094)) ;
#30060 = CARTESIAN_POINT('Ctrl Pts',(-18.9516190265467,4.26659051511602,-331.158112550982)) ;
#30061 = CARTESIAN_POINT('Ctrl Pts',(-19.0163859465048,3.96499112006096,-331.154284912674)) ;
#30062 = CARTESIAN_POINT('Ctrl Pts',(-19.039731394866,3.85132671920606,-331.152851743723)) ;
#30063 = CARTESIAN_POINT('Ctrl Pts',(-19.086773875808,3.61139733433789,-331.149845963584)) ;
#30064 = CARTESIAN_POINT('Ctrl Pts',(-19.1102395940689,3.48509259576566,-331.148274937152)) ;
#30065 = CARTESIAN_POINT('Ctrl Pts',(-19.1652895313905,3.17149424870167,-331.144401062335)) ;
#30066 = CARTESIAN_POINT('Ctrl Pts',(-19.1953829449298,2.98395246974467,-331.142108007504)) ;
#30067 = CARTESIAN_POINT('Ctrl Pts',(-19.2986898218603,2.27370936039285,-331.133502633434)) ;
#30068 = CARTESIAN_POINT('Ctrl Pts',(-19.3533406346527,1.74853959813532,-331.12730638308)) ;
#30069 = CARTESIAN_POINT('Ctrl Pts',(-19.4248319342674,0.614170808014305,
-331.114023253272)) ;
#30070 = CARTESIAN_POINT('Ctrl Pts',(-19.4345380838159,0.00508200935372204,
-331.106955117943)) ;
#30071 = CARTESIAN_POINT('Ctrl Pts',(-19.4122294674355,-0.712681329477538,
-331.098325319068)) ;
#30072 = CARTESIAN_POINT('Ctrl Pts',(-19.4079128409369,-0.821879968633598,
-331.097003834431)) ;
#30073 = CARTESIAN_POINT('Ctrl Pts',(-19.3997291682074,-0.992426653349981,
-331.094922963838)) ;
#30074 = CARTESIAN_POINT('Ctrl Pts',(-19.3964920087444,-1.05380273969823,
-331.094170661844)) ;
#30075 = CARTESIAN_POINT('Ctrl Pts',(-19.3888339309363,-1.18697869874726,
-331.092529909088)) ;
#30076 = CARTESIAN_POINT('Ctrl Pts',(-19.3843053549776,-1.25877143327545,
-331.091640164774)) ;
#30077 = CARTESIAN_POINT('Ctrl Pts',(-19.3705551367299,-1.45904442080467,
-331.089145104652)) ;
#30078 = CARTESIAN_POINT('Ctrl Pts',(-19.3604541808115,-1.58746047584606,
-331.087530297816)) ;
#30079 = CARTESIAN_POINT('Ctrl Pts',(-19.3338682327726,-1.88727608978324,
-331.083732471144)) ;
#30080 = CARTESIAN_POINT('Ctrl Pts',(-19.3163800236605,-2.05857585171063,
-331.081541412064)) ;
#30081 = CARTESIAN_POINT('Ctrl Pts',(-19.2387950090773,-2.73004819154784,
-331.072895872852)) ;
#30082 = CARTESIAN_POINT('Ctrl Pts',(-19.1615284085456,-3.22803746948053,
-331.066364867967)) ;
#30083 = CARTESIAN_POINT('Ctrl Pts',(-18.9749274874972,-4.18373507064429,
-331.053838058016)) ;
#30084 = CARTESIAN_POINT('Ctrl Pts',(-18.8681515431548,-4.64159151181229,
-331.047839442751)) ;
#30085 = CARTESIAN_POINT('Ctrl Pts',(-18.7046641370253,-5.24305883587811,
-331.040021539713)) ;
#30086 = CARTESIAN_POINT('Ctrl Pts',(-18.6627036336701,-5.39051199823045,
-331.038109534483)) ;
#30087 = CARTESIAN_POINT('Ctrl Pts',(-18.5830784803378,-5.65824173993203,
-331.034646763535)) ;
#30088 = CARTESIAN_POINT('Ctrl Pts',(-18.5459803184889,-5.77867800357317,
-331.033092341189)) ;
#30089 = CARTESIAN_POINT('Ctrl Pts',(-18.4673126107459,-6.02550328362981,
-331.029913036015)) ;
#30090 = CARTESIAN_POINT('Ctrl Pts',(-18.4256111792053,-6.1518434321073,-331.028289141783)) ;
#30091 = CARTESIAN_POINT('Ctrl Pts',(-18.3128463043304,-6.48204371838377,
-331.024052565633)) ;
#30092 = CARTESIAN_POINT('Ctrl Pts',(-18.2396765042545,-6.6851650518102,-331.021454242966)) ;
#30093 = CARTESIAN_POINT('Ctrl Pts',(-18.1116586833711,-7.02278618811575,
-331.017140974204)) ;
#30094 = CARTESIAN_POINT('Ctrl Pts',(-18.058660651361,-7.15796630620107,-331.015415448825)) ;
#30095 = CARTESIAN_POINT('Ctrl Pts',(-17.8274634880234,-7.72875633338713,
-331.008127264169)) ;
#30096 = CARTESIAN_POINT('Ctrl Pts',(-17.634979747844,-8.15840784149597,-331.002639648016)) ;
#30097 = CARTESIAN_POINT('Ctrl Pts',(-17.3995424610263,-8.63657536145363,
-330.996412990582)) ;
#30098 = CARTESIAN_POINT('Ctrl Pts',(-17.3717338276901,-8.69237456889157,
-330.995684419256)) ;
#30099 = CARTESIAN_POINT('Ctrl Pts',(-17.1674965137336,-9.09729068326911,
-330.990380881024)) ;
#30100 = CARTESIAN_POINT('Ctrl Pts',(-16.9808271065427,-9.44114101991094,
-330.985789306889)) ;
#30101 = CARTESIAN_POINT('Ctrl Pts',(-16.7248235438796,-9.88051997812779,
-330.979688802644)) ;
#30102 = CARTESIAN_POINT('Ctrl Pts',(-16.6648250242299,-9.98138289336614,
-330.978271794879)) ;
#30103 = CARTESIAN_POINT('Ctrl Pts',(-16.5713053719243,-10.1354038547098,
-330.976078039556)) ;
#30104 = CARTESIAN_POINT('Ctrl Pts',(-16.538434104238,-10.1889533513697,-330.975309699002)) ;
#30105 = CARTESIAN_POINT('Ctrl Pts',(-16.4684341509548,-10.301756696567,-330.973678298799)) ;
#30106 = CARTESIAN_POINT('Ctrl Pts',(-16.4312441854975,-10.3609714269547,
-330.972814302207)) ;
#30107 = CARTESIAN_POINT('Ctrl Pts',(-16.3300739797615,-10.5201422646501,
-330.970472670263)) ;
#30108 = CARTESIAN_POINT('Ctrl Pts',(-16.2654961231903,-10.6197149329542,
-330.968987269506)) ;
#30109 = CARTESIAN_POINT('Ctrl Pts',(-16.1550346448633,-10.7866641723192,
-330.966466050456)) ;
#30110 = CARTESIAN_POINT('Ctrl Pts',(-16.1096319930367,-10.8543551340401,
-330.965435157717)) ;
#30111 = CARTESIAN_POINT('Ctrl Pts',(-15.7672491658867,-11.3579343855912,
-330.957706666126)) ;
#30112 = CARTESIAN_POINT('Ctrl Pts',(-15.4530517845319,-11.7818508726733,
-330.950873599303)) ;
#30113 = CARTESIAN_POINT('Ctrl Pts',(-14.7746704770437,-12.6232301223945,
-330.936942382117)) ;
#30114 = CARTESIAN_POINT('Ctrl Pts',(-14.4090979695469,-13.0389694989348,
-330.929855391493)) ;
#30115 = CARTESIAN_POINT('Ctrl Pts',(-13.9197885755823,-13.5496790992831,
-330.920982898976)) ;
#30116 = CARTESIAN_POINT('Ctrl Pts',(-13.8119838383127,-13.6595541735275,
-330.919062926041)) ;
#30117 = CARTESIAN_POINT('Ctrl Pts',(-13.6134688231621,-13.8571283579793,
-330.915590458838)) ;
#30118 = CARTESIAN_POINT('Ctrl Pts',(-13.5231882670627,-13.9452471785663,
-330.914034232333)) ;
#30119 = CARTESIAN_POINT('Ctrl Pts',(-13.346716337236,-14.1141681907648,-330.911035974264)) ;
#30120 = CARTESIAN_POINT('Ctrl Pts',(-13.2606335339846,-14.1950758723145,
-330.909593032186)) ;
#30121 = CARTESIAN_POINT('Ctrl Pts',(-13.1699067672301,-14.2788027883436,
-330.908092150886)) ;
#30122 = CARTESIAN_POINT('Ctrl Pts',(-13.1659940537106,-14.2824106474933,
-330.90802746166)) ;
#30123 = CARTESIAN_POINT('Ctrl Pts',(-13.1579043470016,-14.289863905213,-330.907893792867)) ;
#30124 = CARTESIAN_POINT('Ctrl Pts',(-13.1537271496615,-14.2937090815021,
-330.9078248152)) ;
#30125 = CARTESIAN_POINT('Ctrl Pts',(-13.1450454851963,-14.3016936625354,
-330.907681545887)) ;
#30126 = CARTESIAN_POINT('Ctrl Pts',(-13.1405407471776,-14.3058327718681,
-330.90760725676)) ;
#30127 = CARTESIAN_POINT('Ctrl Pts',(-13.1311302780127,-14.3144712417989,
-330.907452170609)) ;
#30128 = CARTESIAN_POINT('Ctrl Pts',(-13.1262241878562,-14.3189702101993,
-330.907371376918)) ;
#30129 = CARTESIAN_POINT('Ctrl Pts',(-13.1159235063309,-14.3284063682432,
-330.90720186952)) ;
#30130 = CARTESIAN_POINT('Ctrl Pts',(-13.110528437521,-14.3333430352586,-330.907113160237)) ;
#30131 = CARTESIAN_POINT('Ctrl Pts',(-13.0991448293914,-14.3437476099942,
-330.906926134182)) ;
#30132 = CARTESIAN_POINT('Ctrl Pts',(-13.0931556511202,-14.3492148167117,
-330.90682782332)) ;
#30133 = CARTESIAN_POINT('Ctrl Pts',(-13.0804569693467,-14.360792207424,-330.906619563303)) ;
#30134 = CARTESIAN_POINT('Ctrl Pts',(-13.0737466040408,-14.366901443425,-330.906509622107)) ;
#30135 = CARTESIAN_POINT('Ctrl Pts',(-13.0594515520137,-14.379897604564,-330.906275647762)) ;
#30136 = CARTESIAN_POINT('Ctrl Pts',(-13.0518656929647,-14.3867832363587,
-330.906151625416)) ;
#30137 = CARTESIAN_POINT('Ctrl Pts',(-13.0356324391991,-14.4014946422293,
-330.905886522223)) ;
#30138 = CARTESIAN_POINT('Ctrl Pts',(-13.0269834365479,-14.4093186363547,
-330.905745456151)) ;
#30139 = CARTESIAN_POINT('Ctrl Pts',(-13.0083967774867,-14.4261019442397,
-330.905442690165)) ;
#30140 = CARTESIAN_POINT('Ctrl Pts',(-12.9984568996897,-14.435058789388,-330.905281010596)) ;
#30141 = CARTESIAN_POINT('Ctrl Pts',(-12.9770147644486,-14.4543402375308,
-330.904932742837)) ;
#30142 = CARTESIAN_POINT('Ctrl Pts',(-12.9655094221139,-14.4646613968036,
-330.904746182784)) ;
#30143 = CARTESIAN_POINT('Ctrl Pts',(-12.9487538038036,-14.4796563957236,
-330.904474940548)) ;
#30144 = CARTESIAN_POINT('Ctrl Pts',(-12.9435132910517,-14.4843411342772,
-330.904390170528)) ;
#30145 = CARTESIAN_POINT('Ctrl Pts',(-12.9303581890717,-14.4960882523597,
-330.904177535307)) ;
#30146 = CARTESIAN_POINT('Ctrl Pts',(-12.9224403554353,-14.5031469956744,
-330.904049699289)) ;
#30147 = CARTESIAN_POINT('Ctrl Pts',(-12.5958014799049,-14.7938654864636,
-330.898781981125)) ;
#30148 = CARTESIAN_POINT('Ctrl Pts',(-12.2678263181999,-15.0669542219889,
-330.893730121574)) ;
#30149 = CARTESIAN_POINT('Ctrl Pts',(-11.6482163253446,-15.5492188085486,
-330.884513168464)) ;
#30150 = CARTESIAN_POINT('Ctrl Pts',(-11.3592662970941,-15.7615423839009,
-330.880336402993)) ;
#30151 = CARTESIAN_POINT('Ctrl Pts',(-10.7377138213715,-16.1922916213235,
-330.871494332941)) ;
#30152 = CARTESIAN_POINT('Ctrl Pts',(-10.4039410716307,-16.4087420247496,
-330.866827909134)) ;
#30153 = CARTESIAN_POINT('Ctrl Pts',(-9.96463563821109,-16.6748341016949,
-330.860667380911)) ;
#30154 = CARTESIAN_POINT('Ctrl Pts',(-9.86497531991412,-16.7339869009585,
-330.859268449241)) ;
#30155 = CARTESIAN_POINT('Ctrl Pts',(-9.72082005359146,-16.8178140616465,
-330.857239088423)) ;
#30156 = CARTESIAN_POINT('Ctrl Pts',(-9.6767481048739,-16.8432110488327,-330.856617879281)) ;
#30157 = CARTESIAN_POINT('Ctrl Pts',(-9.59049287432927,-16.8924663687887,
-330.85540009264)) ;
#30158 = CARTESIAN_POINT('Ctrl Pts',(-9.54831914442612,-16.9163404759529,
-330.854803686318)) ;
#30159 = CARTESIAN_POINT('Ctrl Pts',(-9.45018271606108,-16.9714105656705,
-330.853413739131)) ;
#30160 = CARTESIAN_POINT('Ctrl Pts',(-9.39415419047365,-17.002487964705,-330.852618639159)) ;
#30161 = CARTESIAN_POINT('Ctrl Pts',(-9.26180208748804,-17.0750459107955,
-330.850737750977)) ;
#30162 = CARTESIAN_POINT('Ctrl Pts',(-9.18535200016055,-17.1162928045992,
-330.849649215486)) ;
#30163 = CARTESIAN_POINT('Ctrl Pts',(-8.97644632944115,-17.2272003754551,
-330.846671659059)) ;
#30164 = CARTESIAN_POINT('Ctrl Pts',(-8.84345834150711,-17.2958453378883,
-330.844772879892)) ;
#30165 = CARTESIAN_POINT('Ctrl Pts',(-8.37195213015958,-17.5323647091539,
-330.838045192709)) ;
#30166 = CARTESIAN_POINT('Ctrl Pts',(-8.02934256317685,-17.6918922796249,
-330.83316607053)) ;
#30167 = CARTESIAN_POINT('Ctrl Pts',(-7.54474823325048,-17.9005538277824,
-330.826359167467)) ;
#30168 = CARTESIAN_POINT('Ctrl Pts',(-7.40651686480447,-17.9581892515512,
-330.82442771812)) ;
#30169 = CARTESIAN_POINT('Ctrl Pts',(-6.81527791660644,-18.1967178971547,
-330.816221325694)) ;
#30170 = CARTESIAN_POINT('Ctrl Pts',(-6.35620850284429,-18.3621123822784,
-330.809990091716)) ;
#30171 = CARTESIAN_POINT('Ctrl Pts',(-5.74424953347748,-18.5568873800967,
-330.801933132721)) ;
#30172 = CARTESIAN_POINT('Ctrl Pts',(-5.59654524475661,-18.6019663840019,
-330.800006756453)) ;
#30173 = CARTESIAN_POINT('Ctrl Pts',(-5.32712333760844,-18.6806938984724,
-330.796526486237)) ;
#30174 = CARTESIAN_POINT('Ctrl Pts',(-5.20558514273602,-18.7149258869327,
-330.794968799171)) ;
#30175 = CARTESIAN_POINT('Ctrl Pts',(-4.97151285361023,-18.7783972044567,
-330.791992001037)) ;
#30176 = CARTESIAN_POINT('Ctrl Pts',(-4.85903298081444,-18.8078159325072,
-330.790571745174)) ;
#30177 = CARTESIAN_POINT('Ctrl Pts',(-4.61901284084109,-18.8682954964984,
-330.787561947591)) ;
#30178 = CARTESIAN_POINT('Ctrl Pts',(-4.49140806555949,-18.8990769141542,
-330.785974290612)) ;
#30179 = CARTESIAN_POINT('Ctrl Pts',(-3.90025969869142,-19.0353512079354,
-330.778672806022)) ;
#30180 = CARTESIAN_POINT('Ctrl Pts',(-3.43325378105262,-19.125098462191,-330.77306078346)) ;
#30181 = CARTESIAN_POINT('Ctrl Pts',(-2.34524013258419,-19.2930488491088,
-330.760164813077)) ;
#30182 = CARTESIAN_POINT('Ctrl Pts',(-1.72280752052367,-19.3585592239145,
-330.752925013063)) ;
#30183 = CARTESIAN_POINT('Ctrl Pts',(-0.941296574230398,-19.402817218473,
-330.743602996482)) ;
#30184 = CARTESIAN_POINT('Ctrl Pts',(-0.784187582285233,-19.4098017754061,
-330.741716527415)) ;
#30185 = CARTESIAN_POINT('Ctrl Pts',(-0.548155794540502,-19.4174245180445,
-330.738853805589)) ;
#30186 = CARTESIAN_POINT('Ctrl Pts',(-0.46928548701264,-19.419490745122,-330.737892423873)) ;
#30187 = CARTESIAN_POINT('Ctrl Pts',(-0.327535873861351,-19.4223402132059,
-330.736154365708)) ;
#30188 = CARTESIAN_POINT('Ctrl Pts',(-0.264661332178073,-19.4232987274662,
-330.735379694964)) ;
#30189 = CARTESIAN_POINT('Ctrl Pts',(-0.134559580638513,-19.4246502730836,
-330.733769429841)) ;
#30190 = CARTESIAN_POINT('Ctrl Pts',(-0.0673327622802353,-19.4249996344579,
-330.732933396708)) ;
#30191 = CARTESIAN_POINT('Ctrl Pts',(-0.00010553887512245,-19.4249999997133,
-330.732093850011)) ;
#30192 = CARTESIAN_POINT('Ctrl Pts',(5.03575626651515E-5,-19.4249999999347,
-330.517882160562)) ;
#30193 = CARTESIAN_POINT('Ctrl Pts',(-0.109383643921926,-19.4250002836325,
-330.519239321665)) ;
#30194 = CARTESIAN_POINT('Ctrl Pts',(-0.218815588222075,-19.4240757949738,
-330.520606794212)) ;
#30195 = CARTESIAN_POINT('Ctrl Pts',(-0.401044244614562,-19.420996148449,
-330.522897922524)) ;
#30196 = CARTESIAN_POINT('Ctrl Pts',(-0.473847218249506,-19.4193562376763,
-330.523816981607)) ;
#30197 = CARTESIAN_POINT('Ctrl Pts',(-0.763832435112605,-19.4111925264556,
-330.52749040625)) ;
#30198 = CARTESIAN_POINT('Ctrl Pts',(-0.980907588565217,-19.401434364168,
-330.530268396036)) ;
#30199 = CARTESIAN_POINT('Ctrl Pts',(-2.03944657170865,-19.3360389151549,
-330.543889642085)) ;
#30200 = CARTESIAN_POINT('Ctrl Pts',(-2.87684738347944,-19.2292876972037,
-330.554852659341)) ;
#30201 = CARTESIAN_POINT('Ctrl Pts',(-3.89251083549517,-19.0319627524741,
-330.567875055589)) ;
#30202 = CARTESIAN_POINT('Ctrl Pts',(-4.07981718600254,-18.9926917184026,
-330.57026726666)) ;
#30203 = CARTESIAN_POINT('Ctrl Pts',(-4.37955302673366,-18.9252098020816,
-330.574079200534)) ;
#30204 = CARTESIAN_POINT('Ctrl Pts',(-4.49236330780916,-18.8987492367985,
-330.575510203298)) ;
#30205 = CARTESIAN_POINT('Ctrl Pts',(-4.72990659535361,-18.8407844248779,
-330.578515926537)) ;
#30206 = CARTESIAN_POINT('Ctrl Pts',(-4.85457708568074,-18.8090471719321,
-330.580089019906)) ;
#30207 = CARTESIAN_POINT('Ctrl Pts',(-5.16354214344152,-18.7271177277252,
-330.583977725882)) ;
#30208 = CARTESIAN_POINT('Ctrl Pts',(-5.34742914969837,-18.6754412932905,
-330.586283367834)) ;
#30209 = CARTESIAN_POINT('Ctrl Pts',(-6.04461305722028,-18.4683750866107,
-330.595002001604)) ;
#30210 = CARTESIAN_POINT('Ctrl Pts',(-6.55215884262199,-18.2944647695834,
-330.60129475374)) ;
#30211 = CARTESIAN_POINT('Ctrl Pts',(-7.60397983251672,-17.8846646187067,
-330.614484949302)) ;
#30212 = CARTESIAN_POINT('Ctrl Pts',(-8.14596864611218,-17.6444021721716,
-330.621368588068)) ;
#30213 = CARTESIAN_POINT('Ctrl Pts',(-8.77644848501478,-17.3296610002707,
-330.629831615065)) ;
#30214 = CARTESIAN_POINT('Ctrl Pts',(-8.87633772169011,-17.2787102236215,
-330.631186815447)) ;
#30215 = CARTESIAN_POINT('Ctrl Pts',(-9.03070414909833,-17.1982802387979,
-330.63330735105)) ;
#30216 = CARTESIAN_POINT('Ctrl Pts',(-9.08549102029803,-17.1694004995042,
-330.634065142394)) ;
#30217 = CARTESIAN_POINT('Ctrl Pts',(-9.20291603010773,-17.1067829583898,
-330.635701417219)) ;
#30218 = CARTESIAN_POINT('Ctrl Pts',(-9.26550881887964,-17.0729620439434,
-330.636581060354)) ;
#30219 = CARTESIAN_POINT('Ctrl Pts',(-9.43741154310013,-16.9788536520004,
-330.639015884429)) ;
#30220 = CARTESIAN_POINT('Ctrl Pts',(-9.54632825747328,-16.9178552038756,
-330.640579864895)) ;
#30221 = CARTESIAN_POINT('Ctrl Pts',(-9.79765324946986,-16.773901607098,-330.64423179819)) ;
#30222 = CARTESIAN_POINT('Ctrl Pts',(-9.93960891715943,-16.6901755167978,
-330.646327008174)) ;
#30223 = CARTESIAN_POINT('Ctrl Pts',(-10.4721870967643,-16.366853823257,-330.65428898829)) ;
#30224 = CARTESIAN_POINT('Ctrl Pts',(-10.8553550838812,-16.1152683074099,
-330.660222740504)) ;
#30225 = CARTESIAN_POINT('Ctrl Pts',(-11.3797767304201,-15.7437393804565,
-330.668502957782)) ;
#30226 = CARTESIAN_POINT('Ctrl Pts',(-11.5287603961236,-15.6349714395217,
-330.6708746482)) ;
#30227 = CARTESIAN_POINT('Ctrl Pts',(-11.9730957657495,-15.3007725488647,
-330.677994615142)) ;
#30228 = CARTESIAN_POINT('Ctrl Pts',(-12.2635512886728,-15.0689738763107,
-330.6827107555)) ;
#30229 = CARTESIAN_POINT('Ctrl Pts',(-12.6679914644066,-14.7267668430725,
-330.689343109839)) ;
#30230 = CARTESIAN_POINT('Ctrl Pts',(-12.7875486623785,-14.6230731617917,
-330.6913125079)) ;
#30231 = CARTESIAN_POINT('Ctrl Pts',(-12.9988221246711,-14.4352599934615,
-330.694808338038)) ;
#30232 = CARTESIAN_POINT('Ctrl Pts',(-13.0910223209699,-14.3516982391118,
-330.696339412337)) ;
#30233 = CARTESIAN_POINT('Ctrl Pts',(-13.2870765208819,-14.1705514621277,
-330.69960749561)) ;
#30234 = CARTESIAN_POINT('Ctrl Pts',(-13.390672476077,-14.0726977484564,-330.701342012162)) ;
#30235 = CARTESIAN_POINT('Ctrl Pts',(-13.6874134023531,-13.7861612017981,
-330.706335127412)) ;
#30236 = CARTESIAN_POINT('Ctrl Pts',(-13.8777130980579,-13.5945800188833,
-330.709567868658)) ;
#30237 = CARTESIAN_POINT('Ctrl Pts',(-14.5346164437145,-12.9050811120067,
-330.720873816135)) ;
#30238 = CARTESIAN_POINT('Ctrl Pts',(-14.9789182179962,-12.386613789824,-330.728775681188)) ;
#30239 = CARTESIAN_POINT('Ctrl Pts',(-15.5962871770699,-11.5842730369867,
-330.7406521795)) ;
#30240 = CARTESIAN_POINT('Ctrl Pts',(-15.7908579681024,-11.3176127876404,
-330.744549737181)) ;
#30241 = CARTESIAN_POINT('Ctrl Pts',(-16.0349031381681,-10.9645944095316,
-330.749719699498)) ;
#30242 = CARTESIAN_POINT('Ctrl Pts',(-16.0906417276774,-10.8826328601742,
-330.750920798574)) ;
#30243 = CARTESIAN_POINT('Ctrl Pts',(-16.1827580401535,-10.7449242682418,
-330.752942999139)) ;
#30244 = CARTESIAN_POINT('Ctrl Pts',(-16.2194809354834,-10.6894103442735,
-330.753759376281)) ;
#30245 = CARTESIAN_POINT('Ctrl Pts',(-16.2990879908049,-10.5677137856019,
-330.755552347349)) ;
#30246 = CARTESIAN_POINT('Ctrl Pts',(-16.3418558202475,-10.5014566758946,
-330.756530443555)) ;
#30247 = CARTESIAN_POINT('Ctrl Pts',(-16.4736501247837,-10.294522421551,-330.759588850281)) ;
#30248 = CARTESIAN_POINT('Ctrl Pts',(-16.5612723386543,-10.1529600952451,
-330.761686198041)) ;
#30249 = CARTESIAN_POINT('Ctrl Pts',(-16.7154441866806,-9.89657303695557,
-330.765482103599)) ;
#30250 = CARTESIAN_POINT('Ctrl Pts',(-16.7826574781856,-9.78215927861785,
-330.767175124178)) ;
#30251 = CARTESIAN_POINT('Ctrl Pts',(-17.1382223352435,-9.16244661736475,
-330.776324293651)) ;
#30252 = CARTESIAN_POINT('Ctrl Pts',(-17.4049353997936,-8.64507478365913,
-330.783878532853)) ;
#30253 = CARTESIAN_POINT('Ctrl Pts',(-17.8130191564934,-7.7577637368678,-330.796399308548)) ;
#30254 = CARTESIAN_POINT('Ctrl Pts',(-17.9670351678522,-7.39406506878113,
-330.801417049817)) ;
#30255 = CARTESIAN_POINT('Ctrl Pts',(-18.1674321508323,-6.87752649898721,
-330.808354400557)) ;
#30256 = CARTESIAN_POINT('Ctrl Pts',(-18.2231788022412,-6.72842597773595,
-330.810335577701)) ;
#30257 = CARTESIAN_POINT('Ctrl Pts',(-18.3192566071755,-6.46149879788646,
-330.813844317712)) ;
#30258 = CARTESIAN_POINT('Ctrl Pts',(-18.3602991120824,-6.34393772956422,
-330.8153766548)) ;
#30259 = CARTESIAN_POINT('Ctrl Pts',(-18.4456960153687,-6.0915568552642,-330.81863910699)) ;
#30260 = CARTESIAN_POINT('Ctrl Pts',(-18.4897089444165,-5.95662904927668,
-330.82036682283)) ;
#30261 = CARTESIAN_POINT('Ctrl Pts',(-18.6121069816489,-5.56696752573591,
-330.825311487338)) ;
#30262 = CARTESIAN_POINT('Ctrl Pts',(-18.6867334791185,-5.31108708168226,
-330.828503405246)) ;
#30263 = CARTESIAN_POINT('Ctrl Pts',(-18.9834646161529,-4.20982401420183,
-330.842048519428)) ;
#30264 = CARTESIAN_POINT('Ctrl Pts',(-19.1536387280904,-3.35151597096332,
-330.852077771041)) ;
#30265 = CARTESIAN_POINT('Ctrl Pts',(-19.2888465797758,-2.30315448832917,
-330.864625399001)) ;
#30266 = CARTESIAN_POINT('Ctrl Pts',(-19.3096908029976,-2.12131182845833,
-330.86681465962)) ;
#30267 = CARTESIAN_POINT('Ctrl Pts',(-19.3362182933276,-1.8569132293746,-330.870031354084)) ;
#30268 = CARTESIAN_POINT('Ctrl Pts',(-19.3439488482247,-1.77457250128458,
-330.871037838639)) ;
#30269 = CARTESIAN_POINT('Ctrl Pts',(-19.3568380500606,-1.62717672532804,
-330.872849775708)) ;
#30270 = CARTESIAN_POINT('Ctrl Pts',(-19.3621951373493,-1.5621404642525,-330.873652974005)) ;
#30271 = CARTESIAN_POINT('Ctrl Pts',(-19.3743421431742,-1.40499853434457,
-330.875602349452)) ;
#30272 = CARTESIAN_POINT('Ctrl Pts',(-19.3808031020424,-1.31286916722493,
-330.876752239382)) ;
#30273 = CARTESIAN_POINT('Ctrl Pts',(-19.4034994741604,-0.952414834257095,
-330.881273907144)) ;
#30274 = CARTESIAN_POINT('Ctrl Pts',(-19.414821346963,-0.683810967337861,
-330.884692250171)) ;
#30275 = CARTESIAN_POINT('Ctrl Pts',(-19.4333941850321,0.185209165867029,
-330.895825645696)) ;
#30276 = CARTESIAN_POINT('Ctrl Pts',(-19.4183858938385,0.785750027072752,
-330.903623998144)) ;
#30277 = CARTESIAN_POINT('Ctrl Pts',(-19.3489830945429,1.75692650705994,-330.916094149874)) ;
#30278 = CARTESIAN_POINT('Ctrl Pts',(-19.3116529470566,2.12837945326687,-330.920832691249)) ;
#30279 = CARTESIAN_POINT('Ctrl Pts',(-19.2432337963619,2.65589124783422,-330.927492419551)) ;
#30280 = CARTESIAN_POINT('Ctrl Pts',(-19.2208958041448,2.81300015002547,-330.929467301301)) ;
#30281 = CARTESIAN_POINT('Ctrl Pts',(-19.1776056359031,3.09282390302031,-330.932969133975)) ;
#30282 = CARTESIAN_POINT('Ctrl Pts',(-19.1573941168371,3.2156443087705,-330.934500788558)) ;
#30283 = CARTESIAN_POINT('Ctrl Pts',(-19.1115612297677,3.478373320119,-330.937766208512)) ;
#30284 = CARTESIAN_POINT('Ctrl Pts',(-19.0855808259822,3.618212016481,-330.939497525196)) ;
#30285 = CARTESIAN_POINT('Ctrl Pts',(-19.0061536709267,4.02104000803802,-330.944467797047)) ;
#30286 = CARTESIAN_POINT('Ctrl Pts',(-18.948789883894,4.2832233693699,-330.947681286156)) ;
#30287 = CARTESIAN_POINT('Ctrl Pts',(-18.7972499771282,4.9130429138484,-330.955373094013)) ;
#30288 = CARTESIAN_POINT('Ctrl Pts',(-18.6976973515694,5.27927188342988,-330.95982178649)) ;
#30289 = CARTESIAN_POINT('Ctrl Pts',(-18.4082348089666,6.23284267538835,-330.971468881784)) ;
#30290 = CARTESIAN_POINT('Ctrl Pts',(-18.2009509578486,6.81445635987414,-330.978630429769)) ;
#30291 = CARTESIAN_POINT('Ctrl Pts',(-17.9252345924882,7.48520390493788,-330.987347795917)) ;
#30292 = CARTESIAN_POINT('Ctrl Pts',(-17.8832982708335,7.58485040080098,-330.988655402369)) ;
#30293 = CARTESIAN_POINT('Ctrl Pts',(-17.8139152370466,7.74593934730319,-330.990793320313)) ;
#30294 = CARTESIAN_POINT('Ctrl Pts',(-17.7869772125323,7.80759848444304,-330.991617420497)) ;
#30295 = CARTESIAN_POINT('Ctrl Pts',(-17.7294479002143,7.93743573431328,-330.993366028853)) ;
#30296 = CARTESIAN_POINT('Ctrl Pts',(-17.6987825120908,8.00557970757228,-330.994291410488)) ;
#30297 = CARTESIAN_POINT('Ctrl Pts',(-17.6081667408616,8.20387853485462,-330.997004737687)) ;
#30298 = CARTESIAN_POINT('Ctrl Pts',(-17.5471684667196,8.33354892509288,-330.998804862371)) ;
#30299 = CARTESIAN_POINT('Ctrl Pts',(-17.397463177574,8.64286038531919,-331.003150931144)) ;
#30300 = CARTESIAN_POINT('Ctrl Pts',(-17.3074008334412,8.82182729780902,-331.005708189282)) ;
#30301 = CARTESIAN_POINT('Ctrl Pts',(-16.8699117524567,9.65868528235885,-331.017820176187)) ;
#30302 = CARTESIAN_POINT('Ctrl Pts',(-16.4876420828482,10.2976594043948,-331.027496797488)) ;
#30303 = CARTESIAN_POINT('Ctrl Pts',(-15.924123175725,11.1274453814007,-331.040228694641)) ;
#30304 = CARTESIAN_POINT('Ctrl Pts',(-15.7743053148953,11.3388285046095,-331.043490531975)) ;
#30305 = CARTESIAN_POINT('Ctrl Pts',(-15.5358784895606,11.6613582105786,-331.048490760577)) ;
#30306 = CARTESIAN_POINT('Ctrl Pts',(-15.4502026991812,11.7746351273239,-331.050251590252)) ;
#30307 = CARTESIAN_POINT('Ctrl Pts',(-15.2947309151183,11.9755744748375,-331.05338363624)) ;
#30308 = CARTESIAN_POINT('Ctrl Pts',(-15.2254041235981,12.0635917982819,-331.054758573104)) ;
#30309 = CARTESIAN_POINT('Ctrl Pts',(-15.0585477967697,12.2717030686127,-331.058017300648)) ;
#30310 = CARTESIAN_POINT('Ctrl Pts',(-14.9603373874767,12.391241394261,-331.059895347255)) ;
#30311 = CARTESIAN_POINT('Ctrl Pts',(-14.6325596356343,12.7806233341624,-331.066037554248)) ;
#30312 = CARTESIAN_POINT('Ctrl Pts',(-14.3970377085091,13.0453608723597,-331.070252134838)) ;
#30313 = CARTESIAN_POINT('Ctrl Pts',(-13.7090266865031,13.777377372025,-331.082095264247)) ;
#30314 = CARTESIAN_POINT('Ctrl Pts',(-13.2401313112787,14.2285789934572,-331.089615235417)) ;
#30315 = CARTESIAN_POINT('Ctrl Pts',(-12.7064547124593,14.6928515837352,-331.097953515442)) ;
#30316 = CARTESIAN_POINT('Ctrl Pts',(-12.6632524946571,14.7301023511176,-331.098627143809)) ;
#30317 = CARTESIAN_POINT('Ctrl Pts',(-12.4617243056367,14.9023265668085,-331.101764427376)) ;
#30318 = CARTESIAN_POINT('Ctrl Pts',(-12.3014007019916,15.0349409799813,-331.104245770373)) ;
#30319 = CARTESIAN_POINT('Ctrl Pts',(-12.0713018612641,15.2191264893781,-331.107807888769)) ;
#30320 = CARTESIAN_POINT('Ctrl Pts',(-12.0032637410207,15.2728451593789,-331.108861299042)) ;
#30321 = CARTESIAN_POINT('Ctrl Pts',(-11.8830645250443,15.366447655184,-331.110724564635)) ;
#30322 = CARTESIAN_POINT('Ctrl Pts',(-11.8310566653302,15.4065257023405,-331.111531616058)) ;
#30323 = CARTESIAN_POINT('Ctrl Pts',(-11.7100692391109,15.4987865468811,-331.113411205779)) ;
#30324 = CARTESIAN_POINT('Ctrl Pts',(-11.640942540443,15.5507737027415,-331.114486479666)) ;
#30325 = CARTESIAN_POINT('Ctrl Pts',(-11.3967472830981,15.7318815403067,-331.118286277072)) ;
#30326 = CARTESIAN_POINT('Ctrl Pts',(-11.2198593801426,15.85852138844,-331.121040936249)) ;
#30327 = CARTESIAN_POINT('Ctrl Pts',(-10.7212332974238,16.2029848856168,-331.128772615892)) ;
#30328 = CARTESIAN_POINT('Ctrl Pts',(-10.3950316962106,16.414167001091,-331.133791522867)) ;
#30329 = CARTESIAN_POINT('Ctrl Pts',(-9.88495471592185,16.7230824041626,-331.141484406092)) ;
#30330 = CARTESIAN_POINT('Ctrl Pts',(-9.70547547893952,16.8278804557197,-331.144163293726)) ;
#30331 = CARTESIAN_POINT('Ctrl Pts',(-9.1625393651518,17.1333252785833,-331.152163877547)) ;
#30332 = CARTESIAN_POINT('Ctrl Pts',(-8.79429678800166,17.3252217356206,-331.157451926281)) ;
#30333 = CARTESIAN_POINT('Ctrl Pts',(-8.28120864010469,17.5720230164607,-331.164594667441)) ;
#30334 = CARTESIAN_POINT('Ctrl Pts',(-8.14143750739785,17.6372164706472,-331.16651845144)) ;
#30335 = CARTESIAN_POINT('Ctrl Pts',(-7.88588942441923,17.7527266713724,-331.169995561824)) ;
#30336 = CARTESIAN_POINT('Ctrl Pts',(-7.77037003803242,17.8035924971271,-331.171552656667)) ;
#30337 = CARTESIAN_POINT('Ctrl Pts',(-7.53240447057082,17.9056168790374,-331.174730541355)) ;
#30338 = CARTESIAN_POINT('Ctrl Pts',(-7.4099132463587,17.9566538827404,-331.176350414048)) ;
#30339 = CARTESIAN_POINT('Ctrl Pts',(-7.08857207073964,18.0866954036499,-331.180560031698)) ;
#30340 = CARTESIAN_POINT('Ctrl Pts',(-6.88892274665502,18.1636766164957,-331.183135775338)) ;
#30341 = CARTESIAN_POINT('Ctrl Pts',(-6.55348934718931,18.2866875529465,-331.187404742255)) ;
#30342 = CARTESIAN_POINT('Ctrl Pts',(-6.41839437260853,18.3345405727428,-331.189108467082)) ;
#30343 = CARTESIAN_POINT('Ctrl Pts',(-5.84735609148978,18.5297274377507,-331.196252665333)) ;
#30344 = CARTESIAN_POINT('Ctrl Pts',(-5.40677866210083,18.6630414739857,-331.201621130441)) ;
#30345 = CARTESIAN_POINT('Ctrl Pts',(-4.88664933724325,18.8004611273291,-331.207905198598)) ;
#30346 = CARTESIAN_POINT('Ctrl Pts',(-4.81129599690855,18.8198860563384,-331.208814409189)) ;
#30347 = CARTESIAN_POINT('Ctrl Pts',(-4.35714428029066,18.9340535098657,-331.214290652005)) ;
#30348 = CARTESIAN_POINT('Ctrl Pts',(-3.97567707510888,19.0178095230492,-331.218873863164)) ;
#30349 = CARTESIAN_POINT('Ctrl Pts',(-3.47596619974279,19.1118343350458,-331.22497307401)) ;
#30350 = CARTESIAN_POINT('Ctrl Pts',(-3.35978949627325,19.1325995921073,-331.226397870683)) ;
#30351 = CARTESIAN_POINT('Ctrl Pts',(-3.1813651293406,19.1628156478985,-331.228600889527)) ;
#30352 = CARTESIAN_POINT('Ctrl Pts',(-3.11924863708553,19.1730246849707,-331.229370593746)) ;
#30353 = CARTESIAN_POINT('Ctrl Pts',(-2.98816267053531,19.1939151711428,-331.231001667201)) ;
#30354 = CARTESIAN_POINT('Ctrl Pts',(-2.91918308001032,19.2045272230485,-331.231863946603)) ;
#30355 = CARTESIAN_POINT('Ctrl Pts',(-2.73343258707251,19.2320798011709,-331.234195223227)) ;
#30356 = CARTESIAN_POINT('Ctrl Pts',(-2.61656207658776,19.2483284995023,-331.23567187278)) ;
#30357 = CARTESIAN_POINT('Ctrl Pts',(-2.41937249954605,19.2739149766195,-331.238175863511)) ;
#30358 = CARTESIAN_POINT('Ctrl Pts',(-2.3391299330862,19.2838179040819,-331.239198301804)) ;
#30359 = CARTESIAN_POINT('Ctrl Pts',(-2.1259891498276,19.3087721816363,-331.241921423551)) ;
#30360 = CARTESIAN_POINT('Ctrl Pts',(-1.99299336661796,19.3229524249205,-331.243628118754)) ;
#30361 = CARTESIAN_POINT('Ctrl Pts',(-1.27078286024051,19.3924201846598,-331.252920262184)) ;
#30362 = CARTESIAN_POINT('Ctrl Pts',(-0.679421988398216,19.4221326613697,
-331.260605808213)) ;
#30363 = CARTESIAN_POINT('Ctrl Pts',(0.294082953597015,19.4265243163244,-331.273079881172)) ;
#30364 = CARTESIAN_POINT('Ctrl Pts',(0.675763093308313,19.4169945463091,-331.277928199104)) ;
#30365 = CARTESIAN_POINT('Ctrl Pts',(1.21613940107922,19.3875490383569,-331.284704770253)) ;
#30366 = CARTESIAN_POINT('Ctrl Pts',(1.37525128023383,19.3769124674497,-331.286689602766)) ;
#30367 = CARTESIAN_POINT('Ctrl Pts',(1.6583697248742,19.3544812948215,-331.290202361248)) ;
#30368 = CARTESIAN_POINT('Ctrl Pts',(1.78242778168078,19.3434507672801,-331.291735102424)) ;
#30369 = CARTESIAN_POINT('Ctrl Pts',(2.04743223517123,19.3173170485515,-331.294995874371)) ;
#30370 = CARTESIAN_POINT('Ctrl Pts',(2.18833682487586,19.3018625712689,-331.296721534203)) ;
#30371 = CARTESIAN_POINT('Ctrl Pts',(2.59260769684783,19.2530382263045,-331.301651623129)) ;
#30372 = CARTESIAN_POINT('Ctrl Pts',(2.85547576797671,19.2158100044674,-331.304831267606)) ;
#30373 = CARTESIAN_POINT('Ctrl Pts',(3.31312860541289,19.1413972008253,-331.31033834568)) ;
#30374 = CARTESIAN_POINT('Ctrl Pts',(3.50826058420085,19.1065961317247,-331.312677366791)) ;
#30375 = CARTESIAN_POINT('Ctrl Pts',(4.14713309221299,18.9825384146899,-331.320325578312)) ;
#30376 = CARTESIAN_POINT('Ctrl Pts',(4.58828883765788,18.8807595941433,-331.325588122022)) ;
#30377 = CARTESIAN_POINT('Ctrl Pts',(5.37854189113753,18.6691055552241,-331.335171335634)) ;
#30378 = CARTESIAN_POINT('Ctrl Pts',(5.72885818746038,18.5646006623749,-331.339477409204)) ;
#30379 = CARTESIAN_POINT('Ctrl Pts',(6.17160663977121,18.4187954281179,-331.345090650365)) ;
#30380 = CARTESIAN_POINT('Ctrl Pts',(6.26695107226405,18.3865733011086,-331.346309800873)) ;
#30381 = CARTESIAN_POINT('Ctrl Pts',(6.42512708956755,18.3317436429507,-331.348352636374)) ;
#30382 = CARTESIAN_POINT('Ctrl Pts',(6.48810028677848,18.3095504528684,-331.34917136159)) ;
#30383 = CARTESIAN_POINT('Ctrl Pts',(6.62447888903119,18.2606955902884,-331.3509570715)) ;
#30384 = CARTESIAN_POINT('Ctrl Pts',(6.69784030912312,18.2339150805707,-331.351925427461)) ;
#30385 = CARTESIAN_POINT('Ctrl Pts',(6.92288414697814,18.1502216596197,-331.354917680029)) ;
#30386 = CARTESIAN_POINT('Ctrl Pts',(7.07401754044474,18.0918530533116,-331.356957623321)) ;
#30387 = CARTESIAN_POINT('Ctrl Pts',(7.34265980990761,17.9842209029808,-331.360627456576)) ;
#30388 = CARTESIAN_POINT('Ctrl Pts',(7.46044775047311,17.9356787963735,-331.362251767212)) ;
#30389 = CARTESIAN_POINT('Ctrl Pts',(8.06999595128347,17.6774316557039,-331.370723279508)) ;
#30390 = CARTESIAN_POINT('Ctrl Pts',(8.55342321120576,17.4486497086714,-331.377658905016)) ;
#30391 = CARTESIAN_POINT('Ctrl Pts',(9.41813592380486,16.9948423548979,-331.390206336027)) ;
#30392 = CARTESIAN_POINT('Ctrl Pts',(9.8023523837135,16.7761688260788,-331.395837017219)) ;
#30393 = CARTESIAN_POINT('Ctrl Pts',(10.3182349396405,16.4587807320057,-331.40342784363)) ;
#30394 = CARTESIAN_POINT('Ctrl Pts',(10.4566037209068,16.3712209130232,-331.405467394155)) ;
#30395 = CARTESIAN_POINT('Ctrl Pts',(10.6986374708936,16.2137414092363,-331.409040918764)) ;
#30396 = CARTESIAN_POINT('Ctrl Pts',(10.8027653145149,16.1445506542111,-331.410580323744)) ;
#30397 = CARTESIAN_POINT('Ctrl Pts',(11.0215371979506,15.9961171278713,-331.413819361293)) ;
#30398 = CARTESIAN_POINT('Ctrl Pts',(11.1360111170614,15.916636008884,-331.415517017434)) ;
#30399 = CARTESIAN_POINT('Ctrl Pts',(11.4545901149544,15.6903220085739,-331.420251574801)) ;
#30400 = CARTESIAN_POINT('Ctrl Pts',(11.6567141952946,15.5407481779227,-331.423266881358)) ;
#30401 = CARTESIAN_POINT('Ctrl Pts',(12.1267959399637,15.1785511448863,-331.430325725985)) ;
#30402 = CARTESIAN_POINT('Ctrl Pts',(12.3921539857327,14.9626907564532,-331.434346521763)) ;
#30403 = CARTESIAN_POINT('Ctrl Pts',(13.1570025657176,14.3062011665578,-331.446142919059)) ;
#30404 = CARTESIAN_POINT('Ctrl Pts',(13.6396895262847,13.8467675469215,-331.453848006321)) ;
#30405 = CARTESIAN_POINT('Ctrl Pts',(14.1780523753486,13.2788198189066,-331.463237489596)) ;
#30406 = CARTESIAN_POINT('Ctrl Pts',(14.2575165484111,13.1934622731863,-331.464645771229)) ;
#30407 = CARTESIAN_POINT('Ctrl Pts',(14.3785177479979,13.0611172621129,-331.466829156981)) ;
#30408 = CARTESIAN_POINT('Ctrl Pts',(14.4206039870436,13.0146355078446,-331.467595977805)) ;
#30409 = CARTESIAN_POINT('Ctrl Pts',(14.5092485848617,12.9157749124534,-331.469227814815)) ;
#30410 = CARTESIAN_POINT('Ctrl Pts',(14.5557500237847,12.8633462717531,-331.470093798269)) ;
#30411 = CARTESIAN_POINT('Ctrl Pts',(14.6807550183832,12.720861986213,-331.472447370338)) ;
#30412 = CARTESIAN_POINT('Ctrl Pts',(14.7587131279826,12.6303319166457,-331.473942855147)) ;
#30413 = CARTESIAN_POINT('Ctrl Pts',(15.0984885510165,12.2283209781896,-331.480573149272)) ;
#30414 = CARTESIAN_POINT('Ctrl Pts',(15.3513163869708,11.9093775960655,-331.485803614236)) ;
#30415 = CARTESIAN_POINT('Ctrl Pts',(16.033542328605,10.9908903366001,-331.500554969905)) ;
#30416 = CARTESIAN_POINT('Ctrl Pts',(16.4390966795643,10.3745004117369,-331.510079911123)) ;
#30417 = CARTESIAN_POINT('Ctrl Pts',(16.897800213983,9.58262067576621,-331.521573823901)) ;
#30418 = CARTESIAN_POINT('Ctrl Pts',(16.9848485366414,9.4274700428485,-331.523793649394)) ;
#30419 = CARTESIAN_POINT('Ctrl Pts',(17.1301451745573,9.15995425435194,-331.527565858801)) ;
#30420 = CARTESIAN_POINT('Ctrl Pts',(17.1894489665443,9.04817550223545,-331.529125840211)) ;
#30421 = CARTESIAN_POINT('Ctrl Pts',(17.3096813273314,8.81610667843185,-331.532331734902)) ;
#30422 = CARTESIAN_POINT('Ctrl Pts',(17.3704581071726,8.69574550137857,-331.533976483134)) ;
#30423 = CARTESIAN_POINT('Ctrl Pts',(17.5296641065612,8.37212635753797,-331.538352629366)) ;
#30424 = CARTESIAN_POINT('Ctrl Pts',(17.625810187505,8.16776829460154,-331.541067762122)) ;
#30425 = CARTESIAN_POINT('Ctrl Pts',(17.8375099440627,7.69664565295041,-331.54722982063)) ;
#30426 = CARTESIAN_POINT('Ctrl Pts',(17.9506825314833,7.42887019106929,-331.550661979062)) ;
#30427 = CARTESIAN_POINT('Ctrl Pts',(18.2133268869269,6.76634635651274,-331.559028852291)) ;
#30428 = CARTESIAN_POINT('Ctrl Pts',(18.3560242844578,6.36907305596773,-331.563938108192)) ;
#30429 = CARTESIAN_POINT('Ctrl Pts',(18.5977918864768,5.62013973394375,-331.573155077109)) ;
#30430 = CARTESIAN_POINT('Ctrl Pts',(18.700103592785,5.26972087544843,-331.577453234272)) ;
#30431 = CARTESIAN_POINT('Ctrl Pts',(18.8187032720011,4.81640576130231,-331.583091690668)) ;
#30432 = CARTESIAN_POINT('Ctrl Pts',(18.8441222778304,4.71597421879959,-331.584345860284)) ;
#30433 = CARTESIAN_POINT('Ctrl Pts',(18.8845487659721,4.55070014301087,-331.586421144224)) ;
#30434 = CARTESIAN_POINT('Ctrl Pts',(18.9000285810633,4.48597520402972,-331.587236758795)) ;
#30435 = CARTESIAN_POINT('Ctrl Pts',(18.9325746034242,4.3467329991501,-331.588998506909)) ;
#30436 = CARTESIAN_POINT('Ctrl Pts',(18.9495341267605,4.27219208832658,-331.589945823497)) ;
#30437 = CARTESIAN_POINT('Ctrl Pts',(18.9990398123436,4.04850761125286,-331.592799053409)) ;
#30438 = CARTESIAN_POINT('Ctrl Pts',(19.0302683426821,3.89907865454126,-331.594719023881)) ;
#30439 = CARTESIAN_POINT('Ctrl Pts',(19.1021332306195,3.53375006641528,-331.599434449502)) ;
#30440 = CARTESIAN_POINT('Ctrl Pts',(19.1408746532084,3.31749917776198,-331.602243717838)) ;
#30441 = CARTESIAN_POINT('Ctrl Pts',(19.2747221437745,2.48971750031321,-331.613015256119)) ;
#30442 = CARTESIAN_POINT('Ctrl Pts',(19.3442535973299,1.87442326248503,-331.621047414326)) ;
#30443 = CARTESIAN_POINT('Ctrl Pts',(19.4051245780302,0.935624312395659,-331.63305023746)) ;
#30444 = CARTESIAN_POINT('Ctrl Pts',(19.4179648412124,0.613917664051277,-331.637121206606)) ;
#30445 = CARTESIAN_POINT('Ctrl Pts',(19.4250662502585,0.141622268101417,-331.643022336498)) ;
#30446 = CARTESIAN_POINT('Ctrl Pts',(19.4255805070409,-0.00881706035484106,
-331.644890966908)) ;
#30447 = CARTESIAN_POINT('Ctrl Pts',(19.4233313279023,-0.283162925531712,
-331.648278481003)) ;
#30448 = CARTESIAN_POINT('Ctrl Pts',(19.4211296882431,-0.407066081420953,
-331.649800890658)) ;
#30449 = CARTESIAN_POINT('Ctrl Pts',(19.4136203739906,-0.68169974136198,-331.653159362784)) ;
#30450 = CARTESIAN_POINT('Ctrl Pts',(19.4077425197806,-0.832406708846909,
-331.654991652664)) ;
#30451 = CARTESIAN_POINT('Ctrl Pts',(19.3836808742657,-1.30726358108212,-331.660734603511)) ;
#30452 = CARTESIAN_POINT('Ctrl Pts',(19.3591257274906,-1.63103464049096,-331.664604863635)) ;
#30453 = CARTESIAN_POINT('Ctrl Pts',(19.2726884669947,-2.48594464710716,-331.674756787145)) ;
#30454 = CARTESIAN_POINT('Ctrl Pts',(19.1969731522516,-3.01540431053611,-331.680970272482)) ;
#30455 = CARTESIAN_POINT('Ctrl Pts',(19.0337967053702,-3.89553267246137,-331.691446789089)) ;
#30456 = CARTESIAN_POINT('Ctrl Pts',(18.9582229621502,-4.24810226674831,-331.695685918897)) ;
#30457 = CARTESIAN_POINT('Ctrl Pts',(18.8452227867904,-4.71188446832313,-331.701413104294)) ;
#30458 = CARTESIAN_POINT('Ctrl Pts',(18.8165397460758,-4.82515378529315,-331.702824029085)) ;
#30459 = CARTESIAN_POINT('Ctrl Pts',(18.7708862554957,-4.99883895135747,-331.705010554843)) ;
#30460 = CARTESIAN_POINT('Ctrl Pts',(18.7546420560114,-5.05944295533292,-331.70577783511)) ;
#30461 = CARTESIAN_POINT('Ctrl Pts',(18.7196458418115,-5.18752243341876,-331.707409531894)) ;
#30462 = CARTESIAN_POINT('Ctrl Pts',(18.7008219816499,-5.25497731923986,-331.708274906458)) ;
#30463 = CARTESIAN_POINT('Ctrl Pts',(18.6489665552764,-5.43699239445489,-331.710624823637)) ;
#30464 = CARTESIAN_POINT('Ctrl Pts',(18.6152443889123,-5.55135264194645,-331.712117222362)) ;
#30465 = CARTESIAN_POINT('Ctrl Pts',(18.5565463371486,-5.7438612802859,-331.714652236239)) ;
#30466 = CARTESIAN_POINT('Ctrl Pts',(18.5321242968731,-5.82217514325223,-331.715689907923)) ;
#30467 = CARTESIAN_POINT('Ctrl Pts',(18.3470665836207,-6.40263425173374,-331.723423153028)) ;
#30468 = CARTESIAN_POINT('Ctrl Pts',(18.166543293511,-6.89820861068696,-331.730253415421)) ;
#30469 = CARTESIAN_POINT('Ctrl Pts',(17.7560341800969,-7.89677581851751,-331.744169610642)) ;
#30470 = CARTESIAN_POINT('Ctrl Pts',(17.5242809523818,-8.39853550809977,-331.751244501611)) ;
#30471 = CARTESIAN_POINT('Ctrl Pts',(17.2010805163503,-9.02646678313865,-331.760103505472)) ;
#30472 = CARTESIAN_POINT('Ctrl Pts',(17.1290824203861,-9.16235826844501,-331.762021641249)) ;
#30473 = CARTESIAN_POINT('Ctrl Pts',(16.9951124918703,-9.40811793995196,-331.765491871602)) ;
#30474 = CARTESIAN_POINT('Ctrl Pts',(16.9336696213793,-9.51826480963443,-331.767047680967)) ;
#30475 = CARTESIAN_POINT('Ctrl Pts',(16.8053081033755,-9.74319742647594,-331.770226222535)) ;
#30476 = CARTESIAN_POINT('Ctrl Pts',(16.738275665949,-9.85791074860768,-331.771848003521)) ;
#30477 = CARTESIAN_POINT('Ctrl Pts',(16.5597650232949,-10.1563269993446,-331.776070417144)) ;
#30478 = CARTESIAN_POINT('Ctrl Pts',(16.4464062461246,-10.3388837669153,-331.778656878971)) ;
#30479 = CARTESIAN_POINT('Ctrl Pts',(16.2519482638245,-10.6407517504064,-331.782946859227)) ;
#30480 = CARTESIAN_POINT('Ctrl Pts',(16.172506917948,-10.7611077601991,-331.784660916384)) ;
#30481 = CARTESIAN_POINT('Ctrl Pts',(15.8312171286155,-11.2658556770832,-331.791872992881)) ;
#30482 = CARTESIAN_POINT('Ctrl Pts',(15.5569478501701,-11.6416628477102,-331.797297582334)) ;
#30483 = CARTESIAN_POINT('Ctrl Pts',(15.2041539933649,-12.0903054840791,-331.803964756729)) ;
#30484 = CARTESIAN_POINT('Ctrl Pts',(15.1381763320924,-12.1728140823866,-331.805199370214)) ;
#30485 = CARTESIAN_POINT('Ctrl Pts',(14.8459048393145,-12.5322638751701,-331.810622069613)) ;
#30486 = CARTESIAN_POINT('Ctrl Pts',(14.612661027665,-12.8034630071606,-331.814828187538)) ;
#30487 = CARTESIAN_POINT('Ctrl Pts',(14.2936007362832,-13.1543607239344,-331.820518624368)) ;
#30488 = CARTESIAN_POINT('Ctrl Pts',(14.2143615330848,-13.2399454006237,-331.821927064301)) ;
#30489 = CARTESIAN_POINT('Ctrl Pts',(14.0913424553331,-13.3704384694254,-331.824110638086)) ;
#30490 = CARTESIAN_POINT('Ctrl Pts',(14.048107783899,-13.4158572122377,-331.824877486402)) ;
#30491 = CARTESIAN_POINT('Ctrl Pts',(13.9716475714101,-13.4954050606076,-331.826233460196)) ;
#30492 = CARTESIAN_POINT('Ctrl Pts',(13.9385150065128,-13.5296227964357,-331.826821000509)) ;
#30493 = CARTESIAN_POINT('Ctrl Pts',(13.8606085807449,-13.609490930354,-331.828202022283)) ;
#30494 = CARTESIAN_POINT('Ctrl Pts',(13.8157344951193,-13.6550428033593,-331.828997109471)) ;
#30495 = CARTESIAN_POINT('Ctrl Pts',(13.7692616165892,-13.7017540239607,-331.82981972534)) ;
#30496 = CARTESIAN_POINT('Ctrl Pts',(13.7678866789893,-13.7031355971437,-331.829844062378)) ;
#30497 = CARTESIAN_POINT('Ctrl Pts',(13.7650823617773,-13.7059526001323,-331.829893698622)) ;
#30498 = CARTESIAN_POINT('Ctrl Pts',(13.7636529655195,-13.7073880133427,-331.829918998064)) ;
#30499 = CARTESIAN_POINT('Ctrl Pts',(13.7607365431826,-13.7103157960541,-331.829970615335)) ;
#30500 = CARTESIAN_POINT('Ctrl Pts',(13.759249498805,-13.7118081472885,-331.829996933423)) ;
#30501 = CARTESIAN_POINT('Ctrl Pts',(13.7562143858257,-13.7148531008645,-331.830050647834)) ;
#30502 = CARTESIAN_POINT('Ctrl Pts',(13.7546662970794,-13.716405683089,-331.830078044441)) ;
#30503 = CARTESIAN_POINT('Ctrl Pts',(13.7515054797994,-13.7195746017318,-331.830133979621)) ;
#30504 = CARTESIAN_POINT('Ctrl Pts',(13.7498927290853,-13.7211909159549,-331.830162518506)) ;
#30505 = CARTESIAN_POINT('Ctrl Pts',(13.7465987356688,-13.7244910237956,-331.830220806126)) ;
#30506 = CARTESIAN_POINT('Ctrl Pts',(13.7449174684897,-13.7261747929328,-331.830250555202)) ;
#30507 = CARTESIAN_POINT('Ctrl Pts',(13.7414823366226,-13.7296137727576,-331.830311335531)) ;
#30508 = CARTESIAN_POINT('Ctrl Pts',(13.7397284448924,-13.7313689564231,-331.83034236716)) ;
#30509 = CARTESIAN_POINT('Ctrl Pts',(13.7361436871001,-13.7349549803189,-331.830405789673)) ;
#30510 = CARTESIAN_POINT('Ctrl Pts',(13.7343127911914,-13.7367857906339,-331.83043818097)) ;
#30511 = CARTESIAN_POINT('Ctrl Pts',(13.7318804184366,-13.7392170772611,-331.830481211385)) ;
#30512 = CARTESIAN_POINT('Ctrl Pts',(13.7312792681265,-13.7398178802729,-331.83049184601)) ;
#30513 = CARTESIAN_POINT('Ctrl Pts',(13.7300057996842,-13.741090445955,-331.83051437392)) ;
#30514 = CARTESIAN_POINT('Ctrl Pts',(13.7293334717162,-13.7417621987025,-331.830526267341)) ;
#30515 = CARTESIAN_POINT('Ctrl Pts',(13.727908788006,-13.7431854545801,-331.830551469452)) ;
#30516 = CARTESIAN_POINT('Ctrl Pts',(13.7271564198459,-13.7439369452817,-331.830564778311)) ;
#30517 = CARTESIAN_POINT('Ctrl Pts',(13.7255616016073,-13.7455296419539,-331.830592988992)) ;
#30518 = CARTESIAN_POINT('Ctrl Pts',(13.724719135905,-13.7463708322551,-331.830607891027)) ;
#30519 = CARTESIAN_POINT('Ctrl Pts',(13.7229326966182,-13.7481542391314,-331.830639489967)) ;
#30520 = CARTESIAN_POINT('Ctrl Pts',(13.7219887032735,-13.7490964359878,-331.830656187142)) ;
#30521 = CARTESIAN_POINT('Ctrl Pts',(13.7199862039139,-13.7510947127911,-331.830691606132)) ;
#30522 = CARTESIAN_POINT('Ctrl Pts',(13.7189276730188,-13.7521507677242,-331.830710328285)) ;
#30523 = CARTESIAN_POINT('Ctrl Pts',(13.7166812751135,-13.7543913937036,-331.830750059085)) ;
#30524 = CARTESIAN_POINT('Ctrl Pts',(13.7154933765718,-13.7555759331062,-331.83077106816)) ;
#30525 = CARTESIAN_POINT('Ctrl Pts',(13.7129713221462,-13.7580902041727,-331.83081567165)) ;
#30526 = CARTESIAN_POINT('Ctrl Pts',(13.7116371262557,-13.7594198956949,-331.830839266607)) ;
#30527 = CARTESIAN_POINT('Ctrl Pts',(13.7088031344191,-13.7622434981691,-331.830889383391)) ;
#30528 = CARTESIAN_POINT('Ctrl Pts',(13.7073032876514,-13.7637373580543,-331.830915905903)) ;
#30529 = CARTESIAN_POINT('Ctrl Pts',(13.7041158552415,-13.7669110295604,-331.830972268592)) ;
#30530 = CARTESIAN_POINT('Ctrl Pts',(13.7024282048685,-13.7685907761156,-331.831002109636)) ;
#30531 = CARTESIAN_POINT('Ctrl Pts',(13.6988397977451,-13.7721610643623,-331.831065557031)) ;
#30532 = CARTESIAN_POINT('Ctrl Pts',(13.6969389584011,-13.7740515229491,-331.831099164484)) ;
#30533 = CARTESIAN_POINT('Ctrl Pts',(13.692895080019,-13.7780716522924,-331.831170657896)) ;
#30534 = CARTESIAN_POINT('Ctrl Pts',(13.6907519353816,-13.7802012166716,-331.831208545256)) ;
#30535 = CARTESIAN_POINT('Ctrl Pts',(13.6861900592354,-13.7847320713513,-331.831289187172)) ;
#30536 = CARTESIAN_POINT('Ctrl Pts',(13.683771192387,-13.7871332252523,-331.831331943514)) ;
#30537 = CARTESIAN_POINT('Ctrl Pts',(13.6786195459683,-13.7922444558256,-331.831422998825)) ;
#30538 = CARTESIAN_POINT('Ctrl Pts',(13.6758865927008,-13.7949543571621,-331.83147130007)) ;
#30539 = CARTESIAN_POINT('Ctrl Pts',(13.6700627845725,-13.8007256110362,-331.831574219964)) ;
#30540 = CARTESIAN_POINT('Ctrl Pts',(13.6669717063328,-13.8037867378325,-331.831628841517)) ;
#30541 = CARTESIAN_POINT('Ctrl Pts',(13.6603811915282,-13.8103090091323,-331.831745290105)) ;
#30542 = CARTESIAN_POINT('Ctrl Pts',(13.656881467316,-13.8137698624688,-331.831807120845)) ;
#30543 = CARTESIAN_POINT('Ctrl Pts',(13.64941585599,-13.821146944279,-331.831939004371)) ;
#30544 = CARTESIAN_POINT('Ctrl Pts',(13.6454495979948,-13.8250627967355,-331.832009061882)) ;
#30545 = CARTESIAN_POINT('Ctrl Pts',(13.6369848234021,-13.8334128046799,-331.83215856017)) ;
#30546 = CARTESIAN_POINT('Ctrl Pts',(13.6324858282832,-13.8378464740736,-331.83223800697)) ;
#30547 = CARTESIAN_POINT('Ctrl Pts',(13.5248819640244,-13.9437845153581,-331.834137890175)) ;
#30548 = CARTESIAN_POINT('Ctrl Pts',(13.4206484766666,-14.0441358984069,-331.835972293926)) ;
#30549 = CARTESIAN_POINT('Ctrl Pts',(13.0571938880751,-14.3863123139277,-331.842334198098)) ;
#30550 = CARTESIAN_POINT('Ctrl Pts',(12.7924806054615,-14.6222000338135,-331.846907147341)) ;
#30551 = CARTESIAN_POINT('Ctrl Pts',(12.0368699259241,-15.2592974549705,-331.859658796925)) ;
#30552 = CARTESIAN_POINT('Ctrl Pts',(11.5325684342379,-15.6439210804992,-331.86782089299)) ;
#30553 = CARTESIAN_POINT('Ctrl Pts',(10.8557137067247,-16.1096040968912,-331.878155817881)) ;
#30554 = CARTESIAN_POINT('Ctrl Pts',(10.6995260174173,-16.2137598168998,-331.880501359426)) ;
#30555 = CARTESIAN_POINT('Ctrl Pts',(10.4353333422919,-16.3844599024988,-331.884402626645)) ;
#30556 = CARTESIAN_POINT('Ctrl Pts',(10.3281421015145,-16.4522396360513,-331.885967651436)) ;
#30557 = CARTESIAN_POINT('Ctrl Pts',(10.1280936850837,-16.5760097265774,-331.888855868632)) ;
#30558 = CARTESIAN_POINT('Ctrl Pts',(10.0354165986346,-16.6322816796704,-331.890181159595)) ;
#30559 = CARTESIAN_POINT('Ctrl Pts',(9.80015059935628,-16.772448889877,-331.893514190319)) ;
#30560 = CARTESIAN_POINT('Ctrl Pts',(9.65695198137309,-16.8553039742803,-331.895514152812)) ;
#30561 = CARTESIAN_POINT('Ctrl Pts',(9.33334597599243,-17.0370654714374,-331.899973650054)) ;
#30562 = CARTESIAN_POINT('Ctrl Pts',(9.15239033309964,-17.1349554519541,-331.902426150856)) ;
#30563 = CARTESIAN_POINT('Ctrl Pts',(8.58442224059697,-17.4306396560204,-331.910012974524)) ;
#30564 = CARTESIAN_POINT('Ctrl Pts',(8.1923038977197,-17.6183331030163,-331.915090653946)) ;
#30565 = CARTESIAN_POINT('Ctrl Pts',(7.66602066844943,-17.8488750695102,-331.92180113646)) ;
#30566 = CARTESIAN_POINT('Ctrl Pts',(7.53721722725401,-17.9036468518039,-331.923435695687)) ;
#30567 = CARTESIAN_POINT('Ctrl Pts',(7.34270465750832,-17.9838893707481,-331.925897699522)) ;
#30568 = CARTESIAN_POINT('Ctrl Pts',(7.27743047854187,-18.0104023889908,-331.926722822383)) ;
#30569 = CARTESIAN_POINT('Ctrl Pts',(6.90069431434913,-18.1610423311331,-331.931481700634)) ;
#30570 = CARTESIAN_POINT('Ctrl Pts',(6.58620492388242,-18.2774435932866,-331.935439991101)) ;
#30571 = CARTESIAN_POINT('Ctrl Pts',(6.17521892875224,-18.4175754268229,-331.940671119721)) ;
#30572 = CARTESIAN_POINT('Ctrl Pts',(6.08133368959512,-18.448788413838,-331.941870077088)) ;
#30573 = CARTESIAN_POINT('Ctrl Pts',(5.92391672859546,-18.4997908838497,-331.943889841785)) ;
#30574 = CARTESIAN_POINT('Ctrl Pts',(5.86051436307038,-18.5199736382629,-331.944705952644)) ;
#30575 = CARTESIAN_POINT('Ctrl Pts',(5.73778777951122,-18.5583476229468,-331.946291398161)) ;
#30576 = CARTESIAN_POINT('Ctrl Pts',(5.67847777592145,-18.5765810964998,-331.947060036303)) ;
#30577 = CARTESIAN_POINT('Ctrl Pts',(5.52302576657717,-18.6235571428067,-331.949080058718)) ;
#30578 = CARTESIAN_POINT('Ctrl Pts',(5.42674666363849,-18.6518394503323,-331.950336557173)) ;
#30579 = CARTESIAN_POINT('Ctrl Pts',(5.30139047913159,-18.6876104640521,-331.951977601693)) ;
#30580 = CARTESIAN_POINT('Ctrl Pts',(5.27250906713572,-18.6957795773398,-331.952356039048)) ;
#30581 = CARTESIAN_POINT('Ctrl Pts',(4.94498569454738,-18.7876003276764,-331.95665115048)) ;
#30582 = CARTESIAN_POINT('Ctrl Pts',(4.6444007520759,-18.8641551819347,-331.960625419525)) ;
#30583 = CARTESIAN_POINT('Ctrl Pts',(3.89897388127834,-19.0351077689637,-331.970469728847)) ;
#30584 = CARTESIAN_POINT('Ctrl Pts',(3.45240317785248,-19.1211463596962,-331.976355057538)) ;
#30585 = CARTESIAN_POINT('Ctrl Pts',(2.61281186644438,-19.2525321724997,-331.987250745142)) ;
#30586 = CARTESIAN_POINT('Ctrl Pts',(2.22062357708149,-19.3016997471526,-331.992272942745)) ;
#30587 = CARTESIAN_POINT('Ctrl Pts',(1.66796369768334,-19.3539171064948,-331.999224795714)) ;
#30588 = CARTESIAN_POINT('Ctrl Pts',(1.50853908457495,-19.3669956418256,-332.001215935438)) ;
#30589 = CARTESIAN_POINT('Ctrl Pts',(1.22963635803475,-19.3864109415802,-332.004674157661)) ;
#30590 = CARTESIAN_POINT('Ctrl Pts',(1.11022744190597,-19.3936156978999,-332.006146731842)) ;
#30591 = CARTESIAN_POINT('Ctrl Pts',(0.874553115364349,-19.4056517797823,
-332.009037717497)) ;
#30592 = CARTESIAN_POINT('Ctrl Pts',(0.758295660510367,-19.4105422870817,
-332.010456452545)) ;
#30593 = CARTESIAN_POINT('Ctrl Pts',(0.42797158224745,-19.4214655497624,-332.01446774434)) ;
#30594 = CARTESIAN_POINT('Ctrl Pts',(0.213839356670802,-19.4250033901669,
-332.017044336313)) ;
#30595 = CARTESIAN_POINT('Ctrl Pts',(-0.000307738671744689,-19.4249999975623,
-332.019601838681)) ;
#30596 = CARTESIAN_POINT('Origin',(0.,0.,-328.125)) ;
#30597 = CARTESIAN_POINT('',(0.000433346557224641,-19.4249999951663,-333.731156854276)) ;
#30598 = CARTESIAN_POINT('',(0.000492969430210768,-19.4249999937447,-333.518704187163)) ;
#30599 = CARTESIAN_POINT('',(-2.37887640734373E-15,-19.425,-328.125)) ;
#30600 = CARTESIAN_POINT('Ctrl Pts',(0.000438550581743774,-19.4249999950495,
-333.731600905675)) ;
#30601 = CARTESIAN_POINT('Ctrl Pts',(0.240637510252596,-19.4249945721721,
-333.728785913431)) ;
#30602 = CARTESIAN_POINT('Ctrl Pts',(0.480815547108525,-19.4205338949269,
-333.725958859962)) ;
#30603 = CARTESIAN_POINT('Ctrl Pts',(0.851896410024764,-19.4067538423618,
-333.721539728974)) ;
#30604 = CARTESIAN_POINT('Ctrl Pts',(0.982891383366073,-19.4005604725508,
-333.719969787331)) ;
#30605 = CARTESIAN_POINT('Ctrl Pts',(1.1856194422729,-19.3889170571926,-333.717518864773)) ;
#30606 = CARTESIAN_POINT('Ctrl Pts',(1.25740195541675,-19.3843941979241,-333.716646894659)) ;
#30607 = CARTESIAN_POINT('Ctrl Pts',(1.38947859584908,-19.3753356091217,-333.715033671219)) ;
#30608 = CARTESIAN_POINT('Ctrl Pts',(1.44977988429964,-19.3709168346406,-333.714293738554)) ;
#30609 = CARTESIAN_POINT('Ctrl Pts',(1.57220891118611,-19.3613705653717,-333.712783745029)) ;
#30610 = CARTESIAN_POINT('Ctrl Pts',(1.63433456706251,-19.3562253950017,-333.71201348384)) ;
#30611 = CARTESIAN_POINT('Ctrl Pts',(1.81051038550961,-19.3407805040398,-333.709818819947)) ;
#30612 = CARTESIAN_POINT('Ctrl Pts',(1.92449566265621,-19.3297712027147,-333.708386561347)) ;
#30613 = CARTESIAN_POINT('Ctrl Pts',(2.5999750293889,-19.2584957632611,-333.699838990668)) ;
#30614 = CARTESIAN_POINT('Ctrl Pts',(3.15872159764124,-19.1747752559848,-333.692530727464)) ;
#30615 = CARTESIAN_POINT('Ctrl Pts',(4.24737628719546,-18.9627735279104,-333.678224856074)) ;
#30616 = CARTESIAN_POINT('Ctrl Pts',(4.77711907509256,-18.8362979798261,-333.671231879681)) ;
#30617 = CARTESIAN_POINT('Ctrl Pts',(5.40873053154289,-18.6571389482682,-333.662960360255)) ;
#30618 = CARTESIAN_POINT('Ctrl Pts',(5.51634448419811,-18.6256045072849,-333.661553077209)) ;
#30619 = CARTESIAN_POINT('Ctrl Pts',(5.70502109786341,-18.5685373961315,-333.659089687623)) ;
#30620 = CARTESIAN_POINT('Ctrl Pts',(5.78620050290883,-18.5434012660412,-333.658031091294)) ;
#30621 = CARTESIAN_POINT('Ctrl Pts',(5.97797491577687,-18.4826389040108,-333.65553345334)) ;
#30622 = CARTESIAN_POINT('Ctrl Pts',(6.08842041596543,-18.4465514887318,-333.654097522711)) ;
#30623 = CARTESIAN_POINT('Ctrl Pts',(6.31779703954782,-18.3693195669106,-333.651120324027)) ;
#30624 = CARTESIAN_POINT('Ctrl Pts',(6.43666556746504,-18.3280058163714,-333.649580287407)) ;
#30625 = CARTESIAN_POINT('Ctrl Pts',(6.69866248205231,-18.2340833859465,-333.64619124668)) ;
#30626 = CARTESIAN_POINT('Ctrl Pts',(6.84158987289766,-18.180938481442,-333.644345993119)) ;
#30627 = CARTESIAN_POINT('Ctrl Pts',(7.72305880153826,-17.8413141327266,-333.632979958776)) ;
#30628 = CARTESIAN_POINT('Ctrl Pts',(8.44412843827558,-17.5115625117154,-333.623778977472)) ;
#30629 = CARTESIAN_POINT('Ctrl Pts',(9.38866556836915,-17.0076771927583,-333.611255258856)) ;
#30630 = CARTESIAN_POINT('Ctrl Pts',(9.6314419268088,-16.8713796318123,-333.60798790257)) ;
#30631 = CARTESIAN_POINT('Ctrl Pts',(9.98008412303638,-16.6656691367316,-333.603178597004)) ;
#30632 = CARTESIAN_POINT('Ctrl Pts',(10.0883338937597,-16.6003652389277,-333.601668449972)) ;
#30633 = CARTESIAN_POINT('Ctrl Pts',(10.2814157660855,-16.4812984826206,-333.598938309033)) ;
#30634 = CARTESIAN_POINT('Ctrl Pts',(10.3664830675631,-16.4279255720008,-333.597722542869)) ;
#30635 = CARTESIAN_POINT('Ctrl Pts',(10.494207516735,-16.3464015905828,-333.595874829783)) ;
#30636 = CARTESIAN_POINT('Ctrl Pts',(10.5371737812345,-16.3187378514082,-333.595249415472)) ;
#30637 = CARTESIAN_POINT('Ctrl Pts',(10.6314799209429,-16.2574912953265,-333.593867677147)) ;
#30638 = CARTESIAN_POINT('Ctrl Pts',(10.6827708388103,-16.2238341865602,-333.593110217067)) ;
#30639 = CARTESIAN_POINT('Ctrl Pts',(10.8243970424172,-16.1299362351075,-333.591003098212)) ;
#30640 = CARTESIAN_POINT('Ctrl Pts',(10.9143879648912,-16.0691801154643,-333.589646533754)) ;
#30641 = CARTESIAN_POINT('Ctrl Pts',(11.5215268367352,-15.6518256337858,-333.58038651016)) ;
#30642 = CARTESIAN_POINT('Ctrl Pts',(12.021622763175,-15.2710776274608,-333.572237469274)) ;
#30643 = CARTESIAN_POINT('Ctrl Pts',(12.7873928977199,-14.6270940283031,-333.559340496345)) ;
#30644 = CARTESIAN_POINT('Ctrl Pts',(13.0654454696614,-14.3792709244846,-333.554558504026)) ;
#30645 = CARTESIAN_POINT('Ctrl Pts',(13.4742372492339,-13.9932697159809,-333.547419731746)) ;
#30646 = CARTESIAN_POINT('Ctrl Pts',(13.6103537476888,-13.8609140320651,-333.545023222651)) ;
#30647 = CARTESIAN_POINT('Ctrl Pts',(13.7544823748773,-13.7165972027297,-333.542466301195)) ;
#30648 = CARTESIAN_POINT('Ctrl Pts',(13.7644455230011,-13.7065992743329,-333.542289447753)) ;
#30649 = CARTESIAN_POINT('Ctrl Pts',(13.7830246751824,-13.6879145781381,-333.541959464384)) ;
#30650 = CARTESIAN_POINT('Ctrl Pts',(13.7916433861455,-13.6792305121496,-333.541806311618)) ;
#30651 = CARTESIAN_POINT('Ctrl Pts',(13.8077909014775,-13.6629297779574,-333.541519230739)) ;
#30652 = CARTESIAN_POINT('Ctrl Pts',(13.8153216225214,-13.6553150151375,-333.541385286366)) ;
#30653 = CARTESIAN_POINT('Ctrl Pts',(13.8294972378057,-13.6409574725932,-333.541133043452)) ;
#30654 = CARTESIAN_POINT('Ctrl Pts',(13.8361435077236,-13.6342160556912,-333.54101473319)) ;
#30655 = CARTESIAN_POINT('Ctrl Pts',(13.8487128104924,-13.6214481569775,-333.540790900817)) ;
#30656 = CARTESIAN_POINT('Ctrl Pts',(13.8546368443151,-13.615422663762,-333.540685370147)) ;
#30657 = CARTESIAN_POINT('Ctrl Pts',(13.8658920265613,-13.6039597652379,-333.540484801485)) ;
#30658 = CARTESIAN_POINT('Ctrl Pts',(13.8712239129569,-13.5985230868316,-333.540389757162)) ;
#30659 = CARTESIAN_POINT('Ctrl Pts',(13.8814001372614,-13.5881346481681,-333.54020830311)) ;
#30660 = CARTESIAN_POINT('Ctrl Pts',(13.8862450259025,-13.5831834290828,-333.540121888645)) ;
#30661 = CARTESIAN_POINT('Ctrl Pts',(13.8955331773685,-13.5736812681853,-333.539956176413)) ;
#30662 = CARTESIAN_POINT('Ctrl Pts',(13.8999768555668,-13.5691307337038,-333.539876875067)) ;
#30663 = CARTESIAN_POINT('Ctrl Pts',(13.9085334324928,-13.5603597844987,-333.539724135804)) ;
#30664 = CARTESIAN_POINT('Ctrl Pts',(13.9126466472052,-13.5561396790471,-333.539650695158)) ;
#30665 = CARTESIAN_POINT('Ctrl Pts',(13.9206014394819,-13.5479707304881,-333.539508629722)) ;
#30666 = CARTESIAN_POINT('Ctrl Pts',(13.9244432587766,-13.5440221235859,-333.539440002842)) ;
#30667 = CARTESIAN_POINT('Ctrl Pts',(13.9319053410319,-13.5363460937028,-333.539306676764)) ;
#30668 = CARTESIAN_POINT('Ctrl Pts',(13.9355257892056,-13.5326188514406,-333.539241975963)) ;
#30669 = CARTESIAN_POINT('Ctrl Pts',(13.9425882455676,-13.5253422307925,-333.539115736432)) ;
#30670 = CARTESIAN_POINT('Ctrl Pts',(13.9460303950204,-13.5217929900834,-333.539054196478)) ;
#30671 = CARTESIAN_POINT('Ctrl Pts',(13.9527741011949,-13.5148341612684,-333.53893360574)) ;
#30672 = CARTESIAN_POINT('Ctrl Pts',(13.9560757641447,-13.5114246765845,-333.538874554035)) ;
#30673 = CARTESIAN_POINT('Ctrl Pts',(13.9625724828677,-13.5047108738972,-333.538758334752)) ;
#30674 = CARTESIAN_POINT('Ctrl Pts',(13.9657676160324,-13.501406631232,-333.538701166502)) ;
#30675 = CARTESIAN_POINT('Ctrl Pts',(13.9720826110679,-13.4948713473917,-333.538588155489)) ;
#30676 = CARTESIAN_POINT('Ctrl Pts',(13.9752025257003,-13.4916403576,-333.538532312267)) ;
#30677 = CARTESIAN_POINT('Ctrl Pts',(13.9813968663759,-13.4852210320213,-333.538421419588)) ;
#30678 = CARTESIAN_POINT('Ctrl Pts',(13.984471323107,-13.4820327262166,-333.538366369865)) ;
#30679 = CARTESIAN_POINT('Ctrl Pts',(13.9906040330922,-13.4756685633107,-333.538256540576)) ;
#30680 = CARTESIAN_POINT('Ctrl Pts',(13.9936622961041,-13.4724927159592,-333.538201760927)) ;
#30681 = CARTESIAN_POINT('Ctrl Pts',(13.9997924986543,-13.4661224795987,-333.538091936751)) ;
#30682 = CARTESIAN_POINT('Ctrl Pts',(14.0028644267675,-13.4629280799721,-333.538036892327)) ;
#30683 = CARTESIAN_POINT('Ctrl Pts',(14.0090536557543,-13.4564876890003,-333.537925970241)) ;
#30684 = CARTESIAN_POINT('Ctrl Pts',(14.0121709212934,-13.4532416660988,-333.537870092898)) ;
#30685 = CARTESIAN_POINT('Ctrl Pts',(14.0969610276311,-13.3648878995049,-333.536349938729)) ;
#30686 = CARTESIAN_POINT('Ctrl Pts',(14.1778581501325,-13.2790390125067,-333.534892481846)) ;
#30687 = CARTESIAN_POINT('Ctrl Pts',(14.3437921448222,-13.099703096016,-333.531887900899)) ;
#30688 = CARTESIAN_POINT('Ctrl Pts',(14.4287088015307,-13.0061122810377,-333.53034187031)) ;
#30689 = CARTESIAN_POINT('Ctrl Pts',(14.6156678756097,-12.7959709185598,-333.526918072474)) ;
#30690 = CARTESIAN_POINT('Ctrl Pts',(14.7172416424833,-12.67901485605,-333.525044355498)) ;
#30691 = CARTESIAN_POINT('Ctrl Pts',(15.3832693379302,-11.8933357322318,-333.512657361094)) ;
#30692 = CARTESIAN_POINT('Ctrl Pts',(15.9033764841782,-11.1883431515826,-333.502545468447)) ;
#30693 = CARTESIAN_POINT('Ctrl Pts',(16.4948363777841,-10.2616420118615,-333.489644641934)) ;
#30694 = CARTESIAN_POINT('Ctrl Pts',(16.6122131415321,-10.0705162834489,-333.487000214077)) ;
#30695 = CARTESIAN_POINT('Ctrl Pts',(16.8049719276461,-9.74410123903481,-333.482481987595)) ;
#30696 = CARTESIAN_POINT('Ctrl Pts',(16.882093585185,-9.60986506154454,-333.480623304129)) ;
#30697 = CARTESIAN_POINT('Ctrl Pts',(16.9950777308637,-9.40764907160485,-333.477812999067)) ;
#30698 = CARTESIAN_POINT('Ctrl Pts',(17.0321548694654,-9.34035484420517,-333.47687607463)) ;
#30699 = CARTESIAN_POINT('Ctrl Pts',(17.1005348416455,-9.21448553897886,-333.475118932505)) ;
#30700 = CARTESIAN_POINT('Ctrl Pts',(17.1319383526833,-9.15596657166212,-333.474299997191)) ;
#30701 = CARTESIAN_POINT('Ctrl Pts',(17.2030771676023,-9.02175531729164,-333.472417988342)) ;
#30702 = CARTESIAN_POINT('Ctrl Pts',(17.242614147293,-8.94595944447764,-333.471352434968)) ;
#30703 = CARTESIAN_POINT('Ctrl Pts',(17.4089068035397,-8.6219637138026,-333.466790218713)) ;
#30704 = CARTESIAN_POINT('Ctrl Pts',(17.5308133724107,-8.37131270202806,-333.463242772097)) ;
#30705 = CARTESIAN_POINT('Ctrl Pts',(17.6766582056498,-8.05427338104472,-333.458769373237)) ;
#30706 = CARTESIAN_POINT('Ctrl Pts',(17.7056851451043,-7.99026148217449,-333.457866826918)) ;
#30707 = CARTESIAN_POINT('Ctrl Pts',(17.9065774092179,-7.54077188782342,-333.451536561651)) ;
#30708 = CARTESIAN_POINT('Ctrl Pts',(18.0661870262132,-7.14993998904863,-333.44607308749)) ;
#30709 = CARTESIAN_POINT('Ctrl Pts',(18.2909961221862,-6.54373610484607,-333.437762920931)) ;
#30710 = CARTESIAN_POINT('Ctrl Pts',(18.3653988659806,-6.3319148780479,-333.434888503684)) ;
#30711 = CARTESIAN_POINT('Ctrl Pts',(18.4791414337213,-5.98920826684635,-333.430294562081)) ;
#30712 = CARTESIAN_POINT('Ctrl Pts',(18.5208007287333,-5.8591146267667,-333.428563567169)) ;
#30713 = CARTESIAN_POINT('Ctrl Pts',(18.6221282529397,-5.53080557296592,-333.424229583725)) ;
#30714 = CARTESIAN_POINT('Ctrl Pts',(18.6800068279149,-5.33205552028042,-333.421637317276)) ;
#30715 = CARTESIAN_POINT('Ctrl Pts',(18.7694276428676,-5.00564565263722,-333.417432985661)) ;
#30716 = CARTESIAN_POINT('Ctrl Pts',(18.8028696943002,-4.87852372702762,-333.415808554372)) ;
#30717 = CARTESIAN_POINT('Ctrl Pts',(18.8660930589882,-4.62788276621338,-333.412630856239)) ;
#30718 = CARTESIAN_POINT('Ctrl Pts',(18.895957867395,-4.50439147180606,-333.411077101227)) ;
#30719 = CARTESIAN_POINT('Ctrl Pts',(18.9672562780315,-4.19637667499849,-333.407230124622)) ;
#30720 = CARTESIAN_POINT('Ctrl Pts',(19.0072107745175,-4.01152422887809,-333.404946720168)) ;
#30721 = CARTESIAN_POINT('Ctrl Pts',(19.1428539485452,-3.33636178791636,-333.396688758531)) ;
#30722 = CARTESIAN_POINT('Ctrl Pts',(19.2223194384042,-2.84299208022768,-333.390816015683)) ;
#30723 = CARTESIAN_POINT('Ctrl Pts',(19.3470593237684,-1.8181911737485,-333.378745123188)) ;
#30724 = CARTESIAN_POINT('Ctrl Pts',(19.3896502954353,-1.2868498898905,-333.372556822471)) ;
#30725 = CARTESIAN_POINT('Ctrl Pts',(19.4170699836498,-0.58138533240423,-333.364163615815)) ;
#30726 = CARTESIAN_POINT('Ctrl Pts',(19.4214814729503,-0.408255901899993,
-333.362089097568)) ;
#30727 = CARTESIAN_POINT('Ctrl Pts',(19.4245452607997,-0.155121042115437,
-333.35902157745)) ;
#30728 = CARTESIAN_POINT('Ctrl Pts',(19.4250192841486,-0.0751459607953256,
-333.35804740894)) ;
#30729 = CARTESIAN_POINT('Ctrl Pts',(19.42498291383,0.0711353845930604,-333.35625470279)) ;
#30730 = CARTESIAN_POINT('Ctrl Pts',(19.4246269351351,0.13744032643945,-333.355437890318)) ;
#30731 = CARTESIAN_POINT('Ctrl Pts',(19.4229132651343,0.30081453407795,-333.353415409582)) ;
#30732 = CARTESIAN_POINT('Ctrl Pts',(19.4211673764434,0.397877856347019,-333.352205381687)) ;
#30733 = CARTESIAN_POINT('Ctrl Pts',(19.4110232288516,0.79589075797672,-333.347214618815)) ;
#30734 = CARTESIAN_POINT('Ctrl Pts',(19.3963565899525,1.09663818462654,-333.34337610559)) ;
#30735 = CARTESIAN_POINT('Ctrl Pts',(19.3649781136623,1.53184404487331,-333.337775533208)) ;
#30736 = CARTESIAN_POINT('Ctrl Pts',(19.3538411250613,1.66666049391692,-333.336034092772)) ;
#30737 = CARTESIAN_POINT('Ctrl Pts',(19.2940586134025,2.30855218855928,-333.327724472805)) ;
#30738 = CARTESIAN_POINT('Ctrl Pts',(19.2268873405422,2.81370144019565,-333.321136516688)) ;
#30739 = CARTESIAN_POINT('Ctrl Pts',(19.1020428751769,3.53438463478772,-333.311808267238)) ;
#30740 = CARTESIAN_POINT('Ctrl Pts',(19.0603993295577,3.75247843096919,-333.308993793443)) ;
#30741 = CARTESIAN_POINT('Ctrl Pts',(18.9767904615134,4.15295719201776,-333.303847912289)) ;
#30742 = CARTESIAN_POINT('Ctrl Pts',(18.9359104768492,4.33554197612063,-333.301510378501)) ;
#30743 = CARTESIAN_POINT('Ctrl Pts',(18.8626337201872,4.64198831378599,-333.297602588198)) ;
#30744 = CARTESIAN_POINT('Ctrl Pts',(18.8316386548188,4.76617162854907,-333.296023293535)) ;
#30745 = CARTESIAN_POINT('Ctrl Pts',(18.7661338509389,5.01800030823523,-333.292829023471)) ;
#30746 = CARTESIAN_POINT('Ctrl Pts',(18.7315435367731,5.14561790168791,-333.291214678661)) ;
#30747 = CARTESIAN_POINT('Ctrl Pts',(18.6382919252303,5.47625357992298,-333.287042181389)) ;
#30748 = CARTESIAN_POINT('Ctrl Pts',(18.5776158972644,5.67868531791672,-333.284497542635)) ;
#30749 = CARTESIAN_POINT('Ctrl Pts',(18.4245379764094,6.16065623749146,-333.278453034908)) ;
#30750 = CARTESIAN_POINT('Ctrl Pts',(18.3290603761536,6.43916384565315,-333.274971985635)) ;
#30751 = CARTESIAN_POINT('Ctrl Pts',(18.1470893756267,6.93307949700225,-333.268786554412)) ;
#30752 = CARTESIAN_POINT('Ctrl Pts',(18.0629953022918,7.14931079914399,-333.266074255217)) ;
#30753 = CARTESIAN_POINT('Ctrl Pts',(17.8248729960615,7.73055324125156,-333.258737004916)) ;
#30754 = CARTESIAN_POINT('Ctrl Pts',(17.663519593666,8.09244249423578,-333.254119711503)) ;
#30755 = CARTESIAN_POINT('Ctrl Pts',(17.4441586451935,8.54655825261737,-333.24815564068)) ;
#30756 = CARTESIAN_POINT('Ctrl Pts',(17.3962896764393,8.6435776311753,-333.246871197402)) ;
#30757 = CARTESIAN_POINT('Ctrl Pts',(17.2824082550688,8.86961051525614,-333.243849920018)) ;
#30758 = CARTESIAN_POINT('Ctrl Pts',(17.2157575925383,8.998295182807,-333.24210766899)) ;
#30759 = CARTESIAN_POINT('Ctrl Pts',(17.1124238202571,9.19245370898263,-333.239437189531)) ;
#30760 = CARTESIAN_POINT('Ctrl Pts',(17.0767909004466,9.25848079978737,-333.238521615424)) ;
#30761 = CARTESIAN_POINT('Ctrl Pts',(17.008547787013,9.38319961716122,-333.236776611772)) ;
#30762 = CARTESIAN_POINT('Ctrl Pts',(16.9760141219689,9.44193186655502,-333.235948141072)) ;
#30763 = CARTESIAN_POINT('Ctrl Pts',(16.890721527033,9.59404263872836,-333.233786034316)) ;
#30764 = CARTESIAN_POINT('Ctrl Pts',(16.8374925734254,9.68715498223381,-333.232446387797)) ;
#30765 = CARTESIAN_POINT('Ctrl Pts',(16.4692086308292,10.3191799888549,-333.223255042643)) ;
#30766 = CARTESIAN_POINT('Ctrl Pts',(16.1291054287192,10.8430745638096,-333.215158950642)) ;
#30767 = CARTESIAN_POINT('Ctrl Pts',(15.4879929477942,11.7335606980522,-333.201013931531)) ;
#30768 = CARTESIAN_POINT('Ctrl Pts',(15.1976861145089,12.107217305967,-333.194946031525)) ;
#30769 = CARTESIAN_POINT('Ctrl Pts',(14.7583180814734,12.6319976359357,-333.186307815645)) ;
#30770 = CARTESIAN_POINT('Ctrl Pts',(14.6199694614354,12.7918649944131,-333.18365902057)) ;
#30771 = CARTESIAN_POINT('Ctrl Pts',(14.3908860959917,13.0480078332665,-333.179388674162)) ;
#30772 = CARTESIAN_POINT('Ctrl Pts',(14.3017291188879,13.1456705919147,-333.177753975643)) ;
#30773 = CARTESIAN_POINT('Ctrl Pts',(14.1253409408252,13.3349680079283,-333.174572372322)) ;
#30774 = CARTESIAN_POINT('Ctrl Pts',(14.0381979334757,13.4266759585693,-333.173024806631)) ;
#30775 = CARTESIAN_POINT('Ctrl Pts',(13.8419523826118,13.6292025028445,-333.169592290601)) ;
#30776 = CARTESIAN_POINT('Ctrl Pts',(13.7324023107616,13.7395754478356,-333.167711465801)) ;
#30777 = CARTESIAN_POINT('Ctrl Pts',(13.2333692518717,14.230425622525,-333.159294352496)) ;
#30778 = CARTESIAN_POINT('Ctrl Pts',(12.8293183219051,14.5957414397109,-333.152892147122)) ;
#30779 = CARTESIAN_POINT('Ctrl Pts',(11.9950124408525,15.2886210585865,-333.140213387796)) ;
#30780 = CARTESIAN_POINT('Ctrl Pts',(11.5653628260783,15.6161658991078,-333.133941007662)) ;
#30781 = CARTESIAN_POINT('Ctrl Pts',(10.9887083838154,16.018913677342,-333.125567869635)) ;
#30782 = CARTESIAN_POINT('Ctrl Pts',(10.8536155118191,16.110752233322,-333.123608789363)) ;
#30783 = CARTESIAN_POINT('Ctrl Pts',(10.6520543157837,16.2440912011431,-333.120678513776)) ;
#30784 = CARTESIAN_POINT('Ctrl Pts',(10.5864672598366,16.2869110341224,-333.119723883043)) ;
#30785 = CARTESIAN_POINT('Ctrl Pts',(10.4645500408342,16.3654595645565,-333.117945661744)) ;
#30786 = CARTESIAN_POINT('Ctrl Pts',(10.40829148202,16.4012969824107,-333.117123515636)) ;
#30787 = CARTESIAN_POINT('Ctrl Pts',(10.2670895262562,16.4902253317346,-333.115056802837)) ;
#30788 = CARTESIAN_POINT('Ctrl Pts',(10.1819179910304,16.5429503056695,-333.113807403652)) ;
#30789 = CARTESIAN_POINT('Ctrl Pts',(9.79143710092742,16.7805173730125,-333.10807359189)) ;
#30790 = CARTESIAN_POINT('Ctrl Pts',(9.48147752154305,16.9575819899353,-333.103507420401)) ;
#30791 = CARTESIAN_POINT('Ctrl Pts',(9.05011184033831,17.1884735491353,-333.097212351778)) ;
#30792 = CARTESIAN_POINT('Ctrl Pts',(8.93277116644243,17.2497462748253,-333.095505690404)) ;
#30793 = CARTESIAN_POINT('Ctrl Pts',(8.39656519742377,17.5228026665727,-333.087743567385)) ;
#30794 = CARTESIAN_POINT('Ctrl Pts',(7.97073415744361,17.7205620325568,-333.081684402296)) ;
#30795 = CARTESIAN_POINT('Ctrl Pts',(7.34124518317848,17.9856163017766,-333.072982606548)) ;
#30796 = CARTESIAN_POINT('Ctrl Pts',(7.14297669632664,18.0652749415487,-333.070276864771)) ;
#30797 = CARTESIAN_POINT('Ctrl Pts',(6.77343519647141,18.2067112280152,-333.065303854228)) ;
#30798 = CARTESIAN_POINT('Ctrl Pts',(6.60252975588462,18.2693831058139,-333.063031185004)) ;
#30799 = CARTESIAN_POINT('Ctrl Pts',(6.31076977857024,18.371744118536,-333.05919829711)) ;
#30800 = CARTESIAN_POINT('Ctrl Pts',(6.19036035022939,18.412665096058,-333.057629841057)) ;
#30801 = CARTESIAN_POINT('Ctrl Pts',(5.95798393448758,18.4891007902471,-333.054628162201)) ;
#30802 = CARTESIAN_POINT('Ctrl Pts',(5.84607953364291,18.5247881154073,-333.053193821013)) ;
#30803 = CARTESIAN_POINT('Ctrl Pts',(5.54137466680489,18.6189252659338,-333.049317416442)) ;
#30804 = CARTESIAN_POINT('Ctrl Pts',(5.34797741724409,18.6753942121836,-333.046888667499)) ;
#30805 = CARTESIAN_POINT('Ctrl Pts',(4.84618034748603,18.8134769387792,-333.040659276442)) ;
#30806 = CARTESIAN_POINT('Ctrl Pts',(4.53658575028656,18.8905206043487,-333.03688640497)) ;
#30807 = CARTESIAN_POINT('Ctrl Pts',(3.67056456854031,19.0835143101628,-333.026462374713)) ;
#30808 = CARTESIAN_POINT('Ctrl Pts',(3.11073880895119,19.1827230887492,-333.019877242723)) ;
#30809 = CARTESIAN_POINT('Ctrl Pts',(2.41727197784791,19.2744557206303,-333.011635316856)) ;
#30810 = CARTESIAN_POINT('Ctrl Pts',(2.28700117345289,19.2903466201257,-333.010082926058)) ;
#30811 = CARTESIAN_POINT('Ctrl Pts',(2.07729245154048,19.3137734778656,-333.007571641244)) ;
#30812 = CARTESIAN_POINT('Ctrl Pts',(1.99795165563897,19.3221421962073,-333.00661870617)) ;
#30813 = CARTESIAN_POINT('Ctrl Pts',(1.80226361975563,19.3415648101887,-333.004259342461)) ;
#30814 = CARTESIAN_POINT('Ctrl Pts',(1.68586394131653,19.3520579312369,-333.002848097146)) ;
#30815 = CARTESIAN_POINT('Ctrl Pts',(1.50003123457104,19.3671208934029,-333.000578089761)) ;
#30816 = CARTESIAN_POINT('Ctrl Pts',(1.43065596303526,19.3723692128409,-332.999726879193)) ;
#30817 = CARTESIAN_POINT('Ctrl Pts',(1.29826167994031,19.3816699287012,-332.998094109423)) ;
#30818 = CARTESIAN_POINT('Ctrl Pts',(1.23524819987431,19.3857879511827,-332.997313438438)) ;
#30819 = CARTESIAN_POINT('Ctrl Pts',(1.05330017153295,19.3967877846189,-332.995050180763)) ;
#30820 = CARTESIAN_POINT('Ctrl Pts',(0.934321034145954,19.4028828207357,-332.993558974389)) ;
#30821 = CARTESIAN_POINT('Ctrl Pts',(0.344803090013214,19.4276475084637,-332.986127106287)) ;
#30822 = CARTESIAN_POINT('Ctrl Pts',(-0.126249964269435,19.4302968777024,
-332.980056226613)) ;
#30823 = CARTESIAN_POINT('Ctrl Pts',(-0.613677451346516,19.4153111143555,
-332.973764851327)) ;
#30824 = CARTESIAN_POINT('Ctrl Pts',(-0.630422417915108,19.4147746125597,
-332.973548702031)) ;
#30825 = CARTESIAN_POINT('Ctrl Pts',(-1.09323222780011,19.3993469962056,-332.967574260517)) ;
#30826 = CARTESIAN_POINT('Ctrl Pts',(-1.53865354229193,19.3691085770876,-332.961819045718)) ;
#30827 = CARTESIAN_POINT('Ctrl Pts',(-2.12266817744188,19.3091874467497,-332.954344620164)) ;
#30828 = CARTESIAN_POINT('Ctrl Pts',(-2.26253874258408,19.2932982804835,-332.95255960314)) ;
#30829 = CARTESIAN_POINT('Ctrl Pts',(-2.61193680723005,19.2497551538605,-332.948115738213)) ;
#30830 = CARTESIAN_POINT('Ctrl Pts',(-2.82120903691092,19.2201994567889,-332.945467837388)) ;
#30831 = CARTESIAN_POINT('Ctrl Pts',(-3.16056135704347,19.1666105411561,-332.941198535374)) ;
#30832 = CARTESIAN_POINT('Ctrl Pts',(-3.2909513116916,19.144653228733,-332.93956399948)) ;
#30833 = CARTESIAN_POINT('Ctrl Pts',(-3.5456423729203,19.0990850743006,-332.93638246423)) ;
#30834 = CARTESIAN_POINT('Ctrl Pts',(-3.66995717124761,19.0755876691145,-332.934834806657)) ;
#30835 = CARTESIAN_POINT('Ctrl Pts',(-3.94657833863177,19.0204978175994,-332.931401770917)) ;
#30836 = CARTESIAN_POINT('Ctrl Pts',(-4.09875276839955,18.9882870117658,-332.929520522777)) ;
#30837 = CARTESIAN_POINT('Ctrl Pts',(-4.78169548142166,18.8351359186851,-332.921104345019)) ;
#30838 = CARTESIAN_POINT('Ctrl Pts',(-5.30762564895109,18.6937440965461,-332.914703423215)) ;
#30839 = CARTESIAN_POINT('Ctrl Pts',(-6.34208945927371,18.3684557387305,-332.902025849827)) ;
#30840 = CARTESIAN_POINT('Ctrl Pts',(-6.85027615390731,18.1850482239758,-332.895753390762)) ;
#30841 = CARTESIAN_POINT('Ctrl Pts',(-7.50136367455804,17.9188964974645,-332.887380125592)) ;
#30842 = CARTESIAN_POINT('Ctrl Pts',(-7.65178360874278,17.8551817723879,-332.885420997911)) ;
#30843 = CARTESIAN_POINT('Ctrl Pts',(-7.87311477003433,17.7581199462056,-332.882490665805)) ;
#30844 = CARTESIAN_POINT('Ctrl Pts',(-7.94465681822003,17.7262288213319,-332.881536026868)) ;
#30845 = CARTESIAN_POINT('Ctrl Pts',(-8.076762594974,17.6663799425577,-332.879757799825)) ;
#30846 = CARTESIAN_POINT('Ctrl Pts',(-8.13737885336472,17.6385413130128,-332.878935656299)) ;
#30847 = CARTESIAN_POINT('Ctrl Pts',(-8.28866081048154,17.5681177284296,-332.876868963693)) ;
#30848 = CARTESIAN_POINT('Ctrl Pts',(-8.37914272793705,17.5251426714995,-332.875619582335)) ;
#30849 = CARTESIAN_POINT('Ctrl Pts',(-8.79015125641648,17.3260204187595,-332.869890381904)) ;
#30850 = CARTESIAN_POINT('Ctrl Pts',(-9.10667336779391,17.1617668660758,-332.865328981874)) ;
#30851 = CARTESIAN_POINT('Ctrl Pts',(-9.49909402530684,16.944212304047,-332.859556101753)) ;
#30852 = CARTESIAN_POINT('Ctrl Pts',(-9.57937449631672,16.8989556529289,-332.858368672963)) ;
#30853 = CARTESIAN_POINT('Ctrl Pts',(-9.69243588238736,16.8341547964933,-332.856688416188)) ;
#30854 = CARTESIAN_POINT('Ctrl Pts',(-9.72548593257093,16.815082646887,-332.856196273777)) ;
#30855 = CARTESIAN_POINT('Ctrl Pts',(-10.1656923120821,16.5593213256834,-332.849628992767)) ;
#30856 = CARTESIAN_POINT('Ctrl Pts',(-10.5641669132355,16.3079980912009,-332.843548740347)) ;
#30857 = CARTESIAN_POINT('Ctrl Pts',(-11.1298541913737,15.9217703062943,-332.834821740233)) ;
#30858 = CARTESIAN_POINT('Ctrl Pts',(-11.3045891844606,15.7981862118039,-332.832111456035)) ;
#30859 = CARTESIAN_POINT('Ctrl Pts',(-11.6242732331865,15.5640646243421,-332.827131203072)) ;
#30860 = CARTESIAN_POINT('Ctrl Pts',(-11.769777477771,15.4543254171097,-332.824855804296)) ;
#30861 = CARTESIAN_POINT('Ctrl Pts',(-12.0141859922302,15.2645386657135,-332.821019772923)) ;
#30862 = CARTESIAN_POINT('Ctrl Pts',(-12.1138871596305,15.1855373190068,-332.819450869595)) ;
#30863 = CARTESIAN_POINT('Ctrl Pts',(-12.3166206303322,15.021627870495,-332.816251814469)) ;
#30864 = CARTESIAN_POINT('Ctrl Pts',(-12.4195680638307,14.9366253483159,-332.814622564063)) ;
#30865 = CARTESIAN_POINT('Ctrl Pts',(-12.6886292837425,14.709759595904,-332.810350125)) ;
#30866 = CARTESIAN_POINT('Ctrl Pts',(-12.8532405659061,14.5661438839606,-332.807721776794)) ;
#30867 = CARTESIAN_POINT('Ctrl Pts',(-13.2211306525875,14.2340837596221,-332.801803677417)) ;
#30868 = CARTESIAN_POINT('Ctrl Pts',(-13.4228689011077,14.0440032395445,-332.798526908168)) ;
#30869 = CARTESIAN_POINT('Ctrl Pts',(-14.0308187103431,13.4461144793822,-332.788505310189)) ;
#30870 = CARTESIAN_POINT('Ctrl Pts',(-14.4230275582335,13.0245208219857,-332.781837196636)) ;
#30871 = CARTESIAN_POINT('Ctrl Pts',(-14.8814798855379,12.4855761398134,-332.773501312507)) ;
#30872 = CARTESIAN_POINT('Ctrl Pts',(-14.9659948553096,12.3841452295847,-332.77193975059)) ;
#30873 = CARTESIAN_POINT('Ctrl Pts',(-15.1001252726387,12.2197897119688,-332.769415276397)) ;
#30874 = CARTESIAN_POINT('Ctrl Pts',(-15.1503968620899,12.1574059223313,-332.768458391324)) ;
#30875 = CARTESIAN_POINT('Ctrl Pts',(-15.2732690360566,12.002983772505,-332.766090895236)) ;
#30876 = CARTESIAN_POINT('Ctrl Pts',(-15.3454251302086,11.9105958710813,-332.764675456101)) ;
#30877 = CARTESIAN_POINT('Ctrl Pts',(-15.459108180474,11.7622892844271,-332.762400392098)) ;
#30878 = CARTESIAN_POINT('Ctrl Pts',(-15.5011783715631,11.7067905096707,-332.761548377623)) ;
#30879 = CARTESIAN_POINT('Ctrl Pts',(-15.5807867785326,11.6005899825796,-332.75991560678)) ;
#30880 = CARTESIAN_POINT('Ctrl Pts',(-15.6183782225291,11.5499292754922,-332.75913575286)) ;
#30881 = CARTESIAN_POINT('Ctrl Pts',(-15.7260335864455,11.4033591557038,-332.756877824472)) ;
#30882 = CARTESIAN_POINT('Ctrl Pts',(-15.7954654458562,11.3069891519533,-332.75539119039)) ;
#30883 = CARTESIAN_POINT('Ctrl Pts',(-16.1173902631968,10.8514116843935,-332.748365342679)) ;
#30884 = CARTESIAN_POINT('Ctrl Pts',(-16.3585409384819,10.4843474655009,-332.742713310106)) ;
#30885 = CARTESIAN_POINT('Ctrl Pts',(-16.8360655268671,9.70084898028878,-332.730878625599)) ;
#30886 = CARTESIAN_POINT('Ctrl Pts',(-17.0699045422516,9.28320708008778,-332.724698969283)) ;
#30887 = CARTESIAN_POINT('Ctrl Pts',(-17.354916199073,8.72691190692555,-332.716733552557)) ;
#30888 = CARTESIAN_POINT('Ctrl Pts',(-17.4202701927891,8.59571370979229,-332.714873279382)) ;
#30889 = CARTESIAN_POINT('Ctrl Pts',(-17.5788073100672,8.26821449266512,-332.71027760955)) ;
#30890 = CARTESIAN_POINT('Ctrl Pts',(-17.6701934479759,8.0710656725557,-332.707553453045)) ;
#30891 = CARTESIAN_POINT('Ctrl Pts',(-17.8122731492108,7.75056884177899,-332.703195100815)) ;
#30892 = CARTESIAN_POINT('Ctrl Pts',(-17.8650376699087,7.62815975342177,-332.701546691436)) ;
#30893 = CARTESIAN_POINT('Ctrl Pts',(-17.9651731074605,7.38911532081692,-332.698358711702)) ;
#30894 = CARTESIAN_POINT('Ctrl Pts',(-18.0126783998465,7.27254335959728,-332.696818261432)) ;
#30895 = CARTESIAN_POINT('Ctrl Pts',(-18.1260197636965,6.98649319462234,-332.693071763595)) ;
#30896 = CARTESIAN_POINT('Ctrl Pts',(-18.1906159799789,6.81653651325428,-332.690874347761)) ;
#30897 = CARTESIAN_POINT('Ctrl Pts',(-18.4917111519331,5.98956016241263,-332.680308407736)) ;
#30898 = CARTESIAN_POINT('Ctrl Pts',(-18.69505245603,5.32101745546163,-332.672169990785)) ;
#30899 = CARTESIAN_POINT('Ctrl Pts',(-18.965211654889,4.22350506080342,-332.658963549937)) ;
#30900 = CARTESIAN_POINT('Ctrl Pts',(-19.0544461727274,3.80070091297439,-332.653906380235)) ;
#30901 = CARTESIAN_POINT('Ctrl Pts',(-19.1507426307205,3.25493685063842,-332.647264359849)) ;
#30902 = CARTESIAN_POINT('Ctrl Pts',(-19.1708395548099,3.13440072529529,-332.645790136637)) ;
#30903 = CARTESIAN_POINT('Ctrl Pts',(-19.2007539260998,2.94391927657953,-332.64344396133)) ;
#30904 = CARTESIAN_POINT('Ctrl Pts',(-19.2113295496236,2.87409619899446,-332.642580457603)) ;
#30905 = CARTESIAN_POINT('Ctrl Pts',(-19.2305162936662,2.74258053620003,-332.640946234512)) ;
#30906 = CARTESIAN_POINT('Ctrl Pts',(-19.239211882411,2.6809011640435,-332.640176605136)) ;
#30907 = CARTESIAN_POINT('Ctrl Pts',(-19.2630127144438,2.50599567505363,-332.637986163198)) ;
#30908 = CARTESIAN_POINT('Ctrl Pts',(-19.2774160923569,2.39267672415011,-332.636557541114)) ;
#30909 = CARTESIAN_POINT('Ctrl Pts',(-19.3556851459913,1.73022966808652,-332.628163658032)) ;
#30910 = CARTESIAN_POINT('Ctrl Pts',(-19.3970848131271,1.17870348039104,-332.621013138847)) ;
#30911 = CARTESIAN_POINT('Ctrl Pts',(-19.4189239420216,0.501558483573225,
-332.612273500629)) ;
#30912 = CARTESIAN_POINT('Ctrl Pts',(-19.4217430305178,0.376915967196436,
-332.61066603836)) ;
#30913 = CARTESIAN_POINT('Ctrl Pts',(-19.4277516205274,-0.0857390490145371,
-332.604709669678)) ;
#30914 = CARTESIAN_POINT('Ctrl Pts',(-19.423318112687,-0.423790456247844,
-332.600378949753)) ;
#30915 = CARTESIAN_POINT('Ctrl Pts',(-19.4002828798608,-1.0108996640172,-332.592930403635)) ;
#30916 = CARTESIAN_POINT('Ctrl Pts',(-19.3856959856753,-1.2600339100366,-332.589792231301)) ;
#30917 = CARTESIAN_POINT('Ctrl Pts',(-19.3555143204028,-1.64742822420008,
-332.584952291665)) ;
#30918 = CARTESIAN_POINT('Ctrl Pts',(-19.3432274914321,-1.78591843074365,
-332.583229919181)) ;
#30919 = CARTESIAN_POINT('Ctrl Pts',(-19.317062796762,-2.04874569984758,-332.579975981516)) ;
#30920 = CARTESIAN_POINT('Ctrl Pts',(-19.3034684240235,-2.17310397516719,
-332.578442664486)) ;
#30921 = CARTESIAN_POINT('Ctrl Pts',(-19.269232337167,-2.46055545674489,-332.574912190885)) ;
#30922 = CARTESIAN_POINT('Ctrl Pts',(-19.247719616884,-2.62353533827136,-332.57292078095)) ;
#30923 = CARTESIAN_POINT('Ctrl Pts',(-19.158438627005,-3.23954867857116,-332.565426998394)) ;
#30924 = CARTESIAN_POINT('Ctrl Pts',(-19.0767220977745,-3.69040940486956,
-332.560013957573)) ;
#30925 = CARTESIAN_POINT('Ctrl Pts',(-18.9649286932409,-4.20316046581644,
-332.55386231649)) ;
#30926 = CARTESIAN_POINT('Ctrl Pts',(-18.9503772606234,-4.2682877039268,-332.553080961274)) ;
#30927 = CARTESIAN_POINT('Ctrl Pts',(-18.8307665069412,-4.7909535890797,-332.546807934775)) ;
#30928 = CARTESIAN_POINT('Ctrl Pts',(-18.7094882783897,-5.24462112942083,
-332.541352269244)) ;
#30929 = CARTESIAN_POINT('Ctrl Pts',(-18.5230373785132,-5.85281963444294,
-332.533843442027)) ;
#30930 = CARTESIAN_POINT('Ctrl Pts',(-18.4721306018671,-6.01155573116635,
-332.531864900236)) ;
#30931 = CARTESIAN_POINT('Ctrl Pts',(-18.3792129446722,-6.28895833144694,
-332.528361140513)) ;
#30932 = CARTESIAN_POINT('Ctrl Pts',(-18.3380798814535,-6.4079085160051,-332.526843669243)) ;
#30933 = CARTESIAN_POINT('Ctrl Pts',(-18.2718215176671,-6.59365257124561,
-332.524444998102)) ;
#30934 = CARTESIAN_POINT('Ctrl Pts',(-18.2474791858175,-6.66072211932476,
-332.523572879237)) ;
#30935 = CARTESIAN_POINT('Ctrl Pts',(-18.2013629439761,-6.78563420988526,
-332.521936181542)) ;
#30936 = CARTESIAN_POINT('Ctrl Pts',(-18.1796814251312,-6.84350991195361,
-332.521172819736)) ;
#30937 = CARTESIAN_POINT('Ctrl Pts',(-18.1181597730131,-7.00537742165052,
-332.519024754052)) ;
#30938 = CARTESIAN_POINT('Ctrl Pts',(-18.077701063549,-7.10913149298922,-332.517632702517)) ;
#30939 = CARTESIAN_POINT('Ctrl Pts',(-17.7803149815643,-7.85280380534435,
-332.507560122073)) ;
#30940 = CARTESIAN_POINT('Ctrl Pts',(-17.4903657112314,-8.47898793077572,
-332.498590331982)) ;
#30941 = CARTESIAN_POINT('Ctrl Pts',(-17.0112787635502,-9.3839673760511,-332.485410776379)) ;
#30942 = CARTESIAN_POINT('Ctrl Pts',(-16.8472160760208,-9.67542040438931,
-332.481127569767)) ;
#30943 = CARTESIAN_POINT('Ctrl Pts',(-16.6156281858173,-10.0630636209073,
-332.47540424251)) ;
#30944 = CARTESIAN_POINT('Ctrl Pts',(-16.5546361838925,-10.163088620157,-332.473924858382)) ;
#30945 = CARTESIAN_POINT('Ctrl Pts',(-16.3944887207595,-10.4204583249398,
-332.470112734989)) ;
#30946 = CARTESIAN_POINT('Ctrl Pts',(-16.2939717182453,-10.5769418034851,
-332.467789520545)) ;
#30947 = CARTESIAN_POINT('Ctrl Pts',(-16.1206128116088,-10.8384870647885,
-332.463898298816)) ;
#30948 = CARTESIAN_POINT('Ctrl Pts',(-16.0489528599848,-10.9443168550778,
-332.462321431671)) ;
#30949 = CARTESIAN_POINT('Ctrl Pts',(-15.9008859070986,-11.1584052570647,
-332.459126296506)) ;
#30950 = CARTESIAN_POINT('Ctrl Pts',(-15.8244051026833,-11.2666047997321,
-332.457508719485)) ;
#30951 = CARTESIAN_POINT('Ctrl Pts',(-15.6221841714602,-11.5465708177693,
-332.453314506119)) ;
#30952 = CARTESIAN_POINT('Ctrl Pts',(-15.4947170122384,-11.7170679291378,
-332.450751668014)) ;
#30953 = CARTESIAN_POINT('Ctrl Pts',(-15.1866665206812,-12.1152892190306,
-332.444735104618)) ;
#30954 = CARTESIAN_POINT('Ctrl Pts',(-15.0037239967095,-12.3411239143907,
-332.441298887799)) ;
#30955 = CARTESIAN_POINT('Ctrl Pts',(-14.4450966118055,-12.9999358605913,
-332.431148299937)) ;
#30956 = CARTESIAN_POINT('Ctrl Pts',(-14.055242733301,-13.4204805629253,-332.4245072442)) ;
#30957 = CARTESIAN_POINT('Ctrl Pts',(-13.5535984731228,-13.9157448947969,
-332.416201980336)) ;
#30958 = CARTESIAN_POINT('Ctrl Pts',(-13.4588912874011,-14.0073635210805,
-332.414643392202)) ;
#30959 = CARTESIAN_POINT('Ctrl Pts',(-13.2429961554026,-14.2120067553671,
-332.411103372992)) ;
#30960 = CARTESIAN_POINT('Ctrl Pts',(-13.121279367638,-14.324458481653,-332.409116592753)) ;
#30961 = CARTESIAN_POINT('Ctrl Pts',(-12.9396326178462,-14.4880202591157,
-332.406153316191)) ;
#30962 = CARTESIAN_POINT('Ctrl Pts',(-12.8808066171937,-14.5403453942164,
-332.405193916987)) ;
#30963 = CARTESIAN_POINT('Ctrl Pts',(-12.7716375520807,-14.6362677641729,
-332.403412307077)) ;
#30964 = CARTESIAN_POINT('Ctrl Pts',(-12.7213853650103,-14.6799664231755,
-332.402591610123)) ;
#30965 = CARTESIAN_POINT('Ctrl Pts',(-12.5955901877638,-14.7882252954947,
-332.400536390685)) ;
#30966 = CARTESIAN_POINT('Ctrl Pts',(-12.5197746705447,-14.8524658467341,
-332.39929715802)) ;
#30967 = CARTESIAN_POINT('Ctrl Pts',(-12.1717865264776,-15.142767842328,-332.393613267457)) ;
#30968 = CARTESIAN_POINT('Ctrl Pts',(-11.8939622737829,-15.3619486310123,
-332.389087928359)) ;
#30969 = CARTESIAN_POINT('Ctrl Pts',(-11.5326942342993,-15.6312814798705,
-332.383291120064)) ;
#30970 = CARTESIAN_POINT('Ctrl Pts',(-11.4546489307258,-15.6885631869735,
-332.382043785992)) ;
#30971 = CARTESIAN_POINT('Ctrl Pts',(-10.973894048919,-16.0359155823469,-332.374396324313)) ;
#30972 = CARTESIAN_POINT('Ctrl Pts',(-10.5606171535038,-16.3110485875344,
-332.367981417839)) ;
#30973 = CARTESIAN_POINT('Ctrl Pts',(-10.009640622601,-16.6481260620061,-332.35974641017)) ;
#30974 = CARTESIAN_POINT('Ctrl Pts',(-9.88112539612904,-16.7247232485876,
-332.357846756401)) ;
#30975 = CARTESIAN_POINT('Ctrl Pts',(-9.5611658863874,-16.9104490365189,-332.353172232872)) ;
#30976 = CARTESIAN_POINT('Ctrl Pts',(-9.36872500665138,-17.0178192410676,
-332.350408746948)) ;
#30977 = CARTESIAN_POINT('Ctrl Pts',(-9.056522161754,-17.1851082658492,-332.346004484073)) ;
#30978 = CARTESIAN_POINT('Ctrl Pts',(-8.93789510671079,-17.2471032609878,
-332.344348925304)) ;
#30979 = CARTESIAN_POINT('Ctrl Pts',(-8.70673695856695,-17.364882054619,-332.341157168328)) ;
#30980 = CARTESIAN_POINT('Ctrl Pts',(-8.59428682941758,-17.4208102905137,
-332.339619980433)) ;
#30981 = CARTESIAN_POINT('Ctrl Pts',(-8.31943551522749,-17.5542014850658,
-332.33589927257)) ;
#30982 = CARTESIAN_POINT('Ctrl Pts',(-8.15648508900026,-17.630506180893,-332.333724084194)) ;
#30983 = CARTESIAN_POINT('Ctrl Pts',(-7.33356451188227,-18.0020036892799,
-332.322880931629)) ;
#30984 = CARTESIAN_POINT('Ctrl Pts',(-6.65853711032058,-18.2624529937872,
-332.31446363226)) ;
#30985 = CARTESIAN_POINT('Ctrl Pts',(-5.57574936940371,-18.6121946282473,
-332.301164450802)) ;
#30986 = CARTESIAN_POINT('Ctrl Pts',(-5.17694700309865,-18.7270389564152,
-332.296302070594)) ;
#30987 = CARTESIAN_POINT('Ctrl Pts',(-4.65811098238901,-18.8586084530582,
-332.289884674294)) ;
#30988 = CARTESIAN_POINT('Ctrl Pts',(-4.54117471486675,-18.8871078478145,
-332.288432204837)) ;
#30989 = CARTESIAN_POINT('Ctrl Pts',(-4.35557352657564,-18.9305187430926,
-332.286112390987)) ;
#30990 = CARTESIAN_POINT('Ctrl Pts',(-4.28707947926307,-18.9461476337104,
-332.285253182086)) ;
#30991 = CARTESIAN_POINT('Ctrl Pts',(-4.1574320401589,-18.9749913832687,-332.283619788843)) ;
#30992 = CARTESIAN_POINT('Ctrl Pts',(-4.09629665022204,-18.9882830426053,
-332.282846627552)) ;
#30993 = CARTESIAN_POINT('Ctrl Pts',(-3.9218102891493,-19.0253368425524,-332.280632682393)) ;
#30994 = CARTESIAN_POINT('Ctrl Pts',(-3.80830964206489,-19.0483809161981,
-332.279183829931)) ;
#30995 = CARTESIAN_POINT('Ctrl Pts',(-3.17972743981411,-19.1701594293648,
-332.271124448513)) ;
#30996 = CARTESIAN_POINT('Ctrl Pts',(-2.6610169450038,-19.2490172959982,-332.264348663488)) ;
#30997 = CARTESIAN_POINT('Ctrl Pts',(-1.71549596462045,-19.3538085133732,
-332.252075231236)) ;
#30998 = CARTESIAN_POINT('Ctrl Pts',(-1.28980314857844,-19.3868315955085,
-332.246576467878)) ;
#30999 = CARTESIAN_POINT('Ctrl Pts',(-0.575820481165384,-19.4185968412911,
-332.237483147593)) ;
#31000 = CARTESIAN_POINT('Ctrl Pts',(-0.288023300897207,-19.4249971845775,
-332.233852058736)) ;
#31001 = CARTESIAN_POINT('Ctrl Pts',(-0.00018994165136052,-19.4249999990714,
-332.23026054535)) ;
#31002 = CARTESIAN_POINT('Ctrl Pts',(-0.000307707308464245,-19.4249999975628,
-332.019601838307)) ;
#31003 = CARTESIAN_POINT('Ctrl Pts',(-0.951439775158993,-19.4249849308813,
-332.030960958138)) ;
#31004 = CARTESIAN_POINT('Ctrl Pts',(-1.90128001069508,-19.3551129679746,
-332.041854748475)) ;
#31005 = CARTESIAN_POINT('Ctrl Pts',(-2.97483821811274,-19.1963264387993,
-332.054729320748)) ;
#31006 = CARTESIAN_POINT('Ctrl Pts',(-3.10730053904505,-19.1753303611542,
-332.056329149228)) ;
#31007 = CARTESIAN_POINT('Ctrl Pts',(-3.31967132845602,-19.1394099407424,
-332.058918618489)) ;
#31008 = CARTESIAN_POINT('Ctrl Pts',(-3.39972210395476,-19.1253528125581,
-332.059900316459)) ;
#31009 = CARTESIAN_POINT('Ctrl Pts',(-3.54100130439389,-19.09962877773,-332.061644494685)) ;
#31010 = CARTESIAN_POINT('Ctrl Pts',(-3.60226624863132,-19.0881687845743,
-332.062404717117)) ;
#31011 = CARTESIAN_POINT('Ctrl Pts',(-3.72859414795776,-19.0639085075207,
-332.063981187286)) ;
#31012 = CARTESIAN_POINT('Ctrl Pts',(-3.79364867445113,-19.0510695659084,
-332.064798046553)) ;
#31013 = CARTESIAN_POINT('Ctrl Pts',(-3.95380799781003,-19.0186081794214,
-332.06682094192)) ;
#31014 = CARTESIAN_POINT('Ctrl Pts',(-4.04883375871283,-18.9986052099552,
-332.068031342115)) ;
#31015 = CARTESIAN_POINT('Ctrl Pts',(-4.4347662699367,-18.9143392250366,-332.072983066224)) ;
#31016 = CARTESIAN_POINT('Ctrl Pts',(-4.72432617156596,-18.8441004511013,
-332.076780831277)) ;
#31017 = CARTESIAN_POINT('Ctrl Pts',(-5.60018938653857,-18.6101840807685,
-332.088415359661)) ;
#31018 = CARTESIAN_POINT('Ctrl Pts',(-6.18051791537393,-18.4255874638366,
-332.096317378858)) ;
#31019 = CARTESIAN_POINT('Ctrl Pts',(-6.97572807306964,-18.1308348139672,
-332.107155093707)) ;
#31020 = CARTESIAN_POINT('Ctrl Pts',(-7.19867741351687,-18.0434751910813,
-332.110196346514)) ;
#31021 = CARTESIAN_POINT('Ctrl Pts',(-7.55712179396332,-17.895322409297,-332.115082258856)) ;
#31022 = CARTESIAN_POINT('Ctrl Pts',(-7.69363442015092,-17.8370581494356,
-332.116942252803)) ;
#31023 = CARTESIAN_POINT('Ctrl Pts',(-7.89351260812988,-17.749027616591,-332.119663759718)) ;
#31024 = CARTESIAN_POINT('Ctrl Pts',(-7.95740633862362,-17.7204742317892,
-332.120533453343)) ;
#31025 = CARTESIAN_POINT('Ctrl Pts',(-8.12623069554891,-17.643931331889,-332.122830681574)) ;
#31026 = CARTESIAN_POINT('Ctrl Pts',(-8.23089046721392,-17.5953510995359,
-332.124254041529)) ;
#31027 = CARTESIAN_POINT('Ctrl Pts',(-8.43988527275577,-17.4960686010512,
-332.12709509048)) ;
#31028 = CARTESIAN_POINT('Ctrl Pts',(-8.54421142404382,-17.4453584396755,
-332.12851265188)) ;
#31029 = CARTESIAN_POINT('Ctrl Pts',(-8.82016514828314,-17.3081554988732,
-332.132261505826)) ;
#31030 = CARTESIAN_POINT('Ctrl Pts',(-8.99097401522743,-17.2200449021287,
-332.134581100717)) ;
#31031 = CARTESIAN_POINT('Ctrl Pts',(-9.69381805701577,-16.8441788132686,
-332.144134165511)) ;
#31032 = CARTESIAN_POINT('Ctrl Pts',(-10.2135758742315,-16.5341869339315,
-332.151207780682)) ;
#31033 = CARTESIAN_POINT('Ctrl Pts',(-11.0248944697991,-15.9974284287092,
-332.162569420456)) ;
#31034 = CARTESIAN_POINT('Ctrl Pts',(-11.3259363983318,-15.785727047809,-332.166864059495)) ;
#31035 = CARTESIAN_POINT('Ctrl Pts',(-11.7390432636421,-15.4773146486361,
-332.172966141708)) ;
#31036 = CARTESIAN_POINT('Ctrl Pts',(-11.8562933575024,-15.3876805663342,
-332.174722745356)) ;
#31037 = CARTESIAN_POINT('Ctrl Pts',(-12.0570342057736,-15.2305637441514,
-332.177782219564)) ;
#31038 = CARTESIAN_POINT('Ctrl Pts',(-12.1410080832767,-15.1637089288877,
-332.179078145417)) ;
#31039 = CARTESIAN_POINT('Ctrl Pts',(-12.2255574507256,-15.0952433616759,
-332.180401551843)) ;
#31040 = CARTESIAN_POINT('Ctrl Pts',(-12.2266913522466,-15.0943249503285,
-332.180419303618)) ;
#31041 = CARTESIAN_POINT('Ctrl Pts',(-12.228994943295,-15.0924587110059,-332.180455374399)) ;
#31042 = CARTESIAN_POINT('Ctrl Pts',(-12.2301646261241,-15.0915108748082,
-332.18047369352)) ;
#31043 = CARTESIAN_POINT('Ctrl Pts',(-12.2325396076684,-15.0895858841255,
-332.180510896976)) ;
#31044 = CARTESIAN_POINT('Ctrl Pts',(-12.2337448995204,-15.0886087211854,
-332.18052978143)) ;
#31045 = CARTESIAN_POINT('Ctrl Pts',(-12.2361908825572,-15.0866252103536,
-332.180568112855)) ;
#31046 = CARTESIAN_POINT('Ctrl Pts',(-12.2374315667093,-15.0856188538011,
-332.180587559949)) ;
#31047 = CARTESIAN_POINT('Ctrl Pts',(-12.2399480783119,-15.0835771201652,
-332.180627013358)) ;
#31048 = CARTESIAN_POINT('Ctrl Pts',(-12.2412238985732,-15.0825417342284,
-332.180647019799)) ;
#31049 = CARTESIAN_POINT('Ctrl Pts',(-12.2438103920022,-15.080442133277,-332.180687588083)) ;
#31050 = CARTESIAN_POINT('Ctrl Pts',(-12.2451210577871,-15.0793779092692,
-332.180708150054)) ;
#31051 = CARTESIAN_POINT('Ctrl Pts',(-12.2477769226022,-15.0772208466292,
-332.180749825136)) ;
#31052 = CARTESIAN_POINT('Ctrl Pts',(-12.2491221141719,-15.076127998792,-332.180770938378)) ;
#31053 = CARTESIAN_POINT('Ctrl Pts',(-12.2510140309455,-15.0745905652572,
-332.180800639532)) ;
#31054 = CARTESIAN_POINT('Ctrl Pts',(-12.2515608783424,-15.0741461297426,
-332.180809225283)) ;
#31055 = CARTESIAN_POINT('Ctrl Pts',(-12.2527455125578,-15.0731832430996,
-332.180827826327)) ;
#31056 = CARTESIAN_POINT('Ctrl Pts',(-12.2533832906134,-15.0726647812813,
-332.180837841773)) ;
#31057 = CARTESIAN_POINT('Ctrl Pts',(-12.2547627292948,-15.071543264126,-332.180859506384)) ;
#31058 = CARTESIAN_POINT('Ctrl Pts',(-12.2555043782651,-15.0709401945619,
-332.180871155752)) ;
#31059 = CARTESIAN_POINT('Ctrl Pts',(-12.2571056448104,-15.0696379332673,
-332.180896310687)) ;
#31060 = CARTESIAN_POINT('Ctrl Pts',(-12.2579652472085,-15.0689387226188,
-332.180909816528)) ;
#31061 = CARTESIAN_POINT('Ctrl Pts',(-12.3060966463666,-15.0297812356691,
-332.181666156376)) ;
#31062 = CARTESIAN_POINT('Ctrl Pts',(-12.3531872611223,-14.9911007985688,
-332.182412210617)) ;
#31063 = CARTESIAN_POINT('Ctrl Pts',(-12.4486230672338,-14.9119543775599,
-332.183937416464)) ;
#31064 = CARTESIAN_POINT('Ctrl Pts',(-12.4969548139917,-14.8714733632677,
-332.184716766015)) ;
#31065 = CARTESIAN_POINT('Ctrl Pts',(-12.6356024881665,-14.7541936275622,
-332.186971400356)) ;
#31066 = CARTESIAN_POINT('Ctrl Pts',(-12.7254134726544,-14.6768025034912,
-332.188455207695)) ;
#31067 = CARTESIAN_POINT('Ctrl Pts',(-13.115198781367,-14.3346525834505,-332.194987196964)) ;
#31068 = CARTESIAN_POINT('Ctrl Pts',(-13.4076605370497,-14.061484337325,-332.200128175233)) ;
#31069 = CARTESIAN_POINT('Ctrl Pts',(-13.9510611975513,-13.5215541457519,
-332.21000327909)) ;
#31070 = CARTESIAN_POINT('Ctrl Pts',(-14.2033054706494,-13.2563437306619,
-332.214732895086)) ;
#31071 = CARTESIAN_POINT('Ctrl Pts',(-14.639493158379,-12.7709834122329,-332.223107656365)) ;
#31072 = CARTESIAN_POINT('Ctrl Pts',(-14.8263370842533,-12.5535853980457,
-332.226765010315)) ;
#31073 = CARTESIAN_POINT('Ctrl Pts',(-15.1503124976644,-12.1593047735721,
-332.233215559331)) ;
#31074 = CARTESIAN_POINT('Ctrl Pts',(-15.2893271087701,-11.984036806253,-332.23602183866)) ;
#31075 = CARTESIAN_POINT('Ctrl Pts',(-15.5069999323951,-11.6996433312443,
-332.240476032222)) ;
#31076 = CARTESIAN_POINT('Ctrl Pts',(-15.5876054753994,-11.5920341866365,
-332.242139355618)) ;
#31077 = CARTESIAN_POINT('Ctrl Pts',(-15.7419976289247,-11.381396752822,-332.245352930139)) ;
#31078 = CARTESIAN_POINT('Ctrl Pts',(-15.8159060672609,-11.2784660621457,
-332.246904107956)) ;
#31079 = CARTESIAN_POINT('Ctrl Pts',(-15.9918278283731,-11.0283335164022,
-332.250628687595)) ;
#31080 = CARTESIAN_POINT('Ctrl Pts',(-16.0928228896023,-10.8804296337474,
-332.25279404405)) ;
#31081 = CARTESIAN_POINT('Ctrl Pts',(-16.5954006564032,-10.1221122501266,
-332.263721035737)) ;
#31082 = CARTESIAN_POINT('Ctrl Pts',(-16.9643593381631,-9.49078458366264,
-332.272225256033)) ;
#31083 = CARTESIAN_POINT('Ctrl Pts',(-17.4835040906425,-8.47501530310121,
-332.285559362289)) ;
#31084 = CARTESIAN_POINT('Ctrl Pts',(-17.6585226967641,-8.10403444756312,
-332.29036685726)) ;
#31085 = CARTESIAN_POINT('Ctrl Pts',(-17.8693367872057,-7.6178596528184,-332.296720849966)) ;
#31086 = CARTESIAN_POINT('Ctrl Pts',(-17.915987951277,-7.50748683455282,-332.298167030131)) ;
#31087 = CARTESIAN_POINT('Ctrl Pts',(-17.9883263876698,-7.33182512590009,
-332.3004792319)) ;
#31088 = CARTESIAN_POINT('Ctrl Pts',(-18.0146863553376,-7.26681645687894,
-332.301337207854)) ;
#31089 = CARTESIAN_POINT('Ctrl Pts',(-18.0639193856539,-7.14348416703496,
-332.302970422312)) ;
#31090 = CARTESIAN_POINT('Ctrl Pts',(-18.0868635660893,-7.085189901955,-332.303744657638)) ;
#31091 = CARTESIAN_POINT('Ctrl Pts',(-18.1515929910921,-6.91836836933145,
-332.305965705484)) ;
#31092 = CARTESIAN_POINT('Ctrl Pts',(-18.1926861617147,-6.80957554994537,
-332.307420665331)) ;
#31093 = CARTESIAN_POINT('Ctrl Pts',(-18.3545756949256,-6.36905103519003,
-332.313328893853)) ;
#31094 = CARTESIAN_POINT('Ctrl Pts',(-18.4672950971057,-6.03442383918995,
-332.317853922846)) ;
#31095 = CARTESIAN_POINT('Ctrl Pts',(-18.6016568407138,-5.59643050870255,
-332.323753268223)) ;
#31096 = CARTESIAN_POINT('Ctrl Pts',(-18.6316651657819,-5.49570057430084,
-332.325108519062)) ;
#31097 = CARTESIAN_POINT('Ctrl Pts',(-18.7910735249853,-4.94429298854793,
-332.332512834497)) ;
#31098 = CARTESIAN_POINT('Ctrl Pts',(-18.9049409099176,-4.48928590308809,
-332.338565768473)) ;
#31099 = CARTESIAN_POINT('Ctrl Pts',(-19.0322950044249,-3.8888767709539,-332.346385218203)) ;
#31100 = CARTESIAN_POINT('Ctrl Pts',(-19.0607707745075,-3.74681641094796,
-332.348223595899)) ;
#31101 = CARTESIAN_POINT('Ctrl Pts',(-19.1276543112821,-3.39262933653316,
-332.352775250304)) ;
#31102 = CARTESIAN_POINT('Ctrl Pts',(-19.1641252752612,-3.18015658956369,
-332.355477369648)) ;
#31103 = CARTESIAN_POINT('Ctrl Pts',(-19.2173652942855,-2.83569758372706,
-332.359809990587)) ;
#31104 = CARTESIAN_POINT('Ctrl Pts',(-19.2363281062274,-2.70406928300005,
-332.361454390973)) ;
#31105 = CARTESIAN_POINT('Ctrl Pts',(-19.2706293561641,-2.44731645927699,
-332.364640382477)) ;
#31106 = CARTESIAN_POINT('Ctrl Pts',(-19.2861044002777,-2.32221677378434,
-332.366182790691)) ;
#31107 = CARTESIAN_POINT('Ctrl Pts',(-19.317716192861,-2.04450813738184,-332.369585730242)) ;
#31108 = CARTESIAN_POINT('Ctrl Pts',(-19.3332643806804,-1.89184061186663,
-332.371442391225)) ;
#31109 = CARTESIAN_POINT('Ctrl Pts',(-19.3892511202734,-1.26896965949256,
-332.378965628)) ;
#31110 = CARTESIAN_POINT('Ctrl Pts',(-19.4143569974093,-0.797550452465386,
-332.384535355409)) ;
#31111 = CARTESIAN_POINT('Ctrl Pts',(-19.4252749986705,-0.146454517787673,
-332.392162686992)) ;
#31112 = CARTESIAN_POINT('Ctrl Pts',(-19.4257993727771,0.0328092926956076,
-332.394256452771)) ;
#31113 = CARTESIAN_POINT('Ctrl Pts',(-19.4198018815971,0.582169251885124,
-332.400672972894)) ;
#31114 = CARTESIAN_POINT('Ctrl Pts',(-19.4051834745485,0.952092324516055,
-332.404992617901)) ;
#31115 = CARTESIAN_POINT('Ctrl Pts',(-19.3699347202311,1.46907142367132,-332.411125563733)) ;
#31116 = CARTESIAN_POINT('Ctrl Pts',(-19.3581759989151,1.61665204059852,-332.412887533737)) ;
#31117 = CARTESIAN_POINT('Ctrl Pts',(-19.334241369452,1.87911634506717,-332.416050488706)) ;
#31118 = CARTESIAN_POINT('Ctrl Pts',(-19.3227254735061,1.9940531057691,-332.417445658719)) ;
#31119 = CARTESIAN_POINT('Ctrl Pts',(-19.3026602360087,2.17778258347615,-332.419696308407)) ;
#31120 = CARTESIAN_POINT('Ctrl Pts',(-19.2947666182339,2.2466442345652,-332.42054446127)) ;
#31121 = CARTESIAN_POINT('Ctrl Pts',(-19.2778310352548,2.38770816712964,-332.422292582599)) ;
#31122 = CARTESIAN_POINT('Ctrl Pts',(-19.268751595483,2.45990480503155,-332.423192933375)) ;
#31123 = CARTESIAN_POINT('Ctrl Pts',(-19.2419247586514,2.66395507253136,-332.425751941356)) ;
#31124 = CARTESIAN_POINT('Ctrl Pts',(-19.2232281358396,2.79567970256964,-332.427420847213)) ;
#31125 = CARTESIAN_POINT('Ctrl Pts',(-19.142664934783,3.32419458236349,-332.434171356912)) ;
#31126 = CARTESIAN_POINT('Ctrl Pts',(-19.0698539343263,3.71921504313502,-332.439338386003)) ;
#31127 = CARTESIAN_POINT('Ctrl Pts',(-18.9816921153021,4.12628310752134,-332.444709778016)) ;
#31128 = CARTESIAN_POINT('Ctrl Pts',(-18.9785154974058,4.14086915492972,-332.444902311319)) ;
#31129 = CARTESIAN_POINT('Ctrl Pts',(-18.873323934961,4.62121256983114,-332.451244822057)) ;
#31130 = CARTESIAN_POINT('Ctrl Pts',(-18.7542116031314,5.08306113614125,-332.457402211653)) ;
#31131 = CARTESIAN_POINT('Ctrl Pts',(-18.5765087687407,5.6802591136536,-332.465342018263)) ;
#31132 = CARTESIAN_POINT('Ctrl Pts',(-18.5332081995949,5.81998415168714,-332.467198479046)) ;
#31133 = CARTESIAN_POINT('Ctrl Pts',(-18.4217667368634,6.16572931278951,-332.471786494001)) ;
#31134 = CARTESIAN_POINT('Ctrl Pts',(-18.3517440861384,6.37112210684672,-332.474506822288)) ;
#31135 = CARTESIAN_POINT('Ctrl Pts',(-18.2331939049386,6.70067293632887,-332.478860705002)) ;
#31136 = CARTESIAN_POINT('Ctrl Pts',(-18.1868039746501,6.8255797570648,-332.480508418207)) ;
#31137 = CARTESIAN_POINT('Ctrl Pts',(-18.0940849993818,7.06757139849144,-332.483696046075)) ;
#31138 = CARTESIAN_POINT('Ctrl Pts',(-18.0478953287191,7.18470261663132,-332.485236829812)) ;
#31139 = CARTESIAN_POINT('Ctrl Pts',(-17.9321610439444,7.47003005996469,-332.488985931035)) ;
#31140 = CARTESIAN_POINT('Ctrl Pts',(-17.8613850174887,7.63771393777761,-332.491185586413)) ;
#31141 = CARTESIAN_POINT('Ctrl Pts',(-17.5060943264401,8.44751630380189,-332.501801973352)) ;
#31142 = CARTESIAN_POINT('Ctrl Pts',(-17.1892537988264,9.07487878020027,-332.509985568648)) ;
#31143 = CARTESIAN_POINT('Ctrl Pts',(-16.681154859224,9.95841987901278,-332.521895121165)) ;
#31144 = CARTESIAN_POINT('Ctrl Pts',(-16.5164731476687,10.2292310654247,-332.525604710508)) ;
#31145 = CARTESIAN_POINT('Ctrl Pts',(-16.2717131248583,10.6103955832704,-332.530976731591)) ;
#31146 = CARTESIAN_POINT('Ctrl Pts',(-16.1969846593275,10.7241237555622,-332.532599465547)) ;
#31147 = CARTESIAN_POINT('Ctrl Pts',(-16.0604812899361,10.927184419568,-332.535540293521)) ;
#31148 = CARTESIAN_POINT('Ctrl Pts',(-15.9991404240994,11.0168019064017,-332.536853685179)) ;
#31149 = CARTESIAN_POINT('Ctrl Pts',(-15.8981493742989,11.1617248321356,-332.539006630466)) ;
#31150 = CARTESIAN_POINT('Ctrl Pts',(-15.858954338678,11.2173446968817,-332.539839976194)) ;
#31151 = CARTESIAN_POINT('Ctrl Pts',(-15.7760317342591,11.3337129830864,-332.541599483263)) ;
#31152 = CARTESIAN_POINT('Ctrl Pts',(-15.7322437134957,11.3944168338817,-332.542526432763)) ;
#31153 = CARTESIAN_POINT('Ctrl Pts',(-15.6032171233982,11.5711262614762,-332.545249604931)) ;
#31154 = CARTESIAN_POINT('Ctrl Pts',(-15.5170386270037,11.6864391370296,-332.547058134858)) ;
#31155 = CARTESIAN_POINT('Ctrl Pts',(-15.0588465204583,12.2855277381321,-332.556597945434)) ;
#31156 = CARTESIAN_POINT('Ctrl Pts',(-14.6654691378138,12.7525317234778,-332.564520907751)) ;
#31157 = CARTESIAN_POINT('Ctrl Pts',(-14.0150958320654,13.454664007329,-332.576846162247)) ;
#31158 = CARTESIAN_POINT('Ctrl Pts',(-13.7726572702083,13.7027299153684,-332.581292063254)) ;
#31159 = CARTESIAN_POINT('Ctrl Pts',(-13.3416103969075,14.1207792413035,-332.588907541145)) ;
#31160 = CARTESIAN_POINT('Ctrl Pts',(-13.1560707461509,14.2938020574615,-332.592098857732)) ;
#31161 = CARTESIAN_POINT('Ctrl Pts',(-12.8631468947255,14.5564283219298,-332.597000238133)) ;
#31162 = CARTESIAN_POINT('Ctrl Pts',(-12.758094556452,14.6485895867739,-332.598731794467)) ;
#31163 = CARTESIAN_POINT('Ctrl Pts',(-12.5572621011422,14.8209783917265,-332.601993000319)) ;
#31164 = CARTESIAN_POINT('Ctrl Pts',(-12.4616845566394,14.9014311400923,-332.603524521271)) ;
#31165 = CARTESIAN_POINT('Ctrl Pts',(-12.239634706448,15.0847119185599,-332.607036561693)) ;
#31166 = CARTESIAN_POINT('Ctrl Pts',(-12.1126308864883,15.1868813296355,-332.609011539671)) ;
#31167 = CARTESIAN_POINT('Ctrl Pts',(-11.6807329638849,15.525461132819,-332.615620354055)) ;
#31168 = CARTESIAN_POINT('Ctrl Pts',(-11.3700858147713,15.7543840066875,-332.620195103011)) ;
#31169 = CARTESIAN_POINT('Ctrl Pts',(-10.5751372633674,16.3044329621867,-332.631559884871)) ;
#31170 = CARTESIAN_POINT('Ctrl Pts',(-10.0828617378029,16.6133669017344,-332.638289209997)) ;
#31171 = CARTESIAN_POINT('Ctrl Pts',(-9.46212466471949,16.9651526365882,-332.646694305598)) ;
#31172 = CARTESIAN_POINT('Ctrl Pts',(-9.34609816972103,17.0293469077564,-332.648262536072)) ;
#31173 = CARTESIAN_POINT('Ctrl Pts',(-9.15871136320605,17.1305309116395,-332.650796593944)) ;
#31174 = CARTESIAN_POINT('Ctrl Pts',(-9.0877628722214,17.168274494321,-332.651756344326)) ;
#31175 = CARTESIAN_POINT('Ctrl Pts',(-8.91252410717003,17.2601083670129,-332.654129735758)) ;
#31176 = CARTESIAN_POINT('Ctrl Pts',(-8.80797349649241,17.3136948577398,-332.655548213167)) ;
#31177 = CARTESIAN_POINT('Ctrl Pts',(-8.64063794099014,17.3975532145856,-332.657826942176)) ;
#31178 = CARTESIAN_POINT('Ctrl Pts',(-8.57816495760147,17.4284413485401,-332.658679540645)) ;
#31179 = CARTESIAN_POINT('Ctrl Pts',(-8.45886878010149,17.4866273995058,-332.660312321856)) ;
#31180 = CARTESIAN_POINT('Ctrl Pts',(-8.40207629998039,17.5139862020692,-332.661091591915)) ;
#31181 = CARTESIAN_POINT('Ctrl Pts',(-8.23812798589591,17.5919845056805,-332.663345706882)) ;
#31182 = CARTESIAN_POINT('Ctrl Pts',(-8.13064064003027,17.6419203682814,-332.664829068499)) ;
#31183 = CARTESIAN_POINT('Ctrl Pts',(-7.65866279998202,17.8559594888764,-332.671355872311)) ;
#31184 = CARTESIAN_POINT('Ctrl Pts',(-7.28961378087681,18.0097733234336,-332.676491945733)) ;
#31185 = CARTESIAN_POINT('Ctrl Pts',(-6.57506149291105,18.2820231290669,-332.686349256319)) ;
#31186 = CARTESIAN_POINT('Ctrl Pts',(-6.23044537861813,18.4023192573496,-332.69106594326)) ;
#31187 = CARTESIAN_POINT('Ctrl Pts',(-5.60878618085292,18.5998579120733,-332.699437691383)) ;
#31188 = CARTESIAN_POINT('Ctrl Pts',(-5.33302918488979,18.6807921919778,-332.703104605044)) ;
#31189 = CARTESIAN_POINT('Ctrl Pts',(-4.83922451433934,18.8138975493996,-332.709569592744)) ;
#31190 = CARTESIAN_POINT('Ctrl Pts',(-4.6218777917697,18.868467898529,-332.712380843555)) ;
#31191 = CARTESIAN_POINT('Ctrl Pts',(-4.27262091889825,18.9497606903381,-332.71684083581)) ;
#31192 = CARTESIAN_POINT('Ctrl Pts',(-4.14129308742704,18.978893839237,-332.718505059916)) ;
#31193 = CARTESIAN_POINT('Ctrl Pts',(-3.88572102613006,19.0328096983907,-332.72171914528)) ;
#31194 = CARTESIAN_POINT('Ctrl Pts',(-3.76151597773658,19.0577456826991,-332.723269946789)) ;
#31195 = CARTESIAN_POINT('Ctrl Pts',(-3.46137128063637,19.1149555993557,-332.726991524299)) ;
#31196 = CARTESIAN_POINT('Ctrl Pts',(-3.28521240182119,19.1460178186432,-332.729154289542)) ;
#31197 = CARTESIAN_POINT('Ctrl Pts',(-2.38620068584094,19.2917682442597,-332.740093801473)) ;
#31198 = CARTESIAN_POINT('Ctrl Pts',(-1.65770878656152,19.3679704069865,-332.74861199613)) ;
#31199 = CARTESIAN_POINT('Ctrl Pts',(-0.517637276200755,19.4224189521836,
-332.761953595217)) ;
#31200 = CARTESIAN_POINT('Ctrl Pts',(-0.108099806806295,19.4290148804684,
-332.766754223067)) ;
#31201 = CARTESIAN_POINT('Ctrl Pts',(0.421081211273075,19.4208047584362,-332.773100279281)) ;
#31202 = CARTESIAN_POINT('Ctrl Pts',(0.540804409498887,19.4178396681817,-332.774545667479)) ;
#31203 = CARTESIAN_POINT('Ctrl Pts',(0.730587800434719,19.4113828853774,-332.776856911019)) ;
#31204 = CARTESIAN_POINT('Ctrl Pts',(0.800669779955762,19.4086184967789,-332.777714732002)) ;
#31205 = CARTESIAN_POINT('Ctrl Pts',(0.933329644431869,19.4026659695296,-332.779347925939)) ;
#31206 = CARTESIAN_POINT('Ctrl Pts',(0.995910069984909,19.3995544812717,-332.780122298234)) ;
#31207 = CARTESIAN_POINT('Ctrl Pts',(1.17465513176301,19.3898001151477,-332.782344250563)) ;
#31208 = CARTESIAN_POINT('Ctrl Pts',(1.2907765404271,19.3824162334728,-332.783799987968)) ;
#31209 = CARTESIAN_POINT('Ctrl Pts',(1.7597563838488,19.3483616931963,-332.789719431497)) ;
#31210 = CARTESIAN_POINT('Ctrl Pts',(2.11192170133388,19.3130947471029,-332.794255238131)) ;
#31211 = CARTESIAN_POINT('Ctrl Pts',(2.9985047355511,19.1997688963305,-332.805764730046)) ;
#31212 = CARTESIAN_POINT('Ctrl Pts',(3.53099754033945,19.1090087269549,-332.812756511182)) ;
#31213 = CARTESIAN_POINT('Ctrl Pts',(4.37803642169187,18.9280173990274,-332.823810937845)) ;
#31214 = CARTESIAN_POINT('Ctrl Pts',(4.69528922442561,18.8518249892294,-332.827937604129)) ;
#31215 = CARTESIAN_POINT('Ctrl Pts',(5.15639586540763,18.7287217355113,-332.833900871855)) ;
#31216 = CARTESIAN_POINT('Ctrl Pts',(5.3018595103528,18.6880636231466,-332.835777165975)) ;
#31217 = CARTESIAN_POINT('Ctrl Pts',(5.56578347683712,18.6109654665928,-332.839172417575)) ;
#31218 = CARTESIAN_POINT('Ctrl Pts',(5.68439749280751,18.5750802555426,-332.840694989585)) ;
#31219 = CARTESIAN_POINT('Ctrl Pts',(5.94602210090458,18.4931882740085,-332.844046528912)) ;
#31220 = CARTESIAN_POINT('Ctrl Pts',(6.08885885420201,18.4466525227567,-332.845871813009)) ;
#31221 = CARTESIAN_POINT('Ctrl Pts',(6.53459891640948,18.2956905004917,-332.851556916245)) ;
#31222 = CARTESIAN_POINT('Ctrl Pts',(6.83546749279926,18.1854243461246,-332.855377578623)) ;
#31223 = CARTESIAN_POINT('Ctrl Pts',(7.75515833716328,17.8223142726826,-332.86706352596)) ;
#31224 = CARTESIAN_POINT('Ctrl Pts',(8.36376086390613,17.5449385488919,-332.87479309188)) ;
#31225 = CARTESIAN_POINT('Ctrl Pts',(9.20570521869414,17.107433071553,-332.885958357462)) ;
#31226 = CARTESIAN_POINT('Ctrl Pts',(9.4517284328849,16.9727459150251,-332.889283622524)) ;
#31227 = CARTESIAN_POINT('Ctrl Pts',(9.77574235800309,16.786131847062,-332.893794817613)) ;
#31228 = CARTESIAN_POINT('Ctrl Pts',(9.8563984009187,16.7388999509152,-332.894928942998)) ;
#31229 = CARTESIAN_POINT('Ctrl Pts',(9.99336662489437,16.65735861703,-332.896876483446)) ;
#31230 = CARTESIAN_POINT('Ctrl Pts',(10.0498506987496,16.6233412264064,-332.897686042666)) ;
#31231 = CARTESIAN_POINT('Ctrl Pts',(10.1764089524122,16.5462410276427,-332.89951489572)) ;
#31232 = CARTESIAN_POINT('Ctrl Pts',(10.2463847022609,16.5029994795317,-332.900536254257)) ;
#31233 = CARTESIAN_POINT('Ctrl Pts',(10.4750458545714,16.3596832119398,-332.903904447575)) ;
#31234 = CARTESIAN_POINT('Ctrl Pts',(10.6325562092451,16.2577541100572,-332.906273341475)) ;
#31235 = CARTESIAN_POINT('Ctrl Pts',(11.512525695155,15.6700441407369,-332.919733147003)) ;
#31236 = CARTESIAN_POINT('Ctrl Pts',(12.2031638722667,15.138405944195,-332.93111674204)) ;
#31237 = CARTESIAN_POINT('Ctrl Pts',(13.0556329510556,14.3858305828786,-332.945556867364)) ;
#31238 = CARTESIAN_POINT('Ctrl Pts',(13.2518033584738,14.2053293340077,-332.948913822778)) ;
#31239 = CARTESIAN_POINT('Ctrl Pts',(13.5466390717352,13.9226196533746,-332.954006002188)) ;
#31240 = CARTESIAN_POINT('Ctrl Pts',(13.6480012761273,13.8232712983814,-332.955765583982)) ;
#31241 = CARTESIAN_POINT('Ctrl Pts',(13.8362298720489,13.6346936907985,-332.95905017065)) ;
#31242 = CARTESIAN_POINT('Ctrl Pts',(13.9233447226969,13.5457226050846,-332.960577402193)) ;
#31243 = CARTESIAN_POINT('Ctrl Pts',(14.11985368302,13.3411277824146,-332.964039509232)) ;
#31244 = CARTESIAN_POINT('Ctrl Pts',(14.2286942265889,13.2249846591956,-332.965969403081)) ;
#31245 = CARTESIAN_POINT('Ctrl Pts',(14.6002130666653,12.8186430556208,-332.972604926997)) ;
#31246 = CARTESIAN_POINT('Ctrl Pts',(14.8555396680625,12.5218518400703,-332.977248349292)) ;
#31247 = CARTESIAN_POINT('Ctrl Pts',(15.4694125434608,11.7630630501135,-332.988724987734)) ;
#31248 = CARTESIAN_POINT('Ctrl Pts',(15.8163948939545,11.292210924903,-332.995496618422)) ;
#31249 = CARTESIAN_POINT('Ctrl Pts',(16.2155983937038,10.6959188602019,-333.003949500851)) ;
#31250 = CARTESIAN_POINT('Ctrl Pts',(16.2884462982189,10.5846506162908,-333.005522292819)) ;
#31251 = CARTESIAN_POINT('Ctrl Pts',(16.403561993799,10.4048192664751,-333.008062902962)) ;
#31252 = CARTESIAN_POINT('Ctrl Pts',(16.4465560073873,10.336726054856,-333.00902460996)) ;
#31253 = CARTESIAN_POINT('Ctrl Pts',(16.5513203752515,10.168493588557,-333.011402025205)) ;
#31254 = CARTESIAN_POINT('Ctrl Pts',(16.612606688774,10.0680567622816,-333.012822575403)) ;
#31255 = CARTESIAN_POINT('Ctrl Pts',(16.708753103041,9.90722243438955,-333.015103805458)) ;
#31256 = CARTESIAN_POINT('Ctrl Pts',(16.7442070469886,9.84718320068299,-333.015956802993)) ;
#31257 = CARTESIAN_POINT('Ctrl Pts',(16.8110823292512,9.73252823750605,-333.01758959551)) ;
#31258 = CARTESIAN_POINT('Ctrl Pts',(16.8425626827219,9.67794798715886,-333.018368470866)) ;
#31259 = CARTESIAN_POINT('Ctrl Pts',(16.9324052968254,9.52041392657122,-333.020620005819)) ;
#31260 = CARTESIAN_POINT('Ctrl Pts',(16.9900929482566,9.41707874115112,-333.022101153134)) ;
#31261 = CARTESIAN_POINT('Ctrl Pts',(17.3571183864579,8.74527895506652,-333.031741881167)) ;
#31262 = CARTESIAN_POINT('Ctrl Pts',(17.6388271783303,8.16218343631383,-333.040148176756)) ;
#31263 = CARTESIAN_POINT('Ctrl Pts',(18.0275342779838,7.24304337877152,-333.053002058919)) ;
#31264 = CARTESIAN_POINT('Ctrl Pts',(18.1553873651541,6.91632704941147,-333.057500179498)) ;
#31265 = CARTESIAN_POINT('Ctrl Pts',(18.3609612707661,6.34594487241042,-333.065190985208)) ;
#31266 = CARTESIAN_POINT('Ctrl Pts',(18.4428474099819,6.10387540020582,-333.068406056403)) ;
#31267 = CARTESIAN_POINT('Ctrl Pts',(18.562189085288,5.72672494866377,-333.073334865681)) ;
#31268 = CARTESIAN_POINT('Ctrl Pts',(18.6029983375919,5.59273593100718,-333.075070497916)) ;
#31269 = CARTESIAN_POINT('Ctrl Pts',(18.6774395802552,5.33848905934159,-333.078334996046)) ;
#31270 = CARTESIAN_POINT('Ctrl Pts',(18.711368072532,5.2183253647359,-333.079865785902)) ;
#31271 = CARTESIAN_POINT('Ctrl Pts',(18.7867547087438,4.94113805520366,-333.083369996614)) ;
#31272 = CARTESIAN_POINT('Ctrl Pts',(18.8274069419168,4.78390485994989,-333.085337963309)) ;
#31273 = CARTESIAN_POINT('Ctrl Pts',(18.9674860778513,4.21264640956687,-333.092421980478)) ;
#31274 = CARTESIAN_POINT('Ctrl Pts',(19.0552654038366,3.79588980486646,-333.097462568134)) ;
#31275 = CARTESIAN_POINT('Ctrl Pts',(19.2249088583184,2.83481333668933,-333.108917883733)) ;
#31276 = CARTESIAN_POINT('Ctrl Pts',(19.29748011242,2.28922411432976,-333.115295851395)) ;
#31277 = CARTESIAN_POINT('Ctrl Pts',(19.3583782397329,1.61260980982352,-333.12330253624)) ;
#31278 = CARTESIAN_POINT('Ctrl Pts',(19.368676077332,1.48381448806581,-333.124831359226)) ;
#31279 = CARTESIAN_POINT('Ctrl Pts',(19.3890957028787,1.19178001904634,-333.128316197844)) ;
#31280 = CARTESIAN_POINT('Ctrl Pts',(19.3984423736851,1.02849653318006,-333.130277594457)) ;
#31281 = CARTESIAN_POINT('Ctrl Pts',(19.409215878971,0.786831851089578,-333.133210631411)) ;
#31282 = CARTESIAN_POINT('Ctrl Pts',(19.4122320366345,0.708528569487368,-333.134165662925)) ;
#31283 = CARTESIAN_POINT('Ctrl Pts',(19.4169380638603,0.563550603007795,-333.13594416531)) ;
#31284 = CARTESIAN_POINT('Ctrl Pts',(19.4187585037866,0.496881468035375,-333.13676618588)) ;
#31285 = CARTESIAN_POINT('Ctrl Pts',(19.422452487332,0.330128079846534,-333.13883191478)) ;
#31286 = CARTESIAN_POINT('Ctrl Pts',(19.4238958101808,0.230036274229013,-333.140080445144)) ;
#31287 = CARTESIAN_POINT('Ctrl Pts',(19.4270698777963,-0.244458714760322,
-333.14603287715)) ;
#31288 = CARTESIAN_POINT('Ctrl Pts',(19.4187494218004,-0.618848962459257,
-333.150827319851)) ;
#31289 = CARTESIAN_POINT('Ctrl Pts',(19.3780453184075,-1.41424887511556,-333.161079880492)) ;
#31290 = CARTESIAN_POINT('Ctrl Pts',(19.3427456569787,-1.83491993450364,-333.166541354533)) ;
#31291 = CARTESIAN_POINT('Ctrl Pts',(19.2601708873612,-2.54170945163216,-333.175675757334)) ;
#31292 = CARTESIAN_POINT('Ctrl Pts',(19.2201434189485,-2.82852557794944,-333.179371529156)) ;
#31293 = CARTESIAN_POINT('Ctrl Pts',(19.1376070818677,-3.33666811908569,-333.185880055281)) ;
#31294 = CARTESIAN_POINT('Ctrl Pts',(19.0976305425937,-3.55835170827102,-333.188706267461)) ;
#31295 = CARTESIAN_POINT('Ctrl Pts',(19.0275956722537,-3.91144208003365,-333.193183707811)) ;
#31296 = CARTESIAN_POINT('Ctrl Pts',(19.0000093963871,-4.04331784664598,-333.194850640627)) ;
#31297 = CARTESIAN_POINT('Ctrl Pts',(18.9438480090212,-4.29851957321614,-333.198066286175)) ;
#31298 = CARTESIAN_POINT('Ctrl Pts',(18.9154348509784,-4.42187430369103,-333.199615979712)) ;
#31299 = CARTESIAN_POINT('Ctrl Pts',(18.8441201687388,-4.71821162476563,-333.203328665025)) ;
#31300 = CARTESIAN_POINT('Ctrl Pts',(18.8000397681945,-4.89089876322019,-333.205483748462)) ;
#31301 = CARTESIAN_POINT('Ctrl Pts',(18.5618979501145,-5.77299505741351,-333.216459641285)) ;
#31302 = CARTESIAN_POINT('Ctrl Pts',(18.3300361759063,-6.47157643830683,-333.225018562004)) ;
#31303 = CARTESIAN_POINT('Ctrl Pts',(17.9089230325428,-7.53441237786723,-333.238382301947)) ;
#31304 = CARTESIAN_POINT('Ctrl Pts',(17.7468226703079,-7.90867736604197,-333.243163215145)) ;
#31305 = CARTESIAN_POINT('Ctrl Pts',(17.522114550048,-8.38572730206592,-333.249486482239)) ;
#31306 = CARTESIAN_POINT('Ctrl Pts',(17.4701670450243,-8.49342004410461,-333.250929590514)) ;
#31307 = CARTESIAN_POINT('Ctrl Pts',(17.3861919973148,-8.66347889543662,-333.253238075894)) ;
#31308 = CARTESIAN_POINT('Ctrl Pts',(17.3548153459296,-8.72616313401462,-333.25409545113)) ;
#31309 = CARTESIAN_POINT('Ctrl Pts',(17.2947373336564,-8.8445811305174,-333.255728588559)) ;
#31310 = CARTESIAN_POINT('Ctrl Pts',(17.2661041365587,-8.90034846222215,-333.256503357367)) ;
#31311 = CARTESIAN_POINT('Ctrl Pts',(17.1834748891403,-9.05938159961081,-333.258727926446)) ;
#31312 = CARTESIAN_POINT('Ctrl Pts',(17.1288189211743,-9.16230137789719,-333.260185913156)) ;
#31313 = CARTESIAN_POINT('Ctrl Pts',(16.90332863112,-9.57783996479055,-333.266137820814)) ;
#31314 = CARTESIAN_POINT('Ctrl Pts',(16.7248356904525,-9.88622311924342,-333.27070483042)) ;
#31315 = CARTESIAN_POINT('Ctrl Pts',(16.484558840113,-10.2762011549869,-333.27660368282)) ;
#31316 = CARTESIAN_POINT('Ctrl Pts',(16.4304729180761,-10.3624586857424,-333.27791649911)) ;
#31317 = CARTESIAN_POINT('Ctrl Pts',(16.1236353937982,-10.8433684022128,-333.285275320516)) ;
#31318 = CARTESIAN_POINT('Ctrl Pts',(15.8573438776645,-11.2291986851869,-333.291325147242)) ;
#31319 = CARTESIAN_POINT('Ctrl Pts',(15.4908284405833,-11.7211704948601,-333.299141011212)) ;
#31320 = CARTESIAN_POINT('Ctrl Pts',(15.4030008387464,-11.8363494696315,-333.300978845954)) ;
#31321 = CARTESIAN_POINT('Ctrl Pts',(15.1813009182394,-12.120444598585,-333.305529407308)) ;
#31322 = CARTESIAN_POINT('Ctrl Pts',(15.0458898880883,-12.2881354381344,-333.308230978633)) ;
#31323 = CARTESIAN_POINT('Ctrl Pts',(14.8224643107209,-12.5555907606716,-333.312562959636)) ;
#31324 = CARTESIAN_POINT('Ctrl Pts',(14.7361665580548,-12.65676510103,-333.314207260307)) ;
#31325 = CARTESIAN_POINT('Ctrl Pts',(14.5660524821867,-12.8521060465932,-333.317393203597)) ;
#31326 = CARTESIAN_POINT('Ctrl Pts',(14.4823448536997,-12.9463586515116,-333.318935661738)) ;
#31327 = CARTESIAN_POINT('Ctrl Pts',(14.2947016590603,-13.1535426070349,-333.322338891705)) ;
#31328 = CARTESIAN_POINT('Ctrl Pts',(14.1903330704038,-13.2660704833762,-333.324195790675)) ;
#31329 = CARTESIAN_POINT('Ctrl Pts',(13.7594534229826,-13.7197317547138,-333.331722487689)) ;
#31330 = CARTESIAN_POINT('Ctrl Pts',(13.421888348565,-14.0501427902272,-333.337295314231)) ;
#31331 = CARTESIAN_POINT('Ctrl Pts',(12.7015345834842,-14.7055548048673,-333.348702412302)) ;
#31332 = CARTESIAN_POINT('Ctrl Pts',(12.317509887149,-15.0286816392346,-333.354526683944)) ;
#31333 = CARTESIAN_POINT('Ctrl Pts',(11.8240181317288,-15.4122819906828,-333.361899701347)) ;
#31334 = CARTESIAN_POINT('Ctrl Pts',(11.7259087475863,-15.487056044977,-333.363360570929)) ;
#31335 = CARTESIAN_POINT('Ctrl Pts',(11.5001026505558,-15.6557783104405,-333.366718420019)) ;
#31336 = CARTESIAN_POINT('Ctrl Pts',(11.3719547499849,-15.7491079274222,-333.368620831042)) ;
#31337 = CARTESIAN_POINT('Ctrl Pts',(11.1794869001049,-15.8857074864134,-333.371483458221)) ;
#31338 = CARTESIAN_POINT('Ctrl Pts',(11.116027001697,-15.9301780709183,-333.372428175945)) ;
#31339 = CARTESIAN_POINT('Ctrl Pts',(10.9972409608892,-16.0123639533652,-333.374199691141)) ;
#31340 = CARTESIAN_POINT('Ctrl Pts',(10.9419827254241,-16.0501751431529,-333.375025190049)) ;
#31341 = CARTESIAN_POINT('Ctrl Pts',(10.8021120515768,-16.1448254862809,-333.37711742042)) ;
#31342 = CARTESIAN_POINT('Ctrl Pts',(10.7172456875459,-16.2012857387479,-333.378389255005)) ;
#31343 = CARTESIAN_POINT('Ctrl Pts',(10.3246394516554,-16.4580456695274,-333.384276581815)) ;
#31344 = CARTESIAN_POINT('Ctrl Pts',(10.0117038658228,-16.6502622160299,-333.388977930046)) ;
#31345 = CARTESIAN_POINT('Ctrl Pts',(9.21641465754357,-17.108226793826,-333.400790599979)) ;
#31346 = CARTESIAN_POINT('Ctrl Pts',(8.72785441120039,-17.3625540304771,-333.407922750224)) ;
#31347 = CARTESIAN_POINT('Ctrl Pts',(8.02100651293836,-17.6931308867377,-333.417883994498)) ;
#31348 = CARTESIAN_POINT('Ctrl Pts',(7.81114898600246,-17.7867753631974,-333.420799568417)) ;
#31349 = CARTESIAN_POINT('Ctrl Pts',(7.42322370461186,-17.9516890171919,-333.42610525806)) ;
#31350 = CARTESIAN_POINT('Ctrl Pts',(7.24566690246012,-18.0240866632313,-333.42850221011)) ;
#31351 = CARTESIAN_POINT('Ctrl Pts',(6.94712249236005,-18.1406917051086,-333.432478913702)) ;
#31352 = CARTESIAN_POINT('Ctrl Pts',(6.82671479110414,-18.1863457482993,-333.434068452753)) ;
#31353 = CARTESIAN_POINT('Ctrl Pts',(6.5972197469767,-18.2707612514217,-333.437071326147)) ;
#31354 = CARTESIAN_POINT('Ctrl Pts',(6.48822241123192,-18.3097513657635,-333.438486180836)) ;
#31355 = CARTESIAN_POINT('Ctrl Pts',(6.19881025011907,-18.4103699602981,-333.442213941053)) ;
#31356 = CARTESIAN_POINT('Ctrl Pts',(6.0178254491308,-18.4703207229875,-333.444515410412)) ;
#31357 = CARTESIAN_POINT('Ctrl Pts',(5.25501892101676,-18.7105963011268,-333.454103335524)) ;
#31358 = CARTESIAN_POINT('Ctrl Pts',(4.6657639393848,-18.8661677606078,-333.461226575795)) ;
#31359 = CARTESIAN_POINT('Ctrl Pts',(3.71107003857639,-19.0707488819094,-333.472629833237)) ;
#31360 = CARTESIAN_POINT('Ctrl Pts',(3.34985446408966,-19.1375018783846,-333.47691651829)) ;
#31361 = CARTESIAN_POINT('Ctrl Pts',(2.84128348302247,-19.2166456540221,-333.483008777668)) ;
#31362 = CARTESIAN_POINT('Ctrl Pts',(2.69534889049852,-19.2376572454649,-333.484763668503)) ;
#31363 = CARTESIAN_POINT('Ctrl Pts',(2.43502184707032,-19.2721186238964,-333.487915387629)) ;
#31364 = CARTESIAN_POINT('Ctrl Pts',(2.32072221776043,-19.2862162172956,-333.489306460008)) ;
#31365 = CARTESIAN_POINT('Ctrl Pts',(2.13750616189181,-19.3071615580235,-333.491552181983)) ;
#31366 = CARTESIAN_POINT('Ctrl Pts',(2.0686666245353,-19.3146586409899,-333.492399561775)) ;
#31367 = CARTESIAN_POINT('Ctrl Pts',(1.93665750548425,-19.3283214718026,-333.494032544694)) ;
#31368 = CARTESIAN_POINT('Ctrl Pts',(1.8734949467549,-19.3345460221858,-333.494817329822)) ;
#31369 = CARTESIAN_POINT('Ctrl Pts',(1.68990157678104,-19.3517307026508,-333.497107314673)) ;
#31370 = CARTESIAN_POINT('Ctrl Pts',(1.56939759749294,-19.3618759329444,-333.498621437269)) ;
#31371 = CARTESIAN_POINT('Ctrl Pts',(0.966876196038792,-19.4069403018975,
-333.506234317399)) ;
#31372 = CARTESIAN_POINT('Ctrl Pts',(0.483768668098201,-19.42498772913,-333.512469026684)) ;
#31373 = CARTESIAN_POINT('Ctrl Pts',(0.000492969417159733,-19.4249999937447,
-333.518704187163)) ;
#31374 = CARTESIAN_POINT('Origin',(0.,0.,-328.125)) ;
#31375 = CARTESIAN_POINT('',(-0.000504255346276296,-19.424999993455,-335.231156847152)) ;
#31376 = CARTESIAN_POINT('',(-0.000488271649964467,-19.425000024638,-335.01863418612)) ;
#31377 = CARTESIAN_POINT('',(-2.37887640734373E-15,-19.425,-328.125)) ;
#31378 = CARTESIAN_POINT('Ctrl Pts',(-0.000504255346276296,-19.424999993455,
-335.231156847152)) ;
#31379 = CARTESIAN_POINT('Ctrl Pts',(0.401697001557673,-19.4250104342341,
-335.226213897056)) ;
#31380 = CARTESIAN_POINT('Ctrl Pts',(0.803933718099742,-19.4125249605364,
-335.22127094696)) ;
#31381 = CARTESIAN_POINT('Ctrl Pts',(1.20541431535202,-19.3875630580108,-335.216327996863)) ;
#31382 = CARTESIAN_POINT('Ctrl Pts',(1.60686285129883,-19.3626031488845,-335.2113854415)) ;
#31383 = CARTESIAN_POINT('Ctrl Pts',(2.00755514881831,-19.3251688159696,-335.206442886136)) ;
#31384 = CARTESIAN_POINT('Ctrl Pts',(2.40670260443344,-19.2753315814233,-335.201500330772)) ;
#31385 = CARTESIAN_POINT('Ctrl Pts',(2.80884240561074,-19.2251207249848,-335.19652072185)) ;
#31386 = CARTESIAN_POINT('Ctrl Pts',(3.209413862284,-19.1623202687843,-335.191541112928)) ;
#31387 = CARTESIAN_POINT('Ctrl Pts',(3.60761705354232,-19.0870564570599,-335.186561504006)) ;
#31388 = CARTESIAN_POINT('Ctrl Pts',(4.00289111256762,-19.0123462764005,-335.181618524456)) ;
#31389 = CARTESIAN_POINT('Ctrl Pts',(4.39583139329134,-18.9253555340871,-335.176675544907)) ;
#31390 = CARTESIAN_POINT('Ctrl Pts',(4.78566548879298,-18.8262590768686,-335.171732565357)) ;
#31391 = CARTESIAN_POINT('Ctrl Pts',(5.1798328143229,-18.7260611055724,-335.166734641749)) ;
#31392 = CARTESIAN_POINT('Ctrl Pts',(5.5708242503035,-18.6134867699796,-335.16173671814)) ;
#31393 = CARTESIAN_POINT('Ctrl Pts',(5.95785535789883,-18.4887691460074,-335.156738794532)) ;
#31394 = CARTESIAN_POINT('Ctrl Pts',(6.34488646549424,-18.3640515220352,-335.151740870923)) ;
#31395 = CARTESIAN_POINT('Ctrl Pts',(6.72795700563771,-18.2271906946848,-335.146742947315)) ;
#31396 = CARTESIAN_POINT('Ctrl Pts',(7.10630024801675,-18.0784712236693,-335.141745023707)) ;
#31397 = CARTESIAN_POINT('Ctrl Pts',(7.48194286066495,-17.9308133183961,-335.136782775484)) ;
#31398 = CARTESIAN_POINT('Ctrl Pts',(7.85303165451542,-17.7714238280823,-335.131820527261)) ;
#31399 = CARTESIAN_POINT('Ctrl Pts',(8.21883012953624,-17.600609543474,-335.126858279038)) ;
#31400 = CARTESIAN_POINT('Ctrl Pts',(8.58435151182593,-17.4299246508666,-335.121899789724)) ;
#31401 = CARTESIAN_POINT('Ctrl Pts',(8.94459037186042,-17.2478323664877,-335.116941300409)) ;
#31402 = CARTESIAN_POINT('Ctrl Pts',(9.29883308421554,-17.0546864020391,-335.111982811095)) ;
#31403 = CARTESIAN_POINT('Ctrl Pts',(9.65303778078999,-16.8615611651719,-335.107024853904)) ;
#31404 = CARTESIAN_POINT('Ctrl Pts',(10.0012474066032,-16.6573847311153,-335.102066896713)) ;
#31405 = CARTESIAN_POINT('Ctrl Pts',(10.3427729638405,-16.4425567482205,-335.097108939522)) ;
#31406 = CARTESIAN_POINT('Ctrl Pts',(10.6842777656993,-16.2277418209696,-335.092151283638)) ;
#31407 = CARTESIAN_POINT('Ctrl Pts',(11.0190991096253,-16.0022767644142,-335.087193627755)) ;
#31408 = CARTESIAN_POINT('Ctrl Pts',(11.346575608599,-15.7666054354876,-335.082235971871)) ;
#31409 = CARTESIAN_POINT('Ctrl Pts',(11.6745642237066,-15.5305655577025,-335.077270563079)) ;
#31410 = CARTESIAN_POINT('Ctrl Pts',(11.9951848021529,-15.2842875892346,-335.072305154286)) ;
#31411 = CARTESIAN_POINT('Ctrl Pts',(12.3078034626076,-15.0282600099221,-335.067339745493)) ;
#31412 = CARTESIAN_POINT('Ctrl Pts',(12.6199660245349,-14.7726059649396,-335.06238158104)) ;
#31413 = CARTESIAN_POINT('Ctrl Pts',(12.9241498258517,-14.5072308991849,-335.057423416587)) ;
#31414 = CARTESIAN_POINT('Ctrl Pts',(13.2197570537452,-14.2326613266793,-335.052465252133)) ;
#31415 = CARTESIAN_POINT('Ctrl Pts',(13.5160121461063,-13.957489996662,-335.047496221171)) ;
#31416 = CARTESIAN_POINT('Ctrl Pts',(13.8036528449718,-13.6730839657378,-335.042527190209)) ;
#31417 = CARTESIAN_POINT('Ctrl Pts',(14.0821136007754,-13.380011268114,-335.037558159247)) ;
#31418 = CARTESIAN_POINT('Ctrl Pts',(14.3605743565788,-13.0869385704903,-335.032589128284)) ;
#31419 = CARTESIAN_POINT('Ctrl Pts',(14.6298550090504,-12.7851993845068,-335.027620097322)) ;
#31420 = CARTESIAN_POINT('Ctrl Pts',(14.8894287474079,-12.4753972512247,-335.02265106636)) ;
#31421 = CARTESIAN_POINT('Ctrl Pts',(15.148648166975,-12.1660179986153,-335.017688818137)) ;
#31422 = CARTESIAN_POINT('Ctrl Pts',(15.3982560705094,-11.8485155623468,-335.012726569915)) ;
#31423 = CARTESIAN_POINT('Ctrl Pts',(15.6377524923644,-11.5235117037972,-335.007764321692)) ;
#31424 = CARTESIAN_POINT('Ctrl Pts',(15.8770674954108,-11.1987540360355,-335.002805832378)) ;
#31425 = CARTESIAN_POINT('Ctrl Pts',(16.1062861889675,-10.8665064975775,-334.997847343064)) ;
#31426 = CARTESIAN_POINT('Ctrl Pts',(16.3249511423696,-10.5274211086688,-334.992888853749)) ;
#31427 = CARTESIAN_POINT('Ctrl Pts',(16.5435926296039,-10.1883721089232,-334.987930896559)) ;
#31428 = CARTESIAN_POINT('Ctrl Pts',(16.7516825102272,-9.84248692379159,-334.982972939368)) ;
#31429 = CARTESIAN_POINT('Ctrl Pts',(16.9488069570013,-9.49044612936103,-334.978014982177)) ;
#31430 = CARTESIAN_POINT('Ctrl Pts',(17.1459194240202,-9.13842672934713,-334.973057326295)) ;
#31431 = CARTESIAN_POINT('Ctrl Pts',(17.3320676725531,-8.78025267442093,-334.968099670412)) ;
#31432 = CARTESIAN_POINT('Ctrl Pts',(17.5068832716601,-8.41663015181654,-334.963142014529)) ;
#31433 = CARTESIAN_POINT('Ctrl Pts',(17.681972251898,-8.0524389869573,-334.958176605736)) ;
#31434 = CARTESIAN_POINT('Ctrl Pts',(17.8456929947439,-7.68278250932546,-334.953211196943)) ;
#31435 = CARTESIAN_POINT('Ctrl Pts',(17.9977225714819,-7.30839293141586,-334.94824578815)) ;
#31436 = CARTESIAN_POINT('Ctrl Pts',(18.1495303429329,-6.93454957345618,-334.943287623697)) ;
#31437 = CARTESIAN_POINT('Ctrl Pts',(18.2896809616296,-6.555987141927,-334.938329459244)) ;
#31438 = CARTESIAN_POINT('Ctrl Pts',(18.4179013681401,-6.17345399217179,-334.933371294792)) ;
#31439 = CARTESIAN_POINT('Ctrl Pts',(18.5464027875771,-5.79008246759955,-334.928402263829)) ;
#31440 = CARTESIAN_POINT('Ctrl Pts',(18.6629215540654,-5.40272302320347,-334.923433232866)) ;
#31441 = CARTESIAN_POINT('Ctrl Pts',(18.7672328037281,-5.0121450388703,-334.918464201903)) ;
#31442 = CARTESIAN_POINT('Ctrl Pts',(18.8715440533908,-4.62156705453713,-334.913495170941)) ;
#31443 = CARTESIAN_POINT('Ctrl Pts',(18.9636477308124,-4.22777076354923,-334.908526139978)) ;
#31444 = CARTESIAN_POINT('Ctrl Pts',(19.0433699771015,-3.83153819180081,-334.903557109015)) ;
#31445 = CARTESIAN_POINT('Ctrl Pts',(19.1229834023199,-3.43584647852945,-334.898594860793)) ;
#31446 = CARTESIAN_POINT('Ctrl Pts',(19.1902703496577,-3.03761994844676,-334.89363261257)) ;
#31447 = CARTESIAN_POINT('Ctrl Pts',(19.2450892507532,-2.63764378386144,-334.888670364347)) ;
#31448 = CARTESIAN_POINT('Ctrl Pts',(19.2998666264733,-2.23797060164256,-334.883711875033)) ;
#31449 = CARTESIAN_POINT('Ctrl Pts',(19.3421948056454,-1.83655066995297,-334.878753385718)) ;
#31450 = CARTESIAN_POINT('Ctrl Pts',(19.3719840476789,-1.43417539250789,-334.873794896404)) ;
#31451 = CARTESIAN_POINT('Ctrl Pts',(19.4017700928612,-1.03184329621813,-334.868836939213)) ;
#31452 = CARTESIAN_POINT('Ctrl Pts',(19.4190198710382,-0.628556295574683,
-334.863878982022)) ;
#31453 = CARTESIAN_POINT('Ctrl Pts',(19.4236955928532,-0.225110009052542,
-334.858921024831)) ;
#31454 = CARTESIAN_POINT('Ctrl Pts',(19.4283710305126,0.178311759007074,-334.853963368947)) ;
#31455 = CARTESIAN_POINT('Ctrl Pts',(19.4204739356573,0.5818925563304,-334.849005713064)) ;
#31456 = CARTESIAN_POINT('Ctrl Pts',(19.4000186357227,0.984835993256649,-334.84404805718)) ;
#31457 = CARTESIAN_POINT('Ctrl Pts',(19.3795313472662,1.38840956344723,-334.839082648388)) ;
#31458 = CARTESIAN_POINT('Ctrl Pts',(19.3464465438132,1.79134353924963,-334.834117239595)) ;
#31459 = CARTESIAN_POINT('Ctrl Pts',(19.3008309607296,2.19284044685003,-334.829151830803)) ;
#31460 = CARTESIAN_POINT('Ctrl Pts',(19.2552819290164,2.59375158599994,-334.824193666349)) ;
#31461 = CARTESIAN_POINT('Ctrl Pts',(19.1972386964926,2.99322961251154,-334.819235501896)) ;
#31462 = CARTESIAN_POINT('Ctrl Pts',(19.1268195133082,3.39048673575542,-334.814277337443)) ;
#31463 = CARTESIAN_POINT('Ctrl Pts',(19.0562459966626,3.78861450338956,-334.80930830648)) ;
#31464 = CARTESIAN_POINT('Ctrl Pts',(18.9732422499562,4.18451138403192,-334.804339275518)) ;
#31465 = CARTESIAN_POINT('Ctrl Pts',(18.8779789038953,4.57739418272927,-334.799370244556)) ;
#31466 = CARTESIAN_POINT('Ctrl Pts',(18.7827155578344,4.97027698142663,-334.794401213594)) ;
#31467 = CARTESIAN_POINT('Ctrl Pts',(18.6751926753652,5.36014546681486,-334.789432182632)) ;
#31468 = CARTESIAN_POINT('Ctrl Pts',(18.5556317262961,5.74622974114971,-334.784463151669)) ;
#31469 = CARTESIAN_POINT('Ctrl Pts',(18.4362339782159,6.13178700950241,-334.779500903447)) ;
#31470 = CARTESIAN_POINT('Ctrl Pts',(18.304799277508,6.51367288511617,-334.774538655224)) ;
#31471 = CARTESIAN_POINT('Ctrl Pts',(18.1615789593283,6.89113014708642,-334.769576407001)) ;
#31472 = CARTESIAN_POINT('Ctrl Pts',(18.0184671306969,7.26830148476646,-334.764617917687)) ;
#31473 = CARTESIAN_POINT('Ctrl Pts',(17.8635876173225,7.64105069352826,-334.759659428373)) ;
#31474 = CARTESIAN_POINT('Ctrl Pts',(17.6972402422889,8.00863988494365,-334.754700939059)) ;
#31475 = CARTESIAN_POINT('Ctrl Pts',(17.5309107189271,8.3761896282968,-334.749742981868)) ;
#31476 = CARTESIAN_POINT('Ctrl Pts',(17.3531158898041,8.73858024415288,-334.744785024677)) ;
#31477 = CARTESIAN_POINT('Ctrl Pts',(17.1642032143184,9.09509499772164,-334.739827067486)) ;
#31478 = CARTESIAN_POINT('Ctrl Pts',(16.9753020195385,9.45158808497829,-334.734869411603)) ;
#31479 = CARTESIAN_POINT('Ctrl Pts',(16.7752844393008,9.80220581365237,-334.72991175572)) ;
#31480 = CARTESIAN_POINT('Ctrl Pts',(16.5645440672102,10.1462557057,-334.724954099837)) ;
#31481 = CARTESIAN_POINT('Ctrl Pts',(16.3534741339166,10.4908436317998,-334.719988691044)) ;
#31482 = CARTESIAN_POINT('Ctrl Pts',(16.1316479583973,10.8288429527156,-334.715023282251)) ;
#31483 = CARTESIAN_POINT('Ctrl Pts',(15.899505673852,11.1595853116121,-334.710057873459)) ;
#31484 = CARTESIAN_POINT('Ctrl Pts',(15.6677020759331,11.4898451301822,-334.705099709006)) ;
#31485 = CARTESIAN_POINT('Ctrl Pts',(15.4256125974639,11.8128689604294,-334.700141544553)) ;
#31486 = CARTESIAN_POINT('Ctrl Pts',(15.173717975584,12.1280215945322,-334.6951833801)) ;
#31487 = CARTESIAN_POINT('Ctrl Pts',(14.9212712914812,12.4438649296211,-334.690214349137)) ;
#31488 = CARTESIAN_POINT('Ctrl Pts',(14.6589765761222,12.7518023329777,-334.685245318175)) ;
#31489 = CARTESIAN_POINT('Ctrl Pts',(14.3873583648343,13.0512276925136,-334.680276287212)) ;
#31490 = CARTESIAN_POINT('Ctrl Pts',(14.1157401535463,13.3506530520495,-334.67530725625)) ;
#31491 = CARTESIAN_POINT('Ctrl Pts',(13.8347986122943,13.6415661947121,-334.670338225287)) ;
#31492 = CARTESIAN_POINT('Ctrl Pts',(13.5450965579716,13.9233970077429,-334.665369194325)) ;
#31493 = CARTESIAN_POINT('Ctrl Pts',(13.255789947683,14.2048431210039,-334.660406946102)) ;
#31494 = CARTESIAN_POINT('Ctrl Pts',(12.9576698274976,14.4773065065886,-334.655444697879)) ;
#31495 = CARTESIAN_POINT('Ctrl Pts',(12.6513191750186,14.7402424719476,-334.650482449656)) ;
#31496 = CARTESIAN_POINT('Ctrl Pts',(12.3452005834881,15.0029792630302,-334.645523960342)) ;
#31497 = CARTESIAN_POINT('Ctrl Pts',(12.0308641044568,15.2562029077659,-334.640565471028)) ;
#31498 = CARTESIAN_POINT('Ctrl Pts',(11.7089260450411,15.4994088878176,-334.635606981713)) ;
#31499 = CARTESIAN_POINT('Ctrl Pts',(11.3870225346129,15.7425887680648,-334.630649024522)) ;
#31500 = CARTESIAN_POINT('Ctrl Pts',(11.0575192624823,15.9757529878346,-334.625691067331)) ;
#31501 = CARTESIAN_POINT('Ctrl Pts',(10.7210642461646,16.198438394784,-334.62073311014)) ;
#31502 = CARTESIAN_POINT('Ctrl Pts',(10.3846296770743,16.4211102685745,-334.615775454257)) ;
#31503 = CARTESIAN_POINT('Ctrl Pts',(10.0412444056747,16.6333044707947,-334.610817798374)) ;
#31504 = CARTESIAN_POINT('Ctrl Pts',(9.69158535623311,16.8346012213788,-334.60586014249)) ;
#31505 = CARTESIAN_POINT('Ctrl Pts',(9.34137950100503,17.0362127649825,-334.600894733698)) ;
#31506 = CARTESIAN_POINT('Ctrl Pts',(8.98488043018721,17.2268926160082,-334.595929324905)) ;
#31507 = CARTESIAN_POINT('Ctrl Pts',(8.62279439562653,17.4062644415955,-334.590963916112)) ;
#31508 = CARTESIAN_POINT('Ctrl Pts',(8.261236630593,17.5853745706233,-334.586005751659)) ;
#31509 = CARTESIAN_POINT('Ctrl Pts',(7.8941084119804,17.7532095538587,-334.581047587206)) ;
#31510 = CARTESIAN_POINT('Ctrl Pts',(7.52213578782325,17.9094415934598,-334.576089422753)) ;
#31511 = CARTESIAN_POINT('Ctrl Pts',(7.14934793375844,18.066016037375,-334.57112039179)) ;
#31512 = CARTESIAN_POINT('Ctrl Pts',(6.77169463145451,18.2109365167461,-334.566151360828)) ;
#31513 = CARTESIAN_POINT('Ctrl Pts',(6.38992646928316,18.3439217376534,-334.561182329866)) ;
#31514 = CARTESIAN_POINT('Ctrl Pts',(6.0081583071118,18.4769069585608,-334.556213298903)) ;
#31515 = CARTESIAN_POINT('Ctrl Pts',(5.62227551360419,18.5979568484436,-334.551244267941)) ;
#31516 = CARTESIAN_POINT('Ctrl Pts',(5.23304507031604,18.7068400402644,-334.546275236979)) ;
#31517 = CARTESIAN_POINT('Ctrl Pts',(4.84434592755306,18.8155746062571,-334.541312988756)) ;
#31518 = CARTESIAN_POINT('Ctrl Pts',(4.45220494496474,18.9122045825489,-334.536350740533)) ;
#31519 = CARTESIAN_POINT('Ctrl Pts',(4.057394646156,18.9965305696947,-334.53138849231)) ;
#31520 = CARTESIAN_POINT('Ctrl Pts',(3.66288341657788,19.0807926798135,-334.526430002996)) ;
#31521 = CARTESIAN_POINT('Ctrl Pts',(3.26570714556296,19.1527693846673,-334.521471513682)) ;
#31522 = CARTESIAN_POINT('Ctrl Pts',(2.86664840399438,19.212312508594,-334.516513024367)) ;
#31523 = CARTESIAN_POINT('Ctrl Pts',(2.46763248766517,19.2718492426129,-334.511555067177)) ;
#31524 = CARTESIAN_POINT('Ctrl Pts',(2.06673473895779,19.3189550257579,-334.506597109986)) ;
#31525 = CARTESIAN_POINT('Ctrl Pts',(1.66474578406556,19.3535331780643,-334.501639152795)) ;
#31526 = CARTESIAN_POINT('Ctrl Pts',(1.26278125907246,19.3881092289677,-334.496681496912)) ;
#31527 = CARTESIAN_POINT('Ctrl Pts',(0.85972589679546,19.4101591496573,-334.491723841029)) ;
#31528 = CARTESIAN_POINT('Ctrl Pts',(0.456374956919836,19.4196381763074,-334.486766185145)) ;
#31529 = CARTESIAN_POINT('Ctrl Pts',(0.052393246489807,19.4291320265028,-334.481800776353)) ;
#31530 = CARTESIAN_POINT('Ctrl Pts',(-0.351884728504625,19.4260156153053,
-334.47683536756)) ;
#31531 = CARTESIAN_POINT('Ctrl Pts',(-0.755658741192586,19.4102963621594,
-334.471869958768)) ;
#31532 = CARTESIAN_POINT('Ctrl Pts',(-1.15884366319998,19.3946000427964,-334.466911794314)) ;
#31533 = CARTESIAN_POINT('Ctrl Pts',(-1.5615258552778,19.3663376529126,-334.461953629861)) ;
#31534 = CARTESIAN_POINT('Ctrl Pts',(-1.96291092729285,19.325568702926,-334.456995465408)) ;
#31535 = CARTESIAN_POINT('Ctrl Pts',(-2.36517569070632,19.2847104020963,-334.452026434446)) ;
#31536 = CARTESIAN_POINT('Ctrl Pts',(-2.76613740260173,19.2312906708978,-334.447057403483)) ;
#31537 = CARTESIAN_POINT('Ctrl Pts',(-3.16500237188338,19.1654215968753,-334.442088372521)) ;
#31538 = CARTESIAN_POINT('Ctrl Pts',(-3.56386734116495,19.0995525228527,-334.437119341558)) ;
#31539 = CARTESIAN_POINT('Ctrl Pts',(-3.96063533243817,19.0212341516236,-334.432150310596)) ;
#31540 = CARTESIAN_POINT('Ctrl Pts',(-4.35452214552194,18.930630255862,-334.427181279634)) ;
#31541 = CARTESIAN_POINT('Ctrl Pts',(-4.74787130211817,18.8401500346454,-334.422219031411)) ;
#31542 = CARTESIAN_POINT('Ctrl Pts',(-5.13845170566674,18.7373937652141,-334.417256783188)) ;
#31543 = CARTESIAN_POINT('Ctrl Pts',(-5.52548958343109,18.6225559433552,-334.412294534965)) ;
#31544 = CARTESIAN_POINT('Ctrl Pts',(-5.9122342795839,18.5078051112707,-334.407336045651)) ;
#31545 = CARTESIAN_POINT('Ctrl Pts',(-6.29544158712495,18.3809910909594,-334.402377556337)) ;
#31546 = CARTESIAN_POINT('Ctrl Pts',(-6.67435341722363,18.2423581661471,-334.397419067022)) ;
#31547 = CARTESIAN_POINT('Ctrl Pts',(-7.05322458416268,18.1037401188138,-334.392461109831)) ;
#31548 = CARTESIAN_POINT('Ctrl Pts',(-7.42780097154076,17.9533057818234,-334.38750315264)) ;
#31549 = CARTESIAN_POINT('Ctrl Pts',(-7.79734205372781,17.7913485126105,-334.382545195449)) ;
#31550 = CARTESIAN_POINT('Ctrl Pts',(-8.16686067795821,17.6294010859551,-334.377587539566)) ;
#31551 = CARTESIAN_POINT('Ctrl Pts',(-8.53134439099051,17.4559322213099,-334.372629883683)) ;
#31552 = CARTESIAN_POINT('Ctrl Pts',(-8.89007343634173,17.2712830819384,-334.3676722278)) ;
#31553 = CARTESIAN_POINT('Ctrl Pts',(-9.24936347137597,17.0863451835062,-334.362706819007)) ;
#31554 = CARTESIAN_POINT('Ctrl Pts',(-9.60288060766997,16.8901921120831,-334.357741410214)) ;
#31555 = CARTESIAN_POINT('Ctrl Pts',(-9.94992569266374,16.6832132309837,-334.352776001422)) ;
#31556 = CARTESIAN_POINT('Ctrl Pts',(-10.2964644522903,16.476536324073,-334.347817836968)) ;
#31557 = CARTESIAN_POINT('Ctrl Pts',(-10.6365498351517,16.2590653079337,-334.342859672515)) ;
#31558 = CARTESIAN_POINT('Ctrl Pts',(-10.9695127356894,16.0312324960231,-334.337901508062)) ;
#31559 = CARTESIAN_POINT('Ctrl Pts',(-11.3032053708883,15.8029003567114,-334.3329324771)) ;
#31560 = CARTESIAN_POINT('Ctrl Pts',(-11.6297440639063,15.5641610762247,-334.327963446137)) ;
#31561 = CARTESIAN_POINT('Ctrl Pts',(-11.948485477212,15.3154928030688,-334.322994415175)) ;
#31562 = CARTESIAN_POINT('Ctrl Pts',(-12.2672268905179,15.0668245299129,-334.318025384212)) ;
#31563 = CARTESIAN_POINT('Ctrl Pts',(-12.5781708392292,14.8082274167643,-334.31305635325)) ;
#31564 = CARTESIAN_POINT('Ctrl Pts',(-12.8807070474881,14.5402204576406,-334.308087322288)) ;
#31565 = CARTESIAN_POINT('Ctrl Pts',(-13.182830293066,14.2725793286865,-334.303125074065)) ;
#31566 = CARTESIAN_POINT('Ctrl Pts',(-13.47664905564,13.9954828882491,-334.298162825842)) ;
#31567 = CARTESIAN_POINT('Ctrl Pts',(-13.7615769146786,13.7094721204496,-334.293200577619)) ;
#31568 = CARTESIAN_POINT('Ctrl Pts',(-14.0462889405564,13.4236780061156,-334.288242088305)) ;
#31569 = CARTESIAN_POINT('Ctrl Pts',(-14.3221233598798,13.1289832328028,-334.283283598991)) ;
#31570 = CARTESIAN_POINT('Ctrl Pts',(-14.5885313443723,12.8259650012881,-334.278325109676)) ;
#31571 = CARTESIAN_POINT('Ctrl Pts',(-14.854910739124,12.5229792883659,-334.273367152485)) ;
#31572 = CARTESIAN_POINT('Ctrl Pts',(-15.1118655628799,12.2116720795278,-334.268409195295)) ;
#31573 = CARTESIAN_POINT('Ctrl Pts',(-15.3588858881755,11.8926552659196,-334.263451238104)) ;
#31574 = CARTESIAN_POINT('Ctrl Pts',(-15.6058912014136,11.5736578397797,-334.25849358222)) ;
#31575 = CARTESIAN_POINT('Ctrl Pts',(-15.8429630770454,11.2469519325026,-334.253535926337)) ;
#31576 = CARTESIAN_POINT('Ctrl Pts',(-16.0696326970679,10.9131814784382,-334.248578270454)) ;
#31577 = CARTESIAN_POINT('Ctrl Pts',(-16.2966567888581,10.5788890655738,-334.243612861662)) ;
#31578 = CARTESIAN_POINT('Ctrl Pts',(-16.5132459196395,10.2375101829376,-334.238647452869)) ;
#31579 = CARTESIAN_POINT('Ctrl Pts',(-16.7189724243879,9.88972123330872,-334.233682044076)) ;
#31580 = CARTESIAN_POINT('Ctrl Pts',(-16.924398782118,9.54243969431409,-334.228723879623)) ;
#31581 = CARTESIAN_POINT('Ctrl Pts',(-17.1189940787293,9.18876699104686,-334.22376571517)) ;
#31582 = CARTESIAN_POINT('Ctrl Pts',(-17.3023775827306,8.82940286682075,-334.218807550717)) ;
#31583 = CARTESIAN_POINT('Ctrl Pts',(-17.4861629972697,8.46925114597181,-334.213838519754)) ;
#31584 = CARTESIAN_POINT('Ctrl Pts',(-17.6586872990454,8.10338323622678,-334.208869488792)) ;
#31585 = CARTESIAN_POINT('Ctrl Pts',(-17.8196143128186,7.73252680191873,-334.20390045783)) ;
#31586 = CARTESIAN_POINT('Ctrl Pts',(-17.9805413265917,7.36167036761077,-334.198931426867)) ;
#31587 = CARTESIAN_POINT('Ctrl Pts',(-18.1298709630558,6.98582563126151,-334.193962395905)) ;
#31588 = CARTESIAN_POINT('Ctrl Pts',(-18.2673156208678,6.60574030730857,-334.188993364943)) ;
#31589 = CARTESIAN_POINT('Ctrl Pts',(-18.4045726663784,6.22617380077244,-334.18403111672)) ;
#31590 = CARTESIAN_POINT('Ctrl Pts',(-18.5300136547585,5.84227738117756,-334.179068868497)) ;
#31591 = CARTESIAN_POINT('Ctrl Pts',(-18.6433824533151,5.45480666013219,-334.174106620274)) ;
#31592 = CARTESIAN_POINT('Ctrl Pts',(-18.7566653748843,5.06762944857674,-334.16914813096)) ;
#31593 = CARTESIAN_POINT('Ctrl Pts',(-18.8578943223797,4.67688357657028,-334.164189641646)) ;
#31594 = CARTESIAN_POINT('Ctrl Pts',(-18.9468635008799,4.28333847355357,-334.159231152331)) ;
#31595 = CARTESIAN_POINT('Ctrl Pts',(-19.0358231315961,3.88983560408043,-334.15427319514)) ;
#31596 = CARTESIAN_POINT('Ctrl Pts',(-19.1125255688101,3.49353433503265,-334.149315237949)) ;
#31597 = CARTESIAN_POINT('Ctrl Pts',(-19.1768157742415,3.09521594736152,-334.144357280758)) ;
#31598 = CARTESIAN_POINT('Ctrl Pts',(-19.2411020725932,2.69692176651476,-334.139399624875)) ;
#31599 = CARTESIAN_POINT('Ctrl Pts',(-19.2929776083019,2.29661094620041,-334.134441968992)) ;
#31600 = CARTESIAN_POINT('Ctrl Pts',(-19.3323387727382,1.89507323765717,-334.129484313109)) ;
#31601 = CARTESIAN_POINT('Ctrl Pts',(-19.3717614911733,1.49290759414245,-334.124518904316)) ;
#31602 = CARTESIAN_POINT('Ctrl Pts',(-19.3986306302936,1.08951145825837,-334.119553495523)) ;
#31603 = CARTESIAN_POINT('Ctrl Pts',(-19.4128942527724,0.685683404113655,
-334.114588086731)) ;
#31604 = CARTESIAN_POINT('Ctrl Pts',(-19.4271370651773,0.282444519490505,
-334.109629922277)) ;
#31605 = CARTESIAN_POINT('Ctrl Pts',(-19.4288111225219,-0.121224785798165,
-334.104671757824)) ;
#31606 = CARTESIAN_POINT('Ctrl Pts',(-19.4179168678447,-0.524527895798856,
-334.099713593371)) ;
#31607 = CARTESIAN_POINT('Ctrl Pts',(-19.4069987368883,-0.928714900840813,
-334.094744562408)) ;
#31608 = CARTESIAN_POINT('Ctrl Pts',(-19.3834571348805,-1.33253386406551,
-334.089775531446)) ;
#31609 = CARTESIAN_POINT('Ctrl Pts',(-19.3473449890827,-1.73518496807009,
-334.084806500484)) ;
#31610 = CARTESIAN_POINT('Ctrl Pts',(-19.3112328432849,-2.13783607207458,
-334.079837469521)) ;
#31611 = CARTESIAN_POINT('Ctrl Pts',(-19.2625501817346,-2.53931907872982,
-334.074868438559)) ;
#31612 = CARTESIAN_POINT('Ctrl Pts',(-19.2014021782866,-2.93883980299876,
-334.069899407596)) ;
#31613 = CARTESIAN_POINT('Ctrl Pts',(-19.1403376420162,-3.33781518048016,
-334.064937159373)) ;
#31614 = CARTESIAN_POINT('Ctrl Pts',(-19.066825550336,-3.73493968856343,-334.059974911151)) ;
#31615 = CARTESIAN_POINT('Ctrl Pts',(-18.9810024888263,-4.12942726285024,
-334.055012662928)) ;
#31616 = CARTESIAN_POINT('Ctrl Pts',(-18.8952444383777,-4.5236160123761,-334.050054173613)) ;
#31617 = CARTESIAN_POINT('Ctrl Pts',(-18.7971941126643,-4.91517158944148,
-334.045095684299)) ;
#31618 = CARTESIAN_POINT('Ctrl Pts',(-18.6870389110983,-5.30331987863233,
-334.040137194985)) ;
#31619 = CARTESIAN_POINT('Ctrl Pts',(-18.5768955309073,-5.69142651344479,
-334.035179237794)) ;
#31620 = CARTESIAN_POINT('Ctrl Pts',(-18.4546499342569,-6.07612636245392,
-334.030221280603)) ;
#31621 = CARTESIAN_POINT('Ctrl Pts',(-18.3205397614761,-6.456659186311,-334.025263323412)) ;
#31622 = CARTESIAN_POINT('Ctrl Pts',(-18.1864377389124,-6.83716888421797,
-334.020305667528)) ;
#31623 = CARTESIAN_POINT('Ctrl Pts',(-18.0404726595519,-7.21351183908467,
-334.015348011645)) ;
#31624 = CARTESIAN_POINT('Ctrl Pts',(-17.8829313779694,-7.58494497876132,
-334.010390355762)) ;
#31625 = CARTESIAN_POINT('Ctrl Pts',(-17.7251437292923,-7.9569589751034,-334.005424946969)) ;
#31626 = CARTESIAN_POINT('Ctrl Pts',(-17.5557437243768,-8.32404756306942,
-334.000459538177)) ;
#31627 = CARTESIAN_POINT('Ctrl Pts',(-17.37506781293,-8.68548464370782,-333.995494129384)) ;
#31628 = CARTESIAN_POINT('Ctrl Pts',(-17.1946555006545,-9.04639440161577,
-333.990535964931)) ;
#31629 = CARTESIAN_POINT('Ctrl Pts',(-17.0030002797343,-9.40166892475343,
-333.985577800478)) ;
#31630 = CARTESIAN_POINT('Ctrl Pts',(-16.8004836597507,-9.75060889372814,
-333.980619636025)) ;
#31631 = CARTESIAN_POINT('Ctrl Pts',(-16.5975231963353,-10.1003136133358,
-333.975650605062)) ;
#31632 = CARTESIAN_POINT('Ctrl Pts',(-16.3836537805527,-10.4436557678626,
-333.9706815741)) ;
#31633 = CARTESIAN_POINT('Ctrl Pts',(-16.1593045415395,-10.7799583363657,
-333.965712543137)) ;
#31634 = CARTESIAN_POINT('Ctrl Pts',(-15.9349553025264,-11.1162609048688,
-333.960743512175)) ;
#31635 = CARTESIAN_POINT('Ctrl Pts',(-15.7001263788299,-11.4455236916539,
-333.955774481213)) ;
#31636 = CARTESIAN_POINT('Ctrl Pts',(-15.4552900841601,-11.7670996177675,
-333.95080545025)) ;
#31637 = CARTESIAN_POINT('Ctrl Pts',(-15.2107879916426,-12.0882365919404,
-333.945843202028)) ;
#31638 = CARTESIAN_POINT('Ctrl Pts',(-14.9562408442818,-12.4017930498775,
-333.940880953805)) ;
#31639 = CARTESIAN_POINT('Ctrl Pts',(-14.6921446542139,-12.7071440717281,
-333.935918705582)) ;
#31640 = CARTESIAN_POINT('Ctrl Pts',(-14.4282485172965,-13.0122637898483,
-333.930960216268)) ;
#31641 = CARTESIAN_POINT('Ctrl Pts',(-14.1548179543914,-13.309190318756,-333.926001726953)) ;
#31642 = CARTESIAN_POINT('Ctrl Pts',(-13.8723878820347,-13.5973335419257,
-333.921043237639)) ;
#31643 = CARTESIAN_POINT('Ctrl Pts',(-13.5899881188345,-13.8854458428286,
-333.916085280448)) ;
#31644 = CARTESIAN_POINT('Ctrl Pts',(-13.2985909412687,-14.164776551195,-333.911127323257)) ;
#31645 = CARTESIAN_POINT('Ctrl Pts',(-12.9987687452168,-14.4347717719532,
-333.906169366066)) ;
#31646 = CARTESIAN_POINT('Ctrl Pts',(-12.6989647701228,-14.7047505844146,
-333.901211710183)) ;
#31647 = CARTESIAN_POINT('Ctrl Pts',(-12.3907369757437,-14.9653948838844,
-333.8962540543)) ;
#31648 = CARTESIAN_POINT('Ctrl Pts',(-12.0746927611949,-15.2161893955993,
-333.891296398416)) ;
#31649 = CARTESIAN_POINT('Ctrl Pts',(-11.7581543086052,-15.4673761061978,
-333.886330989624)) ;
#31650 = CARTESIAN_POINT('Ctrl Pts',(-11.4337751481267,-15.708682039252,-333.881365580831)) ;
#31651 = CARTESIAN_POINT('Ctrl Pts',(-11.1021981093919,-15.9396305521745,
-333.876400172039)) ;
#31652 = CARTESIAN_POINT('Ctrl Pts',(-10.7711048287413,-16.1702421201428,
-333.871442007586)) ;
#31653 = CARTESIAN_POINT('Ctrl Pts',(-10.4328348610376,-16.3905263443745,
-333.866483843132)) ;
#31654 = CARTESIAN_POINT('Ctrl Pts',(-10.0880577922883,-16.6000516559272,
-333.861525678679)) ;
#31655 = CARTESIAN_POINT('Ctrl Pts',(-9.74252509648156,-16.810036171438,-333.856556647717)) ;
#31656 = CARTESIAN_POINT('Ctrl Pts',(-9.39045694281454,-17.0092144264153,
-333.851587616755)) ;
#31657 = CARTESIAN_POINT('Ctrl Pts',(-9.03255406527089,-17.1971972151848,
-333.846618585792)) ;
#31658 = CARTESIAN_POINT('Ctrl Pts',(-8.67465118772716,-17.3851800039543,
-333.84164955483)) ;
#31659 = CARTESIAN_POINT('Ctrl Pts',(-8.31091380159397,-17.5619672209556,
-333.836680523868)) ;
#31660 = CARTESIAN_POINT('Ctrl Pts',(-7.94206623749012,-17.7272166139899,
-333.831711492905)) ;
#31661 = CARTESIAN_POINT('Ctrl Pts',(-7.57542016948373,-17.8914797028453,
-333.82677212)) ;
#31662 = CARTESIAN_POINT('Ctrl Pts',(-7.20362005613073,-18.0443891674317,
-333.821832747096)) ;
#31663 = CARTESIAN_POINT('Ctrl Pts',(-6.82739290416258,-18.1856352963593,
-333.816893374191)) ;
#31664 = CARTESIAN_POINT('Ctrl Pts',(-6.45122839700186,-18.3268579066852,
-333.811954823731)) ;
#31665 = CARTESIAN_POINT('Ctrl Pts',(-6.07063854896628,-18.4564209748887,
-333.807016273271)) ;
#31666 = CARTESIAN_POINT('Ctrl Pts',(-5.68636928654813,-18.5740633501935,
-333.802077722811)) ;
#31667 = CARTESIAN_POINT('Ctrl Pts',(-5.30214293324897,-18.6916925890569,
-333.79713972381)) ;
#31668 = CARTESIAN_POINT('Ctrl Pts',(-4.91423821668825,-18.7974037230299,
-333.792201724809)) ;
#31669 = CARTESIAN_POINT('Ctrl Pts',(-4.52341669546291,-18.8909853210257,
-333.787263725808)) ;
#31670 = CARTESIAN_POINT('Ctrl Pts',(-4.13258414277082,-18.9845695604888,
-333.782325587426)) ;
#31671 = CARTESIAN_POINT('Ctrl Pts',(-3.73883485478379,-19.0660235209341,
-333.777387449043)) ;
#31672 = CARTESIAN_POINT('Ctrl Pts',(-3.342942861601,-19.1351863859245,-333.772449310661)) ;
#31673 = CARTESIAN_POINT('Ctrl Pts',(-2.94705968997046,-19.2043477097778,
-333.767511282313)) ;
#31674 = CARTESIAN_POINT('Ctrl Pts',(-2.54903414638424,-19.2612184453507,
-333.762573253966)) ;
#31675 = CARTESIAN_POINT('Ctrl Pts',(-2.14964907568037,-19.3056891576402,
-333.757635225619)) ;
#31676 = CARTESIAN_POINT('Ctrl Pts',(-1.75019814895231,-19.3501672028635,
-333.752696383022)) ;
#31677 = CARTESIAN_POINT('Ctrl Pts',(-1.34938748670992,-19.3822411103973,
-333.747757540426)) ;
#31678 = CARTESIAN_POINT('Ctrl Pts',(-0.948005606204455,-19.4018532715461,
-333.742818697829)) ;
#31679 = CARTESIAN_POINT('Ctrl Pts',(-0.632084577866105,-19.4172896786661,
-333.738931416645)) ;
#31680 = CARTESIAN_POINT('Ctrl Pts',(-0.315809823623688,-19.4250070501413,
-333.73504413546)) ;
#31681 = CARTESIAN_POINT('Ctrl Pts',(0.000433346557224641,-19.4249999951663,
-333.731156854276)) ;
#31682 = CARTESIAN_POINT('Ctrl Pts',(0.00049296941716015,-19.4249999937447,
-333.518704187163)) ;
#31683 = CARTESIAN_POINT('Ctrl Pts',(-0.634377794024984,-19.4250161055527,
-333.526895207536)) ;
#31684 = CARTESIAN_POINT('Ctrl Pts',(-1.26886984962391,-19.3939078124572,
-333.535071304866)) ;
#31685 = CARTESIAN_POINT('Ctrl Pts',(-2.08814708294686,-19.3133566103983,
-333.545427955287)) ;
#31686 = CARTESIAN_POINT('Ctrl Pts',(-2.27531831103279,-19.2922012363027,
-333.54778157939)) ;
#31687 = CARTESIAN_POINT('Ctrl Pts',(-2.5880520073918,-19.2522393847525,-333.551692190441)) ;
#31688 = CARTESIAN_POINT('Ctrl Pts',(-2.71379097667053,-19.2349180685968,
-333.553258578115)) ;
#31689 = CARTESIAN_POINT('Ctrl Pts',(-2.96955422421659,-19.1971272757905,
-333.556433013483)) ;
#31690 = CARTESIAN_POINT('Ctrl Pts',(-3.09955840904494,-19.1765660548772,
-333.558040375671)) ;
#31691 = CARTESIAN_POINT('Ctrl Pts',(-3.43440878247859,-19.120112663677,-333.562165822838)) ;
#31692 = CARTESIAN_POINT('Ctrl Pts',(-3.63890566184248,-19.0822492840032,
-333.56467100356)) ;
#31693 = CARTESIAN_POINT('Ctrl Pts',(-3.97755774036059,-19.0139046811789,
-333.56880235924)) ;
#31694 = CARTESIAN_POINT('Ctrl Pts',(-4.11206753742703,-18.9852689582846,
-333.570438778873)) ;
#31695 = CARTESIAN_POINT('Ctrl Pts',(-4.8889902194043,-18.8112261640848,-333.579873963237)) ;
#31696 = CARTESIAN_POINT('Ctrl Pts',(-5.52397797503081,-18.6346484022811,
-333.587502859057)) ;
#31697 = CARTESIAN_POINT('Ctrl Pts',(-6.45655009296665,-18.3234512419332,
-333.599039042833)) ;
#31698 = CARTESIAN_POINT('Ctrl Pts',(-6.76171162596236,-18.2130491550333,
-333.602872010311)) ;
#31699 = CARTESIAN_POINT('Ctrl Pts',(-7.15629336903421,-18.0590119933025,
-333.607974761023)) ;
#31700 = CARTESIAN_POINT('Ctrl Pts',(-7.24834591687685,-18.0222620774717,
-333.609175844674)) ;
#31701 = CARTESIAN_POINT('Ctrl Pts',(-7.40173864602791,-17.9596581345363,
-333.611198027685)) ;
#31702 = CARTESIAN_POINT('Ctrl Pts',(-7.46323449639608,-17.9341904237043,
-333.612014402899)) ;
#31703 = CARTESIAN_POINT('Ctrl Pts',(-7.59730253902076,-17.8778588825336,
-333.613807380551)) ;
#31704 = CARTESIAN_POINT('Ctrl Pts',(-7.6698199724682,-17.84686823121,-333.614785485383)) ;
#31705 = CARTESIAN_POINT('Ctrl Pts',(-7.89483493865592,-17.7490823127808,
-333.617843951232)) ;
#31706 = CARTESIAN_POINT('Ctrl Pts',(-8.04666373334751,-17.6807676379174,
-333.619941350387)) ;
#31707 = CARTESIAN_POINT('Ctrl Pts',(-8.31789712404011,-17.5545099886051,
-333.623737369494)) ;
#31708 = CARTESIAN_POINT('Ctrl Pts',(-8.43762187156459,-17.4972789486582,
-333.625430452278)) ;
#31709 = CARTESIAN_POINT('Ctrl Pts',(-9.07908498771921,-17.1825306939237,
-333.634580265556)) ;
#31710 = CARTESIAN_POINT('Ctrl Pts',(-9.58964074187833,-16.9028973008236,
-333.64213509543)) ;
#31711 = CARTESIAN_POINT('Ctrl Pts',(-10.4242964122772,-16.3957481446031,
-333.654655823424)) ;
#31712 = CARTESIAN_POINT('Ctrl Pts',(-10.7553897361116,-16.1804853398693,
-333.659672961205)) ;
#31713 = CARTESIAN_POINT('Ctrl Pts',(-11.21043332849,-15.8644932222774,-333.666609681646)) ;
#31714 = CARTESIAN_POINT('Ctrl Pts',(-11.3400527938041,-15.7721007904114,
-333.668590815108)) ;
#31715 = CARTESIAN_POINT('Ctrl Pts',(-11.5690204990481,-15.6046113045006,
-333.672099507132)) ;
#31716 = CARTESIAN_POINT('Ctrl Pts',(-11.6688097120516,-15.5301322989524,
-333.673631839425)) ;
#31717 = CARTESIAN_POINT('Ctrl Pts',(-11.880790810823,-15.3687207248924,-333.676894311884)) ;
#31718 = CARTESIAN_POINT('Ctrl Pts',(-11.9927600583853,-15.2815075584804,
-333.678622052446)) ;
#31719 = CARTESIAN_POINT('Ctrl Pts',(-12.3122233639389,-15.027002904733,-333.683566892419)) ;
#31720 = CARTESIAN_POINT('Ctrl Pts',(-12.5172433336689,-14.8566577724609,
-333.686758958099)) ;
#31721 = CARTESIAN_POINT('Ctrl Pts',(-13.3784181426972,-14.1106485051642,
-333.700290106059)) ;
#31722 = CARTESIAN_POINT('Ctrl Pts',(-13.9988696326359,-13.495336643232,-333.710306358222)) ;
#31723 = CARTESIAN_POINT('Ctrl Pts',(-14.6873365459008,-12.7138201991444,
-333.722668430197)) ;
#31724 = CARTESIAN_POINT('Ctrl Pts',(-14.797186343034,-12.5857997381955,-333.724684708977)) ;
#31725 = CARTESIAN_POINT('Ctrl Pts',(-14.9567467823962,-12.3948688424859,
-333.727690860287)) ;
#31726 = CARTESIAN_POINT('Ctrl Pts',(-15.0077578550807,-12.3330552612761,
-333.728663964886)) ;
#31727 = CARTESIAN_POINT('Ctrl Pts',(-15.1001491280674,-12.2196764387105,
-333.730450272513)) ;
#31728 = CARTESIAN_POINT('Ctrl Pts',(-15.1416513777497,-12.1682122563362,
-333.731261710531)) ;
#31729 = CARTESIAN_POINT('Ctrl Pts',(-15.2334276378244,-12.0532100187903,
-333.733076894494)) ;
#31730 = CARTESIAN_POINT('Ctrl Pts',(-15.2835683696731,-11.9895674326024,
-333.734082503568)) ;
#31731 = CARTESIAN_POINT('Ctrl Pts',(-15.443606743269,-11.7837987324861,-333.737334675666)) ;
#31732 = CARTESIAN_POINT('Ctrl Pts',(-15.5519312085663,-11.6404612154855,
-333.739601342375)) ;
#31733 = CARTESIAN_POINT('Ctrl Pts',(-15.8248690241512,-11.2686917240223,
-333.745462468966)) ;
#31734 = CARTESIAN_POINT('Ctrl Pts',(-15.9865325735823,-11.0381460746716,
-333.749079907081)) ;
#31735 = CARTESIAN_POINT('Ctrl Pts',(-16.5745066961902,-10.1596202300234,
-333.76270219977)) ;
#31736 = CARTESIAN_POINT('Ctrl Pts',(-16.9668986651267,-9.48981112800607,
-333.772735206145)) ;
#31737 = CARTESIAN_POINT('Ctrl Pts',(-17.389210438649,-8.65855465042104,-333.784437923188)) ;
#31738 = CARTESIAN_POINT('Ctrl Pts',(-17.4585320656547,-8.51791444651106,
-333.786394586159)) ;
#31739 = CARTESIAN_POINT('Ctrl Pts',(-17.5808205479466,-8.26204884621995,
-333.789911880438)) ;
#31740 = CARTESIAN_POINT('Ctrl Pts',(-17.6343762150223,-8.14711469375784,
-333.791476594318)) ;
#31741 = CARTESIAN_POINT('Ctrl Pts',(-17.7412973315182,-7.91166004604576,
-333.794651497065)) ;
#31742 = CARTESIAN_POINT('Ctrl Pts',(-17.7945691683645,-7.79110414875335,
-333.796260960422)) ;
#31743 = CARTESIAN_POINT('Ctrl Pts',(-17.9291227409596,-7.47802457544677,
-333.800400587902)) ;
#31744 = CARTESIAN_POINT('Ctrl Pts',(-18.0085320546082,-7.28471463050536,
-333.802917665049)) ;
#31745 = CARTESIAN_POINT('Ctrl Pts',(-18.1353558997643,-6.96122623787912,
-333.807072133883)) ;
#31746 = CARTESIAN_POINT('Ctrl Pts',(-18.1845245625784,-6.83175459364493,
-333.808719814951)) ;
#31747 = CARTESIAN_POINT('Ctrl Pts',(-18.3821408107369,-6.29413533803565,
-333.815506504031)) ;
#31748 = CARTESIAN_POINT('Ctrl Pts',(-18.5182644386963,-5.88159188289777,
-333.820580729743)) ;
#31749 = CARTESIAN_POINT('Ctrl Pts',(-18.6796300960854,-5.331176608105,-333.827279740326)) ;
#31750 = CARTESIAN_POINT('Ctrl Pts',(-18.7173756970051,-5.19710222717293,
-333.828906361971)) ;
#31751 = CARTESIAN_POINT('Ctrl Pts',(-18.7726314959133,-4.99241639642702,
-333.831386999337)) ;
#31752 = CARTESIAN_POINT('Ctrl Pts',(-18.7911924004187,-4.92209334769814,
-333.832238793075)) ;
#31753 = CARTESIAN_POINT('Ctrl Pts',(-18.8927928610358,-4.52820004483407,
-333.837010193975)) ;
#31754 = CARTESIAN_POINT('Ctrl Pts',(-18.9678696745375,-4.20263450562384,
-333.840954228702)) ;
#31755 = CARTESIAN_POINT('Ctrl Pts',(-19.0542615433035,-3.77829863155859,
-333.846171093305)) ;
#31756 = CARTESIAN_POINT('Ctrl Pts',(-19.0732678405119,-3.68115163446636,
-333.847370654727)) ;
#31757 = CARTESIAN_POINT('Ctrl Pts',(-19.1038078518183,-3.51846253403099,
-333.849391106166)) ;
#31758 = CARTESIAN_POINT('Ctrl Pts',(-19.1157488118805,-3.45299875643084,
-333.850207291852)) ;
#31759 = CARTESIAN_POINT('Ctrl Pts',(-19.1411172677412,-3.30975594454825,
-333.8520009225)) ;
#31760 = CARTESIAN_POINT('Ctrl Pts',(-19.1544075363511,-3.23195398795656,
-333.85297988125)) ;
#31761 = CARTESIAN_POINT('Ctrl Pts',(-19.1943198331489,-2.98940797272952,
-333.85604420457)) ;
#31762 = CARTESIAN_POINT('Ctrl Pts',(-19.2192933105096,-2.82440053416878,
-333.85814669636)) ;
#31763 = CARTESIAN_POINT('Ctrl Pts',(-19.2603674821564,-2.52717319999682,
-333.861953973039)) ;
#31764 = CARTESIAN_POINT('Ctrl Pts',(-19.2772404053223,-2.39507040272328,
-333.863653225687)) ;
#31765 = CARTESIAN_POINT('Ctrl Pts',(-19.3610532645679,-1.68047897078858,
-333.872867192125)) ;
#31766 = CARTESIAN_POINT('Ctrl Pts',(-19.4029529317605,-1.09535937448209,
-333.880480907722)) ;
#31767 = CARTESIAN_POINT('Ctrl Pts',(-19.4224441328253,-0.352124682352392,
-333.890010289483)) ;
#31768 = CARTESIAN_POINT('Ctrl Pts',(-19.424657459709,-0.194962874678155,
-333.892018032003)) ;
#31769 = CARTESIAN_POINT('Ctrl Pts',(-19.4255111694189,0.243847458051502,
-333.897598177308)) ;
#31770 = CARTESIAN_POINT('Ctrl Pts',(-19.4199338945183,0.525465325456291,
-333.901149453673)) ;
#31771 = CARTESIAN_POINT('Ctrl Pts',(-19.4022376525988,0.951129909222373,
-333.90646402678)) ;
#31772 = CARTESIAN_POINT('Ctrl Pts',(-19.3946316050709,1.09532598287024,-333.908255236887)) ;
#31773 = CARTESIAN_POINT('Ctrl Pts',(-19.3774938025193,1.36337266285042,-333.911568008291)) ;
#31774 = CARTESIAN_POINT('Ctrl Pts',(-19.3683804326872,1.4872425981483,-333.913092183635)) ;
#31775 = CARTESIAN_POINT('Ctrl Pts',(-19.344969578548,1.7685489203768,-333.916539000137)) ;
#31776 = CARTESIAN_POINT('Ctrl Pts',(-19.3299369724226,1.9259153700103,-333.918456787977)) ;
#31777 = CARTESIAN_POINT('Ctrl Pts',(-19.2718928924541,2.46406271261185,-333.924983894577)) ;
#31778 = CARTESIAN_POINT('Ctrl Pts',(-19.219536221626,2.84374560318721,-333.929533760456)) ;
#31779 = CARTESIAN_POINT('Ctrl Pts',(-19.02760865851,3.98495661289765,-333.943151099483)) ;
#31780 = CARTESIAN_POINT('Ctrl Pts',(-18.8537237035872,4.73992233222652,-333.952057623934)) ;
#31781 = CARTESIAN_POINT('Ctrl Pts',(-18.595520069256,5.61756917537427,-333.962985451683)) ;
#31782 = CARTESIAN_POINT('Ctrl Pts',(-18.5543129387541,5.7522101282501,-333.964679219269)) ;
#31783 = CARTESIAN_POINT('Ctrl Pts',(-18.4891439782415,5.9571548415608,-333.96729126482)) ;
#31784 = CARTESIAN_POINT('Ctrl Pts',(-18.4662366996387,6.02778906313,-333.968197700335)) ;
#31785 = CARTESIAN_POINT('Ctrl Pts',(-18.4214640392247,6.16319403724513,-333.969948670654)) ;
#31786 = CARTESIAN_POINT('Ctrl Pts',(-18.3996606681789,6.22798405172113,-333.970792500178)) ;
#31787 = CARTESIAN_POINT('Ctrl Pts',(-18.3417566032372,6.39709112056289,-333.973009519479)) ;
#31788 = CARTESIAN_POINT('Ctrl Pts',(-18.3051079115303,6.50121791613505,-333.974389132721)) ;
#31789 = CARTESIAN_POINT('Ctrl Pts',(-18.0976765588818,7.07491243554616,-333.982059551711)) ;
#31790 = CARTESIAN_POINT('Ctrl Pts',(-17.9097129459894,7.53806764257432,-333.988504886171)) ;
#31791 = CARTESIAN_POINT('Ctrl Pts',(-17.441099631996,8.57596357037019,-334.003197205166)) ;
#31792 = CARTESIAN_POINT('Ctrl Pts',(-17.1495075145107,9.14513557604694,-334.011429167314)) ;
#31793 = CARTESIAN_POINT('Ctrl Pts',(-16.7365603605633,9.86171826123412,-334.021833258483)) ;
#31794 = CARTESIAN_POINT('Ctrl Pts',(-16.6403729353542,10.0231695833263,-334.024181372581)) ;
#31795 = CARTESIAN_POINT('Ctrl Pts',(-16.4753577366656,10.2912246138698,-334.028085613267)) ;
#31796 = CARTESIAN_POINT('Ctrl Pts',(-16.4078009288665,10.3985953538322,-334.02965107128)) ;
#31797 = CARTESIAN_POINT('Ctrl Pts',(-16.2679630988419,10.6160892467489,-334.032825758557)) ;
#31798 = CARTESIAN_POINT('Ctrl Pts',(-16.1956038888716,10.7261544371592,-334.034434280181)) ;
#31799 = CARTESIAN_POINT('Ctrl Pts',(-16.0058174326016,11.0085381814168,-334.03856755477)) ;
#31800 = CARTESIAN_POINT('Ctrl Pts',(-15.886724897396,11.1797172061345,-334.041079302723)) ;
#31801 = CARTESIAN_POINT('Ctrl Pts',(-15.6136749186512,11.5590128266572,-334.046667662037)) ;
#31802 = CARTESIAN_POINT('Ctrl Pts',(-15.4582666947986,11.7660364210973,-334.049733608004)) ;
#31803 = CARTESIAN_POINT('Ctrl Pts',(-14.8267557090714,12.573173142812,-334.061798558308)) ;
#31804 = CARTESIAN_POINT('Ctrl Pts',(-14.3194752461305,13.1480031934642,-334.070615137339)) ;
#31805 = CARTESIAN_POINT('Ctrl Pts',(-13.6723612371942,13.7992863954528,-334.081562388432)) ;
#31806 = CARTESIAN_POINT('Ctrl Pts',(-13.5638751844945,13.9059360232863,-334.083389500396)) ;
#31807 = CARTESIAN_POINT('Ctrl Pts',(-13.3990762927668,14.0641817690922,-334.086161963129)) ;
#31808 = CARTESIAN_POINT('Ctrl Pts',(-13.3436935429148,14.1167381836986,-334.087093183689)) ;
#31809 = CARTESIAN_POINT('Ctrl Pts',(-13.2388643695025,14.2150495386456,-334.088856388651)) ;
#31810 = CARTESIAN_POINT('Ctrl Pts',(-13.1894870589464,14.2608763497804,-334.089687277657)) ;
#31811 = CARTESIAN_POINT('Ctrl Pts',(-13.0628509588499,14.3771863180403,-334.091818229695)) ;
#31812 = CARTESIAN_POINT('Ctrl Pts',(-12.9852595440676,14.4473041127236,-334.093123805156)) ;
#31813 = CARTESIAN_POINT('Ctrl Pts',(-12.8559948557357,14.5622353610732,-334.095295896157)) ;
#31814 = CARTESIAN_POINT('Ctrl Pts',(-12.8046443065917,14.6074086207401,-334.096158005758)) ;
#31815 = CARTESIAN_POINT('Ctrl Pts',(-12.6028574243775,14.783039597545,-334.099541042289)) ;
#31816 = CARTESIAN_POINT('Ctrl Pts',(-12.450657432261,14.9114521202667,-334.10208246997)) ;
#31817 = CARTESIAN_POINT('Ctrl Pts',(-11.7312234350435,15.4997498138426,-334.114001191108)) ;
#31818 = CARTESIAN_POINT('Ctrl Pts',(-11.1403181042868,15.9297572552004,-334.123498200318)) ;
#31819 = CARTESIAN_POINT('Ctrl Pts',(-10.2979503832235,16.4729131206968,-334.136232765216)) ;
#31820 = CARTESIAN_POINT('Ctrl Pts',(-10.0662176184587,16.6155322541338,-334.139660829656)) ;
#31821 = CARTESIAN_POINT('Ctrl Pts',(-9.70837105736396,16.8255329776774,-334.144834577377)) ;
#31822 = CARTESIAN_POINT('Ctrl Pts',(-9.58438292326255,16.8964680516786,-334.146605895128)) ;
#31823 = CARTESIAN_POINT('Ctrl Pts',(-9.36185898784423,17.020539078971,-334.149747255704)) ;
#31824 = CARTESIAN_POINT('Ctrl Pts',(-9.26362498593705,17.0742029506824,-334.151121145487)) ;
#31825 = CARTESIAN_POINT('Ctrl Pts',(-9.02955205330633,17.1994590255382,-334.154365026376)) ;
#31826 = CARTESIAN_POINT('Ctrl Pts',(-8.89331722638138,17.2702955924288,-334.156229438772)) ;
#31827 = CARTESIAN_POINT('Ctrl Pts',(-8.44821656927212,17.4950664046412,-334.162248417962)) ;
#31828 = CARTESIAN_POINT('Ctrl Pts',(-8.13608545504577,17.6423871938157,-334.166356350361)) ;
#31829 = CARTESIAN_POINT('Ctrl Pts',(-7.26145445614535,18.0270485847878,-334.177627740218)) ;
#31830 = CARTESIAN_POINT('Ctrl Pts',(-6.69144257907105,18.2463091121516,-334.184697804073)) ;
#31831 = CARTESIAN_POINT('Ctrl Pts',(-5.83097877883014,18.53154060576,-334.195351718606)) ;
#31832 = CARTESIAN_POINT('Ctrl Pts',(-5.54780808086928,18.6182742365684,-334.198857161506)) ;
#31833 = CARTESIAN_POINT('Ctrl Pts',(-5.16952436517516,18.7247436726624,-334.203594046749)) ;
#31834 = CARTESIAN_POINT('Ctrl Pts',(-5.07608752347006,18.7502891494303,-334.204768451229)) ;
#31835 = CARTESIAN_POINT('Ctrl Pts',(-4.91840038492085,18.7921354768562,-334.2067604979)) ;
#31836 = CARTESIAN_POINT('Ctrl Pts',(-4.85425063662515,18.8088082793602,-334.207573762549)) ;
#31837 = CARTESIAN_POINT('Ctrl Pts',(-4.71239121114863,18.8449040834322,-334.209379186949)) ;
#31838 = CARTESIAN_POINT('Ctrl Pts',(-4.6346443741653,18.8641753687738,-334.210373057371)) ;
#31839 = CARTESIAN_POINT('Ctrl Pts',(-4.38770282220305,18.9237665649291,-334.21354124599)) ;
#31840 = CARTESIAN_POINT('Ctrl Pts',(-4.21808483359718,18.9622951466243,-334.215734308373)) ;
#31841 = CARTESIAN_POINT('Ctrl Pts',(-3.78625431788715,19.0543042198343,-334.221341561554)) ;
#31842 = CARTESIAN_POINT('Ctrl Pts',(-3.52341190293161,19.1046538658482,-334.224776523735)) ;
#31843 = CARTESIAN_POINT('Ctrl Pts',(-2.45960639989161,19.2857335125215,-334.238674905473)) ;
#31844 = CARTESIAN_POINT('Ctrl Pts',(-1.65184645812952,19.3716441231337,-334.249182942896)) ;
#31845 = CARTESIAN_POINT('Ctrl Pts',(-0.689503890939881,19.4133518377827,
-334.261261090429)) ;
#31846 = CARTESIAN_POINT('Ctrl Pts',(-0.537850230463686,19.4181451844941,
-334.263152901883)) ;
#31847 = CARTESIAN_POINT('Ctrl Pts',(-0.260502263392738,19.4236597643566,
-334.266591167595)) ;
#31848 = CARTESIAN_POINT('Ctrl Pts',(-0.134827284795461,19.4249386542778,
-334.268141087538)) ;
#31849 = CARTESIAN_POINT('Ctrl Pts',(0.124518842200064,19.4250607994973,-334.271323305699)) ;
#31850 = CARTESIAN_POINT('Ctrl Pts',(0.2581835305543,19.4237440605022,-334.272954489055)) ;
#31851 = CARTESIAN_POINT('Ctrl Pts',(0.61113973312722,19.416623088611,-334.27723986224)) ;
#31852 = CARTESIAN_POINT('Ctrl Pts',(0.830364918795019,19.4084836673696,-334.279879036645)) ;
#31853 = CARTESIAN_POINT('Ctrl Pts',(1.32753338176573,19.3815856349554,-334.285823989006)) ;
#31854 = CARTESIAN_POINT('Ctrl Pts',(1.60530578702086,19.3605578498618,-334.289116639316)) ;
#31855 = CARTESIAN_POINT('Ctrl Pts',(2.25685442342576,19.2971158559699,-334.29680947418)) ;
#31856 = CARTESIAN_POINT('Ctrl Pts',(2.63004145476046,19.2498040050695,-334.301191236327)) ;
#31857 = CARTESIAN_POINT('Ctrl Pts',(3.23823228134206,19.1546817263087,-334.308387622607)) ;
#31858 = CARTESIAN_POINT('Ctrl Pts',(3.47414076295643,19.1133023341043,-334.311193211085)) ;
#31859 = CARTESIAN_POINT('Ctrl Pts',(3.93147985578674,19.0243359513042,-334.316697805706)) ;
#31860 = CARTESIAN_POINT('Ctrl Pts',(4.15296303474062,18.9772176552967,-334.319393892073)) ;
#31861 = CARTESIAN_POINT('Ctrl Pts',(4.45229957401473,18.9080454469311,-334.323104769871)) ;
#31862 = CARTESIAN_POINT('Ctrl Pts',(4.53091348121899,18.8893614800622,-334.324085692013)) ;
#31863 = CARTESIAN_POINT('Ctrl Pts',(4.67372734080227,18.8544764314364,-334.325880952515)) ;
#31864 = CARTESIAN_POINT('Ctrl Pts',(4.73796539112706,18.8384365783743,-334.326693441782)) ;
#31865 = CARTESIAN_POINT('Ctrl Pts',(4.88008928481094,18.8021761623923,-334.328502711755)) ;
#31866 = CARTESIAN_POINT('Ctrl Pts',(4.95793384102203,18.7817994844825,-334.329501264188)) ;
#31867 = CARTESIAN_POINT('Ctrl Pts',(5.20582194639987,18.7152634994681,-334.332702706351)) ;
#31868 = CARTESIAN_POINT('Ctrl Pts',(5.37536487826349,18.6672740978224,-334.334924872975)) ;
#31869 = CARTESIAN_POINT('Ctrl Pts',(5.80592576708458,18.5390509134454,-334.340631766853)) ;
#31870 = CARTESIAN_POINT('Ctrl Pts',(6.06594783206197,18.4556078031719,-334.344138120188)) ;
#31871 = CARTESIAN_POINT('Ctrl Pts',(7.08209615220398,18.1057221974789,-334.357982670507)) ;
#31872 = CARTESIAN_POINT('Ctrl Pts',(7.82319024184046,17.7980607967928,-334.368358698966)) ;
#31873 = CARTESIAN_POINT('Ctrl Pts',(8.67977105247503,17.3785885647298,-334.380319051033)) ;
#31874 = CARTESIAN_POINT('Ctrl Pts',(8.81560029398608,17.3100825407098,-334.382215952489)) ;
#31875 = CARTESIAN_POINT('Ctrl Pts',(9.06222758245143,17.1820392440777,-334.385660385211)) ;
#31876 = CARTESIAN_POINT('Ctrl Pts',(9.17327890013426,17.1230077851434,-334.387211430201)) ;
#31877 = CARTESIAN_POINT('Ctrl Pts',(9.40102028807281,16.9990960422778,-334.390392855248)) ;
#31878 = CARTESIAN_POINT('Ctrl Pts',(9.51763054201109,16.9340827219558,-334.392022152738)) ;
#31879 = CARTESIAN_POINT('Ctrl Pts',(9.82326402869296,16.7595296492867,-334.396294905916)) ;
#31880 = CARTESIAN_POINT('Ctrl Pts',(10.0111256431434,16.6479942883146,-334.398923516916)) ;
#31881 = CARTESIAN_POINT('Ctrl Pts',(10.3228053863565,16.4557630767802,-334.403296424333)) ;
#31882 = CARTESIAN_POINT('Ctrl Pts',(10.4476559343108,16.3767803618156,-334.40505140074)) ;
#31883 = CARTESIAN_POINT('Ctrl Pts',(10.9786591694058,16.0323142947773,-334.412538912018)) ;
#31884 = CARTESIAN_POINT('Ctrl Pts',(11.3756880836951,15.7530879412827,-334.418192080288)) ;
#31885 = CARTESIAN_POINT('Ctrl Pts',(11.864769683699,15.3809814757215,-334.425373483521)) ;
#31886 = CARTESIAN_POINT('Ctrl Pts',(11.9669103162139,15.3016472404185,-334.426886135509)) ;
#31887 = CARTESIAN_POINT('Ctrl Pts',(12.3149650574973,15.0256910292463,-334.432095155414)) ;
#31888 = CARTESIAN_POINT('Ctrl Pts',(12.5568864500716,14.8241140441618,-334.435809919664)) ;
#31889 = CARTESIAN_POINT('Ctrl Pts',(12.8770812712878,14.5438527268276,-334.440922023936)) ;
#31890 = CARTESIAN_POINT('Ctrl Pts',(12.9597372553524,14.4702482503935,-334.442260007276)) ;
#31891 = CARTESIAN_POINT('Ctrl Pts',(13.0874778812556,14.3545237920577,-334.444360258854)) ;
#31892 = CARTESIAN_POINT('Ctrl Pts',(13.1329985978956,14.3128885418513,-334.44511521892)) ;
#31893 = CARTESIAN_POINT('Ctrl Pts',(13.2308768379954,14.2225047265733,-334.44675361316)) ;
#31894 = CARTESIAN_POINT('Ctrl Pts',(13.2831649466434,14.173682357935,-334.447638273811)) ;
#31895 = CARTESIAN_POINT('Ctrl Pts',(13.4273839481385,14.0375234280768,-334.450102943273)) ;
#31896 = CARTESIAN_POINT('Ctrl Pts',(13.5187311184769,13.9495739202564,-334.451692091572)) ;
#31897 = CARTESIAN_POINT('Ctrl Pts',(13.7294001720252,13.7427278049008,-334.455416038119)) ;
#31898 = CARTESIAN_POINT('Ctrl Pts',(13.8480497449699,13.6231609674283,-334.457558474823)) ;
#31899 = CARTESIAN_POINT('Ctrl Pts',(14.2988121341239,13.1569393685709,-334.465849427585)) ;
#31900 = CARTESIAN_POINT('Ctrl Pts',(14.6195865231154,12.7995613987023,-334.472069508058)) ;
#31901 = CARTESIAN_POINT('Ctrl Pts',(15.2455699376987,12.047878240723,-334.484664107277)) ;
#31902 = CARTESIAN_POINT('Ctrl Pts',(15.5495062383087,11.652966621828,-334.491030249142)) ;
#31903 = CARTESIAN_POINT('Ctrl Pts',(15.9272817524453,11.1209774255067,-334.499215896157)) ;
#31904 = CARTESIAN_POINT('Ctrl Pts',(16.0151343417675,10.994085456421,-334.501141069363)) ;
#31905 = CARTESIAN_POINT('Ctrl Pts',(16.17208476471,10.7615164683546,-334.504619873024)) ;
#31906 = CARTESIAN_POINT('Ctrl Pts',(16.2416822384837,10.6561869563588,-334.506177285148)) ;
#31907 = CARTESIAN_POINT('Ctrl Pts',(16.3822961557718,10.4388023738032,-334.50935501507)) ;
#31908 = CARTESIAN_POINT('Ctrl Pts',(16.453201442586,10.3266831403083,-334.51097442404)) ;
#31909 = CARTESIAN_POINT('Ctrl Pts',(16.6353392518003,10.0320385648566,-334.515180930944)) ;
#31910 = CARTESIAN_POINT('Ctrl Pts',(16.7447174510192,9.84838806535011,-334.517754068654)) ;
#31911 = CARTESIAN_POINT('Ctrl Pts',(16.922227487327,9.53883217616622,-334.522017931058)) ;
#31912 = CARTESIAN_POINT('Ctrl Pts',(16.9920384034922,9.4139116930759,-334.523719148186)) ;
#31913 = CARTESIAN_POINT('Ctrl Pts',(17.2799231723973,8.88512992007277,-334.530846968818)) ;
#31914 = CARTESIAN_POINT('Ctrl Pts',(17.4850282774572,8.47437697204201,-334.536201904592)) ;
#31915 = CARTESIAN_POINT('Ctrl Pts',(17.8696485059172,7.63057312607779,-334.547033824975)) ;
#31916 = CARTESIAN_POINT('Ctrl Pts',(18.0484281152728,7.19751514768427,-334.552507699877)) ;
#31917 = CARTESIAN_POINT('Ctrl Pts',(18.2527768518267,6.64687286975248,-334.55955143004)) ;
#31918 = CARTESIAN_POINT('Ctrl Pts',(18.2931477771119,6.53494652555024,-334.560987653462)) ;
#31919 = CARTESIAN_POINT('Ctrl Pts',(18.3533579661568,6.36308577665903,-334.563204274281)) ;
#31920 = CARTESIAN_POINT('Ctrl Pts',(18.3739376464864,6.30341372487098,-334.563975990038)) ;
#31921 = CARTESIAN_POINT('Ctrl Pts',(18.4165977216969,6.17773403193171,-334.565606685783)) ;
#31922 = CARTESIAN_POINT('Ctrl Pts',(18.4386149160791,6.11170592877813,-334.566466537116)) ;
#31923 = CARTESIAN_POINT('Ctrl Pts',(18.4966957532922,5.93435459209416,-334.568783110975)) ;
#31924 = CARTESIAN_POINT('Ctrl Pts',(18.5321091190621,5.82282145989313,-334.570247325835)) ;
#31925 = CARTESIAN_POINT('Ctrl Pts',(18.7398594809636,5.14742023960839,-334.579144123232)) ;
#31926 = CARTESIAN_POINT('Ctrl Pts',(18.8874578434867,4.57626528498771,-334.58678395247)) ;
#31927 = CARTESIAN_POINT('Ctrl Pts',(19.0621695167566,3.74584977088118,-334.597725919259)) ;
#31928 = CARTESIAN_POINT('Ctrl Pts',(19.1104161528741,3.49137392110125,-334.601058634067)) ;
#31929 = CARTESIAN_POINT('Ctrl Pts',(19.2118003405683,2.89129282172694,-334.608842610779)) ;
#31930 = CARTESIAN_POINT('Ctrl Pts',(19.2607239090064,2.54506619183486,-334.613275146882)) ;
#31931 = CARTESIAN_POINT('Ctrl Pts',(19.3181680777768,2.04059127631761,-334.619629037976)) ;
#31932 = CARTESIAN_POINT('Ctrl Pts',(19.3341396084398,1.88326215243514,-334.621596152364)) ;
#31933 = CARTESIAN_POINT('Ctrl Pts',(19.3592230421088,1.60204096113557,-334.625086341218)) ;
#31934 = CARTESIAN_POINT('Ctrl Pts',(19.3690709023552,1.47822341394301,-334.626614070654)) ;
#31935 = CARTESIAN_POINT('Ctrl Pts',(19.3877949863084,1.21031753268275,-334.629900872155)) ;
#31936 = CARTESIAN_POINT('Ctrl Pts',(19.3962538865434,1.06620739104831,-334.6316571584)) ;
#31937 = CARTESIAN_POINT('Ctrl Pts',(19.4164624701931,0.640933667484384,-334.636808043619)) ;
#31938 = CARTESIAN_POINT('Ctrl Pts',(19.4237098311887,0.359593733983076,-334.640174001494)) ;
#31939 = CARTESIAN_POINT('Ctrl Pts',(19.4264955186439,-0.332409683582954,
-334.648380355026)) ;
#31940 = CARTESIAN_POINT('Ctrl Pts',(19.4151288650228,-0.742964319775833,
-334.653184693709)) ;
#31941 = CARTESIAN_POINT('Ctrl Pts',(19.3578940572392,-1.70564529116212,-334.664449441326)) ;
#31942 = CARTESIAN_POINT('Ctrl Pts',(19.301404710087,-2.25678104368422,-334.670894887691)) ;
#31943 = CARTESIAN_POINT('Ctrl Pts',(19.2049678140431,-2.91768092711522,-334.678912798869)) ;
#31944 = CARTESIAN_POINT('Ctrl Pts',(19.1874937363946,-3.03046775120494,-334.680291650034)) ;
#31945 = CARTESIAN_POINT('Ctrl Pts',(19.1589506884336,-3.20454541803918,-334.682440136039)) ;
#31946 = CARTESIAN_POINT('Ctrl Pts',(19.1485792102026,-3.26594810704615,-334.683201900217)) ;
#31947 = CARTESIAN_POINT('Ctrl Pts',(19.1258123312159,-3.39689829664632,-334.684835799605)) ;
#31948 = CARTESIAN_POINT('Ctrl Pts',(19.1133324431301,-3.46643019059573,-334.685709006972)) ;
#31949 = CARTESIAN_POINT('Ctrl Pts',(19.0782086967679,-3.65616452493381,-334.688105686054)) ;
#31950 = CARTESIAN_POINT('Ctrl Pts',(19.054808361097,-3.77622355869785,-334.689637530054)) ;
#31951 = CARTESIAN_POINT('Ctrl Pts',(18.9981436465971,-4.05300239806385,-334.69319815189)) ;
#31952 = CARTESIAN_POINT('Ctrl Pts',(18.9640712454272,-4.2095477366355,-334.695233716727)) ;
#31953 = CARTESIAN_POINT('Ctrl Pts',(18.8309354854158,-4.78678148261534,-334.702799672112)) ;
#31954 = CARTESIAN_POINT('Ctrl Pts',(18.7197773055192,-5.20455047700074,-334.708391575344)) ;
#31955 = CARTESIAN_POINT('Ctrl Pts',(18.5684397585047,-5.70543268815176,-334.715137184554)) ;
#31956 = CARTESIAN_POINT('Ctrl Pts',(18.5414894993282,-5.79241610868852,-334.71631028718)) ;
#31957 = CARTESIAN_POINT('Ctrl Pts',(18.3697224867553,-6.3333193812925,-334.723612021278)) ;
#31958 = CARTESIAN_POINT('Ctrl Pts',(18.2088570919137,-6.78197347736084,-334.729693862465)) ;
#31959 = CARTESIAN_POINT('Ctrl Pts',(17.9749958220313,-7.36568822842079,-334.737579636723)) ;
#31960 = CARTESIAN_POINT('Ctrl Pts',(17.9166711744184,-7.50644602941054,-334.739479558734)) ;
#31961 = CARTESIAN_POINT('Ctrl Pts',(17.807171071639,-7.76215900802771,-334.742927654322)) ;
#31962 = CARTESIAN_POINT('Ctrl Pts',(17.7565230416508,-7.87733099218671,-334.744479370161)) ;
#31963 = CARTESIAN_POINT('Ctrl Pts',(17.6498706987718,-8.11359893735732,-334.7476603437)) ;
#31964 = CARTESIAN_POINT('Ctrl Pts',(17.593730467232,-8.23462638514033,-334.749288537846)) ;
#31965 = CARTESIAN_POINT('Ctrl Pts',(17.4426099123047,-8.55181150737795,-334.753553906259)) ;
#31966 = CARTESIAN_POINT('Ctrl Pts',(17.3455674619773,-8.74696577419348,-334.756176335411)) ;
#31967 = CARTESIAN_POINT('Ctrl Pts',(17.1775069612165,-9.07113834075854,-334.760537050718)) ;
#31968 = CARTESIAN_POINT('Ctrl Pts',(17.108268710975,-9.20105635074467,-334.762285996648)) ;
#31969 = CARTESIAN_POINT('Ctrl Pts',(16.8059554315782,-9.75310181943261,-334.769732223868)) ;
#31970 = CARTESIAN_POINT('Ctrl Pts',(16.558683069537,-10.1672586446759,-334.775351045869)) ;
#31971 = CARTESIAN_POINT('Ctrl Pts',(16.1822448993713,-10.7475328032465,-334.783433351497)) ;
#31972 = CARTESIAN_POINT('Ctrl Pts',(16.0653969918523,-10.9214253069532,-334.785884418162)) ;
#31973 = CARTESIAN_POINT('Ctrl Pts',(15.7902093765532,-11.3169828494484,-334.791556433841)) ;
#31974 = CARTESIAN_POINT('Ctrl Pts',(15.6299740795108,-11.5372753581351,-334.794786836622)) ;
#31975 = CARTESIAN_POINT('Ctrl Pts',(15.4134379894353,-11.8221766417319,-334.79910280901)) ;
#31976 = CARTESIAN_POINT('Ctrl Pts',(15.3612674408727,-11.8898861974324,-334.800139098917)) ;
#31977 = CARTESIAN_POINT('Ctrl Pts',(15.2677723592363,-12.0095862745577,-334.801991920674)) ;
#31978 = CARTESIAN_POINT('Ctrl Pts',(15.2266248676298,-12.0617134126996,-334.802805937522)) ;
#31979 = CARTESIAN_POINT('Ctrl Pts',(15.1372936228876,-12.1736958606878,-334.804571030093)) ;
#31980 = CARTESIAN_POINT('Ctrl Pts',(15.0890204863635,-12.2334782411454,-334.805523357729)) ;
#31981 = CARTESIAN_POINT('Ctrl Pts',(14.9424018823832,-12.4128654115637,-334.808409244295)) ;
#31982 = CARTESIAN_POINT('Ctrl Pts',(14.842979855528,-12.5315821277078,-334.810357316582)) ;
#31983 = CARTESIAN_POINT('Ctrl Pts',(14.6645607892344,-12.7395242798043,-334.813828429465)) ;
#31984 = CARTESIAN_POINT('Ctrl Pts',(14.5861420288576,-12.8292354678863,-334.815345872513)) ;
#31985 = CARTESIAN_POINT('Ctrl Pts',(14.1944166568483,-13.2691352533951,-334.822875088162)) ;
#31986 = CARTESIAN_POINT('Ctrl Pts',(13.8693005980717,-13.6085971192817,-334.828961637716)) ;
#31987 = CARTESIAN_POINT('Ctrl Pts',(13.4868948813232,-13.9799241303449,-334.8358266719)) ;
#31988 = CARTESIAN_POINT('Ctrl Pts',(13.4413793458772,-14.023691864575,-334.836639339529)) ;
#31989 = CARTESIAN_POINT('Ctrl Pts',(13.0619152649048,-14.3850399041647,-334.843376442844)) ;
#31990 = CARTESIAN_POINT('Ctrl Pts',(12.7169748762829,-14.690866395463,-334.849252819499)) ;
#31991 = CARTESIAN_POINT('Ctrl Pts',(12.2346115849936,-15.088802343119,-334.857090671779)) ;
#31992 = CARTESIAN_POINT('Ctrl Pts',(12.1064144226376,-15.1918533010078,-334.859139626251)) ;
#31993 = CARTESIAN_POINT('Ctrl Pts',(11.8784274358333,-15.3704013742308,-334.862723697414)) ;
#31994 = CARTESIAN_POINT('Ctrl Pts',(11.7791879937148,-15.4465856100895,-334.86426435134)) ;
#31995 = CARTESIAN_POINT('Ctrl Pts',(11.5763506343292,-15.5992084459143,-334.867374646476)) ;
#31996 = CARTESIAN_POINT('Ctrl Pts',(11.4727148317295,-15.6755865149792,-334.868943753308)) ;
#31997 = CARTESIAN_POINT('Ctrl Pts',(11.1812381850836,-15.8859615339028,-334.873302931403)) ;
#31998 = CARTESIAN_POINT('Ctrl Pts',(10.9917577893027,-16.0176503323075,-334.876074902452)) ;
#31999 = CARTESIAN_POINT('Ctrl Pts',(10.5475633085915,-16.3147709755197,-334.882445318473)) ;
#32000 = CARTESIAN_POINT('Ctrl Pts',(10.2912255975046,-16.4776673049456,-334.886026786228)) ;
#32001 = CARTESIAN_POINT('Ctrl Pts',(9.73819263880107,-16.8111654154795,-334.89360137547)) ;
#32002 = CARTESIAN_POINT('Ctrl Pts',(9.44059423175864,-16.9800724097364,-334.897587649871)) ;
#32003 = CARTESIAN_POINT('Ctrl Pts',(9.0159245438828,-17.2064838124149,-334.903215431777)) ;
#32004 = CARTESIAN_POINT('Ctrl Pts',(8.89245874074754,-17.2706154517907,-334.904844765602)) ;
#32005 = CARTESIAN_POINT('Ctrl Pts',(8.50494782159208,-17.4666424705805,-334.90994895841)) ;
#32006 = CARTESIAN_POINT('Ctrl Pts',(8.23857914032455,-17.5938497693262,-334.91344319999)) ;
#32007 = CARTESIAN_POINT('Ctrl Pts',(7.88120251882413,-17.7546227337772,-334.918166919395)) ;
#32008 = CARTESIAN_POINT('Ctrl Pts',(7.79269356099606,-17.793647984327,-334.919339719362)) ;
#32009 = CARTESIAN_POINT('Ctrl Pts',(7.6430660818716,-17.8582909855102,-334.921329968823)) ;
#32010 = CARTESIAN_POINT('Ctrl Pts',(7.58210126016342,-17.8842600221946,-334.922143061582)) ;
#32011 = CARTESIAN_POINT('Ctrl Pts',(7.46899527689833,-17.931757207155,-334.923656138937)) ;
#32012 = CARTESIAN_POINT('Ctrl Pts',(7.41689106658348,-17.9533711007519,-334.924354843448)) ;
#32013 = CARTESIAN_POINT('Ctrl Pts',(7.35876822609363,-17.9771854359115,-334.925135815056)) ;
#32014 = CARTESIAN_POINT('Ctrl Pts',(7.35284176862584,-17.9796102273674,-334.925215464332)) ;
#32015 = CARTESIAN_POINT('Ctrl Pts',(7.34059571155037,-17.9846135956811,-334.925380082952)) ;
#32016 = CARTESIAN_POINT('Ctrl Pts',(7.33427594971204,-17.9871917730326,-334.925465056875)) ;
#32017 = CARTESIAN_POINT('Ctrl Pts',(7.32110337465282,-17.9925574921708,-334.925642212687)) ;
#32018 = CARTESIAN_POINT('Ctrl Pts',(7.31425032521435,-17.9953444510382,-334.925734401166)) ;
#32019 = CARTESIAN_POINT('Ctrl Pts',(7.29984921075362,-18.0011914282705,-334.9259281745)) ;
#32020 = CARTESIAN_POINT('Ctrl Pts',(7.29230081000141,-18.0042506157132,-334.926029768605)) ;
#32021 = CARTESIAN_POINT('Ctrl Pts',(7.28313043062368,-18.0079604393346,-334.926153224825)) ;
#32022 = CARTESIAN_POINT('Ctrl Pts',(7.28151028477896,-18.0086156055032,-334.926175037244)) ;
#32023 = CARTESIAN_POINT('Ctrl Pts',(7.27777929594972,-18.0101237836594,-334.926225271219)) ;
#32024 = CARTESIAN_POINT('Ctrl Pts',(7.27566839139559,-18.0109766431955,-334.926253694441)) ;
#32025 = CARTESIAN_POINT('Ctrl Pts',(7.27077911679054,-18.0129510356304,-334.926319532947)) ;
#32026 = CARTESIAN_POINT('Ctrl Pts',(7.26800063717667,-18.0140722968232,-334.926356951185)) ;
#32027 = CARTESIAN_POINT('Ctrl Pts',(7.26151933851884,-18.0166860946971,-334.926444243946)) ;
#32028 = CARTESIAN_POINT('Ctrl Pts',(7.25781631861398,-18.0181781327578,-334.926494123855)) ;
#32029 = CARTESIAN_POINT('Ctrl Pts',(7.24910376199596,-18.0216855150923,-334.926611496741)) ;
#32030 = CARTESIAN_POINT('Ctrl Pts',(7.24409384452291,-18.0236999123046,-334.926678999855)) ;
#32031 = CARTESIAN_POINT('Ctrl Pts',(7.23218566214197,-18.028482209982,-334.926839475173)) ;
#32032 = CARTESIAN_POINT('Ctrl Pts',(7.22528664743942,-18.0312482404754,-334.926932467153)) ;
#32033 = CARTESIAN_POINT('Ctrl Pts',(7.00269667854131,-18.1203432502996,-334.929933403537)) ;
#32034 = CARTESIAN_POINT('Ctrl Pts',(6.78547612516215,-18.2027996114837,-334.932881126412)) ;
#32035 = CARTESIAN_POINT('Ctrl Pts',(6.13301935114675,-18.4371682293537,-334.941741166967)) ;
#32036 = CARTESIAN_POINT('Ctrl Pts',(5.6938002848191,-18.5775062096151,-334.947710492633)) ;
#32037 = CARTESIAN_POINT('Ctrl Pts',(5.0463101262993,-18.7592681318011,-334.956374340118)) ;
#32038 = CARTESIAN_POINT('Ctrl Pts',(4.84169341590354,-18.8131175437422,-334.959093465878)) ;
#32039 = CARTESIAN_POINT('Ctrl Pts',(4.29992491791702,-18.9462716498603,-334.966227774864)) ;
#32040 = CARTESIAN_POINT('Ctrl Pts',(3.96146110807376,-19.0199208859464,-334.970618015183)) ;
#32041 = CARTESIAN_POINT('Ctrl Pts',(3.4660359946238,-19.1139259467775,-334.976928232904)) ;
#32042 = CARTESIAN_POINT('Ctrl Pts',(3.31050942772025,-19.141475858428,-334.97889291829)) ;
#32043 = CARTESIAN_POINT('Ctrl Pts',(3.03212029015865,-19.1872951536998,-334.982380503251)) ;
#32044 = CARTESIAN_POINT('Ctrl Pts',(2.9093858334737,-19.2062886286724,-334.983908030054)) ;
#32045 = CARTESIAN_POINT('Ctrl Pts',(2.67064164709251,-19.2408938998855,-334.986860391166)) ;
#32046 = CARTESIAN_POINT('Ctrl Pts',(2.55465623886165,-19.256636684872,-334.988286018659)) ;
#32047 = CARTESIAN_POINT('Ctrl Pts',(2.29624680491736,-19.2893350293378,-334.991443954951)) ;
#32048 = CARTESIAN_POINT('Ctrl Pts',(2.15376290812911,-19.3057634053631,-334.993172865671)) ;
#32049 = CARTESIAN_POINT('Ctrl Pts',(1.34283424036464,-19.3901741251841,-335.002949862918)) ;
#32050 = CARTESIAN_POINT('Ctrl Pts',(0.671398683770775,-19.4250168820751,
-335.010784597034)) ;
#32051 = CARTESIAN_POINT('Ctrl Pts',(-0.000488257005959863,-19.4249999938637,
-335.018634132644)) ;
#32052 = CARTESIAN_POINT('Origin',(0.,0.,-328.125)) ;
#32053 = CARTESIAN_POINT('',(0.000403208488304671,-19.4249999958153,-336.731156847152)) ;
#32054 = CARTESIAN_POINT('',(2.0594453916303E-9,-19.425,-336.519643262718)) ;
#32055 = CARTESIAN_POINT('',(-2.37887640734373E-15,-19.425,-328.125)) ;
#32056 = CARTESIAN_POINT('Ctrl Pts',(0.000397956517500714,-19.4247394275783,
-336.730705552561)) ;
#32057 = CARTESIAN_POINT('Ctrl Pts',(0.417181488622901,-19.4248114247665,
-336.725723703886)) ;
#32058 = CARTESIAN_POINT('Ctrl Pts',(0.833910655153896,-19.4114928611389,
-336.720789889741)) ;
#32059 = CARTESIAN_POINT('Ctrl Pts',(1.24973803346114,-19.3847950115984,-336.715859644829)) ;
#32060 = CARTESIAN_POINT('Ctrl Pts',(1.66569352250536,-19.3580889368151,-336.710927880977)) ;
#32061 = CARTESIAN_POINT('Ctrl Pts',(2.08074675907296,-19.3179951449265,-336.705999533908)) ;
#32062 = CARTESIAN_POINT('Ctrl Pts',(2.49404451930397,-19.2645639374455,-336.701006302343)) ;
#32063 = CARTESIAN_POINT('Ctrl Pts',(2.77527427666225,-19.2282065047151,-336.697608642262)) ;
#32064 = CARTESIAN_POINT('Ctrl Pts',(3.05569110924822,-19.1856744275963,-336.694180437861)) ;
#32065 = CARTESIAN_POINT('Ctrl Pts',(3.33502460600275,-19.1369946814523,-336.69069454568)) ;
#32066 = CARTESIAN_POINT('Ctrl Pts',(3.73266187925462,-19.0676980101108,-336.685732302778)) ;
#32067 = CARTESIAN_POINT('Ctrl Pts',(4.12817743095628,-18.9859283585497,-336.680653272706)) ;
#32068 = CARTESIAN_POINT('Ctrl Pts',(4.52078979820639,-18.8918837491355,-336.675533912964)) ;
#32069 = CARTESIAN_POINT('Ctrl Pts',(4.91310476537855,-18.7979103776049,-336.670418431087)) ;
#32070 = CARTESIAN_POINT('Ctrl Pts',(5.30252101598689,-18.691680818477,-336.665262846928)) ;
#32071 = CARTESIAN_POINT('Ctrl Pts',(5.68827676331055,-18.5734305685259,-336.660123589436)) ;
#32072 = CARTESIAN_POINT('Ctrl Pts',(6.07399111223989,-18.455193008912,-336.654984883478)) ;
#32073 = CARTESIAN_POINT('Ctrl Pts',(6.45604581295528,-18.3249374404889,-336.649862604335)) ;
#32074 = CARTESIAN_POINT('Ctrl Pts',(6.83369616006065,-18.1829351066735,-336.644791285714)) ;
#32075 = CARTESIAN_POINT('Ctrl Pts',(7.21132355562628,-18.0409414029897,-336.639720275299)) ;
#32076 = CARTESIAN_POINT('Ctrl Pts',(7.58454718817121,-17.8872023967985,-336.634700265376)) ;
#32077 = CARTESIAN_POINT('Ctrl Pts',(7.95263837668096,-17.7220240807298,-336.629742789312)) ;
#32078 = CARTESIAN_POINT('Ctrl Pts',(8.32130519074602,-17.5565874567666,-336.624777560686)) ;
#32079 = CARTESIAN_POINT('Ctrl Pts',(8.68482352257974,-17.3796756825354,-336.61987506014)) ;
#32080 = CARTESIAN_POINT('Ctrl Pts',(9.04247658715762,-17.1916311113474,-336.615023464694)) ;
#32081 = CARTESIAN_POINT('Ctrl Pts',(9.39960785268114,-17.0038608883733,-336.610178947498)) ;
#32082 = CARTESIAN_POINT('Ctrl Pts',(9.75089095264054,-16.8049902574347,-336.605385119696)) ;
#32083 = CARTESIAN_POINT('Ctrl Pts',(10.0956272775635,-16.5953956451601,-336.600607418064)) ;
#32084 = CARTESIAN_POINT('Ctrl Pts',(10.4411191359784,-16.3853416796412,-336.595819245492)) ;
#32085 = CARTESIAN_POINT('Ctrl Pts',(10.7800354361742,-16.1645165305077,-336.591047157463)) ;
#32086 = CARTESIAN_POINT('Ctrl Pts',(11.1116885036331,-15.9333365194949,-336.586234776286)) ;
#32087 = CARTESIAN_POINT('Ctrl Pts',(11.443341571092,-15.7021565084822,-336.581422395109)) ;
#32088 = CARTESIAN_POINT('Ctrl Pts',(11.7677312947932,-15.4606214608348,-336.576569535009)) ;
#32089 = CARTESIAN_POINT('Ctrl Pts',(12.0841867469861,-15.2091874595654,-336.571600497178)) ;
#32090 = CARTESIAN_POINT('Ctrl Pts',(12.4002102400622,-14.9580966636614,-336.566638242043)) ;
#32091 = CARTESIAN_POINT('Ctrl Pts',(12.7084032091301,-14.6970680724526,-336.561559204438)) ;
#32092 = CARTESIAN_POINT('Ctrl Pts',(13.0081741684115,-14.4266494454657,-336.556439840925)) ;
#32093 = CARTESIAN_POINT('Ctrl Pts',(13.3077181659163,-14.156435557097,-336.55132435337)) ;
#32094 = CARTESIAN_POINT('Ctrl Pts',(13.5988530508822,-13.8768459710949,-336.546168767258)) ;
#32095 = CARTESIAN_POINT('Ctrl Pts',(13.8810225436247,-13.5884519413831,-336.541029510624)) ;
#32096 = CARTESIAN_POINT('Ctrl Pts',(14.1631617563221,-13.3000888596811,-336.535890805491)) ;
#32097 = CARTESIAN_POINT('Ctrl Pts',(14.4363376106901,-13.0029232802281,-336.530768529981)) ;
#32098 = CARTESIAN_POINT('Ctrl Pts',(14.7000259285989,-12.6975496750222,-336.525697216853)) ;
#32099 = CARTESIAN_POINT('Ctrl Pts',(14.9636982223526,-12.3921946271573,-336.520626211905)) ;
#32100 = CARTESIAN_POINT('Ctrl Pts',(15.2178841980396,-12.0786325555002,-336.515606209307)) ;
#32101 = CARTESIAN_POINT('Ctrl Pts',(15.4620903737834,-11.7574807799444,-336.510648741478)) ;
#32102 = CARTESIAN_POINT('Ctrl Pts',(15.7066782786258,-11.4358269983383,-336.50568352442)) ;
#32103 = CARTESIAN_POINT('Ctrl Pts',(15.9412551663695,-11.106559723592,-336.500781036268)) ;
#32104 = CARTESIAN_POINT('Ctrl Pts',(16.1653553980525,-10.7703225124114,-336.495929453147)) ;
#32105 = CARTESIAN_POINT('Ctrl Pts',(16.3891288296542,-10.4345756280238,-336.491084944975)) ;
#32106 = CARTESIAN_POINT('Ctrl Pts',(16.6024561041871,-10.0918790576013,-336.486291126198)) ;
#32107 = CARTESIAN_POINT('Ctrl Pts',(16.8049038436912,-9.74289758437938,-336.481513432745)) ;
#32108 = CARTESIAN_POINT('Ctrl Pts',(17.0077950670615,-9.39315162915654,-336.476725273233)) ;
#32109 = CARTESIAN_POINT('Ctrl Pts',(17.1997589195039,-9.03709310484679,-336.471953197376)) ;
#32110 = CARTESIAN_POINT('Ctrl Pts',(17.3803907133679,-8.67541659417091,-336.467140826901)) ;
#32111 = CARTESIAN_POINT('Ctrl Pts',(17.5610225072322,-8.31374008349453,-336.462328456426)) ;
#32112 = CARTESIAN_POINT('Ctrl Pts',(17.7303220614185,-7.9464454861091,-336.457475605556)) ;
#32113 = CARTESIAN_POINT('Ctrl Pts',(17.8879184167642,-7.57425428821266,-336.452506575107)) ;
#32114 = CARTESIAN_POINT('Ctrl Pts',(18.0452997522663,-7.20257089706718,-336.447544324257)) ;
#32115 = CARTESIAN_POINT('Ctrl Pts',(18.1910503965086,-6.82590715285856,-336.442465288938)) ;
#32116 = CARTESIAN_POINT('Ctrl Pts',(18.3249130098465,-6.44502704079927,-336.43734592625)) ;
#32117 = CARTESIAN_POINT('Ctrl Pts',(18.4586741782345,-6.06443557067592,-336.432230443162)) ;
#32118 = CARTESIAN_POINT('Ctrl Pts',(18.5805655177904,-5.67963415908177,-336.427074860113)) ;
#32119 = CARTESIAN_POINT('Ctrl Pts',(18.6903718452331,-5.29139057726848,-336.421935605528)) ;
#32120 = CARTESIAN_POINT('Ctrl Pts',(18.8001663884123,-4.90318866122054,-336.416796902482)) ;
#32121 = CARTESIAN_POINT('Ctrl Pts',(18.8978786366604,-4.51154531074026,-336.411674628045)) ;
#32122 = CARTESIAN_POINT('Ctrl Pts',(18.9833327041114,-4.11723332735543,-336.406603315378)) ;
#32123 = CARTESIAN_POINT('Ctrl Pts',(19.0687815781059,-3.72294530821419,-336.401532310919)) ;
#32124 = CARTESIAN_POINT('Ctrl Pts',(19.1419738207046,-3.32598895314096,-336.396512308198)) ;
#32125 = CARTESIAN_POINT('Ctrl Pts',(19.2027714323094,-2.9271424411949,-336.391554840038)) ;
#32126 = CARTESIAN_POINT('Ctrl Pts',(19.2636641561563,-2.52767197075691,-336.386589616378)) ;
#32127 = CARTESIAN_POINT('Ctrl Pts',(19.3121234236185,-2.12630538368973,-336.38168712158)) ;
#32128 = CARTESIAN_POINT('Ctrl Pts',(19.3480482367358,-1.72383058058084,-336.376835532106)) ;
#32129 = CARTESIAN_POINT('Ctrl Pts',(19.3839206160168,-1.32194320705312,-336.37199102374)) ;
#32130 = CARTESIAN_POINT('Ctrl Pts',(19.4072950430532,-0.918950811292931,
-336.36719720493)) ;
#32131 = CARTESIAN_POINT('Ctrl Pts',(19.4181090048869,-0.515644496032888,
-336.362419511952)) ;
#32132 = CARTESIAN_POINT('Ctrl Pts',(19.4289466765016,-0.111453925347685,
-336.357631343808)) ;
#32133 = CARTESIAN_POINT('Ctrl Pts',(19.4271685926751,0.293051974743328,-336.352859259899)) ;
#32134 = CARTESIAN_POINT('Ctrl Pts',(19.4127516909178,0.697069655333783,-336.348046881928)) ;
#32135 = CARTESIAN_POINT('Ctrl Pts',(19.3983347891605,1.10108733592369,-336.343234503957)) ;
#32136 = CARTESIAN_POINT('Ctrl Pts',(19.3712788624363,1.50461679848425,-336.338381646147)) ;
#32137 = CARTESIAN_POINT('Ctrl Pts',(19.3316033377714,1.9068470059226,-336.333412609093)) ;
#32138 = CARTESIAN_POINT('Ctrl Pts',(19.2919819916405,2.30852795174019,-336.32845035746)) ;
#32139 = CARTESIAN_POINT('Ctrl Pts',(19.2397646789853,2.70901787938607,-336.323371321958)) ;
#32140 = CARTESIAN_POINT('Ctrl Pts',(19.1750909318642,3.1075227944095,-336.318251959449)) ;
#32141 = CARTESIAN_POINT('Ctrl Pts',(19.1104661629915,3.5057259166096,-336.313136473897)) ;
#32142 = CARTESIAN_POINT('Ctrl Pts',(19.0334040050997,3.90194708926831,-336.307980888707)) ;
#32143 = CARTESIAN_POINT('Ctrl Pts',(18.9440828204927,4.29540916073728,-336.302841632186)) ;
#32144 = CARTESIAN_POINT('Ctrl Pts',(18.8547712213034,4.68882900819909,-336.297702927179)) ;
#32145 = CARTESIAN_POINT('Ctrl Pts',(18.7532033333435,5.07949040829823,-336.292580650987)) ;
#32146 = CARTESIAN_POINT('Ctrl Pts',(18.6395944337072,5.46663059300599,-336.287509336649)) ;
#32147 = CARTESIAN_POINT('Ctrl Pts',(18.5259924382392,5.85374725067457,-336.282438330503)) ;
#32148 = CARTESIAN_POINT('Ctrl Pts',(18.4003509336652,6.23734317341979,-336.277418326181)) ;
#32149 = CARTESIAN_POINT('Ctrl Pts',(18.2629210388392,6.61666899676879,-336.272460856384)) ;
#32150 = CARTESIAN_POINT('Ctrl Pts',(18.1252762735369,6.99658789282885,-336.267495635625)) ;
#32151 = CARTESIAN_POINT('Ctrl Pts',(17.9758061945978,7.37222335572817,-336.262593143574)) ;
#32152 = CARTESIAN_POINT('Ctrl Pts',(17.8147990632875,7.74283518875109,-336.257741556614)) ;
#32153 = CARTESIAN_POINT('Ctrl Pts',(17.6540267813688,8.1129064372497,-336.252897046311)) ;
#32154 = CARTESIAN_POINT('Ctrl Pts',(17.4817510074677,8.47796870558782,-336.248103225427)) ;
#32155 = CARTESIAN_POINT('Ctrl Pts',(17.2982953304001,8.83729739527294,-336.243325530142)) ;
#32156 = CARTESIAN_POINT('Ctrl Pts',(17.1144376768194,9.19741342332789,-336.238537366272)) ;
#32157 = CARTESIAN_POINT('Ctrl Pts',(16.9193509244493,9.55177067442556,-336.233765286353)) ;
#32158 = CARTESIAN_POINT('Ctrl Pts',(16.7133992577366,9.89965249773097,-336.228952912242)) ;
#32159 = CARTESIAN_POINT('Ctrl Pts',(16.5074475910245,10.2475343210354,-336.224140538132)) ;
#32160 = CARTESIAN_POINT('Ctrl Pts',(16.2906308274627,10.5889406187893,-336.219287684055)) ;
#32161 = CARTESIAN_POINT('Ctrl Pts',(16.0633540450927,10.9231684924966,-336.214318650879)) ;
#32162 = CARTESIAN_POINT('Ctrl Pts',(15.836387425919,11.2569402475256,-336.209356398912)) ;
#32163 = CARTESIAN_POINT('Ctrl Pts',(15.5989297383643,11.5836399182122,-336.204277363033)) ;
#32164 = CARTESIAN_POINT('Ctrl Pts',(15.3514833758824,11.902637030503,-336.19915800018)) ;
#32165 = CARTESIAN_POINT('Ctrl Pts',(15.1042244749132,12.2213924755467,-336.194042515676)) ;
#32166 = CARTESIAN_POINT('Ctrl Pts',(14.8469921633439,12.532457167964,-336.188886931587)) ;
#32167 = CARTESIAN_POINT('Ctrl Pts',(14.5803148741814,12.835234001684,-336.18374767623)) ;
#32168 = CARTESIAN_POINT('Ctrl Pts',(14.313666203832,13.1379783425222,-336.178608972399)) ;
#32169 = CARTESIAN_POINT('Ctrl Pts',(14.0375746473913,13.4324367087426,-336.173486697444)) ;
#32170 = CARTESIAN_POINT('Ctrl Pts',(13.7525941723335,13.7180422858725,-336.168415384415)) ;
#32171 = CARTESIAN_POINT('Ctrl Pts',(13.4676310163982,14.0036305058906,-336.163344379585)) ;
#32172 = CARTESIAN_POINT('Ctrl Pts',(13.173780031458,14.2803670776265,-336.158324376649)) ;
#32173 = CARTESIAN_POINT('Ctrl Pts',(12.871620246085,14.5477141042196,-336.153366908317)) ;
#32174 = CARTESIAN_POINT('Ctrl Pts',(12.568987890871,14.815479254428,-336.148401686636)) ;
#32175 = CARTESIAN_POINT('Ctrl Pts',(12.2580206829302,15.0738254766371,-336.143499193805)) ;
#32176 = CARTESIAN_POINT('Ctrl Pts',(11.9393258814595,15.3222406935615,-336.138647606194)) ;
#32177 = CARTESIAN_POINT('Ctrl Pts',(11.6210960903992,15.5702934456405,-336.133803097577)) ;
#32178 = CARTESIAN_POINT('Ctrl Pts',(11.2951611748144,15.8084441224461,-336.129009278458)) ;
#32179 = CARTESIAN_POINT('Ctrl Pts',(10.9621519526002,16.0362112462496,-336.124231585018)) ;
#32180 = CARTESIAN_POINT('Ctrl Pts',(10.6284128203053,16.2644776040341,-336.119443419536)) ;
#32181 = CARTESIAN_POINT('Ctrl Pts',(10.2875682265132,16.4823147300163,-336.11467133811)) ;
#32182 = CARTESIAN_POINT('Ctrl Pts',(9.94028083639845,16.6892675465024,-336.109858962474)) ;
#32183 = CARTESIAN_POINT('Ctrl Pts',(9.59299344628393,16.8962203629883,-336.105046586837)) ;
#32184 = CARTESIAN_POINT('Ctrl Pts',(9.23926314635195,17.0922886968174,-336.100193731212)) ;
#32185 = CARTESIAN_POINT('Ctrl Pts',(8.87978193223753,17.2770491112091,-336.095224696288)) ;
#32186 = CARTESIAN_POINT('Ctrl Pts',(8.52079145992081,17.4615573019675,-336.090262444786)) ;
#32187 = CARTESIAN_POINT('Ctrl Pts',(8.155971937366,17.6348361085319,-336.085183409269)) ;
#32188 = CARTESIAN_POINT('Ctrl Pts',(7.78606616485268,17.7965722509237,-336.080064046666)) ;
#32189 = CARTESIAN_POINT('Ctrl Pts',(7.41644058646154,17.9581858823417,-336.074948561848)) ;
#32190 = CARTESIAN_POINT('Ctrl Pts',(7.04173651286741,18.1082745168596,-336.069792977324)) ;
#32191 = CARTESIAN_POINT('Ctrl Pts',(6.66270364660427,18.2465666337444,-336.064653721431)) ;
#32192 = CARTESIAN_POINT('Ctrl Pts',(6.28371145642438,18.3848439097482,-336.05951501706)) ;
#32193 = CARTESIAN_POINT('Ctrl Pts',(5.90039140878735,18.5113273231904,-336.054392741465)) ;
#32194 = CARTESIAN_POINT('Ctrl Pts',(5.51350113652929,18.6257841695783,-336.049321427717)) ;
#32195 = CARTESIAN_POINT('Ctrl Pts',(5.12663437653233,18.7402340601459,-336.044250422164)) ;
#32196 = CARTESIAN_POINT('Ctrl Pts',(4.73619780293921,18.8426589067191,-336.039230418426)) ;
#32197 = CARTESIAN_POINT('Ctrl Pts',(4.34295722055786,18.932863388036,-336.034272949234)) ;
#32198 = CARTESIAN_POINT('Ctrl Pts',(3.94910169708311,19.0232089291642,-336.029307727659)) ;
#32199 = CARTESIAN_POINT('Ctrl Pts',(3.55243334612323,19.1012958438172,-336.024405234849)) ;
#32200 = CARTESIAN_POINT('Ctrl Pts',(3.15373040943338,19.1669649899548,-336.019553647204)) ;
#32201 = CARTESIAN_POINT('Ctrl Pts',(2.7556091460887,19.2325383304475,-336.014709137609)) ;
#32202 = CARTESIAN_POINT('Ctrl Pts',(2.35545918607513,19.2857300515833,-336.009915317477)) ;
#32203 = CARTESIAN_POINT('Ctrl Pts',(1.95406481959108,19.3264191526301,-336.005137623011)) ;
#32204 = CARTESIAN_POINT('Ctrl Pts',(1.55179076985886,19.3671974266288,-336.0003494579)) ;
#32205 = CARTESIAN_POINT('Ctrl Pts',(1.14826681025661,19.3954180707545,-335.995577376822)) ;
#32206 = CARTESIAN_POINT('Ctrl Pts',(0.744292565869232,19.410998503486,-335.99076500158)) ;
#32207 = CARTESIAN_POINT('Ctrl Pts',(0.340318321481302,19.4265789362175,-335.985952626338)) ;
#32208 = CARTESIAN_POINT('Ctrl Pts',(-0.0641062245104881,19.4295189511988,
-335.981099771155)) ;
#32209 = CARTESIAN_POINT('Ctrl Pts',(-0.468170828899835,19.4197777840626,
-335.97613073681)) ;
#32210 = CARTESIAN_POINT('Ctrl Pts',(-0.87168390175727,19.4100499132182,-335.971168484991)) ;
#32211 = CARTESIAN_POINT('Ctrl Pts',(-1.27494321941302,19.3876724375374,-335.966089449256)) ;
#32212 = CARTESIAN_POINT('Ctrl Pts',(-1.67714662679196,19.3527256306513,-335.96097008652)) ;
#32213 = CARTESIAN_POINT('Ctrl Pts',(-2.07904536333704,19.3178052961238,-335.955854601725)) ;
#32214 = CARTESIAN_POINT('Ctrl Pts',(-2.47988983244948,19.2703348553497,-335.950699017313)) ;
#32215 = CARTESIAN_POINT('Ctrl Pts',(-2.87889179669617,19.210434554152,-335.945559761603)) ;
#32216 = CARTESIAN_POINT('Ctrl Pts',(-3.27785094179539,19.150540681193,-335.940421057416)) ;
#32217 = CARTESIAN_POINT('Ctrl Pts',(-3.6749680310441,19.0782197267368,-335.935298782076)) ;
#32218 = CARTESIAN_POINT('Ctrl Pts',(-4.0694664338171,18.9936298163128,-335.930227468632)) ;
#32219 = CARTESIAN_POINT('Ctrl Pts',(-4.46394086191889,18.9090450466327,-335.925156463386)) ;
#32220 = CARTESIAN_POINT('Ctrl Pts',(-4.85579697128176,18.8121928550736,-335.920136460004)) ;
#32221 = CARTESIAN_POINT('Ctrl Pts',(-5.24426884028382,18.7032681041243,-335.9151789912)) ;
#32222 = CARTESIAN_POINT('Ctrl Pts',(-5.63334821378748,18.5941730132306,-335.91021376975)) ;
#32223 = CARTESIAN_POINT('Ctrl Pts',(-6.01903278542061,18.4729675443096,-335.905311277103)) ;
#32224 = CARTESIAN_POINT('Ctrl Pts',(-6.40056302122172,18.339884280041,-335.900459689639)) ;
#32225 = CARTESIAN_POINT('Ctrl Pts',(-6.78153661699106,18.2069951798661,-335.895615180481)) ;
#32226 = CARTESIAN_POINT('Ctrl Pts',(-7.1583680006544,18.0622628466857,-335.890821360796)) ;
#32227 = CARTESIAN_POINT('Ctrl Pts',(-7.53031057479022,17.9059562498481,-335.88604366677)) ;
#32228 = CARTESIAN_POINT('Ctrl Pts',(-7.90306831615217,17.7493070839586,-335.88125550172)) ;
#32229 = CARTESIAN_POINT('Ctrl Pts',(-8.27091576187639,17.5810327139357,-335.876483420698)) ;
#32230 = CARTESIAN_POINT('Ctrl Pts',(-8.63311122904986,17.4014431828012,-335.871671045477)) ;
#32231 = CARTESIAN_POINT('Ctrl Pts',(-8.99530669622332,17.2218536516666,-335.866858670257)) ;
#32232 = CARTESIAN_POINT('Ctrl Pts',(-9.35185010088917,17.030948770167,-335.862005815059)) ;
#32233 = CARTESIAN_POINT('Ctrl Pts',(-9.70201044240801,16.8290803821525,-335.85703678063)) ;
#32234 = CARTESIAN_POINT('Ctrl Pts',(-10.0516928123364,16.6274875460583,-335.852074528972)) ;
#32235 = CARTESIAN_POINT('Ctrl Pts',(-10.3951004725014,16.4149081312252,-335.846995493338)) ;
#32236 = CARTESIAN_POINT('Ctrl Pts',(-10.7315674323518,16.1917963988285,-335.841876130656)) ;
#32237 = CARTESIAN_POINT('Ctrl Pts',(-11.0677795169522,15.9688536745822,-335.836760645915)) ;
#32238 = CARTESIAN_POINT('Ctrl Pts',(-11.3970615415595,15.7353947287877,-335.831605061509)) ;
#32239 = CARTESIAN_POINT('Ctrl Pts',(-11.7187788607783,15.4919022648105,-335.826465805769)) ;
#32240 = CARTESIAN_POINT('Ctrl Pts',(-12.0404616546875,15.2484359313901,-335.821327101552)) ;
#32241 = CARTESIAN_POINT('Ctrl Pts',(-12.3545814670092,14.9949383052232,-335.816204826145)) ;
#32242 = CARTESIAN_POINT('Ctrl Pts',(-12.6605319671979,14.7319197999514,-335.81113351261)) ;
#32243 = CARTESIAN_POINT('Ctrl Pts',(-12.9664638739843,14.4689172789937,-335.806062507272)) ;
#32244 = CARTESIAN_POINT('Ctrl Pts',(-13.264227525505,14.1963950501257,-335.801042503775)) ;
#32245 = CARTESIAN_POINT('Ctrl Pts',(-13.553243570959,13.9148906633192,-335.796085034843)) ;
#32246 = CARTESIAN_POINT('Ctrl Pts',(-13.8427115888996,13.6329460509969,-335.791119813262)) ;
#32247 = CARTESIAN_POINT('Ctrl Pts',(-14.1234046330415,13.3419911239812,-335.786217320472)) ;
#32248 = CARTESIAN_POINT('Ctrl Pts',(-14.3947670080328,13.0425934994147,-335.781365732863)) ;
#32249 = CARTESIAN_POINT('Ctrl Pts',(-14.6657334741274,12.7436326862641,-335.776521223562)) ;
#32250 = CARTESIAN_POINT('Ctrl Pts',(-14.9273964527425,12.4362537254702,-335.771727403734)) ;
#32251 = CARTESIAN_POINT('Ctrl Pts',(-15.179229016747,12.121049997195,-335.766949709574)) ;
#32252 = CARTESIAN_POINT('Ctrl Pts',(-15.4316135093015,11.8051554530303,-335.762161544386)) ;
#32253 = CARTESIAN_POINT('Ctrl Pts',(-15.6741243484905,11.4814016885572,-335.757389463236)) ;
#32254 = CARTESIAN_POINT('Ctrl Pts',(-15.9062585734021,11.1504158006893,-335.752577087905)) ;
#32255 = CARTESIAN_POINT('Ctrl Pts',(-16.1383927983141,10.819429912821,-335.747764712574)) ;
#32256 = CARTESIAN_POINT('Ctrl Pts',(-16.3601502446802,10.4812117755364,-335.742911857287)) ;
#32257 = CARTESIAN_POINT('Ctrl Pts',(-16.5710573305373,10.1364200815959,-335.737942822794)) ;
#32258 = CARTESIAN_POINT('Ctrl Pts',(-16.7816765264918,9.79209903114648,-335.732980571073)) ;
#32259 = CARTESIAN_POINT('Ctrl Pts',(-16.9815294718259,9.44113232479675,-335.727901535404)) ;
#32260 = CARTESIAN_POINT('Ctrl Pts',(-17.1702486707563,9.08423748848073,-335.722782172708)) ;
#32261 = CARTESIAN_POINT('Ctrl Pts',(-17.358824915386,8.72761299907167,-335.717666687915)) ;
#32262 = CARTESIAN_POINT('Ctrl Pts',(-17.5362844577517,8.36506942339514,-335.712511103478)) ;
#32263 = CARTESIAN_POINT('Ctrl Pts',(-17.7023009345826,7.99733426701588,-335.707371847721)) ;
#32264 = CARTESIAN_POINT('Ctrl Pts',(-17.8682995952563,7.62963857435403,-335.702233143487)) ;
#32265 = CARTESIAN_POINT('Ctrl Pts',(-18.0228577688157,7.25675243049972,-335.697110868077)) ;
#32266 = CARTESIAN_POINT('Ctrl Pts',(-18.1656872133452,6.87941412769221,-335.692039554548)) ;
#32267 = CARTESIAN_POINT('Ctrl Pts',(-18.308507977769,6.50209875668508,-335.686968549216)) ;
#32268 = CARTESIAN_POINT('Ctrl Pts',(-18.4396015015549,6.12033174955262,-335.681948545734)) ;
#32269 = CARTESIAN_POINT('Ctrl Pts',(-18.5587162171598,5.73486231995589,-335.67699107682)) ;
#32270 = CARTESIAN_POINT('Ctrl Pts',(-18.6780172066311,5.34879008590577,-335.672025855321)) ;
#32271 = CARTESIAN_POINT('Ctrl Pts',(-18.7853018849544,4.95900379762273,-335.667123362615)) ;
#32272 = CARTESIAN_POINT('Ctrl Pts',(-18.8803538419933,4.56626775423995,-335.662271775086)) ;
#32273 = CARTESIAN_POINT('Ctrl Pts',(-18.9752671225249,4.17410469498566,-335.657427265805)) ;
#32274 = CARTESIAN_POINT('Ctrl Pts',(-19.0579832957413,3.77900043415976,-335.652633445994)) ;
#32275 = CARTESIAN_POINT('Ctrl Pts',(-19.1283235393561,3.38172813075498,-335.647855751845)) ;
#32276 = CARTESIAN_POINT('Ctrl Pts',(-19.1988179427352,2.98358515358625,-335.64306758676)) ;
#32277 = CARTESIAN_POINT('Ctrl Pts',(-19.2568819647207,2.58326456638056,-335.638295505705)) ;
#32278 = CARTESIAN_POINT('Ctrl Pts',(-19.3023739593782,2.18155766970835,-335.633483130463)) ;
#32279 = CARTESIAN_POINT('Ctrl Pts',(-19.3478659540356,1.77985077303668,-335.62867075522)) ;
#32280 = CARTESIAN_POINT('Ctrl Pts',(-19.3807857168242,1.37675753482452,-335.623817900012)) ;
#32281 = CARTESIAN_POINT('Ctrl Pts',(-19.4010325165295,0.973082945256434,
-335.618848865593)) ;
#32282 = CARTESIAN_POINT('Ctrl Pts',(-19.4212516794254,0.569959370063551,
-335.613886613888)) ;
#32283 = CARTESIAN_POINT('Ctrl Pts',(-19.4288372442096,0.166150890841973,
-335.608807578225)) ;
#32284 = CARTESIAN_POINT('Ctrl Pts',(-19.4238097842129,-0.237536593306288,
-335.603688215528)) ;
#32285 = CARTESIAN_POINT('Ctrl Pts',(-19.4187861325342,-0.640918282809963,
-335.598572730766)) ;
#32286 = CARTESIAN_POINT('Ctrl Pts',(-19.4011687499022,-1.04417919004252,
-335.593417146355)) ;
#32287 = CARTESIAN_POINT('Ctrl Pts',(-19.3710191037869,-1.44652433131471,
-335.588277890619)) ;
#32288 = CARTESIAN_POINT('Ctrl Pts',(-19.3408726932006,-1.84882629465552,
-335.583139186406)) ;
#32289 = CARTESIAN_POINT('Ctrl Pts',(-19.298196823703,-2.25021273376001,-335.578016911014)) ;
#32290 = CARTESIAN_POINT('Ctrl Pts',(-19.2430915988317,-2.64989743103697,
-335.572945597502)) ;
#32291 = CARTESIAN_POINT('Ctrl Pts',(-19.1879897228463,-3.04955783844967,
-335.567874592186)) ;
#32292 = CARTESIAN_POINT('Ctrl Pts',(-19.1204600486215,-3.44751675700766,
-335.562854588718)) ;
#32293 = CARTESIAN_POINT('Ctrl Pts',(-19.0406401095888,-3.84299592462276,
-335.557897119818)) ;
#32294 = CARTESIAN_POINT('Ctrl Pts',(-18.9606953457586,-4.23909355433633,
-335.552931898281)) ;
#32295 = CARTESIAN_POINT('Ctrl Pts',(-18.8684218195035,-4.63270370490894,
-335.548029405537)) ;
#32296 = CARTESIAN_POINT('Ctrl Pts',(-18.763995154248,-5.02305168740151,-335.543177817974)) ;
#32297 = CARTESIAN_POINT('Ctrl Pts',(-18.6597208438918,-5.41283016566436,
-335.538333308709)) ;
#32298 = CARTESIAN_POINT('Ctrl Pts',(-18.5433287606616,-5.79935600341102,
-335.533539488917)) ;
#32299 = CARTESIAN_POINT('Ctrl Pts',(-18.4150317737214,-6.18186471457878,
-335.52876179479)) ;
#32300 = CARTESIAN_POINT('Ctrl Pts',(-18.2864536052352,-6.56521174933737,
-335.52397362965)) ;
#32301 = CARTESIAN_POINT('Ctrl Pts',(-18.1459181396667,-6.9445240077796,-335.519201548544)) ;
#32302 = CARTESIAN_POINT('Ctrl Pts',(-17.993679571189,-7.31903885923887,-335.514389173252)) ;
#32303 = CARTESIAN_POINT('Ctrl Pts',(-17.8414410027114,-7.69355371069813,
-335.50957679796)) ;
#32304 = CARTESIAN_POINT('Ctrl Pts',(-17.6774991363662,-8.0632710854823,-335.504723942706)) ;
#32305 = CARTESIAN_POINT('Ctrl Pts',(-17.5021506441656,-8.42743590628459,
-335.499754908239)) ;
#32306 = CARTESIAN_POINT('Ctrl Pts',(-17.3270415037638,-8.79110363980762,
-335.494792656536)) ;
#32307 = CARTESIAN_POINT('Ctrl Pts',(-17.1405107631171,-9.14932858519802,
-335.489713620875)) ;
#32308 = CARTESIAN_POINT('Ctrl Pts',(-16.9429620500801,-9.50141290208948,
-335.484594258182)) ;
#32309 = CARTESIAN_POINT('Ctrl Pts',(-16.7455629801875,-9.85323051512083,
-335.479478773406)) ;
#32310 = CARTESIAN_POINT('Ctrl Pts',(-16.5371627784836,-10.1989169171179,
-335.47432318898)) ;
#32311 = CARTESIAN_POINT('Ctrl Pts',(-16.3181957609453,-10.5378034176016,
-335.469183933231)) ;
#32312 = CARTESIAN_POINT('Ctrl Pts',(-16.0992522419896,-10.8766535502684,
-335.464045229003)) ;
#32313 = CARTESIAN_POINT('Ctrl Pts',(-15.8697442543277,-11.2087053354623,
-335.458922953597)) ;
#32314 = CARTESIAN_POINT('Ctrl Pts',(-15.630135847461,-11.5333162649052,-335.453851640069)) ;
#32315 = CARTESIAN_POINT('Ctrl Pts',(-15.3905420022053,-11.857907466918,-335.448780634739)) ;
#32316 = CARTESIAN_POINT('Ctrl Pts',(-15.1408489840806,-12.1750587802935,
-335.443760631255)) ;
#32317 = CARTESIAN_POINT('Ctrl Pts',(-14.8815499047474,-12.4841525900853,
-335.438803162339)) ;
#32318 = CARTESIAN_POINT('Ctrl Pts',(-14.6218453273732,-12.7937297680969,
-335.433837940815)) ;
#32319 = CARTESIAN_POINT('Ctrl Pts',(-14.3525045804028,-13.095224238069,-335.428935448083)) ;
#32320 = CARTESIAN_POINT('Ctrl Pts',(-14.0740525139215,-13.3880397459356,
-335.424083860531)) ;
#32321 = CARTESIAN_POINT('Ctrl Pts',(-13.7960066976958,-13.6804280478692,
-335.419239351247)) ;
#32322 = CARTESIAN_POINT('Ctrl Pts',(-13.5088760596408,-13.9641626740379,
-335.414445531436)) ;
#32323 = CARTESIAN_POINT('Ctrl Pts',(-13.2132132751,-14.2386741490737,-335.409667837287)) ;
#32324 = CARTESIAN_POINT('Ctrl Pts',(-12.9169025051837,-14.5137872535012,
-335.40487967217)) ;
#32325 = CARTESIAN_POINT('Ctrl Pts',(-12.6120220248791,-14.7796366419539,
-335.400107591085)) ;
#32326 = CARTESIAN_POINT('Ctrl Pts',(-12.2991599105236,-15.0356742392506,
-335.395295215814)) ;
#32327 = CARTESIAN_POINT('Ctrl Pts',(-11.9862977961685,-15.291711836547,-335.390482840544)) ;
#32328 = CARTESIAN_POINT('Ctrl Pts',(-11.6654539099066,-15.5379374882154,
-335.38562998531)) ;
#32329 = CARTESIAN_POINT('Ctrl Pts',(-11.3372500153741,-15.7738300743316,
-335.380660950867)) ;
#32330 = CARTESIAN_POINT('Ctrl Pts',(-11.0094941193816,-16.0094006669069,
-335.375698699158)) ;
#32331 = CARTESIAN_POINT('Ctrl Pts',(-10.6743125509312,-16.2347274182438,
-335.370619663494)) ;
#32332 = CARTESIAN_POINT('Ctrl Pts',(-10.3323936111183,-16.4493906400966,
-335.365500300798)) ;
#32333 = CARTESIAN_POINT('Ctrl Pts',(-9.99073367541036,-16.6638912542399,
-335.360384816027)) ;
#32334 = CARTESIAN_POINT('Ctrl Pts',(-9.64234665101162,-16.8677446656216,
-335.355229231607)) ;
#32335 = CARTESIAN_POINT('Ctrl Pts',(-9.28793384112007,-17.0605714652986,
-335.350089975865)) ;
#32336 = CARTESIAN_POINT('Ctrl Pts',(-8.93355906526314,-17.2533775716457,
-335.344951271644)) ;
#32337 = CARTESIAN_POINT('Ctrl Pts',(-8.57315982150312,-17.4351595538585,
-335.339828996246)) ;
#32338 = CARTESIAN_POINT('Ctrl Pts',(-8.20745099669403,-17.6055752195817,
-335.334757682728)) ;
#32339 = CARTESIAN_POINT('Ctrl Pts',(-7.84176439694247,-17.7759805287106,
-335.329686677406)) ;
#32340 = CARTESIAN_POINT('Ctrl Pts',(-7.47076884789392,-17.9350209668775,
-335.324666673932)) ;
#32341 = CARTESIAN_POINT('Ctrl Pts',(-7.0951928471428,-18.0823901053232,-335.319709205027)) ;
#32342 = CARTESIAN_POINT('Ctrl Pts',(-6.71902951074151,-18.2299897035123,
-335.3147439835)) ;
#32343 = CARTESIAN_POINT('Ctrl Pts',(-6.33827134199943,-18.3658814645726,
-335.309841490767)) ;
#32344 = CARTESIAN_POINT('Ctrl Pts',(-5.95366448937237,-18.4897929017834,
-335.304989903213)) ;
#32345 = CARTESIAN_POINT('Ctrl Pts',(-5.56961876354971,-18.613523556909,-335.300145393942)) ;
#32346 = CARTESIAN_POINT('Ctrl Pts',(-5.18173552463438,-18.725308770049,-335.295351574143)) ;
#32347 = CARTESIAN_POINT('Ctrl Pts',(-4.79077254364982,-18.8249128819126,
-335.290573880007)) ;
#32348 = CARTESIAN_POINT('Ctrl Pts',(-4.39895271232139,-18.9247352901921,
-335.285785714883)) ;
#32349 = CARTESIAN_POINT('Ctrl Pts',(-4.00403956016823,-19.0123230044549,
-335.281013633792)) ;
#32350 = CARTESIAN_POINT('Ctrl Pts',(-3.60681170648216,-19.0874760942272,
-335.276201258515)) ;
#32351 = CARTESIAN_POINT('Ctrl Pts',(-3.20958385279609,-19.1626291839994,
-335.271388883238)) ;
#32352 = CARTESIAN_POINT('Ctrl Pts',(-2.81004125042442,-19.2253474476804,
-335.266536027998)) ;
#32353 = CARTESIAN_POINT('Ctrl Pts',(-2.40897920439023,-19.2754707418096,
-335.261566993546)) ;
#32354 = CARTESIAN_POINT('Ctrl Pts',(-1.98818862475481,-19.3280596372146,
-335.256353528677)) ;
#32355 = CARTESIAN_POINT('Ctrl Pts',(-1.5656546785899,-19.3667931000231,-335.251011760576)) ;
#32356 = CARTESIAN_POINT('Ctrl Pts',(-1.14226732751046,-19.3916351229619,
-335.24562939536)) ;
#32357 = CARTESIAN_POINT('Ctrl Pts',(-0.762155209100447,-19.4139379951208,
-335.240797172009)) ;
#32358 = CARTESIAN_POINT('Ctrl Pts',(-0.381355021190701,-19.4250447171769,
-335.235932049976)) ;
#32359 = CARTESIAN_POINT('Ctrl Pts',(-0.000505252659192643,-19.4249560735629,
-335.231080776623)) ;
#32360 = CARTESIAN_POINT('Ctrl Pts',(-0.000488272271658846,-19.4249999938633,
-335.018634132822)) ;
#32361 = CARTESIAN_POINT('Ctrl Pts',(-0.468717606056336,-19.4249882243189,
-335.024104372837)) ;
#32362 = CARTESIAN_POINT('Ctrl Pts',(-0.936792336862977,-19.4080468254062,
-335.029582516708)) ;
#32363 = CARTESIAN_POINT('Ctrl Pts',(-1.48555256655971,-19.3682853646297,
-335.036195527655)) ;
#32364 = CARTESIAN_POINT('Ctrl Pts',(-1.5672717674808,-19.3618440129123,-335.037185408023)) ;
#32365 = CARTESIAN_POINT('Ctrl Pts',(-1.71125369797793,-19.3495774113658,
-335.038940172386)) ;
#32366 = CARTESIAN_POINT('Ctrl Pts',(-1.77353368560344,-19.343968400327,-335.039702732533)) ;
#32367 = CARTESIAN_POINT('Ctrl Pts',(-1.90166063482093,-19.3318051530813,
-335.041279704335)) ;
#32368 = CARTESIAN_POINT('Ctrl Pts',(-1.96750318988438,-19.325215000439,-335.042094685323)) ;
#32369 = CARTESIAN_POINT('Ctrl Pts',(-2.12867204830871,-19.3082514698797,
-335.044100366175)) ;
#32370 = CARTESIAN_POINT('Ctrl Pts',(-2.22395759981224,-19.2975084420849,
-335.045295244128)) ;
#32371 = CARTESIAN_POINT('Ctrl Pts',(-2.60634702361314,-19.2515258990493,
-335.050121609932)) ;
#32372 = CARTESIAN_POINT('Ctrl Pts',(-2.89272684723886,-19.2105810705904,
-335.053806452374)) ;
#32373 = CARTESIAN_POINT('Ctrl Pts',(-3.35022309201495,-19.1347086954307,
-335.059754882247)) ;
#32374 = CARTESIAN_POINT('Ctrl Pts',(-3.52196899990878,-19.1038427008835,
-335.062002161339)) ;
#32375 = CARTESIAN_POINT('Ctrl Pts',(-4.17682254465237,-18.9770220388341,
-335.070603310764)) ;
#32376 = CARTESIAN_POINT('Ctrl Pts',(-4.65663385048137,-18.8650198705459,
-335.076968430991)) ;
#32377 = CARTESIAN_POINT('Ctrl Pts',(-5.42240760696615,-18.6552671305497,
-335.087090322891)) ;
#32378 = CARTESIAN_POINT('Ctrl Pts',(-5.71125364216025,-18.5688739131451,
-335.090900874196)) ;
#32379 = CARTESIAN_POINT('Ctrl Pts',(-6.08250417820151,-18.4483513254985,
-335.095779205614)) ;
#32380 = CARTESIAN_POINT('Ctrl Pts',(-6.16684668136298,-18.420329142885,-335.096886244625)) ;
#32381 = CARTESIAN_POINT('Ctrl Pts',(-6.36106680269313,-18.3543174701958,
-335.099432528422)) ;
#32382 = CARTESIAN_POINT('Ctrl Pts',(-6.47080165456166,-18.3159183949568,
-335.100868981337)) ;
#32383 = CARTESIAN_POINT('Ctrl Pts',(-6.69896362834188,-18.2337721932833,
-335.103851292836)) ;
#32384 = CARTESIAN_POINT('Ctrl Pts',(-6.81732237804154,-18.1898509541121,
-335.105395876785)) ;
#32385 = CARTESIAN_POINT('Ctrl Pts',(-7.07939981786079,-18.0896804776572,
-335.108811394339)) ;
#32386 = CARTESIAN_POINT('Ctrl Pts',(-7.22289336033244,-18.0328659162564,
-335.110678349121)) ;
#32387 = CARTESIAN_POINT('Ctrl Pts',(-7.81827949264123,-17.7888830666712,
-335.118417418889)) ;
#32388 = CARTESIAN_POINT('Ctrl Pts',(-8.26369844989171,-17.5863908843134,
-335.124184558792)) ;
#32389 = CARTESIAN_POINT('Ctrl Pts',(-8.8406215197942,-17.2973530790208,-335.131738439332)) ;
#32390 = CARTESIAN_POINT('Ctrl Pts',(-8.97939500145368,-17.2257214019571,
-335.133562562827)) ;
#32391 = CARTESIAN_POINT('Ctrl Pts',(-9.44631434337654,-16.9775326429109,
-335.139738403987)) ;
#32392 = CARTESIAN_POINT('Ctrl Pts',(-9.77023828626849,-16.7932103081035,
-335.144086463682)) ;
#32393 = CARTESIAN_POINT('Ctrl Pts',(-10.2651110727269,-16.4924454046484,
-335.150939897255)) ;
#32394 = CARTESIAN_POINT('Ctrl Pts',(-10.4398413964372,-16.3823982406034,
-335.153402423781)) ;
#32395 = CARTESIAN_POINT('Ctrl Pts',(-10.6836412791606,-16.2233655941138,
-335.156919690524)) ;
#32396 = CARTESIAN_POINT('Ctrl Pts',(-10.7541961257338,-16.1766822261781,
-335.15794737896)) ;
#32397 = CARTESIAN_POINT('Ctrl Pts',(-10.8268721074768,-16.1279097815406,
-335.15901726738)) ;
#32398 = CARTESIAN_POINT('Ctrl Pts',(-10.8293001636972,-16.1262795311789,
-335.15905302476)) ;
#32399 = CARTESIAN_POINT('Ctrl Pts',(-10.8327514110086,-16.1239611568537,
-335.159103869138)) ;
#32400 = CARTESIAN_POINT('Ctrl Pts',(-10.8337749049054,-16.1232734837029,
-335.159118949769)) ;
#32401 = CARTESIAN_POINT('Ctrl Pts',(-10.8367519506596,-16.1212728312673,
-335.159162821756)) ;
#32402 = CARTESIAN_POINT('Ctrl Pts',(-10.8387053293361,-16.1199595943694,
-335.159191616757)) ;
#32403 = CARTESIAN_POINT('Ctrl Pts',(-10.8443435223978,-16.1161676055536,
-335.159274754806)) ;
#32404 = CARTESIAN_POINT('Ctrl Pts',(-10.8480277253574,-16.1136879450963,
-335.159329110773)) ;
#32405 = CARTESIAN_POINT('Ctrl Pts',(-10.8548335498523,-16.1091038788023,
-335.159429579171)) ;
#32406 = CARTESIAN_POINT('Ctrl Pts',(-10.8579554106576,-16.1069998284352,
-335.159475686502)) ;
#32407 = CARTESIAN_POINT('Ctrl Pts',(-10.898833902465,-16.0794315371296,-335.160079718477)) ;
#32408 = CARTESIAN_POINT('Ctrl Pts',(-10.9365013771734,-16.0538355732736,
-335.160639585098)) ;
#32409 = CARTESIAN_POINT('Ctrl Pts',(-11.0408883486838,-15.9823642010369,
-335.162200311732)) ;
#32410 = CARTESIAN_POINT('Ctrl Pts',(-11.1074114268968,-15.9362038250601,
-335.163205262736)) ;
#32411 = CARTESIAN_POINT('Ctrl Pts',(-11.3203373948191,-15.7864735229052,
-335.166452672252)) ;
#32412 = CARTESIAN_POINT('Ctrl Pts',(-11.4655951856702,-15.6812917796276,
-335.168715156102)) ;
#32413 = CARTESIAN_POINT('Ctrl Pts',(-12.1000046014807,-15.2083854496675,
-335.178770583222)) ;
#32414 = CARTESIAN_POINT('Ctrl Pts',(-12.5730774465558,-14.8196769065436,
-335.186721695118)) ;
#32415 = CARTESIAN_POINT('Ctrl Pts',(-13.2616118452136,-14.1971933068906,
-335.198657295305)) ;
#32416 = CARTESIAN_POINT('Ctrl Pts',(-13.4909975254565,-13.9794003034446,
-335.20270268335)) ;
#32417 = CARTESIAN_POINT('Ctrl Pts',(-13.8378959456707,-13.6335393509121,
-335.208905543823)) ;
#32418 = CARTESIAN_POINT('Ctrl Pts',(-13.9591798504278,-13.5093322357607,
-335.211091352377)) ;
#32419 = CARTESIAN_POINT('Ctrl Pts',(-14.0857776466956,-13.3761577503329,
-335.213390126188)) ;
#32420 = CARTESIAN_POINT('Ctrl Pts',(-14.0927668114792,-13.3687939497635,
-335.213517092702)) ;
#32421 = CARTESIAN_POINT('Ctrl Pts',(-14.1059375361512,-13.3548954372635,
-335.21375646134)) ;
#32422 = CARTESIAN_POINT('Ctrl Pts',(-14.1121203362033,-13.3483619043902,
-335.213868873829)) ;
#32423 = CARTESIAN_POINT('Ctrl Pts',(-14.1238252084541,-13.3359758258083,
-335.21408176994)) ;
#32424 = CARTESIAN_POINT('Ctrl Pts',(-14.1293481867567,-13.3301241390663,
-335.214182261163)) ;
#32425 = CARTESIAN_POINT('Ctrl Pts',(-14.1398512429717,-13.3189821163414,
-335.214373433112)) ;
#32426 = CARTESIAN_POINT('Ctrl Pts',(-14.1448319917629,-13.3136924147134,
-335.214464119482)) ;
#32427 = CARTESIAN_POINT('Ctrl Pts',(-14.1543459035586,-13.3035769956617,
-335.21463739826)) ;
#32428 = CARTESIAN_POINT('Ctrl Pts',(-14.1588795693581,-13.2987517526085,
-335.214719994908)) ;
#32429 = CARTESIAN_POINT('Ctrl Pts',(-14.1675771576496,-13.2894853002144,
-335.214878498247)) ;
#32430 = CARTESIAN_POINT('Ctrl Pts',(-14.1717414610177,-13.2850444494795,
-335.214954408157)) ;
#32431 = CARTESIAN_POINT('Ctrl Pts',(-14.1797645855679,-13.276480451863,-335.215100698681)) ;
#32432 = CARTESIAN_POINT('Ctrl Pts',(-14.1836236977655,-13.2723575784792,
-335.215171081759)) ;
#32433 = CARTESIAN_POINT('Ctrl Pts',(-14.1910901372963,-13.2643738500591,
-335.215307289755)) ;
#32434 = CARTESIAN_POINT('Ctrl Pts',(-14.194697688281,-13.2605132048995,-335.215373116568)) ;
#32435 = CARTESIAN_POINT('Ctrl Pts',(-14.2017064989729,-13.2530065411227,
-335.215501035847)) ;
#32436 = CARTESIAN_POINT('Ctrl Pts',(-14.2051079309394,-13.2493606839114,
-335.215563129774)) ;
#32437 = CARTESIAN_POINT('Ctrl Pts',(-14.2117436624687,-13.2422426193297,
-335.215684293282)) ;
#32438 = CARTESIAN_POINT('Ctrl Pts',(-14.2149780942441,-13.2387705357059,
-335.215743363987)) ;
#32439 = CARTESIAN_POINT('Ctrl Pts',(-14.2213141558534,-13.2319639290496,
-335.215859104308)) ;
#32440 = CARTESIAN_POINT('Ctrl Pts',(-14.2244158859593,-13.2286294997788,
-335.215915774778)) ;
#32441 = CARTESIAN_POINT('Ctrl Pts',(-14.2305172902006,-13.2220657266557,
-335.216027273568)) ;
#32442 = CARTESIAN_POINT('Ctrl Pts',(-14.2335170383797,-13.2188364520051,
-335.216082102518)) ;
#32443 = CARTESIAN_POINT('Ctrl Pts',(-14.2394427023473,-13.2124530287226,
-335.21619043207)) ;
#32444 = CARTESIAN_POINT('Ctrl Pts',(-14.2423686698649,-13.2092989284551,
-335.216243933112)) ;
#32445 = CARTESIAN_POINT('Ctrl Pts',(-14.2481734218118,-13.2030374189185,
-335.216350092709)) ;
#32446 = CARTESIAN_POINT('Ctrl Pts',(-14.2510522381442,-13.1999300395523,
-335.216402751533)) ;
#32447 = CARTESIAN_POINT('Ctrl Pts',(-14.256788659448,-13.1937341122544,-335.216507700916)) ;
#32448 = CARTESIAN_POINT('Ctrl Pts',(-14.2596462762036,-13.1906455786874,
-335.216559991557)) ;
#32449 = CARTESIAN_POINT('Ctrl Pts',(-14.3441951202398,-13.0992049719767,
-335.218107413801)) ;
#32450 = CARTESIAN_POINT('Ctrl Pts',(-14.4250646849292,-13.0100965954714,
-335.21959547102)) ;
#32451 = CARTESIAN_POINT('Ctrl Pts',(-14.5892261258045,-12.8257983287526,
-335.222632888508)) ;
#32452 = CARTESIAN_POINT('Ctrl Pts',(-14.6724267779877,-12.7305347182748,
-335.224181422136)) ;
#32453 = CARTESIAN_POINT('Ctrl Pts',(-14.8701579558119,-12.4996217037103,
-335.227884708995)) ;
#32454 = CARTESIAN_POINT('Ctrl Pts',(-14.9837708873418,-12.3632014659998,
-335.230031661985)) ;
#32455 = CARTESIAN_POINT('Ctrl Pts',(-15.5607946918287,-11.6507034236138,
-335.241046953763)) ;
#32456 = CARTESIAN_POINT('Ctrl Pts',(-15.9929117975076,-11.0500676134274,
-335.249649783577)) ;
#32457 = CARTESIAN_POINT('Ctrl Pts',(-16.6075928916345,-10.083809877613,-335.263037228399)) ;
#32458 = CARTESIAN_POINT('Ctrl Pts',(-16.8146593927414,-9.7346079187652,-335.267796674189)) ;
#32459 = CARTESIAN_POINT('Ctrl Pts',(-17.068262448583,-9.27465833767664,-335.274095118541)) ;
#32460 = CARTESIAN_POINT('Ctrl Pts',(-17.1249266482483,-9.16961054373564,
-335.275535733547)) ;
#32461 = CARTESIAN_POINT('Ctrl Pts',(-17.2133087105605,-9.00208510118727,
-335.277841203368)) ;
#32462 = CARTESIAN_POINT('Ctrl Pts',(-17.245662926587,-8.93994648477509,-335.278698091801)) ;
#32463 = CARTESIAN_POINT('Ctrl Pts',(-17.3063456584251,-8.82184555696794,
-335.280331171837)) ;
#32464 = CARTESIAN_POINT('Ctrl Pts',(-17.3347406502135,-8.76591841501513,
-335.281106378047)) ;
#32465 = CARTESIAN_POINT('Ctrl Pts',(-17.4152014752633,-8.60552189644457,
-335.283333830865)) ;
#32466 = CARTESIAN_POINT('Ctrl Pts',(-17.466597188511,-8.50071950654463,-335.284794295983)) ;
#32467 = CARTESIAN_POINT('Ctrl Pts',(-17.6721569060288,-8.07182118795383,
-335.290782144169)) ;
#32468 = CARTESIAN_POINT('Ctrl Pts',(-17.8182695260716,-7.74394584960671,
-335.295383716441)) ;
#32469 = CARTESIAN_POINT('Ctrl Pts',(-18.159707420861,-6.91685259050838,-335.306907810768)) ;
#32470 = CARTESIAN_POINT('Ctrl Pts',(-18.3436135433347,-6.41324156320669,
-335.313846308809)) ;
#32471 = CARTESIAN_POINT('Ctrl Pts',(-18.5538387942488,-5.75412902052858,
-335.322675024848)) ;
#32472 = CARTESIAN_POINT('Ctrl Pts',(-18.599426835328,-5.60502062960723,-335.324656587289)) ;
#32473 = CARTESIAN_POINT('Ctrl Pts',(-18.7068627434282,-5.23786913791506,
-335.329493847755)) ;
#32474 = CARTESIAN_POINT('Ctrl Pts',(-18.7666993003637,-5.01926134466978,
-335.332337884868)) ;
#32475 = CARTESIAN_POINT('Ctrl Pts',(-18.8560478070511,-4.66886545578968,
-335.336836107212)) ;
#32476 = CARTESIAN_POINT('Ctrl Pts',(-18.8880344876731,-4.53773035761718,
-335.338506263097)) ;
#32477 = CARTESIAN_POINT('Ctrl Pts',(-18.9473392464463,-4.28310105391946,
-335.341723810595)) ;
#32478 = CARTESIAN_POINT('Ctrl Pts',(-18.9748230942038,-4.15965235934368,
-335.343272230829)) ;
#32479 = CARTESIAN_POINT('Ctrl Pts',(-19.0379699798092,-3.86235877558695,
-335.346974593721)) ;
#32480 = CARTESIAN_POINT('Ctrl Pts',(-19.0724600988067,-3.68827631412663,
-335.349120746758)) ;
#32481 = CARTESIAN_POINT('Ctrl Pts',(-19.2383650879695,-2.78623552285682,
-335.360140046453)) ;
#32482 = CARTESIAN_POINT('Ctrl Pts',(-19.3305051179945,-2.0516753747047,-335.368747317222)) ;
#32483 = CARTESIAN_POINT('Ctrl Pts',(-19.4079650940754,-0.908898808793932,
-335.3821371249)) ;
#32484 = CARTESIAN_POINT('Ctrl Pts',(-19.4227137908521,-0.503382222379939,
-335.38689436078)) ;
#32485 = CARTESIAN_POINT('Ctrl Pts',(-19.4253544977313,0.021627213401816,
-335.393190249366)) ;
#32486 = CARTESIAN_POINT('Ctrl Pts',(-19.4248550878299,0.140960466288975,
-335.394630607076)) ;
#32487 = CARTESIAN_POINT('Ctrl Pts',(-19.4223174750438,0.330327465152303,
-335.396935765745)) ;
#32488 = CARTESIAN_POINT('Ctrl Pts',(-19.4209999186418,0.400367943033998,
-335.397792603982)) ;
#32489 = CARTESIAN_POINT('Ctrl Pts',(-19.4177845371009,0.533107112279973,
-335.39942567836)) ;
#32490 = CARTESIAN_POINT('Ctrl Pts',(-19.4159618319896,0.595806722133799,
-335.400200929935)) ;
#32491 = CARTESIAN_POINT('Ctrl Pts',(-19.4098779021935,0.775173564898709,
-335.402428681672)) ;
#32492 = CARTESIAN_POINT('Ctrl Pts',(-19.4048685757636,0.891812610105692,
-335.403889403669)) ;
#32493 = CARTESIAN_POINT('Ctrl Pts',(-19.3801629671762,1.36708007932384,-335.409880992972)) ;
#32494 = CARTESIAN_POINT('Ctrl Pts',(-19.3515735088423,1.72517434836294,-335.414486164467)) ;
#32495 = CARTESIAN_POINT('Ctrl Pts',(-19.2556494408886,2.61487141692982,-335.426011064085)) ;
#32496 = CARTESIAN_POINT('Ctrl Pts',(-19.1762188862869,3.14487184893335,-335.432946655477)) ;
#32497 = CARTESIAN_POINT('Ctrl Pts',(-19.0455262681809,3.82398398899898,-335.441772099194)) ;
#32498 = CARTESIAN_POINT('Ctrl Pts',(-19.0142262467662,3.97669771167166,-335.443753228237)) ;
#32499 = CARTESIAN_POINT('Ctrl Pts',(-18.932925213169,4.35043845825549,-335.44858963212)) ;
#32500 = CARTESIAN_POINT('Ctrl Pts',(-18.8808881900747,4.57099916093684,-335.451433247436)) ;
#32501 = CARTESIAN_POINT('Ctrl Pts',(-18.7917178537821,4.92140041614273,-335.455930978082)) ;
#32502 = CARTESIAN_POINT('Ctrl Pts',(-18.7570690824531,5.05185128919522,-335.457601057752)) ;
#32503 = CARTESIAN_POINT('Ctrl Pts',(-18.6873254822222,5.30381807260058,-335.460818559719)) ;
#32504 = CARTESIAN_POINT('Ctrl Pts',(-18.6523978254009,5.42537328095011,-335.462367009511)) ;
#32505 = CARTESIAN_POINT('Ctrl Pts',(-18.5656095485827,5.71666551737828,-335.466069613333)) ;
#32506 = CARTESIAN_POINT('Ctrl Pts',(-18.5126048808818,5.88604988075187,-335.468215974972)) ;
#32507 = CARTESIAN_POINT('Ctrl Pts',(-18.2267532672315,6.75744876962215,-335.479234226507)) ;
#32508 = CARTESIAN_POINT('Ctrl Pts',(-17.9562710382641,7.44647428341406,-335.487840336432)) ;
#32509 = CARTESIAN_POINT('Ctrl Pts',(-17.4775899549772,8.48699573708209,-335.501229527281)) ;
#32510 = CARTESIAN_POINT('Ctrl Pts',(-17.2965115328921,8.85019404269283,-335.505987341714)) ;
#32511 = CARTESIAN_POINT('Ctrl Pts',(-17.0476270811357,9.31253334822059,-335.512283899406)) ;
#32512 = CARTESIAN_POINT('Ctrl Pts',(-16.9900939650053,9.41708943659527,-335.513724324487)) ;
#32513 = CARTESIAN_POINT('Ctrl Pts',(-16.8972645931346,9.58216999233022,-335.516029564628)) ;
#32514 = CARTESIAN_POINT('Ctrl Pts',(-16.8625980185336,9.64304519079513,-335.516886416007)) ;
#32515 = CARTESIAN_POINT('Ctrl Pts',(-16.7962688043851,9.75806915620797,-335.518519491861)) ;
#32516 = CARTESIAN_POINT('Ctrl Pts',(-16.7646717087004,9.81225467948012,-335.519294731551)) ;
#32517 = CARTESIAN_POINT('Ctrl Pts',(-16.6735190100144,9.96684588149034,-335.521522404988)) ;
#32518 = CARTESIAN_POINT('Ctrl Pts',(-16.6133200368016,10.0668689421253,-335.522983059698)) ;
#32519 = CARTESIAN_POINT('Ctrl Pts',(-16.3642868687349,10.4723296390465,-335.528973668722)) ;
#32520 = CARTESIAN_POINT('Ctrl Pts',(-16.1679021706417,10.7730455960562,-335.533577897087)) ;
#32521 = CARTESIAN_POINT('Ctrl Pts',(-15.6580332516087,11.5084162372768,-335.545102585639)) ;
#32522 = CARTESIAN_POINT('Ctrl Pts',(-15.3346865724285,11.9358719467092,-335.552038938598)) ;
#32523 = CARTESIAN_POINT('Ctrl Pts',(-14.8949776330543,12.4697461248486,-335.560865239719)) ;
#32524 = CARTESIAN_POINT('Ctrl Pts',(-14.7944249329524,12.5888807319695,-335.562846482339)) ;
#32525 = CARTESIAN_POINT('Ctrl Pts',(-14.5442147919297,12.8781905521565,-335.567683110706)) ;
#32526 = CARTESIAN_POINT('Ctrl Pts',(-14.3929925006144,13.0469821398511,-335.570526836563)) ;
#32527 = CARTESIAN_POINT('Ctrl Pts',(-14.1470423158832,13.3120259946588,-335.57502469607)) ;
#32528 = CARTESIAN_POINT('Ctrl Pts',(-14.0542043784957,13.4100030468764,-335.576694795714)) ;
#32529 = CARTESIAN_POINT('Ctrl Pts',(-13.8724130162241,13.5978960415927,-335.579912309609)) ;
#32530 = CARTESIAN_POINT('Ctrl Pts',(-13.7835876218738,13.687926503664,-335.58146075165)) ;
#32531 = CARTESIAN_POINT('Ctrl Pts',(-13.5680190044615,13.9021933951095,-335.585163292311)) ;
#32532 = CARTESIAN_POINT('Ctrl Pts',(-13.4404399625115,14.0255728810238,-335.587309599264)) ;
#32533 = CARTESIAN_POINT('Ctrl Pts',(-12.7725118632409,14.6540311459201,-335.598328125349)) ;
#32534 = CARTESIAN_POINT('Ctrl Pts',(-12.2053262599333,15.129695942914,-335.606934539384)) ;
#32535 = CARTESIAN_POINT('Ctrl Pts',(-11.2871592626856,15.8144007879201,-335.620323891879)) ;
#32536 = CARTESIAN_POINT('Ctrl Pts',(-10.9543967132614,16.0466952259967,-335.625081554806)) ;
#32537 = CARTESIAN_POINT('Ctrl Pts',(-10.5146619542784,16.3336079936501,-335.63137793728)) ;
#32538 = CARTESIAN_POINT('Ctrl Pts',(-10.4141195227223,16.3978956151936,-335.632818344719)) ;
#32539 = CARTESIAN_POINT('Ctrl Pts',(-10.2536263069596,16.4984447754482,-335.635123563526)) ;
#32540 = CARTESIAN_POINT('Ctrl Pts',(-10.19406065239,16.5353155355663,-335.635980411464)) ;
#32541 = CARTESIAN_POINT('Ctrl Pts',(-10.0807848215183,16.6045878244281,-335.637613486936)) ;
#32542 = CARTESIAN_POINT('Ctrl Pts',(-10.0271146131637,16.6370529830363,-335.638388729742)) ;
#32543 = CARTESIAN_POINT('Ctrl Pts',(-9.87310919136187,16.7291950858579,-335.640616423696)) ;
#32544 = CARTESIAN_POINT('Ctrl Pts',(-9.77239205851055,16.7882282186189,-335.642077096036)) ;
#32545 = CARTESIAN_POINT('Ctrl Pts',(-9.35970890294749,17.0251412801353,-335.648067961863)) ;
#32546 = CARTESIAN_POINT('Ctrl Pts',(-9.04337103664606,17.1952617273774,-335.652672437296)) ;
#32547 = CARTESIAN_POINT('Ctrl Pts',(-8.2438164806741,17.5970771228733,-335.664197181086)) ;
#32548 = CARTESIAN_POINT('Ctrl Pts',(-7.75538450843575,17.8177340412732,-335.671133334483)) ;
#32549 = CARTESIAN_POINT('Ctrl Pts',(-7.11386087053336,18.0761696691357,-335.679959410929)) ;
#32550 = CARTESIAN_POINT('Ctrl Pts',(-6.96856784008059,18.1326773732957,-335.681940623787)) ;
#32551 = CARTESIAN_POINT('Ctrl Pts',(-6.61044241615653,18.2670201688964,-335.686777193329)) ;
#32552 = CARTESIAN_POINT('Ctrl Pts',(-6.39689785167203,18.3428916186177,-335.68962089022)) ;
#32553 = CARTESIAN_POINT('Ctrl Pts',(-6.05412096514747,18.4579647198664,-335.694118715964)) ;
#32554 = CARTESIAN_POINT('Ctrl Pts',(-5.9257230647847,18.4995850893973,-335.695788810376)) ;
#32555 = CARTESIAN_POINT('Ctrl Pts',(-5.67619444389009,18.5776057750132,-335.699006321153)) ;
#32556 = CARTESIAN_POINT('Ctrl Pts',(-5.55512135805032,18.6141678955278,-335.70055476523)) ;
#32557 = CARTESIAN_POINT('Ctrl Pts',(-5.2633124822417,18.6991888339239,-335.704257322457)) ;
#32558 = CARTESIAN_POINT('Ctrl Pts',(-5.0922527103062,18.7464952402663,-335.706403643753)) ;
#32559 = CARTESIAN_POINT('Ctrl Pts',(-4.0807826751397,19.0113501298913,-335.718965577428)) ;
#32560 = CARTESIAN_POINT('Ctrl Pts',(-3.22720415501608,19.1747065159298,-335.728993928958)) ;
#32561 = CARTESIAN_POINT('Ctrl Pts',(-2.14653114354692,19.3072972921911,-335.741774078026)) ;
#32562 = CARTESIAN_POINT('Ctrl Pts',(-1.92705175389449,19.3304370356936,-335.744377046707)) ;
#32563 = CARTESIAN_POINT('Ctrl Pts',(-1.55469452571458,19.3632899309323,-335.748833489649)) ;
#32564 = CARTESIAN_POINT('Ctrl Pts',(-1.40200925360456,19.3749436631064,-335.750672366312)) ;
#32565 = CARTESIAN_POINT('Ctrl Pts',(-1.17283058990149,19.3897124859085,-335.753458936906)) ;
#32566 = CARTESIAN_POINT('Ctrl Pts',(-1.09643039862242,19.3941826907074,-335.754392290496)) ;
#32567 = CARTESIAN_POINT('Ctrl Pts',(-0.953578611560748,19.4016941943485,
-335.756147210947)) ;
#32568 = CARTESIAN_POINT('Ctrl Pts',(-0.887134055795053,19.4048458615229,
-335.75696754852)) ;
#32569 = CARTESIAN_POINT('Ctrl Pts',(-0.717372114571747,19.4120244373768,
-335.759072973522)) ;
#32570 = CARTESIAN_POINT('Ctrl Pts',(-0.614036384668021,19.4155678460163,
-335.760363470728)) ;
#32571 = CARTESIAN_POINT('Ctrl Pts',(-0.145464010118424,19.4278907322384,
-335.766248073594)) ;
#32572 = CARTESIAN_POINT('Ctrl Pts',(0.219947175243785,19.4271902351739,-335.770926314856)) ;
#32573 = CARTESIAN_POINT('Ctrl Pts',(1.00693950659581,19.4034736899051,-335.78106120025)) ;
#32574 = CARTESIAN_POINT('Ctrl Pts',(1.42823334259071,19.3770190790373,-335.786522476523)) ;
#32575 = CARTESIAN_POINT('Ctrl Pts',(2.13771006504435,19.3092031544045,-335.795671930856)) ;
#32576 = CARTESIAN_POINT('Ctrl Pts',(2.42643280787893,19.2750500662543,-335.799382610356)) ;
#32577 = CARTESIAN_POINT('Ctrl Pts',(2.93790715458167,19.2028729964967,-335.805913599525)) ;
#32578 = CARTESIAN_POINT('Ctrl Pts',(3.16096675878464,19.167418166897,-335.808747513376)) ;
#32579 = CARTESIAN_POINT('Ctrl Pts',(3.51613095889253,19.1045970483289,-335.81323393383)) ;
#32580 = CARTESIAN_POINT('Ctrl Pts',(3.64865628121196,19.0797304147725,-335.81490225981)) ;
#32581 = CARTESIAN_POINT('Ctrl Pts',(3.90502407913752,19.0288576192373,-335.818118721493)) ;
#32582 = CARTESIAN_POINT('Ctrl Pts',(4.02889258391949,19.0030171275002,-335.819667858727)) ;
#32583 = CARTESIAN_POINT('Ctrl Pts',(4.32627361890008,18.9379414122439,-335.823376048315)) ;
#32584 = CARTESIAN_POINT('Ctrl Pts',(4.49951697778285,18.8975293478571,-335.825527244058)) ;
#32585 = CARTESIAN_POINT('Ctrl Pts',(5.05450323104763,18.7600044742503,-335.832396258865)) ;
#32586 = CARTESIAN_POINT('Ctrl Pts',(5.43385589438791,18.653658670498,-335.837055457851)) ;
#32587 = CARTESIAN_POINT('Ctrl Pts',(6.33344971196237,18.3716979848589,-335.848120535167)) ;
#32588 = CARTESIAN_POINT('Ctrl Pts',(6.84999272707859,18.185419165304,-335.854483788144)) ;
#32589 = CARTESIAN_POINT('Ctrl Pts',(7.4773912529085,17.9286335358407,-335.862473726898)) ;
#32590 = CARTESIAN_POINT('Ctrl Pts',(7.59634010366043,17.8785597125019,-335.86400083869)) ;
#32591 = CARTESIAN_POINT('Ctrl Pts',(7.86475938980588,17.7624010395596,-335.867482496846)) ;
#32592 = CARTESIAN_POINT('Ctrl Pts',(8.01391258620065,17.6956078128295,-335.869442425844)) ;
#32593 = CARTESIAN_POINT('Ctrl Pts',(8.23329279274307,17.5940231848689,-335.872373713308)) ;
#32594 = CARTESIAN_POINT('Ctrl Pts',(8.30418081290992,17.5606760418493,-335.873328490985)) ;
#32595 = CARTESIAN_POINT('Ctrl Pts',(8.43504732675797,17.498144200191,-335.875106815385)) ;
#32596 = CARTESIAN_POINT('Ctrl Pts',(8.49508084183715,17.469077689153,-335.875928915506)) ;
#32597 = CARTESIAN_POINT('Ctrl Pts',(8.64487238338976,17.3955981586829,-335.877995267685)) ;
#32598 = CARTESIAN_POINT('Ctrl Pts',(8.7344388651488,17.3507991601208,-335.879244348401)) ;
#32599 = CARTESIAN_POINT('Ctrl Pts',(9.15923585859752,17.1342030911272,-335.885225994469)) ;
#32600 = CARTESIAN_POINT('Ctrl Pts',(9.48976834250732,16.9533717272254,-335.890050243089)) ;
#32601 = CARTESIAN_POINT('Ctrl Pts',(10.1790623279319,16.5497872254017,-335.90033326609)) ;
#32602 = CARTESIAN_POINT('Ctrl Pts',(10.5362449572835,16.3247146916703,-335.90579499952)) ;
#32603 = CARTESIAN_POINT('Ctrl Pts',(11.1246149894576,15.9266036031314,-335.914913253124)) ;
#32604 = CARTESIAN_POINT('Ctrl Pts',(11.3597914538405,15.7597239683559,-335.918592986358)) ;
#32605 = CARTESIAN_POINT('Ctrl Pts',(11.7713929167244,15.4536525284395,-335.925077323906)) ;
#32606 = CARTESIAN_POINT('Ctrl Pts',(11.9492819863367,15.3165181403209,-335.927895229523)) ;
#32607 = CARTESIAN_POINT('Ctrl Pts',(12.2299210674897,15.0923084892762,-335.932362983197)) ;
#32608 = CARTESIAN_POINT('Ctrl Pts',(12.3342127994981,15.0071962580834,-335.934028412512)) ;
#32609 = CARTESIAN_POINT('Ctrl Pts',(12.5348849984341,14.8399231725124,-335.937243187685)) ;
#32610 = CARTESIAN_POINT('Ctrl Pts',(12.6313633170866,14.7578901774911,-335.938793491881)) ;
#32611 = CARTESIAN_POINT('Ctrl Pts',(12.8405959111588,14.5764302356289,-335.942166946575)) ;
#32612 = CARTESIAN_POINT('Ctrl Pts',(12.9530121778428,14.4766258971537,-335.943986766317)) ;
#32613 = CARTESIAN_POINT('Ctrl Pts',(13.4061798029301,14.0647940922574,-335.951357962422)) ;
#32614 = CARTESIAN_POINT('Ctrl Pts',(13.7369062771369,13.7419611781387,-335.956816230053)) ;
#32615 = CARTESIAN_POINT('Ctrl Pts',(14.1323392970849,13.3274117999146,-335.963530527086)) ;
#32616 = CARTESIAN_POINT('Ctrl Pts',(14.208182975782,13.2465261796419,-335.964827616629)) ;
#32617 = CARTESIAN_POINT('Ctrl Pts',(14.576358653743,12.8470748738478,-335.971177050621)) ;
#32618 = CARTESIAN_POINT('Ctrl Pts',(14.8586907523923,12.519459757042,-335.976208764485)) ;
#32619 = CARTESIAN_POINT('Ctrl Pts',(15.2303499169125,12.0578912903062,-335.983209849402)) ;
#32620 = CARTESIAN_POINT('Ctrl Pts',(15.3292969887696,11.9318462395133,-335.985113483242)) ;
#32621 = CARTESIAN_POINT('Ctrl Pts',(15.5010153825124,11.7074383465584,-335.988500001492)) ;
#32622 = CARTESIAN_POINT('Ctrl Pts',(15.5744381709813,11.6095850967504,-335.989975834619)) ;
#32623 = CARTESIAN_POINT('Ctrl Pts',(15.6887957362159,11.4541391740718,-335.992323962761)) ;
#32624 = CARTESIAN_POINT('Ctrl Pts',(15.7303490777553,11.3970054729745,-335.993187786119)) ;
#32625 = CARTESIAN_POINT('Ctrl Pts',(15.8079406133976,11.2890883627189,-335.994822083267)) ;
#32626 = CARTESIAN_POINT('Ctrl Pts',(15.8440480979892,11.2383558564305,-335.995591462222)) ;
#32627 = CARTESIAN_POINT('Ctrl Pts',(15.9456335041618,11.0941615034446,-335.997780228086)) ;
#32628 = CARTESIAN_POINT('Ctrl Pts',(16.0105326151956,11.0002951158325,-335.999207406125)) ;
#32629 = CARTESIAN_POINT('Ctrl Pts',(16.3855850565694,10.447489843194,-336.007613311568)) ;
#32630 = CARTESIAN_POINT('Ctrl Pts',(16.6768208230405,9.97602565532701,-336.014778137021)) ;
#32631 = CARTESIAN_POINT('Ctrl Pts',(17.1481353942045,9.13458374899171,-336.027219344601)) ;
#32632 = CARTESIAN_POINT('Ctrl Pts',(17.3373560548407,8.77013419506925,-336.032503228553)) ;
#32633 = CARTESIAN_POINT('Ctrl Pts',(17.6365602947772,8.14625903012451,-336.041301732381)) ;
#32634 = CARTESIAN_POINT('Ctrl Pts',(17.7527075687761,7.88994104496799,-336.044849563252)) ;
#32635 = CARTESIAN_POINT('Ctrl Pts',(17.9199542184514,7.49844667179827,-336.050160207248)) ;
#32636 = CARTESIAN_POINT('Ctrl Pts',(17.9751810094003,7.36507497812842,-336.051950868857)) ;
#32637 = CARTESIAN_POINT('Ctrl Pts',(18.0751527732988,7.11582070932191,-336.055263137615)) ;
#32638 = CARTESIAN_POINT('Ctrl Pts',(18.1202826986435,7.00010050735837,-336.056787352189)) ;
#32639 = CARTESIAN_POINT('Ctrl Pts',(18.2203416760889,6.736080600315,-336.060234938578)) ;
#32640 = CARTESIAN_POINT('Ctrl Pts',(18.2745758429249,6.5875268880064,-336.062153447982)) ;
#32641 = CARTESIAN_POINT('Ctrl Pts',(18.442947427211,6.10824955982248,-336.068279194138)) ;
#32642 = CARTESIAN_POINT('Ctrl Pts',(18.5499664591244,5.77509892452837,-336.072439164663)) ;
#32643 = CARTESIAN_POINT('Ctrl Pts',(18.7203733115832,5.19087480740729,-336.0796116639)) ;
#32644 = CARTESIAN_POINT('Ctrl Pts',(18.7878475444258,4.94108722586867,-336.08264044136)) ;
#32645 = CARTESIAN_POINT('Ctrl Pts',(18.9926711719856,4.11785321353048,-336.092553859892)) ;
#32646 = CARTESIAN_POINT('Ctrl Pts',(19.1089044987125,3.53949682372526,-336.099402211662)) ;
#32647 = CARTESIAN_POINT('Ctrl Pts',(19.2164633242485,2.84110104341549,-336.107879963591)) ;
#32648 = CARTESIAN_POINT('Ctrl Pts',(19.2332294135482,2.72528972725188,-336.109292946476)) ;
#32649 = CARTESIAN_POINT('Ctrl Pts',(19.2582974932836,2.54036355951316,-336.111565048673)) ;
#32650 = CARTESIAN_POINT('Ctrl Pts',(19.2672761955969,2.47134322898719,-336.112416592098)) ;
#32651 = CARTESIAN_POINT('Ctrl Pts',(19.2836898911206,2.33963959939585,-336.114049360738)) ;
#32652 = CARTESIAN_POINT('Ctrl Pts',(19.2911906764554,2.27696542472912,-336.114829691825)) ;
#32653 = CARTESIAN_POINT('Ctrl Pts',(19.3119488024704,2.09604761226497,-336.117090733073)) ;
#32654 = CARTESIAN_POINT('Ctrl Pts',(19.3244253751792,1.9777173707613,-336.118580037919)) ;
#32655 = CARTESIAN_POINT('Ctrl Pts',(19.3806467667172,1.3930360476835,-336.125978195184)) ;
#32656 = CARTESIAN_POINT('Ctrl Pts',(19.408601031983,0.925323421021146,-336.132015947265)) ;
#32657 = CARTESIAN_POINT('Ctrl Pts',(19.4304207575132,-0.00175656256659662,
-336.143979551693)) ;
#32658 = CARTESIAN_POINT('Ctrl Pts',(19.4249557886001,-0.460812106955017,
-336.149901328882)) ;
#32659 = CARTESIAN_POINT('Ctrl Pts',(19.3964656964208,-1.06217678930648,-336.157569146231)) ;
#32660 = CARTESIAN_POINT('Ctrl Pts',(19.3881148957429,-1.20503190508095,-336.159384351076)) ;
#32661 = CARTESIAN_POINT('Ctrl Pts',(19.3633566612534,-1.56100175775195,-336.163889286857)) ;
#32662 = CARTESIAN_POINT('Ctrl Pts',(19.3450087715052,-1.77396266488482,-336.166567950269)) ;
#32663 = CARTESIAN_POINT('Ctrl Pts',(19.3095838071213,-2.11853612078625,-336.17087317959)) ;
#32664 = CARTESIAN_POINT('Ctrl Pts',(19.2946660155655,-2.2503523066438,-336.172513311891)) ;
#32665 = CARTESIAN_POINT('Ctrl Pts',(19.2629184547589,-2.50729636778672,-336.175697296077)) ;
#32666 = CARTESIAN_POINT('Ctrl Pts',(19.24621667837,-2.63243349173348,-336.177241897102)) ;
#32667 = CARTESIAN_POINT('Ctrl Pts',(19.2063885002707,-2.91016914352994,-336.180657512761)) ;
#32668 = CARTESIAN_POINT('Ctrl Pts',(19.1826608814919,-3.06267289414458,-336.182524547727)) ;
#32669 = CARTESIAN_POINT('Ctrl Pts',(19.0655550987178,-3.76049392732415,-336.191035074715)) ;
#32670 = CARTESIAN_POINT('Ctrl Pts',(18.9507238557215,-4.30194988497588,-336.197539000283)) ;
#32671 = CARTESIAN_POINT('Ctrl Pts',(18.6791969513373,-5.35785465170593,-336.210283752651)) ;
#32672 = CARTESIAN_POINT('Ctrl Pts',(18.5239461474595,-5.87217350887204,-336.216522294436)) ;
#32673 = CARTESIAN_POINT('Ctrl Pts',(18.2945098342491,-6.53204827840809,-336.22484090314)) ;
#32674 = CARTESIAN_POINT('Ctrl Pts',(18.2395302320901,-6.68403183406783,-336.226779640034)) ;
#32675 = CARTESIAN_POINT('Ctrl Pts',(18.1552036921936,-6.9083494659383,-336.229685651692)) ;
#32676 = CARTESIAN_POINT('Ctrl Pts',(18.1273070387683,-6.98122145118926,-336.230636748208)) ;
#32677 = CARTESIAN_POINT('Ctrl Pts',(18.074718553917,-7.11615310254565,-336.232412524771)) ;
#32678 = CARTESIAN_POINT('Ctrl Pts',(18.0501443023728,-7.17825719857534,-336.233235812079)) ;
#32679 = CARTESIAN_POINT('Ctrl Pts',(17.9876865531158,-7.33375171384866,-336.2353113631)) ;
#32680 = CARTESIAN_POINT('Ctrl Pts',(17.9493956519603,-7.42697633109431,-336.236568553163)) ;
#32681 = CARTESIAN_POINT('Ctrl Pts',(17.7685866806301,-7.85761479207375,-336.242428491236)) ;
#32682 = CARTESIAN_POINT('Ctrl Pts',(17.6172689575329,-8.1912524325871,-336.247117288097)) ;
#32683 = CARTESIAN_POINT('Ctrl Pts',(17.2583880445812,-8.92652727186592,-336.25764767693)) ;
#32684 = CARTESIAN_POINT('Ctrl Pts',(17.0460545886829,-9.32560296489143,-336.263497832938)) ;
#32685 = CARTESIAN_POINT('Ctrl Pts',(16.7209311660354,-9.88839251163785,-336.271833471019)) ;
#32686 = CARTESIAN_POINT('Ctrl Pts',(16.6192486144482,-10.0583508164693,-336.274363010264)) ;
#32687 = CARTESIAN_POINT('Ctrl Pts',(16.3752969091566,-10.4523047834956,-336.280246521599)) ;
#32688 = CARTESIAN_POINT('Ctrl Pts',(16.2310015222702,-10.6749994920816,-336.283587770418)) ;
#32689 = CARTESIAN_POINT('Ctrl Pts',(16.002703164668,-11.0120026223252,-336.28866190468)) ;
#32690 = CARTESIAN_POINT('Ctrl Pts',(15.9219350634168,-11.1284632468303,-336.290418869715)) ;
#32691 = CARTESIAN_POINT('Ctrl Pts',(15.7678058116543,-11.3455910879825,-336.293701204069)) ;
#32692 = CARTESIAN_POINT('Ctrl Pts',(15.694736780256,-11.4464568620659,-336.295228767429)) ;
#32693 = CARTESIAN_POINT('Ctrl Pts',(15.5258939742687,-11.6748739117895,-336.298695174043)) ;
#32694 = CARTESIAN_POINT('Ctrl Pts',(15.4295090456217,-11.8019623478959,-336.300628987119)) ;
#32695 = CARTESIAN_POINT('Ctrl Pts',(15.0891799257369,-12.2394074793645,-336.307308146187)) ;
#32696 = CARTESIAN_POINT('Ctrl Pts',(14.8373491696948,-12.5435049673477,-336.311990059341)) ;
#32697 = CARTESIAN_POINT('Ctrl Pts',(14.1922744002128,-13.275833017342,-336.323463519854)) ;
#32698 = CARTESIAN_POINT('Ctrl Pts',(13.788742799292,-13.6944866733356,-336.33019611587)) ;
#32699 = CARTESIAN_POINT('Ctrl Pts',(13.2708181332957,-14.185682969699,-336.338604907545)) ;
#32700 = CARTESIAN_POINT('Ctrl Pts',(13.1736534573154,-14.2759612558908,-336.340173492077)) ;
#32701 = CARTESIAN_POINT('Ctrl Pts',(12.9524962889447,-14.4772636366326,-336.343731983731)) ;
#32702 = CARTESIAN_POINT('Ctrl Pts',(12.8279861534573,-14.5877035072095,-336.345727228018)) ;
#32703 = CARTESIAN_POINT('Ctrl Pts',(12.6424151263889,-14.7480908029304,-336.348700579874)) ;
#32704 = CARTESIAN_POINT('Ctrl Pts',(12.5824444545552,-14.799288296626,-336.349661426106)) ;
#32705 = CARTESIAN_POINT('Ctrl Pts',(12.4712773116559,-14.8930284985256,-336.351444083941)) ;
#32706 = CARTESIAN_POINT('Ctrl Pts',(12.4201708051575,-14.9356758393262,-336.352264360868)) ;
#32707 = CARTESIAN_POINT('Ctrl Pts',(12.2924063434799,-15.0411834289602,-336.354316186417)) ;
#32708 = CARTESIAN_POINT('Ctrl Pts',(12.2154845131321,-15.1037210887828,-336.35555240904)) ;
#32709 = CARTESIAN_POINT('Ctrl Pts',(11.8812327865812,-15.371244874611,-336.360921790152)) ;
#32710 = CARTESIAN_POINT('Ctrl Pts',(11.619197284578,-15.5702638142426,-336.365124064473)) ;
#32711 = CARTESIAN_POINT('Ctrl Pts',(11.2130320402589,-15.8627855616346,-336.371557307521)) ;
#32712 = CARTESIAN_POINT('Ctrl Pts',(11.072507449104,-15.9611914363373,-336.373769151282)) ;
#32713 = CARTESIAN_POINT('Ctrl Pts',(10.5476251998511,-16.3184855137077,-336.381960337636)) ;
#32714 = CARTESIAN_POINT('Ctrl Pts',(10.1553433565598,-16.5654571154243,-336.387940941636)) ;
#32715 = CARTESIAN_POINT('Ctrl Pts',(9.63016404898978,-16.8704259850824,-336.395676840117)) ;
#32716 = CARTESIAN_POINT('Ctrl Pts',(9.50492342080253,-16.9413034726601,-336.3975025033)) ;
#32717 = CARTESIAN_POINT('Ctrl Pts',(9.19101110953334,-17.1143792398034,-336.402028541279)) ;
#32718 = CARTESIAN_POINT('Ctrl Pts',(9.00141174488035,-17.2148554687064,-336.404717807719)) ;
#32719 = CARTESIAN_POINT('Ctrl Pts',(8.69182841190599,-17.3724028416349,-336.409035419336)) ;
#32720 = CARTESIAN_POINT('Ctrl Pts',(8.57285555503001,-17.4314201751824,-336.410677480818)) ;
#32721 = CARTESIAN_POINT('Ctrl Pts',(8.33970372192579,-17.5441124569692,-336.413862357455)) ;
#32722 = CARTESIAN_POINT('Ctrl Pts',(8.22558847166244,-17.5979042620308,-336.415405952612)) ;
#32723 = CARTESIAN_POINT('Ctrl Pts',(7.97108788755957,-17.7148547123622,-336.41881577427)) ;
#32724 = CARTESIAN_POINT('Ctrl Pts',(7.8304593726415,-17.7774639835853,-336.420678071071)) ;
#32725 = CARTESIAN_POINT('Ctrl Pts',(7.180939864233,-18.0574343139087,-336.429185815075)) ;
#32726 = CARTESIAN_POINT('Ctrl Pts',(6.66365011223411,-18.2546596843894,-336.435691474728)) ;
#32727 = CARTESIAN_POINT('Ctrl Pts',(5.63817601070086,-18.5962323345682,-336.448326642071)) ;
#32728 = CARTESIAN_POINT('Ctrl Pts',(5.13112309516517,-18.7424774018071,-336.454455553875)) ;
#32729 = CARTESIAN_POINT('Ctrl Pts',(4.45499673814361,-18.9079890758856,-336.462736015455)) ;
#32730 = CARTESIAN_POINT('Ctrl Pts',(4.29072926475043,-18.9459412289238,-336.464756649918)) ;
#32731 = CARTESIAN_POINT('Ctrl Pts',(4.04858103134329,-18.9985760444933,-336.467760200872)) ;
#32732 = CARTESIAN_POINT('Ctrl Pts',(3.97107103327412,-19.0149282121542,-336.468725359217)) ;
#32733 = CARTESIAN_POINT('Ctrl Pts',(3.82833856802639,-19.0441294774557,-336.470511192693)) ;
#32734 = CARTESIAN_POINT('Ctrl Pts',(3.76314614256492,-19.057118743938,-336.471330271087)) ;
#32735 = CARTESIAN_POINT('Ctrl Pts',(3.61698586669218,-19.0854612092665,-336.473173676975)) ;
#32736 = CARTESIAN_POINT('Ctrl Pts',(3.53598441859183,-19.1006342957284,-336.474200022203)) ;
#32737 = CARTESIAN_POINT('Ctrl Pts',(3.22171914446849,-19.1574344562094,-336.47819705375)) ;
#32738 = CARTESIAN_POINT('Ctrl Pts',(2.98779808049232,-19.1953075375904,-336.481204102568)) ;
#32739 = CARTESIAN_POINT('Ctrl Pts',(2.09464684482769,-19.3231912820163,-336.492737977661)) ;
#32740 = CARTESIAN_POINT('Ctrl Pts',(1.4316402263817,-19.3835929583719,-336.50139268135)) ;
#32741 = CARTESIAN_POINT('Ctrl Pts',(0.511344704047695,-19.4199519322021,
-336.513172303539)) ;
#32742 = CARTESIAN_POINT('Ctrl Pts',(0.255680463055959,-19.4249999999729,
-336.516422120054)) ;
#32743 = CARTESIAN_POINT('Ctrl Pts',(2.0594771027449E-9,-19.425,-336.519643262718)) ;
#32744 = CARTESIAN_POINT('Origin',(0.,0.,-10.)) ;
#32745 = CARTESIAN_POINT('',(-8.95436071499832E-8,-22.12975,-1.02655085110559)) ;
#32746 = CARTESIAN_POINT('',(1.7916049440271E-8,-22.12975,-0.560977995021738)) ;
#32747 = CARTESIAN_POINT('',(-2.71011275034311E-15,-22.12975,-10.)) ;
#32748 = CARTESIAN_POINT('',(19.8223774287336,9.83980908931111,-0.000330426971074296)) ;
#32749 = CARTESIAN_POINT('Ctrl Pts',(-8.95436062103849E-8,-22.12975,-1.02655085110559)) ;
#32750 = CARTESIAN_POINT('Ctrl Pts',(0.362609696220858,-22.1297500014672,
-1.01848600551515)) ;
#32751 = CARTESIAN_POINT('Ctrl Pts',(0.72522705394756,-22.1208376234837,-1.01042986688896)) ;
#32752 = CARTESIAN_POINT('Ctrl Pts',(1.53612769302464,-22.0809392872267,-0.992319112084816)) ;
#32753 = CARTESIAN_POINT('Ctrl Pts',(1.98395382077021,-22.0452146938743,-0.982252578822297)) ;
#32754 = CARTESIAN_POINT('Ctrl Pts',(2.77376933583332,-21.9579460610462,-0.964168476362566)) ;
#32755 = CARTESIAN_POINT('Ctrl Pts',(3.11622005686572,-21.9119683960168,-0.956204436732142)) ;
#32756 = CARTESIAN_POINT('Ctrl Pts',(3.9444882237055,-21.7809547225949,-0.936731115874486)) ;
#32757 = CARTESIAN_POINT('Ctrl Pts',(4.42881434833868,-21.6876595690219,-0.925172598567827)) ;
#32758 = CARTESIAN_POINT('Ctrl Pts',(5.77387688743604,-21.3816227828005,-0.892846020575418)) ;
#32759 = CARTESIAN_POINT('Ctrl Pts',(6.62554836549475,-21.1332339814427,-0.872142020144239)) ;
#32760 = CARTESIAN_POINT('Ctrl Pts',(7.98459866969752,-20.6466092522381,-0.83899701975258)) ;
#32761 = CARTESIAN_POINT('Ctrl Pts',(8.50189076450104,-20.4390349407229,-0.82634521033463)) ;
#32762 = CARTESIAN_POINT('Ctrl Pts',(9.71611455548687,-19.8977208160516,-0.796431441609054)) ;
#32763 = CARTESIAN_POINT('Ctrl Pts',(10.4044875617115,-19.5465807129507,-0.779305327577847)) ;
#32764 = CARTESIAN_POINT('Ctrl Pts',(11.5569027476881,-18.8805741829163,-0.749688324724039)) ;
#32765 = CARTESIAN_POINT('Ctrl Pts',(12.0299437418324,-18.5827481545256,-0.737229280268692)) ;
#32766 = CARTESIAN_POINT('Ctrl Pts',(12.7567649357998,-18.0857480739021,-0.717247463297029)) ;
#32767 = CARTESIAN_POINT('Ctrl Pts',(13.0183335205635,-17.8983888437069,-0.709861462377852)) ;
#32768 = CARTESIAN_POINT('Ctrl Pts',(13.9712906261952,-17.1838499002227,-0.682284087339741)) ;
#32769 = CARTESIAN_POINT('Ctrl Pts',(14.6355198505277,-16.6217694411575,-0.661791940043313)) ;
#32770 = CARTESIAN_POINT('Ctrl Pts',(15.7608075048988,-15.54965683489,-0.625490019299988)) ;
#32771 = CARTESIAN_POINT('Ctrl Pts',(16.2344618515354,-15.054472452485,-0.609621715797516)) ;
#32772 = CARTESIAN_POINT('Ctrl Pts',(17.0783717573338,-14.0859755606526,-0.58024669556295)) ;
#32773 = CARTESIAN_POINT('Ctrl Pts',(17.4538110284374,-13.6180019539252,-0.566701247149113)) ;
#32774 = CARTESIAN_POINT('Ctrl Pts',(18.2720246233815,-12.5086140739283,-0.535824299528097)) ;
#32775 = CARTESIAN_POINT('Ctrl Pts',(18.7008625973473,-11.8579107081509,-0.518599680720284)) ;
#32776 = CARTESIAN_POINT('Ctrl Pts',(19.3207214504822,-10.7998076192541,-0.491241644673661)) ;
#32777 = CARTESIAN_POINT('Ctrl Pts',(19.5351702612548,-10.4068842802415,-0.481209390700184)) ;
#32778 = CARTESIAN_POINT('Ctrl Pts',(19.8943100646021,-9.69857774783108,-0.463132144181344)) ;
#32779 = CARTESIAN_POINT('Ctrl Pts',(20.0437768095907,-9.38578656101391,-0.455139564468137)) ;
#32780 = CARTESIAN_POINT('Ctrl Pts',(20.3897033426949,-8.61587365703672,-0.435534276632124)) ;
#32781 = CARTESIAN_POINT('Ctrl Pts',(20.5782156949307,-8.15538584256677,-0.423871110867056)) ;
#32782 = CARTESIAN_POINT('Ctrl Pts',(21.0560121038169,-6.86590010377982,-0.391641309174787)) ;
#32783 = CARTESIAN_POINT('Ctrl Pts',(21.3117412612872,-6.02544075174472,-0.371139443495109)) ;
#32784 = CARTESIAN_POINT('Ctrl Pts',(21.6467235625728,-4.63183043577311,-0.338224605979193)) ;
#32785 = CARTESIAN_POINT('Ctrl Pts',(21.7561801925713,-4.08694554924959,-0.32560717830562)) ;
#32786 = CARTESIAN_POINT('Ctrl Pts',(21.9694215327346,-2.77050134494014,-0.295594424331887)) ;
#32787 = CARTESIAN_POINT('Ctrl Pts',(22.0532381496147,-1.99645952212054,-0.27834037997748)) ;
#32788 = CARTESIAN_POINT('Ctrl Pts',(22.126963222074,-0.660759385464442,-0.248573501066504)) ;
#32789 = CARTESIAN_POINT('Ctrl Pts',(22.1365965856442,-0.100939272688503,
-0.236093430574614)) ;
#32790 = CARTESIAN_POINT('Ctrl Pts',(22.1182742535962,0.782940635789909,-0.216027390570924)) ;
#32791 = CARTESIAN_POINT('Ctrl Pts',(22.1044223123916,1.10705099321042,-0.208578216171669)) ;
#32792 = CARTESIAN_POINT('Ctrl Pts',(21.9965322016293,2.77233645091229,-0.16993458549348)) ;
#32793 = CARTESIAN_POINT('Ctrl Pts',(21.7875385940238,4.10323198088417,-0.138092596463536)) ;
#32794 = CARTESIAN_POINT('Ctrl Pts',(21.3339118596575,5.90359022006686,-0.0953269285021801)) ;
#32795 = CARTESIAN_POINT('Ctrl Pts',(21.1915639711943,6.39576377758073,-0.0836435870746683)) ;
#32796 = CARTESIAN_POINT('Ctrl Pts',(20.7006088227332,7.89606379120685,-0.0479604109604452)) ;
#32797 = CARTESIAN_POINT('Ctrl Pts',(20.2961277010017,8.88426843257487,-0.0244196869317178)) ;
#32798 = CARTESIAN_POINT('Ctrl Pts',(19.8219829119648,9.8394526524738,-0.000629142560504862)) ;
#32799 = CARTESIAN_POINT('',(19.8220328557589,-9.83935203800096,1.66533453693773E-15)) ;
#32800 = CARTESIAN_POINT('Origin',(0.,0.,1.11022302462516E-15)) ;
#32801 = CARTESIAN_POINT('Ctrl Pts',(19.8220328557589,-9.83935203800097,-5.87962838138889E-14)) ;
#32802 = CARTESIAN_POINT('Ctrl Pts',(19.7227624021928,-10.0393390071218,-0.00509820586393841)) ;
#32803 = CARTESIAN_POINT('Ctrl Pts',(19.6204713487578,-10.2378116787129,-0.0102333105362058)) ;
#32804 = CARTESIAN_POINT('Ctrl Pts',(19.2629858100134,-10.9063885188397,-0.0277523314883718)) ;
#32805 = CARTESIAN_POINT('Ctrl Pts',(18.9937589249579,-11.3687753322354,-0.0402408666751295)) ;
#32806 = CARTESIAN_POINT('Ctrl Pts',(18.3810236588299,-12.3385009151472,-0.0670033576910186)) ;
#32807 = CARTESIAN_POINT('Ctrl Pts',(18.0326653279391,-12.8422592393881,-0.0812604592177863)) ;
#32808 = CARTESIAN_POINT('Ctrl Pts',(17.3294415863396,-13.7740513635541,-0.108181886905778)) ;
#32809 = CARTESIAN_POINT('Ctrl Pts',(16.9784569708648,-14.2044374063232,-0.12086245142339)) ;
#32810 = CARTESIAN_POINT('Ctrl Pts',(16.0958552164432,-15.2071942202832,-0.151062922909145)) ;
#32811 = CARTESIAN_POINT('Ctrl Pts',(15.5494020885818,-15.7655134967636,-0.168423762842354)) ;
#32812 = CARTESIAN_POINT('Ctrl Pts',(14.4039919245186,-16.8181873391972,-0.202885386509353)) ;
#32813 = CARTESIAN_POINT('Ctrl Pts',(13.8062473940792,-17.3122478815185,-0.219965866429256)) ;
#32814 = CARTESIAN_POINT('Ctrl Pts',(12.9446389381245,-17.9513466049824,-0.244141957214301)) ;
#32815 = CARTESIAN_POINT('Ctrl Pts',(12.7018989674816,-18.1239146914682,-0.250916992724896)) ;
#32816 = CARTESIAN_POINT('Ctrl Pts',(11.8950105963065,-18.67337101296,-0.273365355048762)) ;
#32817 = CARTESIAN_POINT('Ctrl Pts',(11.3170132879896,-19.0292213673286,-0.289270604881214)) ;
#32818 = CARTESIAN_POINT('Ctrl Pts',(10.1719036387582,-19.6635695184228,-0.319947037687785)) ;
#32819 = CARTESIAN_POINT('Ctrl Pts',(9.6074046478026,-19.9454599331646,-0.334706087224686)) ;
#32820 = CARTESIAN_POINT('Ctrl Pts',(8.52106232577095,-20.4311065996851,-0.362271338155627)) ;
#32821 = CARTESIAN_POINT('Ctrl Pts',(8.0020163974881,-20.6399215203552,-0.375101142193199)) ;
#32822 = CARTESIAN_POINT('Ctrl Pts',(6.61815770165498,-21.1365977990698,-0.408479285520121)) ;
#32823 = CARTESIAN_POINT('Ctrl Pts',(5.74251417470133,-21.3911037495927,-0.428748456364493)) ;
#32824 = CARTESIAN_POINT('Ctrl Pts',(4.38808097926699,-21.6955828842006,-0.459624145952587)) ;
#32825 = CARTESIAN_POINT('Ctrl Pts',(3.91922099362602,-21.7851618163998,-0.47023673397663)) ;
#32826 = CARTESIAN_POINT('Ctrl Pts',(3.11104135450716,-21.9126335258969,-0.488623482855503)) ;
#32827 = CARTESIAN_POINT('Ctrl Pts',(2.77306623558891,-21.9579641625977,-0.496344205641062)) ;
#32828 = CARTESIAN_POINT('Ctrl Pts',(1.74610825411354,-22.0716148026216,-0.520044881800077)) ;
#32829 = CARTESIAN_POINT('Ctrl Pts',(1.05484652816179,-22.1154327344403,-0.536261600369375)) ;
#32830 = CARTESIAN_POINT('Ctrl Pts',(0.241784244200346,-22.1287594266641,
-0.555313852831496)) ;
#32831 = CARTESIAN_POINT('Ctrl Pts',(0.120888776504814,-22.1297499999021,
-0.558146584989623)) ;
#32832 = CARTESIAN_POINT('Ctrl Pts',(1.79160461119543E-8,-22.12975,-0.560977995021737)) ;
#32833 = CARTESIAN_POINT('Origin',(0.,0.,-10.)) ;
#32834 = CARTESIAN_POINT('',(-1.88975816071502E-8,-22.12975,-4.20243196305312)) ;
#32835 = CARTESIAN_POINT('',(-0.000296723799801057,-22.1297499979164,-3.73504651729724)) ;
#32836 = CARTESIAN_POINT('',(-2.71011275034311E-15,-22.12975,-10.)) ;
#32837 = CARTESIAN_POINT('Ctrl Pts',(-1.88975821102666E-8,-22.12975,-4.20243196305312)) ;
#32838 = CARTESIAN_POINT('Ctrl Pts',(0.78300485118741,-22.1297500006686,-4.18423521862199)) ;
#32839 = CARTESIAN_POINT('Ctrl Pts',(1.56551886118347,-22.0881930893127,-4.16579715593098)) ;
#32840 = CARTESIAN_POINT('Ctrl Pts',(3.02567666389269,-21.9326410176014,-4.13149793264282)) ;
#32841 = CARTESIAN_POINT('Ctrl Pts',(3.70337738557218,-21.8284325774216,-4.11561883254211)) ;
#32842 = CARTESIAN_POINT('Ctrl Pts',(4.9623028889739,-21.57452559444,-4.08624955504827)) ;
#32843 = CARTESIAN_POINT('Ctrl Pts',(5.54440609758268,-21.4323160869635,-4.07271992113879)) ;
#32844 = CARTESIAN_POINT('Ctrl Pts',(6.86618024283472,-21.0519419155049,-4.04190991419865)) ;
#32845 = CARTESIAN_POINT('Ctrl Pts',(7.60051623168367,-20.7980970534689,-4.02473541276586)) ;
#32846 = CARTESIAN_POINT('Ctrl Pts',(8.73589994440261,-20.337437042036,-3.99740218876045)) ;
#32847 = CARTESIAN_POINT('Ctrl Pts',(9.14657913863443,-20.1560754837298,-3.98734203485526)) ;
#32848 = CARTESIAN_POINT('Ctrl Pts',(9.86376618477889,-19.8129205153953,-3.96924708911815)) ;
#32849 = CARTESIAN_POINT('Ctrl Pts',(10.1725230076371,-19.6561815526484,-3.96126537294436)) ;
#32850 = CARTESIAN_POINT('Ctrl Pts',(10.9138762948244,-19.2576897257486,-3.94171893335661)) ;
#32851 = CARTESIAN_POINT('Ctrl Pts',(11.3422787689048,-19.0085249251094,-3.93010441909909)) ;
#32852 = CARTESIAN_POINT('Ctrl Pts',(12.5084906178322,-18.2767676092257,-3.89784067067216)) ;
#32853 = CARTESIAN_POINT('Ctrl Pts',(13.2263820873722,-17.7641608524847,-3.87725589537778)) ;
#32854 = CARTESIAN_POINT('Ctrl Pts',(14.3449480049318,-16.8599681317877,-3.84423021760251)) ;
#32855 = CARTESIAN_POINT('Ctrl Pts',(14.7647325830739,-16.493596841325,-3.83158274933754)) ;
#32856 = CARTESIAN_POINT('Ctrl Pts',(15.733125214267,-15.5817944163126,-3.80165297156323)) ;
#32857 = CARTESIAN_POINT('Ctrl Pts',(16.2678412400112,-15.0226792186925,-3.78450734009598)) ;
#32858 = CARTESIAN_POINT('Ctrl Pts',(17.1366560616442,-14.0133137923059,-3.75487365330684)) ;
#32859 = CARTESIAN_POINT('Ctrl Pts',(17.4849461579156,-13.5762511426536,-3.7424175187845)) ;
#32860 = CARTESIAN_POINT('Ctrl Pts',(18.0068635981934,-12.8678626249446,-3.72244984900015)) ;
#32861 = CARTESIAN_POINT('Ctrl Pts',(18.1917492710008,-12.6051290949033,-3.71507520463808)) ;
#32862 = CARTESIAN_POINT('Ctrl Pts',(18.8494782161314,-11.6258307576775,-3.68776265657516)) ;
#32863 = CARTESIAN_POINT('Ctrl Pts',(19.2862352510792,-10.885949687718,-3.66753074198687)) ;
#32864 = CARTESIAN_POINT('Ctrl Pts',(19.9955580434754,-9.50698232095388,-3.63130141047985)) ;
#32865 = CARTESIAN_POINT('Ctrl Pts',(20.2831517821455,-8.87686994284161,-3.61525579695924)) ;
#32866 = CARTESIAN_POINT('Ctrl Pts',(20.7625767009978,-7.68093014452203,-3.58578552089687)) ;
#32867 = CARTESIAN_POINT('Ctrl Pts',(20.961962437541,-7.11880728035882,-3.57231532063576)) ;
#32868 = CARTESIAN_POINT('Ctrl Pts',(21.3650867628127,-5.81769368693727,-3.54179649387805)) ;
#32869 = CARTESIAN_POINT('Ctrl Pts',(21.5536293318583,-5.07479594928609,-3.52484904812858)) ;
#32870 = CARTESIAN_POINT('Ctrl Pts',(21.7954011197627,-3.86117466366818,-3.49725501933999)) ;
#32871 = CARTESIAN_POINT('Ctrl Pts',(21.8727230561259,-3.39590352541369,-3.4866923328178)) ;
#32872 = CARTESIAN_POINT('Ctrl Pts',(21.9814386856978,-2.58160504952151,-3.46798920868275)) ;
#32873 = CARTESIAN_POINT('Ctrl Pts',(22.019517880678,-2.23364242468428,-3.45991686684113)) ;
#32874 = CARTESIAN_POINT('Ctrl Pts',(22.0925718415895,-1.37907841379411,-3.43999185570009)) ;
#32875 = CARTESIAN_POINT('Ctrl Pts',(22.1183948259315,-0.87189240776236,-3.42808647880888)) ;
#32876 = CARTESIAN_POINT('Ctrl Pts',(22.1408557271778,0.492446247477333,-3.39611120558737)) ;
#32877 = CARTESIAN_POINT('Ctrl Pts',(22.1051917487505,1.34926413969942,-3.37610701003947)) ;
#32878 = CARTESIAN_POINT('Ctrl Pts',(21.964606013123,2.75520954571649,-3.34365897132579)) ;
#32879 = CARTESIAN_POINT('Ctrl Pts',(21.8884352135779,3.30628298570175,-3.33102890509898)) ;
#32880 = CARTESIAN_POINT('Ctrl Pts',(21.6560422697815,4.62033004379686,-3.30099688488503)) ;
#32881 = CARTESIAN_POINT('Ctrl Pts',(21.4801585306618,5.37907142113982,-3.28373621250674)) ;
#32882 = CARTESIAN_POINT('Ctrl Pts',(21.1099059788529,6.66409497016883,-3.25397972806693)) ;
#32883 = CARTESIAN_POINT('Ctrl Pts',(20.9348493009641,7.19516294096022,-3.24151647728626)) ;
#32884 = CARTESIAN_POINT('Ctrl Pts',(20.6277345573049,8.02033433692923,-3.22153479730581)) ;
#32885 = CARTESIAN_POINT('Ctrl Pts',(20.5090426254401,8.31915634344553,-3.21415356247645)) ;
#32886 = CARTESIAN_POINT('Ctrl Pts',(20.0454777454888,9.41595734257507,-3.18658348578997)) ;
#32887 = CARTESIAN_POINT('Ctrl Pts',(19.6601908849865,10.1959956136134,-3.16609350199875)) ;
#32888 = CARTESIAN_POINT('Ctrl Pts',(18.8908864215178,11.5468563991095,-3.12978223140487)) ;
#32889 = CARTESIAN_POINT('Ctrl Pts',(18.524266906083,12.1262949679955,-3.1139027623445)) ;
#32890 = CARTESIAN_POINT('Ctrl Pts',(17.7879394254013,13.1785359453817,-3.08453323347962)) ;
#32891 = CARTESIAN_POINT('Ctrl Pts',(17.4247452710093,13.6551403561135,-3.07100370448131)) ;
#32892 = CARTESIAN_POINT('Ctrl Pts',(16.5473917018921,14.7143632602694,-3.0401942464351)) ;
#32893 = CARTESIAN_POINT('Ctrl Pts',(16.0209968529366,15.2858207703453,-3.02302017978602)) ;
#32894 = CARTESIAN_POINT('Ctrl Pts',(15.1446172460368,16.1421148353708,-2.99568718783662)) ;
#32895 = CARTESIAN_POINT('Ctrl Pts',(14.8141058538501,16.4459589627924,-2.98562680814571)) ;
#32896 = CARTESIAN_POINT('Ctrl Pts',(14.2127121157218,16.965980751191,-2.96753211413899)) ;
#32897 = CARTESIAN_POINT('Ctrl Pts',(13.9455635588588,17.1862427666548,-2.95955088865832)) ;
#32898 = CARTESIAN_POINT('Ctrl Pts',(13.2838481960133,17.7062311402656,-2.94000648848942)) ;
#32899 = CARTESIAN_POINT('Ctrl Pts',(12.8841681615987,17.9991514527427,-2.92839353878091)) ;
#32900 = CARTESIAN_POINT('Ctrl Pts',(11.7469408061356,18.7753079532402,-2.89612819949671)) ;
#32901 = CARTESIAN_POINT('Ctrl Pts',(10.9898416888136,19.2282658823658,-2.87554025816708)) ;
#32902 = CARTESIAN_POINT('Ctrl Pts',(9.7135581298685,19.8917784829508,-2.84251145681018)) ;
#32903 = CARTESIAN_POINT('Ctrl Pts',(9.20984560148602,20.129948164333,-2.82986391701871)) ;
#32904 = CARTESIAN_POINT('Ctrl Pts',(7.98680608592124,20.652710061993,-2.79993469071419)) ;
#32905 = CARTESIAN_POINT('Ctrl Pts',(7.26049624586082,20.9190989743876,-2.78278965894124)) ;
#32906 = CARTESIAN_POINT('Ctrl Pts',(5.98788325920292,21.3115742357783,-2.75315661800815)) ;
#32907 = CARTESIAN_POINT('Ctrl Pts',(5.44798861120393,21.4559398592125,-2.74070052636858)) ;
#32908 = CARTESIAN_POINT('Ctrl Pts',(4.589968180642,21.6508941231005,-2.72073293767643)) ;
#32909 = CARTESIAN_POINT('Ctrl Pts',(4.27521349671628,21.7152381899526,-2.71335832994253)) ;
#32910 = CARTESIAN_POINT('Ctrl Pts',(3.11457478013725,21.9262899467058,-2.68604586299899)) ;
#32911 = CARTESIAN_POINT('Ctrl Pts',(2.26175726656313,22.0305974020626,-2.66581398965343)) ;
#32912 = CARTESIAN_POINT('Ctrl Pts',(0.714175751691377,22.1290536445136,-2.62958455912763)) ;
#32913 = CARTESIAN_POINT('Ctrl Pts',(0.0216245513053864,22.1405647277536,
-2.61353880990829)) ;
#32914 = CARTESIAN_POINT('Ctrl Pts',(-1.26624617556435,22.1015361333412,-2.58406840570951)) ;
#32915 = CARTESIAN_POINT('Ctrl Pts',(-1.86119259462364,22.0594027148098,-2.57059820929732)) ;
#32916 = CARTESIAN_POINT('Ctrl Pts',(-3.21492331677136,21.9083718212019,-2.54007944873172)) ;
#32917 = CARTESIAN_POINT('Ctrl Pts',(-3.97120944804521,21.7839845389495,-2.52313206377637)) ;
#32918 = CARTESIAN_POINT('Ctrl Pts',(-5.18021211847231,21.5200740511633,-2.49553798236486)) ;
#32919 = CARTESIAN_POINT('Ctrl Pts',(-5.63756937642704,21.4048123368308,-2.48497517833923)) ;
#32920 = CARTESIAN_POINT('Ctrl Pts',(-6.42737165390238,21.1786974905219,-2.46627185364127)) ;
#32921 = CARTESIAN_POINT('Ctrl Pts',(-6.76151536127838,21.0743977054054,-2.45819943051582)) ;
#32922 = CARTESIAN_POINT('Ctrl Pts',(-7.57395918489904,20.7994889440321,-2.43827410429456)) ;
#32923 = CARTESIAN_POINT('Ctrl Pts',(-8.04913386346131,20.6202580079614,-2.42636849172306)) ;
#32924 = CARTESIAN_POINT('Ctrl Pts',(-9.30852046957356,20.0950591552303,-2.3943935393047)) ;
#32925 = CARTESIAN_POINT('Ctrl Pts',(-10.0795049122872,19.719623648425,-2.37438990042575)) ;
#32926 = CARTESIAN_POINT('Ctrl Pts',(-11.3117935185232,19.0283584423186,-2.34194238675986)) ;
#32927 = CARTESIAN_POINT('Ctrl Pts',(-11.7863812637265,18.7380981065092,-2.3293123087284)) ;
#32928 = CARTESIAN_POINT('Ctrl Pts',(-12.8977356618232,17.9994451284545,-2.29928037167604)) ;
#32929 = CARTESIAN_POINT('Ctrl Pts',(-13.5227583816477,17.5347260953241,-2.28201979107091)) ;
#32930 = CARTESIAN_POINT('Ctrl Pts',(-14.5523612059734,16.6813390151862,-2.25226348711761)) ;
#32931 = CARTESIAN_POINT('Ctrl Pts',(-14.9690529600201,16.3084559135027,-2.23980032374567)) ;
#32932 = CARTESIAN_POINT('Ctrl Pts',(-15.6024542784167,15.6968980650459,-2.21981900498933)) ;
#32933 = CARTESIAN_POINT('Ctrl Pts',(-15.8288355106009,15.4685859272784,-2.21243804525713)) ;
#32934 = CARTESIAN_POINT('Ctrl Pts',(-16.6485931966349,14.6049905149185,-2.18486861910694)) ;
#32935 = CARTESIAN_POINT('Ctrl Pts',(-17.2093610350114,13.9398456805276,-2.16437899105456)) ;
#32936 = CARTESIAN_POINT('Ctrl Pts',(-18.1396885637255,12.6943776160362,-2.12806730355967)) ;
#32937 = CARTESIAN_POINT('Ctrl Pts',(-18.5241009163116,12.1265502537836,-2.11218709079074)) ;
#32938 = CARTESIAN_POINT('Ctrl Pts',(-19.1939231797678,11.0307696365686,-2.08281744373015)) ;
#32939 = CARTESIAN_POINT('Ctrl Pts',(-19.4854276896824,10.5072679986121,-2.06928850416174)) ;
#32940 = CARTESIAN_POINT('Ctrl Pts',(-20.1051828605012,9.27955487831268,-2.03848164596858)) ;
#32941 = CARTESIAN_POINT('Ctrl Pts',(-20.4183165844046,8.56859749036841,-2.02130954992691)) ;
#32942 = CARTESIAN_POINT('Ctrl Pts',(-20.8525291489185,7.42289524805143,-1.99397761802501)) ;
#32943 = CARTESIAN_POINT('Ctrl Pts',(-20.9988066582684,6.99838983381805,-1.98391622678796)) ;
#32944 = CARTESIAN_POINT('Ctrl Pts',(-21.2348329910298,6.23919225199287,-1.96582176560169)) ;
#32945 = CARTESIAN_POINT('Ctrl Pts',(-21.3298238849591,5.90628986974985,-1.95784182554096)) ;
#32946 = CARTESIAN_POINT('Ctrl Pts',(-21.5416370124958,5.09204642411329,-1.93830305965728)) ;
#32947 = CARTESIAN_POINT('Ctrl Pts',(-21.6501856686398,4.60874393128813,-1.92669450677504)) ;
#32948 = CARTESIAN_POINT('Ctrl Pts',(-21.9066916395153,3.25581329932268,-1.89442487885326)) ;
#32949 = CARTESIAN_POINT('Ctrl Pts',(-22.0190220773615,2.38036714803317,-1.87382822227687)) ;
#32950 = CARTESIAN_POINT('Ctrl Pts',(-22.1165872472184,0.944815354558331,
-1.8407901513055)) ;
#32951 = CARTESIAN_POINT('Ctrl Pts',(-22.133361451287,0.387846271600151,-1.82814176368577)) ;
#32952 = CARTESIAN_POINT('Ctrl Pts',(-22.1231949989612,-0.942071459656081,
-1.79821539165576)) ;
#32953 = CARTESIAN_POINT('Ctrl Pts',(-22.0767975374566,-1.71413808165435,
-1.78107391405708)) ;
#32954 = CARTESIAN_POINT('Ctrl Pts',(-21.927440800533,-3.03731095775537,-1.75144495311507)) ;
#32955 = CARTESIAN_POINT('Ctrl Pts',(-21.8437829605374,-3.58985469157925,
-1.73898936360242)) ;
#32956 = CARTESIAN_POINT('Ctrl Pts',(-21.6792430329331,-4.45414533651674,
-1.71902358227166)) ;
#32957 = CARTESIAN_POINT('Ctrl Pts',(-21.6123170743208,-4.76830532813321,
-1.71165027570279)) ;
#32958 = CARTESIAN_POINT('Ctrl Pts',(-21.3415016515141,-5.91632722744004,
-1.68434114745722)) ;
#32959 = CARTESIAN_POINT('Ctrl Pts',(-21.0959858458467,-6.73958475879623,
-1.66411122837106)) ;
#32960 = CARTESIAN_POINT('Ctrl Pts',(-20.567158394392,-8.1973927173502,-1.62788027517404)) ;
#32961 = CARTESIAN_POINT('Ctrl Pts',(-20.3006232293971,-8.83685239021096,
-1.61183118178125)) ;
#32962 = CARTESIAN_POINT('Ctrl Pts',(-19.7496733585932,-10.0015755730293,
-1.58236064140842)) ;
#32963 = CARTESIAN_POINT('Ctrl Pts',(-19.4731341546841,-10.5298701360726,
-1.56889347892619)) ;
#32964 = CARTESIAN_POINT('Ctrl Pts',(-18.7935015006124,-11.7096586900459,
-1.53838759212057)) ;
#32965 = CARTESIAN_POINT('Ctrl Pts',(-18.3772404828784,-12.3526854016887,
-1.52144985819985)) ;
#32966 = CARTESIAN_POINT('Ctrl Pts',(-17.6517188554879,-13.3553576573114,
-1.49385264748403)) ;
#32967 = CARTESIAN_POINT('Ctrl Pts',(-17.3627695643622,-13.7289105407336,
-1.48327654797979)) ;
#32968 = CARTESIAN_POINT('Ctrl Pts',(-16.839231852533,-14.3627495768589,-1.46456053495045)) ;
#32969 = CARTESIAN_POINT('Ctrl Pts',(-16.610001756091,-14.6272397022557,-1.45648915640155)) ;
#32970 = CARTESIAN_POINT('Ctrl Pts',(-16.0331909849394,-15.2617238358109,
-1.43656888437737)) ;
#32971 = CARTESIAN_POINT('Ctrl Pts',(-15.6789654724278,-15.6254109550156,
-1.42466732831652)) ;
#32972 = CARTESIAN_POINT('Ctrl Pts',(-14.6937161027081,-16.5697097847477,
-1.39268799087216)) ;
#32973 = CARTESIAN_POINT('Ctrl Pts',(-14.0409393043516,-17.1263720344066,
-1.37267590563707)) ;
#32974 = CARTESIAN_POINT('Ctrl Pts',(-12.9140564481339,-17.9794982076989,
-1.34021798416833)) ;
#32975 = CARTESIAN_POINT('Ctrl Pts',(-12.4580920903304,-18.2983922120309,
-1.32758571610207)) ;
#32976 = CARTESIAN_POINT('Ctrl Pts',(-11.3366601677733,-19.0213386412986,
-1.29755783226305)) ;
#32977 = CARTESIAN_POINT('Ctrl Pts',(-10.6609471716456,-19.4081270662132,
-1.28030321993197)) ;
#32978 = CARTESIAN_POINT('Ctrl Pts',(-9.46720108948631,-20.0102567895931,
-1.25055321400253)) ;
#32979 = CARTESIAN_POINT('Ctrl Pts',(-8.95877701813951,-20.2429884253592,
-1.23809034144233)) ;
#32980 = CARTESIAN_POINT('Ctrl Pts',(-8.14495636055075,-20.5788446569233,
-1.21811032811782)) ;
#32981 = CARTESIAN_POINT('Ctrl Pts',(-7.84518853795099,-20.6949794436523,
-1.21073036990084)) ;
#32982 = CARTESIAN_POINT('Ctrl Pts',(-6.72591648848527,-21.1007883412187,
-1.18316442353116)) ;
#32983 = CARTESIAN_POINT('Ctrl Pts',(-5.89209133134835,-21.3486412314298,
-1.16267723841777)) ;
#32984 = CARTESIAN_POINT('Ctrl Pts',(-4.37851361886198,-21.703092443609,-1.12636644503436)) ;
#32985 = CARTESIAN_POINT('Ctrl Pts',(-3.7042683138324,-21.8282846544745,-1.11048478203516)) ;
#32986 = CARTESIAN_POINT('Ctrl Pts',(-2.43216842952851,-22.0038381908663,
-1.0811180233647)) ;
#32987 = CARTESIAN_POINT('Ctrl Pts',(-1.83595857765317,-22.0615865643175,
-1.06759326658192)) ;
#32988 = CARTESIAN_POINT('Ctrl Pts',(-0.825758939772332,-22.1181949647166,
-1.04492861924944)) ;
#32989 = CARTESIAN_POINT('Ctrl Pts',(-0.412884428402931,-22.1297499983293,
-1.0357338587638)) ;
#32990 = CARTESIAN_POINT('Ctrl Pts',(-8.95436081532752E-8,-22.12975,-1.02655085110559)) ;
#32991 = CARTESIAN_POINT('Ctrl Pts',(1.79160500324294E-8,-22.12975,-0.560977995021737)) ;
#32992 = CARTESIAN_POINT('Ctrl Pts',(-0.525934233726528,-22.1297500004258,
-0.573296224886261)) ;
#32993 = CARTESIAN_POINT('Ctrl Pts',(-1.05174160701657,-22.1110010115208,
-0.585584835713953)) ;
#32994 = CARTESIAN_POINT('Ctrl Pts',(-2.14236416750074,-22.0331123011704,
-0.610922730527558)) ;
#32995 = CARTESIAN_POINT('Ctrl Pts',(-2.7065473814672,-21.9709437695922,-0.623944376031082)) ;
#32996 = CARTESIAN_POINT('Ctrl Pts',(-4.23937387499394,-21.7420951240243,
-0.659141534859372)) ;
#32997 = CARTESIAN_POINT('Ctrl Pts',(-5.20028927254187,-21.5324869269799,
-0.680968147911927)) ;
#32998 = CARTESIAN_POINT('Ctrl Pts',(-6.57268083743359,-21.1358635940895,
-0.712756985953018)) ;
#32999 = CARTESIAN_POINT('Ctrl Pts',(-6.99742249130262,-20.9990699599077,
-0.722693869659368)) ;
#33000 = CARTESIAN_POINT('Ctrl Pts',(-7.73067864718106,-20.7381959459378,
-0.740209003861003)) ;
#33001 = CARTESIAN_POINT('Ctrl Pts',(-8.04107334303412,-20.6198279101231,
-0.747743458136614)) ;
#33002 = CARTESIAN_POINT('Ctrl Pts',(-8.81179954500836,-20.3058633897718,
-0.766857211105509)) ;
#33003 = CARTESIAN_POINT('Ctrl Pts',(-9.26838307869553,-20.1015663545691,
-0.778518701035829)) ;
#33004 = CARTESIAN_POINT('Ctrl Pts',(-10.3732984113895,-19.5615204702096,
-0.807302275381897)) ;
#33005 = CARTESIAN_POINT('Ctrl Pts',(-11.0126962137024,-19.2088243304817,
-0.824444438292544)) ;
#33006 = CARTESIAN_POINT('Ctrl Pts',(-12.1304611322545,-18.5180732519022,
-0.854979494902476)) ;
#33007 = CARTESIAN_POINT('Ctrl Pts',(-12.6150703659842,-18.1914026816838,
-0.868430106089242)) ;
#33008 = CARTESIAN_POINT('Ctrl Pts',(-13.6524660232289,-17.4306943543624,
-0.897719551719603)) ;
#33009 = CARTESIAN_POINT('Ctrl Pts',(-14.1986607081937,-16.9887309063024,
-0.913470706192331)) ;
#33010 = CARTESIAN_POINT('Ctrl Pts',(-15.363018668484,-15.9511313916318,-0.948224457860342)) ;
#33011 = CARTESIAN_POINT('Ctrl Pts',(-15.9694235822837,-15.344003048714,-0.967138713186487)) ;
#33012 = CARTESIAN_POINT('Ctrl Pts',(-16.748893478574,-14.4672089660127,-0.993584009925753)) ;
#33013 = CARTESIAN_POINT('Ctrl Pts',(-16.9536383825249,-14.2267253122953,
-1.00076556794163)) ;
#33014 = CARTESIAN_POINT('Ctrl Pts',(-17.5040650937794,-13.5514568881276,
-1.0208041086825)) ;
#33015 = CARTESIAN_POINT('Ctrl Pts',(-17.8386303606473,-13.10791899846,-1.03378431894615)) ;
#33016 = CARTESIAN_POINT('Ctrl Pts',(-18.5847678980595,-12.0372028709565,
-1.06435353693008)) ;
#33017 = CARTESIAN_POINT('Ctrl Pts',(-18.9818526392715,-11.4007513249138,
-1.08193672320922)) ;
#33018 = CARTESIAN_POINT('Ctrl Pts',(-19.6190852117209,-10.253484035639,-1.11234484795959)) ;
#33019 = CARTESIAN_POINT('Ctrl Pts',(-19.8734409520661,-9.75134816160269,
-1.12525635915599)) ;
#33020 = CARTESIAN_POINT('Ctrl Pts',(-20.5014056720916,-8.38476047681561,
-1.15940775539414)) ;
#33021 = CARTESIAN_POINT('Ctrl Pts',(-20.8394579939037,-7.50525444662354,
-1.18033985803072)) ;
#33022 = CARTESIAN_POINT('Ctrl Pts',(-21.2598581503898,-6.16134783804295,
-1.21166270583013)) ;
#33023 = CARTESIAN_POINT('Ctrl Pts',(-21.3851008125506,-5.71150035202914,
-1.22205022015792)) ;
#33024 = CARTESIAN_POINT('Ctrl Pts',(-21.5763229745779,-4.92974082849986,
-1.24014546081878)) ;
#33025 = CARTESIAN_POINT('Ctrl Pts',(-21.6490931518115,-4.59965472559595,
-1.24780277003546)) ;
#33026 = CARTESIAN_POINT('Ctrl Pts',(-21.7997270967248,-3.83328101800073,
-1.26572608417951)) ;
#33027 = CARTESIAN_POINT('Ctrl Pts',(-21.8721029768026,-3.39606429648156,
-1.27603579643099)) ;
#33028 = CARTESIAN_POINT('Ctrl Pts',(-22.0342274791183,-2.19361766733191,
-1.30439659115754)) ;
#33029 = CARTESIAN_POINT('Ctrl Pts',(-22.0972252640812,-1.42540587648294,
-1.32250772317673)) ;
#33030 = CARTESIAN_POINT('Ctrl Pts',(-22.1377192723276,-0.0588754101339896,
-1.35430243779505)) ;
#33031 = CARTESIAN_POINT('Ctrl Pts',(-22.1312545947905,0.538199772947654,
-1.36805692004755)) ;
#33032 = CARTESIAN_POINT('Ctrl Pts',(-22.065528057541,1.81882994007757,-1.39727310533383)) ;
#33033 = CARTESIAN_POINT('Ctrl Pts',(-21.9986091500527,2.50137470790254,-1.41266615438963)) ;
#33034 = CARTESIAN_POINT('Ctrl Pts',(-21.7762742344478,4.03269502775326,-1.44717668925988)) ;
#33035 = CARTESIAN_POINT('Ctrl Pts',(-21.6027014919803,4.87770663822004,-1.46619325571305)) ;
#33036 = CARTESIAN_POINT('Ctrl Pts',(-21.2968947637669,6.02267015428563,-1.49287984762274)) ;
#33037 = CARTESIAN_POINT('Ctrl Pts',(-21.206670970756,6.33303944595073,-1.50021806156309)) ;
#33038 = CARTESIAN_POINT('Ctrl Pts',(-20.9218571548879,7.23832996013415,-1.5220267101671)) ;
#33039 = CARTESIAN_POINT('Ctrl Pts',(-20.7087926045076,7.82709588407729,-1.53667526987314)) ;
#33040 = CARTESIAN_POINT('Ctrl Pts',(-20.2192948393412,9.01916079884334,-1.56687112516782)) ;
#33041 = CARTESIAN_POINT('Ctrl Pts',(-19.9401075452378,9.62066852641224,-1.58240309376065)) ;
#33042 = CARTESIAN_POINT('Ctrl Pts',(-19.3722193991147,10.7128810502313,-1.61095405981049)) ;
#33043 = CARTESIAN_POINT('Ctrl Pts',(-19.0907730496586,11.2067433381483,-1.62400700481309)) ;
#33044 = CARTESIAN_POINT('Ctrl Pts',(-18.2527961500009,12.5538053119113,-1.66006314438083)) ;
#33045 = CARTESIAN_POINT('Ctrl Pts',(-17.6559336417536,13.3802321976155,-1.68267092765148)) ;
#33046 = CARTESIAN_POINT('Ctrl Pts',(-16.722694425566,14.5007218651046,-1.71510917494069)) ;
#33047 = CARTESIAN_POINT('Ctrl Pts',(-16.4310763896471,14.8303462408771,-1.72490818097374)) ;
#33048 = CARTESIAN_POINT('Ctrl Pts',(-15.9041529901443,15.3913093400057,-1.74222597187494)) ;
#33049 = CARTESIAN_POINT('Ctrl Pts',(-15.6731395383495,15.6264897734192,-1.74970248122091)) ;
#33050 = CARTESIAN_POINT('Ctrl Pts',(-14.9006423455448,16.3785514108231,-1.77446062695326)) ;
#33051 = CARTESIAN_POINT('Ctrl Pts',(-14.3381829911038,16.8731321797791,-1.79203078367609)) ;
#33052 = CARTESIAN_POINT('Ctrl Pts',(-13.0839306877115,17.8679359134632,-1.82954223027897)) ;
#33053 = CARTESIAN_POINT('Ctrl Pts',(-12.3860618412477,18.3585911314175,-1.84943309023077)) ;
#33054 = CARTESIAN_POINT('Ctrl Pts',(-11.1867634180766,19.1022080556933,-1.88182551786269)) ;
#33055 = CARTESIAN_POINT('Ctrl Pts',(-10.7009131383429,19.3785575509763,-1.89450877185929)) ;
#33056 = CARTESIAN_POINT('Ctrl Pts',(-9.52789998562627,19.9881830934131,-1.9242466888764)) ;
#33057 = CARTESIAN_POINT('Ctrl Pts',(-8.83292272725293,20.3048718476124,-1.9411733310623)) ;
#33058 = CARTESIAN_POINT('Ctrl Pts',(-7.6039256579658,20.7898415854069,-1.97057144166248)) ;
#33059 = CARTESIAN_POINT('Ctrl Pts',(-7.07731797239299,20.974955583818,-1.98301221226514)) ;
#33060 = CARTESIAN_POINT('Ctrl Pts',(-6.23805127550414,21.2347666678504,-2.00294752040356)) ;
#33061 = CARTESIAN_POINT('Ctrl Pts',(-5.92980142995826,21.3228996638014,-2.01030577323518)) ;
#33062 = CARTESIAN_POINT('Ctrl Pts',(-4.79050821283295,21.6220236337416,-2.03757436514442)) ;
#33063 = CARTESIAN_POINT('Ctrl Pts',(-3.94931768438597,21.7913690612007,-2.0577798501529)) ;
#33064 = CARTESIAN_POINT('Ctrl Pts',(-2.4129879761375,22.008756446236,-2.09403330529205)) ;
#33065 = CARTESIAN_POINT('Ctrl Pts',(-1.72134697110337,22.0736233514168,-2.11012757794793)) ;
#33066 = CARTESIAN_POINT('Ctrl Pts',(-0.433185813950684,22.1335156406398,
-2.13962455197018)) ;
#33067 = CARTESIAN_POINT('Ctrl Pts',(0.162303146382963,22.1371594702166,-2.15307465430135)) ;
#33068 = CARTESIAN_POINT('Ctrl Pts',(1.51936022008785,22.0906976721499,-2.18349949427501)) ;
#33069 = CARTESIAN_POINT('Ctrl Pts',(2.27964448276855,22.0252264327582,-2.20037451130819)) ;
#33070 = CARTESIAN_POINT('Ctrl Pts',(3.50678570364562,21.8553222435539,-2.22799575024501)) ;
#33071 = CARTESIAN_POINT('Ctrl Pts',(3.97630900291109,21.7747931750443,-2.23866200647971)) ;
#33072 = CARTESIAN_POINT('Ctrl Pts',(4.78485058601815,21.6090931435798,-2.25745076839496)) ;
#33073 = CARTESIAN_POINT('Ctrl Pts',(5.12512670229219,21.5309259615509,-2.2655014930802)) ;
#33074 = CARTESIAN_POINT('Ctrl Pts',(5.9525599736799,21.3201234746012,-2.28533625510541)) ;
#33075 = CARTESIAN_POINT('Ctrl Pts',(6.43730444714733,21.1788041412342,-2.29717231584179)) ;
#33076 = CARTESIAN_POINT('Ctrl Pts',(7.73623135930551,20.751403406109,-2.32921619425072)) ;
#33077 = CARTESIAN_POINT('Ctrl Pts',(8.53921126501607,20.434086979508,-2.34935847370628)) ;
#33078 = CARTESIAN_POINT('Ctrl Pts',(9.82623942292865,19.8363410055606,-2.38194566386641)) ;
#33079 = CARTESIAN_POINT('Ctrl Pts',(10.3218449881087,19.5830265296391,-2.39458150646353)) ;
#33080 = CARTESIAN_POINT('Ctrl Pts',(11.4853755036592,18.9318682280159,-2.42458785176237)) ;
#33081 = CARTESIAN_POINT('Ctrl Pts',(12.1429194254384,18.5169920943436,-2.44181832507531)) ;
#33082 = CARTESIAN_POINT('Ctrl Pts',(13.233632050842,17.7456816838172,-2.47154335487439)) ;
#33083 = CARTESIAN_POINT('Ctrl Pts',(13.6775906966312,17.4057961959282,-2.48400551785132)) ;
#33084 = CARTESIAN_POINT('Ctrl Pts',(14.3558842376998,16.844517664891,-2.50398567886508)) ;
#33085 = CARTESIAN_POINT('Ctrl Pts',(14.5990675051604,16.6341940420368,-2.51136656529882)) ;
#33086 = CARTESIAN_POINT('Ctrl Pts',(15.4824518518825,15.8358770269977,-2.53893470792046)) ;
#33087 = CARTESIAN_POINT('Ctrl Pts',(16.0924283562774,15.2156191992287,-2.55942312987066)) ;
#33088 = CARTESIAN_POINT('Ctrl Pts',(17.1153048252688,14.0449957290865,-2.59573437156419)) ;
#33089 = CARTESIAN_POINT('Ctrl Pts',(17.5420514525484,13.5082199677597,-2.61161529381933)) ;
#33090 = CARTESIAN_POINT('Ctrl Pts',(18.2937098202633,12.4669420185057,-2.64098365630942)) ;
#33091 = CARTESIAN_POINT('Ctrl Pts',(18.6243656518279,11.9673503159477,-2.65451067440508)) ;
#33092 = CARTESIAN_POINT('Ctrl Pts',(19.3360586677326,10.7909651494682,-2.68530952231401)) ;
#33093 = CARTESIAN_POINT('Ctrl Pts',(19.7025582832172,10.1062994845046,-2.70247564262063)) ;
#33094 = CARTESIAN_POINT('Ctrl Pts',(20.2231451795239,8.99732542747596,-2.72980405391132)) ;
#33095 = CARTESIAN_POINT('Ctrl Pts',(20.4015402034208,8.58513941034812,-2.73986820441059)) ;
#33096 = CARTESIAN_POINT('Ctrl Pts',(20.6949003878055,7.84643286970198,-2.75795728854641)) ;
#33097 = CARTESIAN_POINT('Ctrl Pts',(20.8149780378034,7.52210708541269,-2.76592888200795)) ;
#33098 = CARTESIAN_POINT('Ctrl Pts',(21.0880550767143,6.72784565895061,-2.78543345294672)) ;
#33099 = CARTESIAN_POINT('Ctrl Pts',(21.233010006295,6.25533838774175,-2.79701589963105)) ;
#33100 = CARTESIAN_POINT('Ctrl Pts',(21.5928764928195,4.92495147678466,-2.82931303748762)) ;
#33101 = CARTESIAN_POINT('Ctrl Pts',(21.7723781672084,4.05845211560372,-2.84996349285406)) ;
#33102 = CARTESIAN_POINT('Ctrl Pts',(21.9797079555187,2.63223045739763,-2.88305511207917)) ;
#33103 = CARTESIAN_POINT('Ctrl Pts',(22.0390051115066,2.07809023695964,-2.89570517479943)) ;
#33104 = CARTESIAN_POINT('Ctrl Pts',(22.1304645660627,0.751690054509215,-2.92562200915772)) ;
#33105 = CARTESIAN_POINT('Ctrl Pts',(22.1432169020043,-0.0211741976199246,
-2.94275270633856)) ;
#33106 = CARTESIAN_POINT('Ctrl Pts',(22.0955115780757,-1.35139852307501,-2.97237069737913)) ;
#33107 = CARTESIAN_POINT('Ctrl Pts',(22.0543580756396,-1.90871489643176,-2.98482615231563)) ;
#33108 = CARTESIAN_POINT('Ctrl Pts',(21.9563973499803,-2.78309808608486,-3.00479286697957)) ;
#33109 = CARTESIAN_POINT('Ctrl Pts',(21.9136873453836,-3.1015032382929,-3.01216727806539)) ;
#33110 = CARTESIAN_POINT('Ctrl Pts',(21.7314428907408,-4.26697937008732,-3.03947891539823)) ;
#33111 = CARTESIAN_POINT('Ctrl Pts',(21.549588235056,-5.10665946494792,-3.05971017258317)) ;
#33112 = CARTESIAN_POINT('Ctrl Pts',(21.1337930212615,-6.60059902190559,-3.09593993820866)) ;
#33113 = CARTESIAN_POINT('Ctrl Pts',(20.9169708439003,-7.25847487490876,-3.11198659951746)) ;
#33114 = CARTESIAN_POINT('Ctrl Pts',(20.4567085292055,-8.46193351282878,-3.14145720880366)) ;
#33115 = CARTESIAN_POINT('Ctrl Pts',(20.2213356776939,-9.00992970070769,-3.154926741026)) ;
#33116 = CARTESIAN_POINT('Ctrl Pts',(19.6337100633174,-10.2386404994311,-3.18544255027454)) ;
#33117 = CARTESIAN_POINT('Ctrl Pts',(19.2676571059666,-10.9119072056271,-3.20238769200689)) ;
#33118 = CARTESIAN_POINT('Ctrl Pts',(18.6209405410612,-11.9669919833376,-3.22998262841657)) ;
#33119 = CARTESIAN_POINT('Ctrl Pts',(18.3616471611248,-12.3611582053818,-3.24054865479097)) ;
#33120 = CARTESIAN_POINT('Ctrl Pts',(17.8883871663665,-13.0328011158217,-3.25925418653295)) ;
#33121 = CARTESIAN_POINT('Ctrl Pts',(17.6800607603497,-13.3140432139573,-3.26732546995719)) ;
#33122 = CARTESIAN_POINT('Ctrl Pts',(17.1534578336099,-13.9907945288812,-3.28724616389628)) ;
#33123 = CARTESIAN_POINT('Ctrl Pts',(16.8280722996134,-14.3805225244584,-3.29914825048019)) ;
#33124 = CARTESIAN_POINT('Ctrl Pts',(15.9179591311133,-15.3973711363029,-3.33112665991972)) ;
#33125 = CARTESIAN_POINT('Ctrl Pts',(15.3097173060681,-16.0022822486626,-3.35113728810968)) ;
#33126 = CARTESIAN_POINT('Ctrl Pts',(14.2515089346783,-16.9389964188399,-3.38359171297152)) ;
#33127 = CARTESIAN_POINT('Ctrl Pts',(13.8213458646886,-17.2917758315769,-3.39622195410535)) ;
#33128 = CARTESIAN_POINT('Ctrl Pts',(12.7584059189391,-18.0984697061888,-3.42625283502378)) ;
#33129 = CARTESIAN_POINT('Ctrl Pts',(12.1140750641772,-18.5359304052641,-3.44351224388142)) ;
#33130 = CARTESIAN_POINT('Ctrl Pts',(10.9696712017121,-19.2277040358139,-3.47326739064209)) ;
#33131 = CARTESIAN_POINT('Ctrl Pts',(10.480520705525,-19.4986401396969,-3.48573057414477)) ;
#33132 = CARTESIAN_POINT('Ctrl Pts',(9.69470631030959,-19.8957750505562,-3.50571216183121)) ;
#33133 = CARTESIAN_POINT('Ctrl Pts',(9.40464904100198,-20.0345144078224,-3.51309337529043)) ;
#33134 = CARTESIAN_POINT('Ctrl Pts',(8.31952684369476,-20.524787457452,-3.54066337858747)) ;
#33135 = CARTESIAN_POINT('Ctrl Pts',(7.50698066475757,-20.8357066076486,-3.56115331180284)) ;
#33136 = CARTESIAN_POINT('Ctrl Pts',(6.02489615056135,-21.3048377995494,-3.59746461967355)) ;
#33137 = CARTESIAN_POINT('Ctrl Pts',(5.36227712727311,-21.4811890468595,-3.61334417286704)) ;
#33138 = CARTESIAN_POINT('Ctrl Pts',(4.1960747363392,-21.7342328013673,-3.64063391776006)) ;
#33139 = CARTESIAN_POINT('Ctrl Pts',(3.69604415758763,-21.8248294584951,-3.65213300120995)) ;
#33140 = CARTESIAN_POINT('Ctrl Pts',(2.13577037616094,-22.0523593330427,-3.68754652786183)) ;
#33141 = CARTESIAN_POINT('Ctrl Pts',(1.06842946296467,-22.129765004344,-3.71104938457161)) ;
#33142 = CARTESIAN_POINT('Ctrl Pts',(-0.000310730952457761,-22.1297499978185,
-3.73504649578496)) ;
#33143 = CARTESIAN_POINT('Origin',(0.,0.,-10.)) ;
#33144 = CARTESIAN_POINT('',(-4.10971426655051E-9,-22.12975,-7.37565036637909)) ;
#33145 = CARTESIAN_POINT('',(-0.00028260616734981,-22.1297499981955,-6.91183148751772)) ;
#33146 = CARTESIAN_POINT('',(-2.71011275034311E-15,-22.12975,-10.)) ;
#33147 = CARTESIAN_POINT('Ctrl Pts',(-4.1097096559195E-9,-22.12975,-7.37565036637909)) ;
#33148 = CARTESIAN_POINT('Ctrl Pts',(0.496307662068902,-22.1297500000922,
-7.36418082185928)) ;
#33149 = CARTESIAN_POINT('Ctrl Pts',(0.992494088983844,-22.1130538540768,
-7.35281336153108)) ;
#33150 = CARTESIAN_POINT('Ctrl Pts',(2.36728846219153,-22.0204209047268,-7.32154322916872)) ;
#33151 = CARTESIAN_POINT('Ctrl Pts',(3.24253230519655,-21.9086509499698,-7.3019184235776)) ;
#33152 = CARTESIAN_POINT('Ctrl Pts',(4.59550185240573,-21.6530034652559,-7.27130069620706)) ;
#33153 = CARTESIAN_POINT('Ctrl Pts',(5.0790022644443,-21.544719292526,-7.26029312857459)) ;
#33154 = CARTESIAN_POINT('Ctrl Pts',(5.89354108416853,-21.3333506313142,-7.241394104392)) ;
#33155 = CARTESIAN_POINT('Ctrl Pts',(6.22653636982164,-21.2385479855221,-7.23356203120506)) ;
#33156 = CARTESIAN_POINT('Ctrl Pts',(6.98587369482261,-21.0029731010004,-7.21533578284537)) ;
#33157 = CARTESIAN_POINT('Ctrl Pts',(7.41042930664819,-20.8569615256471,-7.20489586716275)) ;
#33158 = CARTESIAN_POINT('Ctrl Pts',(8.55641784940482,-20.4234262497798,-7.17626174148924)) ;
#33159 = CARTESIAN_POINT('Ctrl Pts',(9.26763108493787,-20.1106849090278,-7.15800347887808)) ;
#33160 = CARTESIAN_POINT('Ctrl Pts',(10.4957909943736,-19.491612650642,-7.12601334926235)) ;
#33161 = CARTESIAN_POINT('Ctrl Pts',(11.0194841439878,-19.2004054548611,-7.11220861145816)) ;
#33162 = CARTESIAN_POINT('Ctrl Pts',(12.1156566581831,-18.5312265814932,-7.08294433729836)) ;
#33163 = CARTESIAN_POINT('Ctrl Pts',(12.6836913137425,-18.1471617251315,-7.06755216845237)) ;
#33164 = CARTESIAN_POINT('Ctrl Pts',(13.9297080673345,-17.217568480866,-7.0328764797819)) ;
#33165 = CARTESIAN_POINT('Ctrl Pts',(14.5951913428042,-16.6571847938103,-7.01369812697652)) ;
#33166 = CARTESIAN_POINT('Ctrl Pts',(15.4592835098897,-15.8379211434953,-6.98687201777148)) ;
#33167 = CARTESIAN_POINT('Ctrl Pts',(15.6877333883636,-15.6116691522672,-6.97956769369083)) ;
#33168 = CARTESIAN_POINT('Ctrl Pts',(16.2996722163591,-14.9786172301129,-6.95932600226643)) ;
#33169 = CARTESIAN_POINT('Ctrl Pts',(16.6728003485183,-14.5621431061368,-6.94626356423777)) ;
#33170 = CARTESIAN_POINT('Ctrl Pts',(17.5267634254894,-13.5330748793806,-6.91494121500932)) ;
#33171 = CARTESIAN_POINT('Ctrl Pts',(17.9918313774377,-12.9083525963353,-6.89668664815354)) ;
#33172 = CARTESIAN_POINT('Ctrl Pts',(18.7311247176936,-11.7974603535927,-6.86579235779266)) ;
#33173 = CARTESIAN_POINT('Ctrl Pts',(19.0216689555042,-11.3230393780551,-6.85304258236847)) ;
#33174 = CARTESIAN_POINT('Ctrl Pts',(19.7137627574503,-10.0909795027729,-6.82097761216475)) ;
#33175 = CARTESIAN_POINT('Ctrl Pts',(20.0897321840658,-9.32003114857441,-6.80188898968452)) ;
#33176 = CARTESIAN_POINT('Ctrl Pts',(20.6156840630731,-8.06083537101872,-6.77154387662993)) ;
#33177 = CARTESIAN_POINT('Ctrl Pts',(20.7951499715355,-7.585857294535,-6.76026821908286)) ;
#33178 = CARTESIAN_POINT('Ctrl Pts',(21.070485255523,-6.77369620850567,-6.74101557182124)) ;
#33179 = CARTESIAN_POINT('Ctrl Pts',(21.1749689073444,-6.43964291964075,-6.73310155986182)) ;
#33180 = CARTESIAN_POINT('Ctrl Pts',(21.4015739580845,-5.64986301072583,-6.71427114495625)) ;
#33181 = CARTESIAN_POINT('Ctrl Pts',(21.5171318797554,-5.19243212120798,-6.70329477168496)) ;
#33182 = CARTESIAN_POINT('Ctrl Pts',(21.7817285490791,-3.98354462693207,-6.67436353817122)) ;
#33183 = CARTESIAN_POINT('Ctrl Pts',(21.9065295868642,-3.22742855079625,-6.65635871501739)) ;
#33184 = CARTESIAN_POINT('Ctrl Pts',(22.0583243522427,-1.87391891094637,-6.62468616832486)) ;
#33185 = CARTESIAN_POINT('Ctrl Pts',(22.1007997555033,-1.27902442930549,-6.61094933754796)) ;
#33186 = CARTESIAN_POINT('Ctrl Pts',(22.1405753799507,0.0088617248840879,
-6.58159446988023)) ;
#33187 = CARTESIAN_POINT('Ctrl Pts',(22.1294618825395,0.70148611629901,-6.56605026013672)) ;
#33188 = CARTESIAN_POINT('Ctrl Pts',(22.0318851110312,2.24916708245715,-6.53146751218405)) ;
#33189 = CARTESIAN_POINT('Ctrl Pts',(21.9280696632736,3.10200898704139,-6.51252370818853)) ;
#33190 = CARTESIAN_POINT('Ctrl Pts',(21.7176951362174,4.26271362501853,-6.48594668174259)) ;
#33191 = CARTESIAN_POINT('Ctrl Pts',(21.6535369038551,4.57748280302964,-6.47864830219849)) ;
#33192 = CARTESIAN_POINT('Ctrl Pts',(21.4590877363213,5.43557422771732,-6.45841988997357)) ;
#33193 = CARTESIAN_POINT('Ctrl Pts',(21.3150409195593,5.97552835276067,-6.44536509524797)) ;
#33194 = CARTESIAN_POINT('Ctrl Pts',(20.9234355198276,7.24794560222024,-6.41418160461128)) ;
#33195 = CARTESIAN_POINT('Ctrl Pts',(20.6576290839189,7.97403542187047,-6.39605827537518)) ;
#33196 = CARTESIAN_POINT('Ctrl Pts',(20.1357787940604,9.1970947982472,-6.36526698125948)) ;
#33197 = CARTESIAN_POINT('Ctrl Pts',(19.8978977926689,9.70102110404991,-6.35249349192216)) ;
#33198 = CARTESIAN_POINT('Ctrl Pts',(19.2343249103643,10.9793777858995,-6.31980670403162)) ;
#33199 = CARTESIAN_POINT('Ctrl Pts',(18.7808252719957,11.7382538801348,-6.30014479502846)) ;
#33200 = CARTESIAN_POINT('Ctrl Pts',(18.0045800719058,12.8765471936912,-6.26950781340728)) ;
#33201 = CARTESIAN_POINT('Ctrl Pts',(17.7123583162599,13.2756442831883,-6.25851846716267)) ;
#33202 = CARTESIAN_POINT('Ctrl Pts',(17.1934144354014,13.9367140277936,-6.2396434699741)) ;
#33203 = CARTESIAN_POINT('Ctrl Pts',(16.973464371159,14.2037672860175,-6.23181695621271)) ;
#33204 = CARTESIAN_POINT('Ctrl Pts',(16.4538468090212,14.8053490809352,-6.2135929915005)) ;
#33205 = CARTESIAN_POINT('Ctrl Pts',(16.1500766897881,15.1361307924852,-6.20314963370124)) ;
#33206 = CARTESIAN_POINT('Ctrl Pts',(15.2943390582676,16.0128511005082,-6.17451825355095)) ;
#33207 = CARTESIAN_POINT('Ctrl Pts',(14.7233751830527,16.5393602674812,-6.15626645606375)) ;
#33208 = CARTESIAN_POINT('Ctrl Pts',(13.6649254194284,17.4170697981906,-6.12428441983908)) ;
#33209 = CARTESIAN_POINT('Ctrl Pts',(13.1885863196782,17.7804866657199,-6.11048140676089)) ;
#33210 = CARTESIAN_POINT('Ctrl Pts',(12.1366814230179,18.5174699092258,-6.08121501655037)) ;
#33211 = CARTESIAN_POINT('Ctrl Pts',(11.5572971722019,18.8845073810979,-6.06581916463472)) ;
#33212 = CARTESIAN_POINT('Ctrl Pts',(10.2067746205897,19.6545929170521,-6.0311419360206)) ;
#33213 = CARTESIAN_POINT('Ctrl Pts',(9.42703538156276,20.0402659451474,-6.01196556578956)) ;
#33214 = CARTESIAN_POINT('Ctrl Pts',(8.33063323822664,20.5043826648788,-5.98514246771099)) ;
#33215 = CARTESIAN_POINT('Ctrl Pts',(8.0319316418891,20.6232207114201,-5.97783925186562)) ;
#33216 = CARTESIAN_POINT('Ctrl Pts',(7.20704314787377,20.9307608265602,-5.95760001351314)) ;
#33217 = CARTESIAN_POINT('Ctrl Pts',(6.67613558175924,21.1060993134591,-5.94453897697726)) ;
#33218 = CARTESIAN_POINT('Ctrl Pts',(5.39243676892041,21.4767677489006,-5.91324250950174)) ;
#33219 = CARTESIAN_POINT('Ctrl Pts',(4.63486479183454,21.6528974215475,-5.89501242673719)) ;
#33220 = CARTESIAN_POINT('Ctrl Pts',(3.32187853024127,21.8860781630063,-5.86413740758064)) ;
#33221 = CARTESIAN_POINT('Ctrl Pts',(2.7706830842171,21.962664141789,-5.85138326708829)) ;
#33222 = CARTESIAN_POINT('Ctrl Pts',(1.35935766125119,22.1047803025969,-5.81919659312306)) ;
#33223 = CARTESIAN_POINT('Ctrl Pts',(0.497213970667352,22.1409564892583,-5.79999541863384)) ;
#33224 = CARTESIAN_POINT('Ctrl Pts',(-0.869765365137659,22.1184167863385,
-5.76959400497232)) ;
#33225 = CARTESIAN_POINT('Ctrl Pts',(-1.37425526351653,22.0928104228207,-5.75837541604237)) ;
#33226 = CARTESIAN_POINT('Ctrl Pts',(-2.22532353515171,22.0203469842369,-5.73919805579457)) ;
#33227 = CARTESIAN_POINT('Ctrl Pts',(-2.57247240361083,21.9824960327275,-5.73130150126133)) ;
#33228 = CARTESIAN_POINT('Ctrl Pts',(-3.39048648996683,21.8736616525,-5.71238792003792)) ;
#33229 = CARTESIAN_POINT('Ctrl Pts',(-3.86024194050749,21.7956647192008,-5.70130768513868)) ;
#33230 = CARTESIAN_POINT('Ctrl Pts',(-5.07516058635754,21.553431296399,-5.67234246688728)) ;
#33231 = CARTESIAN_POINT('Ctrl Pts',(-5.81500044892733,21.3657069296551,-5.65441091981165)) ;
#33232 = CARTESIAN_POINT('Ctrl Pts',(-7.11239366019708,20.9641153432611,-5.62283031380103)) ;
#33233 = CARTESIAN_POINT('Ctrl Pts',(-7.67378713261747,20.7651938283145,-5.60911322905975)) ;
#33234 = CARTESIAN_POINT('Ctrl Pts',(-8.87121184191377,20.2857035967481,-5.57972901047383)) ;
#33235 = CARTESIAN_POINT('Ctrl Pts',(-9.50343639164586,19.9973217219708,-5.56413768632299)) ;
#33236 = CARTESIAN_POINT('Ctrl Pts',(-10.8834548708722,19.2875928238917,-5.52953331972418)) ;
#33237 = CARTESIAN_POINT('Ctrl Pts',(-11.622421315353,18.8515287006678,-5.51061311864944)) ;
#33238 = CARTESIAN_POINT('Ctrl Pts',(-12.6003643592225,18.1950379619678,-5.48407232833942)) ;
#33239 = CARTESIAN_POINT('Ctrl Pts',(-12.862592167643,18.0106166160129,-5.47678759398956)) ;
#33240 = CARTESIAN_POINT('Ctrl Pts',(-13.5699219315696,17.4898317486615,-5.45659083669298)) ;
#33241 = CARTESIAN_POINT('Ctrl Pts',(-14.0064521933666,17.1422369503527,-5.4435548060097)) ;
#33242 = CARTESIAN_POINT('Ctrl Pts',(-15.0056425929214,16.2829421350354,-5.41268607960386)) ;
#33243 = CARTESIAN_POINT('Ctrl Pts',(-15.5559945043242,15.7579998521014,-5.39485881886433)) ;
#33244 = CARTESIAN_POINT('Ctrl Pts',(-16.4625323791601,14.7994475512052,-5.36429728057912)) ;
#33245 = CARTESIAN_POINT('Ctrl Pts',(-16.8312789717815,14.3786882247092,-5.35146753515695)) ;
#33246 = CARTESIAN_POINT('Ctrl Pts',(-17.7736061901449,13.2174587601229,-5.31751744471359)) ;
#33247 = CARTESIAN_POINT('Ctrl Pts',(-18.3167964616073,12.4538055017185,-5.29670184885839)) ;
#33248 = CARTESIAN_POINT('Ctrl Pts',(-19.1658170571993,11.0839305286475,-5.2608621650526)) ;
#33249 = CARTESIAN_POINT('Ctrl Pts',(-19.4951700657963,10.4938263225175,-5.24584525929691)) ;
#33250 = CARTESIAN_POINT('Ctrl Pts',(-19.9462060966197,9.59094087082683,-5.22290208766585)) ;
#33251 = CARTESIAN_POINT('Ctrl Pts',(-20.0886174380408,9.28895736846857,-5.21521891004722)) ;
#33252 = CARTESIAN_POINT('Ctrl Pts',(-20.408764658061,8.56825437477137,-5.19692776974995)) ;
#33253 = CARTESIAN_POINT('Ctrl Pts',(-20.5805318657076,8.14704634224766,-5.18628036926511)) ;
#33254 = CARTESIAN_POINT('Ctrl Pts',(-21.0542000353278,6.87471208972843,-5.15446774294738)) ;
#33255 = CARTESIAN_POINT('Ctrl Pts',(-21.317126839163,6.01008580146231,-5.13333791591706)) ;
#33256 = CARTESIAN_POINT('Ctrl Pts',(-21.6537142677631,4.59819814478098,-5.09995067199544)) ;
#33257 = CARTESIAN_POINT('Ctrl Pts',(-21.7610413984736,4.06003093786366,-5.08746704218324)) ;
#33258 = CARTESIAN_POINT('Ctrl Pts',(-21.8955651861364,3.22468367392709,-5.06839162574475)) ;
#33259 = CARTESIAN_POINT('Ctrl Pts',(-21.9369411081335,2.93001283100947,-5.06171867725492)) ;
#33260 = CARTESIAN_POINT('Ctrl Pts',(-22.1041604726886,1.5354144236028,-5.030326132673)) ;
#33261 = CARTESIAN_POINT('Ctrl Pts',(-22.1532900175718,0.427903943387989,
-5.00602798842732)) ;
#33262 = CARTESIAN_POINT('Ctrl Pts',(-22.1093034917611,-1.00584028333761,
-4.97344579562935)) ;
#33263 = CARTESIAN_POINT('Ctrl Pts',(-22.0920041376088,-1.332803124651,-4.96591970733462)) ;
#33264 = CARTESIAN_POINT('Ctrl Pts',(-22.0350296168648,-2.09054069118996,
-4.94830950104404)) ;
#33265 = CARTESIAN_POINT('Ctrl Pts',(-21.9899651334064,-2.52077807973778,
-4.93819215488364)) ;
#33266 = CARTESIAN_POINT('Ctrl Pts',(-21.8000951345113,-3.93268105860742,
-4.90481740402699)) ;
#33267 = CARTESIAN_POINT('Ctrl Pts',(-21.6018937209033,-4.90595017565772,
-4.88158485777349)) ;
#33268 = CARTESIAN_POINT('Ctrl Pts',(-21.1915603818775,-6.39949874262833,
-4.8460189891286)) ;
#33269 = CARTESIAN_POINT('Ctrl Pts',(-21.0238549325764,-6.93060933036597,
-4.83337592406703)) ;
#33270 = CARTESIAN_POINT('Ctrl Pts',(-20.5754212068982,-8.18398417888593,
-4.80342069968414)) ;
#33271 = CARTESIAN_POINT('Ctrl Pts',(-20.276450118227,-8.89893975599737,-4.78624636284093)) ;
#33272 = CARTESIAN_POINT('Ctrl Pts',(-19.6983124091077,-10.1002237895192,
-4.75658201191927)) ;
#33273 = CARTESIAN_POINT('Ctrl Pts',(-19.4370276470082,-10.5943372339023,
-4.74412407811697)) ;
#33274 = CARTESIAN_POINT('Ctrl Pts',(-18.9964856135211,-11.356170213598,-4.72415289309478)) ;
#33275 = CARTESIAN_POINT('Ctrl Pts',(-18.829609516084,-11.6307724984423,-4.71677660961995)) ;
#33276 = CARTESIAN_POINT('Ctrl Pts',(-18.1950720849967,-12.6254627434472,
-4.68945967525079)) ;
#33277 = CARTESIAN_POINT('Ctrl Pts',(-17.6915982245896,-13.321798334969,-4.66922513240996)) ;
#33278 = CARTESIAN_POINT('Ctrl Pts',(-16.7115399382497,-14.5234014778031,
-4.63299849398948)) ;
#33279 = CARTESIAN_POINT('Ctrl Pts',(-16.2492167693292,-15.0388737558885,
-4.61695800463579)) ;
#33280 = CARTESIAN_POINT('Ctrl Pts',(-15.3450027077108,-15.95657444771,-4.58749093006662)) ;
#33281 = CARTESIAN_POINT('Ctrl Pts',(-14.9095098421141,-16.3642262161272,
-4.5740189923709)) ;
#33282 = CARTESIAN_POINT('Ctrl Pts',(-13.8779849385705,-17.2544051054192,
-4.54349167000361)) ;
#33283 = CARTESIAN_POINT('Ctrl Pts',(-13.27227759947,-17.7245481716059,-4.52653760212552)) ;
#33284 = CARTESIAN_POINT('Ctrl Pts',(-12.2567679246685,-18.4314787636057,
-4.49894613495367)) ;
#33285 = CARTESIAN_POINT('Ctrl Pts',(-11.8616335650097,-18.6882158977968,
-4.48839300048637)) ;
#33286 = CARTESIAN_POINT('Ctrl Pts',(-11.1591150946941,-19.1134125849576,
-4.46969774468818)) ;
#33287 = CARTESIAN_POINT('Ctrl Pts',(-10.8553644412281,-19.2875464494945,
-4.46162338153668)) ;
#33288 = CARTESIAN_POINT('Ctrl Pts',(-10.1010577457714,-19.696509781283,-4.44168992650591)) ;
#33289 = CARTESIAN_POINT('Ctrl Pts',(-9.64629823566461,-19.9231722799568,
-4.42977806295117)) ;
#33290 = CARTESIAN_POINT('Ctrl Pts',(-8.4050733846082,-20.4893586613698,-4.39780899839229)) ;
#33291 = CARTESIAN_POINT('Ctrl Pts',(-7.60602734897138,-20.7992174182761,
-4.37781751014594)) ;
#33292 = CARTESIAN_POINT('Ctrl Pts',(-6.26177191280288,-21.2326468107708,
-4.34538208168149)) ;
#33293 = CARTESIAN_POINT('Ctrl Pts',(-5.72626080505905,-21.3832883719748,
-4.33275235569584)) ;
#33294 = CARTESIAN_POINT('Ctrl Pts',(-4.42889046591634,-21.6960067771973,
-4.30271824734036)) ;
#33295 = CARTESIAN_POINT('Ctrl Pts',(-3.66304172562807,-21.8383586724143,
-4.2854552403341)) ;
#33296 = CARTESIAN_POINT('Ctrl Pts',(-2.33709354084746,-22.0130936651908,
-4.25569627073051)) ;
#33297 = CARTESIAN_POINT('Ctrl Pts',(-1.78033510003659,-22.0651013742485,
-4.24323288237793)) ;
#33298 = CARTESIAN_POINT('Ctrl Pts',(-0.901198406149303,-22.1137296775406,
-4.22325094299919)) ;
#33299 = CARTESIAN_POINT('Ctrl Pts',(-0.57984253157056,-22.1244881814877,
-4.21586959248389)) ;
#33300 = CARTESIAN_POINT('Ctrl Pts',(-0.172242706946389,-22.1292473028186,
-4.2064314930422)) ;
#33301 = CARTESIAN_POINT('Ctrl Pts',(-0.0861183909271938,-22.1297499999265,
-4.20443332226111)) ;
#33302 = CARTESIAN_POINT('Ctrl Pts',(-1.88975816071502E-8,-22.12975,-4.20243196305312)) ;
#33303 = CARTESIAN_POINT('Ctrl Pts',(-0.000310769958409111,-22.1297499978179,
-3.73504649666078)) ;
#33304 = CARTESIAN_POINT('Ctrl Pts',(-0.200541522835967,-22.1297471859604,
-3.73954240658829)) ;
#33305 = CARTESIAN_POINT('Ctrl Pts',(-0.400762522146849,-22.1270268313811,
-3.74405692376472)) ;
#33306 = CARTESIAN_POINT('Ctrl Pts',(-0.768716641826934,-22.1170316004905,
-3.75240859043868)) ;
#33307 = CARTESIAN_POINT('Ctrl Pts',(-0.936456061890543,-22.1105644872954,
-3.75623821292539)) ;
#33308 = CARTESIAN_POINT('Ctrl Pts',(-1.66817341771166,-22.0740118210972,
-3.77305255713291)) ;
#33309 = CARTESIAN_POINT('Ctrl Pts',(-2.23095253771463,-22.0242513029601,
-3.78624144779857)) ;
#33310 = CARTESIAN_POINT('Ctrl Pts',(-3.60621661434526,-21.8493939245641,
-3.81870716164814)) ;
#33311 = CARTESIAN_POINT('Ctrl Pts',(-4.41482808983057,-21.7004635809194,
-3.83798398665093)) ;
#33312 = CARTESIAN_POINT('Ctrl Pts',(-5.73102840938846,-21.3814161944027,
-3.86931673964317)) ;
#33313 = CARTESIAN_POINT('Ctrl Pts',(-6.24407438572413,-21.2372593807404,
-3.88152544266926)) ;
#33314 = CARTESIAN_POINT('Ctrl Pts',(-7.57468034409793,-20.8109915072469,
-3.9132304516488)) ;
#33315 = CARTESIAN_POINT('Ctrl Pts',(-8.38178044918709,-20.4992418609031,
-3.93248203484719)) ;
#33316 = CARTESIAN_POINT('Ctrl Pts',(-9.62712771118747,-19.9323378242688,
-3.96290880854848)) ;
#33317 = CARTESIAN_POINT('Ctrl Pts',(-10.0784171780189,-19.7079979522517,
-3.97410195993235)) ;
#33318 = CARTESIAN_POINT('Ctrl Pts',(-10.8285062145454,-19.3026150680927,
-3.99324575402595)) ;
#33319 = CARTESIAN_POINT('Ctrl Pts',(-11.1313945415384,-19.1295465400972,
-4.00113451966606)) ;
#33320 = CARTESIAN_POINT('Ctrl Pts',(-11.8394751691021,-18.7024400557531,
-4.02008756982268)) ;
#33321 = CARTESIAN_POINT('Ctrl Pts',(-12.240772292093,-18.4422863452518,-4.03121658323939)) ;
#33322 = CARTESIAN_POINT('Ctrl Pts',(-13.258423038794,-17.7347035692855,-4.06019809312191)) ;
#33323 = CARTESIAN_POINT('Ctrl Pts',(-13.8606777930296,-17.2680951606565,
-4.07809559863234)) ;
#33324 = CARTESIAN_POINT('Ctrl Pts',(-14.8885916697527,-16.3832128387353,
-4.10963347141587)) ;
#33325 = CARTESIAN_POINT('Ctrl Pts',(-15.3236639289168,-15.9770196403791,
-4.12334136308469)) ;
#33326 = CARTESIAN_POINT('Ctrl Pts',(-16.2306949339859,-15.059022136013,-4.15273972809553)) ;
#33327 = CARTESIAN_POINT('Ctrl Pts',(-16.6959532686593,-14.5414840903016,
-4.16835345192879)) ;
#33328 = CARTESIAN_POINT('Ctrl Pts',(-17.6782179986661,-13.3394357884123,
-4.2029682176775)) ;
#33329 = CARTESIAN_POINT('Ctrl Pts',(-18.1813772124013,-12.6450561919917,
-4.22187730826934)) ;
#33330 = CARTESIAN_POINT('Ctrl Pts',(-18.8155515565008,-11.653472146878,-4.24840115225942)) ;
#33331 = CARTESIAN_POINT('Ctrl Pts',(-18.9822182306007,-11.3799729444245,
-4.25567957345567)) ;
#33332 = CARTESIAN_POINT('Ctrl Pts',(-19.4225573565425,-10.6207724804839,
-4.27586109499909)) ;
#33333 = CARTESIAN_POINT('Ctrl Pts',(-19.6839032677579,-10.1282026736812,
-4.28888783124412)) ;
#33334 = CARTESIAN_POINT('Ctrl Pts',(-20.2673658974562,-8.92043861104602,
-4.32030592670864)) ;
#33335 = CARTESIAN_POINT('Ctrl Pts',(-20.5706158135332,-8.19695809928377,
-4.33869147029722)) ;
#33336 = CARTESIAN_POINT('Ctrl Pts',(-21.021834729172,-6.93657721917457,-4.36967795612505)) ;
#33337 = CARTESIAN_POINT('Ctrl Pts',(-21.1891242913723,-6.40739082956183,
-4.38239397725943)) ;
#33338 = CARTESIAN_POINT('Ctrl Pts',(-21.5505913360704,-5.09407958436841,
-4.41329471133959)) ;
#33339 = CARTESIAN_POINT('Ctrl Pts',(-21.7220754018432,-4.30454222400385,
-4.43129698086119)) ;
#33340 = CARTESIAN_POINT('Ctrl Pts',(-21.9346704254269,-2.98014012052194,
-4.46112880058563)) ;
#33341 = CARTESIAN_POINT('Ctrl Pts',(-22.0001941963648,-2.44999059466151,
-4.47298184936933)) ;
#33342 = CARTESIAN_POINT('Ctrl Pts',(-22.0775121595318,-1.56125497948422,
-4.49299584415311)) ;
#33343 = CARTESIAN_POINT('Ctrl Pts',(-22.0998842892926,-1.20381656046676,
-4.50108622449457)) ;
#33344 = CARTESIAN_POINT('Ctrl Pts',(-22.1317623476045,-0.37055021076278,
-4.52018548448845)) ;
#33345 = CARTESIAN_POINT('Ctrl Pts',(-22.1346133513152,0.105353776105306,
-4.53125492860899)) ;
#33346 = CARTESIAN_POINT('Ctrl Pts',(-22.1019459321339,1.34924782320897,-4.56034283612349)) ;
#33347 = CARTESIAN_POINT('Ctrl Pts',(-22.0417613568237,2.11595065717036,-4.57841263321092)) ;
#33348 = CARTESIAN_POINT('Ctrl Pts',(-21.8641885173178,3.469778717009,-4.61016664978308)) ;
#33349 = CARTESIAN_POINT('Ctrl Pts',(-21.7626520881668,4.05821216683142,-4.62392093804273)) ;
#33350 = CARTESIAN_POINT('Ctrl Pts',(-21.4926247252075,5.31692106606395,-4.65325094552115)) ;
#33351 = CARTESIAN_POINT('Ctrl Pts',(-21.3162817870169,5.98487320121514,-4.66875455218612)) ;
#33352 = CARTESIAN_POINT('Ctrl Pts',(-20.8510098801605,7.46322647123125,-4.70331895447133)) ;
#33353 = CARTESIAN_POINT('Ctrl Pts',(-20.5454905604847,8.26723441600469,-4.72228336145066)) ;
#33354 = CARTESIAN_POINT('Ctrl Pts',(-20.0623774469812,9.3450733381197,-4.74889227402707)) ;
#33355 = CARTESIAN_POINT('Ctrl Pts',(-19.924372457776,9.63580647890616,-4.7562028171952)) ;
#33356 = CARTESIAN_POINT('Ctrl Pts',(-19.5292677768152,10.4233567425039,-4.77645809541545)) ;
#33357 = CARTESIAN_POINT('Ctrl Pts',(-19.2595988116131,10.913593088194,-4.78952821243563)) ;
#33358 = CARTESIAN_POINT('Ctrl Pts',(-18.5679490044021,12.0653215252867,-4.82099568293175)) ;
#33359 = CARTESIAN_POINT('Ctrl Pts',(-18.1288013307063,12.7156316242544,-4.83938771094345)) ;
#33360 = CARTESIAN_POINT('Ctrl Pts',(-17.3213657906186,13.7842064524659,-4.87039066200427)) ;
#33361 = CARTESIAN_POINT('Ctrl Pts',(-16.9701152389385,14.2144031090547,-4.88311642380444)) ;
#33362 = CARTESIAN_POINT('Ctrl Pts',(-16.0580501673271,15.2494064568733,-4.91441356788873)) ;
#33363 = CARTESIAN_POINT('Ctrl Pts',(-15.4789107718696,15.8369411127266,-4.93278781134249)) ;
#33364 = CARTESIAN_POINT('Ctrl Pts',(-14.4797167438843,16.743325414955,-4.96278872713749)) ;
#33365 = CARTESIAN_POINT('Ctrl Pts',(-14.0786761609113,17.0819207741667,-4.97443814105603)) ;
#33366 = CARTESIAN_POINT('Ctrl Pts',(-13.3865805637117,17.625308040362,-4.99418376146878)) ;
#33367 = CARTESIAN_POINT('Ctrl Pts',(-13.1019374029501,17.8379163231805,-5.00221205674375)) ;
#33368 = CARTESIAN_POINT('Ctrl Pts',(-12.4262785704206,18.3176849515461,-5.0211959024732)) ;
#33369 = CARTESIAN_POINT('Ctrl Pts',(-12.0315617059617,18.579329903176,-5.03221118505256)) ;
#33370 = CARTESIAN_POINT('Ctrl Pts',(-10.975184780307,19.2317773622652,-5.06123625810335)) ;
#33371 = CARTESIAN_POINT('Ctrl Pts',(-10.3010314096455,19.6011402879855,-5.07929759429781)) ;
#33372 = CARTESIAN_POINT('Ctrl Pts',(-9.07144627497917,20.1938320888549,-5.11104100138105)) ;
#33373 = CARTESIAN_POINT('Ctrl Pts',(-8.52358819327445,20.431114612194,-5.12479301574892)) ;
#33374 = CARTESIAN_POINT('Ctrl Pts',(-7.32242041396754,20.8946179175482,-5.15412617223657)) ;
#33375 = CARTESIAN_POINT('Ctrl Pts',(-6.66674359863551,21.1129684717986,-5.16963498145321)) ;
#33376 = CARTESIAN_POINT('Ctrl Pts',(-5.17488102333366,21.5333405703672,-5.20420171504553)) ;
#33377 = CARTESIAN_POINT('Ctrl Pts',(-4.33496867318201,21.7180151301816,-5.22316346411793)) ;
#33378 = CARTESIAN_POINT('Ctrl Pts',(-3.16875812005566,21.904070574223,-5.24976824930907)) ;
#33379 = CARTESIAN_POINT('Ctrl Pts',(-2.84999765764796,21.9478210514412,-5.25707720977021)) ;
#33380 = CARTESIAN_POINT('Ctrl Pts',(-1.97483220502725,22.0485511818991,-5.27732906589829)) ;
#33381 = CARTESIAN_POINT('Ctrl Pts',(-1.41704952437104,22.0914131940008,-5.29039726590137)) ;
#33382 = CARTESIAN_POINT('Ctrl Pts',(-0.0761744825440683,22.1434547999542,
-5.32182810271876)) ;
#33383 = CARTESIAN_POINT('Ctrl Pts',(0.706961598408949,22.1322978877363,-5.34018540968855)) ;
#33384 = CARTESIAN_POINT('Ctrl Pts',(2.04201585686068,22.0423340601216,-5.37116083124624)) ;
#33385 = CARTESIAN_POINT('Ctrl Pts',(2.5945730176349,21.9841423993488,-5.38389257137758)) ;
#33386 = CARTESIAN_POINT('Ctrl Pts',(3.96929825990537,21.7868092126303,-5.41540176041185)) ;
#33387 = CARTESIAN_POINT('Ctrl Pts',(4.78689211074122,21.6218884100961,-5.43397407139527)) ;
#33388 = CARTESIAN_POINT('Ctrl Pts',(6.09621737926986,21.2798548727959,-5.46406798866477)) ;
#33389 = CARTESIAN_POINT('Ctrl Pts',(6.59441139680776,21.130779089994,-5.47561162401545)) ;
#33390 = CARTESIAN_POINT('Ctrl Pts',(7.42200204430552,20.8510156442929,-5.49521776033945)) ;
#33391 = CARTESIAN_POINT('Ctrl Pts',(7.75434879016758,20.7297139969472,-5.50321373789683)) ;
#33392 = CARTESIAN_POINT('Ctrl Pts',(8.52316269327929,20.4280310792644,-5.52213587572265)) ;
#33393 = CARTESIAN_POINT('Ctrl Pts',(8.95704681294598,20.2415430278296,-5.53312128606359)) ;
#33394 = CARTESIAN_POINT('Ctrl Pts',(10.0801606824826,19.715629156828,-5.56211215592589)) ;
#33395 = CARTESIAN_POINT('Ctrl Pts',(10.7582680191723,19.3539491804508,-5.58016929236793)) ;
#33396 = CARTESIAN_POINT('Ctrl Pts',(11.9274044668907,18.6499050700725,-5.61190743373268)) ;
#33397 = CARTESIAN_POINT('Ctrl Pts',(12.4259531766966,18.3215073648659,-5.62565831993863)) ;
#33398 = CARTESIAN_POINT('Ctrl Pts',(13.4716902267222,17.5703337037636,-5.65499305360478)) ;
#33399 = CARTESIAN_POINT('Ctrl Pts',(14.0135813377178,17.1412546618382,-5.67050445835928)) ;
#33400 = CARTESIAN_POINT('Ctrl Pts',(15.1824117125005,16.1232260543807,-5.70507235750584)) ;
#33401 = CARTESIAN_POINT('Ctrl Pts',(15.7968900275897,15.521671756844,-5.72403278287323)) ;
#33402 = CARTESIAN_POINT('Ctrl Pts',(16.5912136510912,14.6478988622716,-5.75063551409591)) ;
#33403 = CARTESIAN_POINT('Ctrl Pts',(16.802376499957,14.4051884839352,-5.75794368786569)) ;
#33404 = CARTESIAN_POINT('Ctrl Pts',(17.365926768366,13.7281867576746,-5.77819383399693)) ;
#33405 = CARTESIAN_POINT('Ctrl Pts',(17.7072580479724,13.2850115320437,-5.79126107171641)) ;
#33406 = CARTESIAN_POINT('Ctrl Pts',(18.4847424476353,12.1922735212756,-5.82267362763488)) ;
#33407 = CARTESIAN_POINT('Ctrl Pts',(18.9039666108296,11.5315781560394,-5.84101361371161)) ;
#33408 = CARTESIAN_POINT('Ctrl Pts',(19.5597153226286,10.3659049976172,-5.87197532144633)) ;
#33409 = CARTESIAN_POINT('Ctrl Pts',(19.8137617581694,9.87164127779549,-5.88471006449852)) ;
#33410 = CARTESIAN_POINT('Ctrl Pts',(20.4035568290975,8.60943617051446,-5.91631948121035)) ;
#33411 = CARTESIAN_POINT('Ctrl Pts',(20.7147973820972,7.83100900801546,-5.93498520188137)) ;
#33412 = CARTESIAN_POINT('Ctrl Pts',(21.1457489774053,6.54607143869715,-5.96512365156787)) ;
#33413 = CARTESIAN_POINT('Ctrl Pts',(21.2930687282403,6.0497084329768,-5.97661799940822)) ;
#33414 = CARTESIAN_POINT('Ctrl Pts',(21.5113686385928,5.20687011928226,-5.99615913005439)) ;
#33415 = CARTESIAN_POINT('Ctrl Pts',(21.5916974680388,4.86303171155186,-6.00414003828569)) ;
#33416 = CARTESIAN_POINT('Ctrl Pts',(21.7600197712438,4.05582412939803,-6.02303301427399)) ;
#33417 = CARTESIAN_POINT('Ctrl Pts',(21.8414955137431,3.59127264945049,-6.03400409591986)) ;
#33418 = CARTESIAN_POINT('Ctrl Pts',(22.0164919121313,2.36424057376675,-6.06297865359718)) ;
#33419 = CARTESIAN_POINT('Ctrl Pts',(22.085270287227,1.59887246678189,-6.08103387237598)) ;
#33420 = CARTESIAN_POINT('Ctrl Pts',(22.1365444622168,0.235181564788166,-6.11276960939535)) ;
#33421 = CARTESIAN_POINT('Ctrl Pts',(22.1348375113695,-0.361783735674271,
-6.12651998052101)) ;
#33422 = CARTESIAN_POINT('Ctrl Pts',(22.0790999003191,-1.64817696238934,-6.15585543692131)) ;
#33423 = CARTESIAN_POINT('Ctrl Pts',(22.0168874746631,-2.33662468130006,-6.17136802927127)) ;
#33424 = CARTESIAN_POINT('Ctrl Pts',(21.8052840313235,-3.87215491530582,-6.20593646212339)) ;
#33425 = CARTESIAN_POINT('Ctrl Pts',(21.638530448543,-4.71571630429198,-6.22489628219893)) ;
#33426 = CARTESIAN_POINT('Ctrl Pts',(21.3425265379606,-5.85882764679597,-6.25149807459006)) ;
#33427 = CARTESIAN_POINT('Ctrl Pts',(21.2551151160185,-6.16841808170601,-6.2588058890153)) ;
#33428 = CARTESIAN_POINT('Ctrl Pts',(20.9973520955256,-7.01068523466416,-6.27905525207966)) ;
#33429 = CARTESIAN_POINT('Ctrl Pts',(20.8135128120323,-7.53897749788815,-6.29212204818657)) ;
#33430 = CARTESIAN_POINT('Ctrl Pts',(20.3252082260409,-8.78764012677162,-6.32352623903764)) ;
#33431 = CARTESIAN_POINT('Ctrl Pts',(20.0021882940404,-9.49995701454437,-6.34185830059628)) ;
#33432 = CARTESIAN_POINT('Ctrl Pts',(19.3862409872981,-10.686822267341,-6.37281373851423)) ;
#33433 = CARTESIAN_POINT('Ctrl Pts',(19.1118392659059,-11.1701439682956,-6.38554986009722)) ;
#33434 = CARTESIAN_POINT('Ctrl Pts',(18.3778314702062,-12.3566189996006,-6.41720408757462)) ;
#33435 = CARTESIAN_POINT('Ctrl Pts',(17.8958499836011,-13.0448950264439,-6.43591152766555)) ;
#33436 = CARTESIAN_POINT('Ctrl Pts',(17.0560146186469,-14.1097512675814,-6.46607000174394)) ;
#33437 = CARTESIAN_POINT('Ctrl Pts',(16.7219960302373,-14.5040532669279,-6.47754245598373)) ;
#33438 = CARTESIAN_POINT('Ctrl Pts',(16.1372058629939,-15.147304920914,-6.49705470885759)) ;
#33439 = CARTESIAN_POINT('Ctrl Pts',(15.8937185273065,-15.4025962308711,-6.50502892159334)) ;
#33440 = CARTESIAN_POINT('Ctrl Pts',(15.3294933987821,-15.9665428946197,-6.52330751926019)) ;
#33441 = CARTESIAN_POINT('Ctrl Pts',(15.0053374985415,-16.2715611622163,-6.53365313101545)) ;
#33442 = CARTESIAN_POINT('Ctrl Pts',(14.0859161431552,-17.085846792298,-6.56234821794787)) ;
#33443 = CARTESIAN_POINT('Ctrl Pts',(13.4724697939694,-17.5736097348172,-6.58076895856172)) ;
#33444 = CARTESIAN_POINT('Ctrl Pts',(12.3450672819344,-18.3762358898492,-6.61296233748966)) ;
#33445 = CARTESIAN_POINT('Ctrl Pts',(11.8416872239089,-18.7045765399974,-6.62681027876094)) ;
#33446 = CARTESIAN_POINT('Ctrl Pts',(10.7403532416062,-19.3606471926614,-6.65602433380518)) ;
#33447 = CARTESIAN_POINT('Ctrl Pts',(10.1393504172356,-19.6820585724023,-6.67132693531074)) ;
#33448 = CARTESIAN_POINT('Ctrl Pts',(8.73780570539514,-20.3503350997291,-6.70596589931371)) ;
#33449 = CARTESIAN_POINT('Ctrl Pts',(7.92966609128081,-20.6786306949514,-6.72519313103484)) ;
#33450 = CARTESIAN_POINT('Ctrl Pts',(6.79854002410633,-21.0620489817465,-6.75209409975387)) ;
#33451 = CARTESIAN_POINT('Ctrl Pts',(6.49057147896317,-21.1589823837779,-6.75942636518843)) ;
#33452 = CARTESIAN_POINT('Ctrl Pts',(5.50761057293395,-21.4448892819535,-6.78295567123037)) ;
#33453 = CARTESIAN_POINT('Ctrl Pts',(4.8257155288337,-21.6085518542192,-6.79939307837907)) ;
#33454 = CARTESIAN_POINT('Ctrl Pts',(3.31406344596355,-21.8962309070508,-6.83545312907827)) ;
#33455 = CARTESIAN_POINT('Ctrl Pts',(2.48267867047688,-22.0060053046048,-6.85502984038374)) ;
#33456 = CARTESIAN_POINT('Ctrl Pts',(1.09890934430578,-22.1092828813567,-6.8869385881317)) ;
#33457 = CARTESIAN_POINT('Ctrl Pts',(0.549410420858502,-22.1297570180054,
-6.89944285905113)) ;
#33458 = CARTESIAN_POINT('Ctrl Pts',(-0.000282606165597638,-22.1297499981955,
-6.91183148751768)) ;
#33459 = CARTESIAN_POINT('Origin',(0.,0.,-10.)) ;
#33460 = CARTESIAN_POINT('',(0.000546534359808369,-22.1297499932512,-10.5515753459688)) ;
#33461 = CARTESIAN_POINT('',(0.000544184811332343,-22.1297499933091,-10.0859246540312)) ;
#33462 = CARTESIAN_POINT('',(-2.71011275034311E-15,-22.12975,-10.)) ;
#33463 = CARTESIAN_POINT('Ctrl Pts',(0.000540719825256331,-22.129749993394,
-10.5513173733145)) ;
#33464 = CARTESIAN_POINT('Ctrl Pts',(0.762095726907136,-22.1297313855069,
-10.5343591835597)) ;
#33465 = CARTESIAN_POINT('Ctrl Pts',(1.52313896987673,-22.0904015410209,-10.5175178070212)) ;
#33466 = CARTESIAN_POINT('Ctrl Pts',(2.46957986378866,-21.9923417204627,-10.4960849774183)) ;
#33467 = CARTESIAN_POINT('Ctrl Pts',(2.65826587189515,-21.9703332061555,-10.4917864962238)) ;
#33468 = CARTESIAN_POINT('Ctrl Pts',(3.20059935057029,-21.8999860919078,-10.4793296251818)) ;
#33469 = CARTESIAN_POINT('Ctrl Pts',(3.55338801608267,-21.8455179729674,-10.4710914043089)) ;
#33470 = CARTESIAN_POINT('Ctrl Pts',(5.0229221375274,-21.5820918098613,-10.4363885586976)) ;
#33471 = CARTESIAN_POINT('Ctrl Pts',(6.12405154544231,-21.2958319946136,-10.4095514665115)) ;
#33472 = CARTESIAN_POINT('Ctrl Pts',(7.70127965579003,-20.7532892737035,-10.370960661644)) ;
#33473 = CARTESIAN_POINT('Ctrl Pts',(8.19782997801918,-20.5622059485252,-10.3587706550181)) ;
#33474 = CARTESIAN_POINT('Ctrl Pts',(9.49776919282978,-20.0073806145368,-10.3266953770978)) ;
#33475 = CARTESIAN_POINT('Ctrl Pts',(10.2871236764243,-19.613209729006,-10.3070717203552)) ;
#33476 = CARTESIAN_POINT('Ctrl Pts',(11.4800427761846,-18.9256397460823,-10.276454588413)) ;
#33477 = CARTESIAN_POINT('Ctrl Pts',(11.9007945870188,-18.6639306469199,-10.2654464559592)) ;
#33478 = CARTESIAN_POINT('Ctrl Pts',(12.6000660078886,-18.1957142696058,-10.246546686971)) ;
#33479 = CARTESIAN_POINT('Ctrl Pts',(12.8831653026854,-17.9963811083354,-10.2387144414267)) ;
#33480 = CARTESIAN_POINT('Ctrl Pts',(13.5223146590674,-17.523535964734,-10.2204881226047)) ;
#33481 = CARTESIAN_POINT('Ctrl Pts',(13.8749505604901,-17.2456675608656,-10.2100483139881)) ;
#33482 = CARTESIAN_POINT('Ctrl Pts',(14.8138223177842,-16.4584114513644,-10.1814141036847)) ;
#33483 = CARTESIAN_POINT('Ctrl Pts',(15.38209214591,-15.9285871194822,-10.1631556407688)) ;
#33484 = CARTESIAN_POINT('Ctrl Pts',(16.3373450500845,-14.9390679654304,-10.1311652604074)) ;
#33485 = CARTESIAN_POINT('Ctrl Pts',(16.7356857981465,-14.491425876617,-10.1173604691735)) ;
#33486 = CARTESIAN_POINT('Ctrl Pts',(17.5498010528388,-13.4981469347963,-10.0880962604202)) ;
#33487 = CARTESIAN_POINT('Ctrl Pts',(17.9593703875175,-12.9482242835916,-10.0727042055298)) ;
#33488 = CARTESIAN_POINT('Ctrl Pts',(18.829054097094,-11.6596808707316,-10.0380285644672)) ;
#33489 = CARTESIAN_POINT('Ctrl Pts',(19.2724686936224,-10.9111580964574,-10.0188501502847)) ;
#33490 = CARTESIAN_POINT('Ctrl Pts',(19.8179927085283,-9.85273357247716,-9.99202394782781)) ;
#33491 = CARTESIAN_POINT('Ctrl Pts',(19.9590351020614,-9.56379168728507,-9.98471958940597)) ;
#33492 = CARTESIAN_POINT('Ctrl Pts',(20.3279332066873,-8.76432668004247,-9.96447782213127)) ;
#33493 = CARTESIAN_POINT('Ctrl Pts',(20.5428169909606,-8.24808799080209,-9.95141534084429)) ;
#33494 = CARTESIAN_POINT('Ctrl Pts',(21.0095885200011,-6.99491189769223,-9.92009218985851)) ;
#33495 = CARTESIAN_POINT('Ctrl Pts',(21.2425882685759,-6.25172432944614,-9.90183686438735)) ;
#33496 = CARTESIAN_POINT('Ctrl Pts',(21.5741080760839,-4.95912883785754,-9.87094197651316)) ;
#33497 = CARTESIAN_POINT('Ctrl Pts',(21.691912650421,-4.41543093035463,-9.85819233589921)) ;
#33498 = CARTESIAN_POINT('Ctrl Pts',(21.9388741959413,-3.0242074697657,-9.8261311893627)) ;
#33499 = CARTESIAN_POINT('Ctrl Pts',(22.0395108236542,-2.17255722896388,-9.80704610589948)) ;
#33500 = CARTESIAN_POINT('Ctrl Pts',(22.1207319068342,-0.810431891061295,
-9.77670275464389)) ;
#33501 = CARTESIAN_POINT('Ctrl Pts',(22.1335020853793,-0.302757897646345,
-9.76542529530909)) ;
#33502 = CARTESIAN_POINT('Ctrl Pts',(22.1255607590194,0.554876675373889,-9.7461702710391)) ;
#33503 = CARTESIAN_POINT('Ctrl Pts',(22.1140182192634,0.90472380008027,-9.73825570784952)) ;
#33504 = CARTESIAN_POINT('Ctrl Pts',(22.0674595242356,1.7249419367817,-9.71942779428143)) ;
#33505 = CARTESIAN_POINT('Ctrl Pts',(22.0256947440072,2.19475769186084,-9.70845457187096)) ;
#33506 = CARTESIAN_POINT('Ctrl Pts',(21.8767902027992,3.42323237869518,-9.67952435369552)) ;
#33507 = CARTESIAN_POINT('Ctrl Pts',(21.7452140933535,4.17829399881221,-9.661517289963)) ;
#33508 = CARTESIAN_POINT('Ctrl Pts',(21.4420736718042,5.50624659832969,-9.6298419328156)) ;
#33509 = CARTESIAN_POINT('Ctrl Pts',(21.2859565341147,6.0818860057907,-9.61610449904824)) ;
#33510 = CARTESIAN_POINT('Ctrl Pts',(20.8987434611677,7.31078572688398,-9.5867505051528)) ;
#33511 = CARTESIAN_POINT('Ctrl Pts',(20.6598334973586,7.96092679006804,-9.57120771241524)) ;
#33512 = CARTESIAN_POINT('Ctrl Pts',(20.0572804006495,9.38979628386058,-9.5366256087694)) ;
#33513 = CARTESIAN_POINT('Ctrl Pts',(19.6779772234578,10.1607070876448,-9.5176810894635)) ;
#33514 = CARTESIAN_POINT('Ctrl Pts',(19.0965251600906,11.1871242592951,-9.49110295988983)) ;
#33515 = CARTESIAN_POINT('Ctrl Pts',(18.9321293204769,11.4631366369296,-9.48380416194124)) ;
#33516 = CARTESIAN_POINT('Ctrl Pts',(18.4655201013132,12.2091157710813,-9.46357480523829)) ;
#33517 = CARTESIAN_POINT('Ctrl Pts',(18.1514306729884,12.6713653519658,-9.45051946233114)) ;
#33518 = CARTESIAN_POINT('Ctrl Pts',(17.3618161468266,13.7437555808279,-9.41932620432493)) ;
#33519 = CARTESIAN_POINT('Ctrl Pts',(16.8711351564821,14.3418369398485,-9.40119365418368)) ;
#33520 = CARTESIAN_POINT('Ctrl Pts',(15.9748183156088,15.3245308590199,-9.37039514729629)) ;
#33521 = CARTESIAN_POINT('Ctrl Pts',(15.5840684437473,15.7217328453806,-9.35762334935739)) ;
#33522 = CARTESIAN_POINT('Ctrl Pts',(14.537273531759,16.7083983983751,-9.32497819411947)) ;
#33523 = CARTESIAN_POINT('Ctrl Pts',(13.8602448884879,17.2741576095613,-9.30535453637654)) ;
#33524 = CARTESIAN_POINT('Ctrl Pts',(12.7528753303465,18.0924125734482,-9.27473740391591)) ;
#33525 = CARTESIAN_POINT('Ctrl Pts',(12.3447027376042,18.3733375654329,-9.26372927195394)) ;
#33526 = CARTESIAN_POINT('Ctrl Pts',(11.6358481714235,18.8269147369149,-9.24482950361424)) ;
#33527 = CARTESIAN_POINT('Ctrl Pts',(11.3399092199787,19.0066341073481,-9.23699725822009)) ;
#33528 = CARTESIAN_POINT('Ctrl Pts',(10.6508634620417,19.4032578182766,-9.21877093945944)) ;
#33529 = CARTESIAN_POINT('Ctrl Pts',(10.2551297930757,19.6152903523379,-9.20833113074951)) ;
#33530 = CARTESIAN_POINT('Ctrl Pts',(9.15802654994961,20.1608330399417,-9.17969692051981)) ;
#33531 = CARTESIAN_POINT('Ctrl Pts',(8.44511392172443,20.4697019334919,-9.16143845777831)) ;
#33532 = CARTESIAN_POINT('Ctrl Pts',(7.15608378908251,20.9493450914963,-9.12944807763529)) ;
#33533 = CARTESIAN_POINT('Ctrl Pts',(6.5864691028667,21.1353501940812,-9.11564328644785)) ;
#33534 = CARTESIAN_POINT('Ctrl Pts',(5.35045348936089,21.4841368253889,-9.08637907763762)) ;
#33535 = CARTESIAN_POINT('Ctrl Pts',(4.68260693566097,21.6395168408771,-9.07098702264814)) ;
#33536 = CARTESIAN_POINT('Ctrl Pts',(3.15375234121765,21.9211149890816,-9.03631138154412)) ;
#33537 = CARTESIAN_POINT('Ctrl Pts',(2.29034965854265,22.0280666194252,-9.017132967415)) ;
#33538 = CARTESIAN_POINT('Ctrl Pts',(1.10207481223357,22.104629039023,-8.99030676503934)) ;
#33539 = CARTESIAN_POINT('Ctrl Pts',(0.780837682334844,22.118306584276,-8.9830024066474)) ;
#33540 = CARTESIAN_POINT('Ctrl Pts',(-0.0994440898910114,22.1365851359504,
-8.96276063943875)) ;
#33541 = CARTESIAN_POINT('Ctrl Pts',(-0.65853778333759,22.127010946221,-8.94969815818945)) ;
#33542 = CARTESIAN_POINT('Ctrl Pts',(-1.99379820879595,22.0534888599294,-8.91837500790101)) ;
#33543 = CARTESIAN_POINT('Ctrl Pts',(-2.76813729940817,21.9697298410208,-8.90011968308962)) ;
#33544 = CARTESIAN_POINT('Ctrl Pts',(-4.08541978207517,21.7564804901518,-8.86922479573512)) ;
#33545 = CARTESIAN_POINT('Ctrl Pts',(-4.63084448323932,21.6469486097091,-8.85647515500396)) ;
#33546 = CARTESIAN_POINT('Ctrl Pts',(-6.00469305098502,21.3167467829983,-8.82441400514067)) ;
#33547 = CARTESIAN_POINT('Ctrl Pts',(-6.82548797393584,21.0682879327733,-8.80532891859824)) ;
#33548 = CARTESIAN_POINT('Ctrl Pts',(-8.106365642801,20.5978255147595,-8.77498556580996)) ;
#33549 = CARTESIAN_POINT('Ctrl Pts',(-8.57675668872774,20.4064406876266,-8.76370810804303)) ;
#33550 = CARTESIAN_POINT('Ctrl Pts',(-9.35960075557722,20.0560764035901,-8.74445308584147)) ;
#33551 = CARTESIAN_POINT('Ctrl Pts',(-9.67561772485194,19.9055456740926,-8.73653852313158)) ;
#33552 = CARTESIAN_POINT('Ctrl Pts',(-10.40872144524,19.5347565258284,-8.71771060739032)) ;
#33553 = CARTESIAN_POINT('Ctrl Pts',(-10.8225995962712,19.308535117142,-8.70673738224158)) ;
#33554 = CARTESIAN_POINT('Ctrl Pts',(-11.8889276660209,18.6806281565569,-8.67780716318418)) ;
#33555 = CARTESIAN_POINT('Ctrl Pts',(-12.5283052020121,18.2579857965525,-8.65980010139932)) ;
#33556 = CARTESIAN_POINT('Ctrl Pts',(-13.6241043880534,17.4489270313781,-8.62812474669491)) ;
#33557 = CARTESIAN_POINT('Ctrl Pts',(-14.089224416217,17.0755684614998,-8.61438731345167)) ;
#33558 = CARTESIAN_POINT('Ctrl Pts',(-15.0606096536722,16.2290820177373,-8.5850333187972)) ;
#33559 = CARTESIAN_POINT('Ctrl Pts',(-15.5608901637451,15.7500404090239,-8.56949052482841)) ;
#33560 = CARTESIAN_POINT('Ctrl Pts',(-16.6294033107615,14.6261996704882,-8.53490842062286)) ;
#33561 = CARTESIAN_POINT('Ctrl Pts',(-17.1842065019089,13.9701754812838,-8.51596390193861)) ;
#33562 = CARTESIAN_POINT('Ctrl Pts',(-17.8923137791708,13.0266699505038,-8.48938577332376)) ;
#33563 = CARTESIAN_POINT('Ctrl Pts',(-18.0795142343541,12.7655860501095,-8.48208697573891)) ;
#33564 = CARTESIAN_POINT('Ctrl Pts',(-18.5765418796839,12.0395196039001,-8.46185761985641)) ;
#33565 = CARTESIAN_POINT('Ctrl Pts',(-18.8745454225178,11.5667398358092,-8.44880227742517)) ;
#33566 = CARTESIAN_POINT('Ctrl Pts',(-19.5415139796137,10.4140630033365,-8.4176090279121)) ;
#33567 = CARTESIAN_POINT('Ctrl Pts',(-19.8933637737102,9.72509976892042,-8.39947648578958)) ;
#33568 = CARTESIAN_POINT('Ctrl Pts',(-20.435440959096,8.51051227232673,-8.36867798517615)) ;
#33569 = CARTESIAN_POINT('Ctrl Pts',(-20.6431614581329,7.9934947300125,-8.35590618576802)) ;
#33570 = CARTESIAN_POINT('Ctrl Pts',(-21.1286823965585,6.63940371242206,-8.3232609942182)) ;
#33571 = CARTESIAN_POINT('Ctrl Pts',(-21.3763634248447,5.7925813686953,-8.3036373031048)) ;
#33572 = CARTESIAN_POINT('Ctrl Pts',(-21.683303496542,4.45034500375449,-8.27302015334947)) ;
#33573 = CARTESIAN_POINT('Ctrl Pts',(-21.7774862922587,3.96387550511088,-8.26201203779432)) ;
#33574 = CARTESIAN_POINT('Ctrl Pts',(-21.90962047365,3.13276422986203,-8.24311229108966)) ;
#33575 = CARTESIAN_POINT('Ctrl Pts',(-21.9559462791796,2.78964227698622,-8.23528005070215)) ;
#33576 = CARTESIAN_POINT('Ctrl Pts',(-22.0438071261427,1.99946841653622,-8.21705373398806)) ;
#33577 = CARTESIAN_POINT('Ctrl Pts',(-22.0798263009291,1.55195789694476,-8.20661392216783)) ;
#33578 = CARTESIAN_POINT('Ctrl Pts',(-22.140932817188,0.328226692957887,-8.17797971439605)) ;
#33579 = CARTESIAN_POINT('Ctrl Pts',(-22.1388188527382,-0.448715751631449,
-8.15972125747283)) ;
#33580 = CARTESIAN_POINT('Ctrl Pts',(-22.0627506162553,-1.82198521596142,
-8.12773088461325)) ;
#33581 = CARTESIAN_POINT('Ctrl Pts',(-22.0053567394348,-2.41844531940688,
-8.11392609497779)) ;
#33582 = CARTESIAN_POINT('Ctrl Pts',(-21.8305664513511,-3.6907799035294,-8.0846618842678)) ;
#33583 = CARTESIAN_POINT('Ctrl Pts',(-21.7058082385966,-4.36501841222752,
-8.06926982596833)) ;
#33584 = CARTESIAN_POINT('Ctrl Pts',(-21.3522931415014,-5.87886159468619,
-8.03459418348151)) ;
#33585 = CARTESIAN_POINT('Ctrl Pts',(-21.1049206091465,-6.7129536335092,-8.0154157711352)) ;
#33586 = CARTESIAN_POINT('Ctrl Pts',(-20.699735332433,-7.83263371932115,-7.98858957146821)) ;
#33587 = CARTESIAN_POINT('Ctrl Pts',(-20.5837638559451,-8.13251862181145,
-7.98128521407379)) ;
#33588 = CARTESIAN_POINT('Ctrl Pts',(-20.2483703159901,-8.94660774221505,
-7.96104344906823)) ;
#33589 = CARTESIAN_POINT('Ctrl Pts',(-20.0159370831783,-9.45518630418543,
-7.94798096907533)) ;
#33590 = CARTESIAN_POINT('Ctrl Pts',(-19.4144002049621,-10.6495382721856,
-7.91665784207625)) ;
#33591 = CARTESIAN_POINT('Ctrl Pts',(-19.0278709007639,-11.3257114971367,
-7.89840253930121)) ;
#33592 = CARTESIAN_POINT('Ctrl Pts',(-18.3054661395498,-12.4476908580898,
-7.86750766930365)) ;
#33593 = CARTESIAN_POINT('Ctrl Pts',(-17.986889867788,-12.9037551818864,-7.85475802465684)) ;
#33594 = CARTESIAN_POINT('Ctrl Pts',(-17.1346663701311,-14.0307964313217,
-7.82269676367692)) ;
#33595 = CARTESIAN_POINT('Ctrl Pts',(-16.5786020927111,-14.683664502367,-7.80361157428743)) ;
#33596 = CARTESIAN_POINT('Ctrl Pts',(-15.6350224924737,-15.6693857281927,
-7.77326817030704)) ;
#33597 = CARTESIAN_POINT('Ctrl Pts',(-15.2714460072982,-16.0239355730493,
-7.76199076490811)) ;
#33598 = CARTESIAN_POINT('Ctrl Pts',(-14.6371726990142,-16.6012500093332,
-7.74273581179304)) ;
#33599 = CARTESIAN_POINT('Ctrl Pts',(-14.3727933196505,-16.8306606707578,
-7.73482126510439)) ;
#33600 = CARTESIAN_POINT('Ctrl Pts',(-13.739694001493,-17.3542215910968,-7.71599327676476)) ;
#33601 = CARTESIAN_POINT('Ctrl Pts',(-13.3667923740043,-17.6430455324717,
-7.70501996014276)) ;
#33602 = CARTESIAN_POINT('Ctrl Pts',(-12.3647437053928,-18.3691474574999,
-7.67608971162199)) ;
#33603 = CARTESIAN_POINT('Ctrl Pts',(-11.7216195426005,-18.7860615277497,
-7.65808271489854)) ;
#33604 = CARTESIAN_POINT('Ctrl Pts',(-10.5417601047706,-19.4667040855886,
-7.62640744180281)) ;
#33605 = CARTESIAN_POINT('Ctrl Pts',(-10.0135125197445,-19.7436280630044,
-7.61267002606845)) ;
#33606 = CARTESIAN_POINT('Ctrl Pts',(-8.84911697564473,-20.2952752545068,
-7.58331600606147)) ;
#33607 = CARTESIAN_POINT('Ctrl Pts',(-8.20994309330438,-20.5621475679191,
-7.56777317096577)) ;
#33608 = CARTESIAN_POINT('Ctrl Pts',(-6.75249793180721,-21.0918595977928,
-7.53319104806491)) ;
#33609 = CARTESIAN_POINT('Ctrl Pts',(-5.92931129098236,-21.3379010690314,
-7.51424655014626)) ;
#33610 = CARTESIAN_POINT('Ctrl Pts',(-4.78132155505225,-21.609442060917,-7.48766845355937)) ;
#33611 = CARTESIAN_POINT('Ctrl Pts',(-4.46715182254049,-21.6765674490351,
-7.48036966812479)) ;
#33612 = CARTESIAN_POINT('Ctrl Pts',(-3.60288431769079,-21.8416383157174,
-7.46014033964834)) ;
#33613 = CARTESIAN_POINT('Ctrl Pts',(-3.05037031223361,-21.9256282809683,
-7.44708501311407)) ;
#33614 = CARTESIAN_POINT('Ctrl Pts',(-1.72714298093534,-22.0757884641218,
-7.4158920472784)) ;
#33615 = CARTESIAN_POINT('Ctrl Pts',(-0.954967361584291,-22.1226469352701,
-7.39775977298584)) ;
#33616 = CARTESIAN_POINT('Ctrl Pts',(-0.121282485391881,-22.1295007483995,
-7.37845459755358)) ;
#33617 = CARTESIAN_POINT('Ctrl Pts',(-0.0606403391054048,-22.1297499999887,
-7.37705174916909)) ;
#33618 = CARTESIAN_POINT('Ctrl Pts',(-4.10971426655051E-9,-22.12975,-7.37565036637909)) ;
#33619 = CARTESIAN_POINT('Ctrl Pts',(-0.00028260616559278,-22.1297499981955,
-6.91183148751768)) ;
#33620 = CARTESIAN_POINT('Ctrl Pts',(-0.819491674422402,-22.129739536553,
-6.93029429545617)) ;
#33621 = CARTESIAN_POINT('Ctrl Pts',(-1.63806773940101,-22.084240462302,-6.94846154174131)) ;
#33622 = CARTESIAN_POINT('Ctrl Pts',(-3.00600318315989,-21.9317179538769,
-6.97908761796101)) ;
#33623 = CARTESIAN_POINT('Ctrl Pts',(-3.55723973935411,-21.849081122676,-6.99151028370669)) ;
#33624 = CARTESIAN_POINT('Ctrl Pts',(-4.41930546700327,-21.6863559688932,
-7.01141476232408)) ;
#33625 = CARTESIAN_POINT('Ctrl Pts',(-4.7325162783671,-21.6201660877683,-7.01876110844946)) ;
#33626 = CARTESIAN_POINT('Ctrl Pts',(-5.87816145295388,-21.3519717096865,
-7.04599713143021)) ;
#33627 = CARTESIAN_POINT('Ctrl Pts',(-6.70010493251782,-21.1084834248527,
-7.06618291258562)) ;
#33628 = CARTESIAN_POINT('Ctrl Pts',(-8.16066684744448,-20.5818817860658,
-7.10246060360338)) ;
#33629 = CARTESIAN_POINT('Ctrl Pts',(-8.80397128374435,-20.3150299762997,
-7.11859724891427)) ;
#33630 = CARTESIAN_POINT('Ctrl Pts',(-9.97165920235242,-19.7647567122671,
-7.1481251015603)) ;
#33631 = CARTESIAN_POINT('Ctrl Pts',(-10.4992490188593,-19.4896221700088,
-7.16156512524228)) ;
#33632 = CARTESIAN_POINT('Ctrl Pts',(-11.6748275289485,-18.8149620897786,
-7.1919367652821)) ;
#33633 = CARTESIAN_POINT('Ctrl Pts',(-12.314579096878,-18.4025959392554,-7.20876954850381)) ;
#33634 = CARTESIAN_POINT('Ctrl Pts',(-13.3206738957914,-17.6780964160283,
-7.23641034551954)) ;
#33635 = CARTESIAN_POINT('Ctrl Pts',(-13.7003229402307,-17.3855282332158,
-7.24714071716105)) ;
#33636 = CARTESIAN_POINT('Ctrl Pts',(-14.3392587644429,-16.8592121000339,
-7.26598459481017)) ;
#33637 = CARTESIAN_POINT('Ctrl Pts',(-14.6030669509428,-16.6312298111907,
-7.27402408190463)) ;
#33638 = CARTESIAN_POINT('Ctrl Pts',(-15.2342651569512,-16.0591489827275,
-7.29381182499496)) ;
#33639 = CARTESIAN_POINT('Ctrl Pts',(-15.5955161441776,-15.7085637566714,
-7.30561174033497)) ;
#33640 = CARTESIAN_POINT('Ctrl Pts',(-16.5447609591361,-14.7222960881541,
-7.33768930536408)) ;
#33641 = CARTESIAN_POINT('Ctrl Pts',(-17.1079171943314,-14.0639364168517,
-7.35790154269754)) ;
#33642 = CARTESIAN_POINT('Ctrl Pts',(-17.9673321132459,-12.9309860791216,
-7.39055633356931)) ;
#33643 = CARTESIAN_POINT('Ctrl Pts',(-18.28676416075,-12.4751628089138,-7.40319231462525)) ;
#33644 = CARTESIAN_POINT('Ctrl Pts',(-19.0100268947019,-11.3555141885319,
-7.43318895118883)) ;
#33645 = CARTESIAN_POINT('Ctrl Pts',(-19.3967513873857,-10.6815197404428,
-7.45040991874401)) ;
#33646 = CARTESIAN_POINT('Ctrl Pts',(-19.99950347,-9.48989114069963,-7.48012403571722)) ;
#33647 = CARTESIAN_POINT('Ctrl Pts',(-20.2327751840765,-8.98181351738652,
-7.49258484537064)) ;
#33648 = CARTESIAN_POINT('Ctrl Pts',(-20.5695113773647,-8.16849666216835,
-7.51256167368171)) ;
#33649 = CARTESIAN_POINT('Ctrl Pts',(-20.6859749634242,-7.86889901321823,
-7.5199406015)) ;
#33650 = CARTESIAN_POINT('Ctrl Pts',(-21.0930406976229,-6.75016920091236,
-7.54750433393836)) ;
#33651 = CARTESIAN_POINT('Ctrl Pts',(-21.3418410333152,-5.91666906812547,
-7.56799044642639)) ;
#33652 = CARTESIAN_POINT('Ctrl Pts',(-21.6980757449775,-4.40333921877305,
-7.60430519930574)) ;
#33653 = CARTESIAN_POINT('Ctrl Pts',(-21.8240741519265,-3.72903289084975,
-7.62019173229536)) ;
#33654 = CARTESIAN_POINT('Ctrl Pts',(-22.0010999877269,-2.45683656664787,
-7.64956534729555)) ;
#33655 = CARTESIAN_POINT('Ctrl Pts',(-22.0595243635142,-1.86060169760572,
-7.66309216097388)) ;
#33656 = CARTESIAN_POINT('Ctrl Pts',(-22.1379700816065,-0.488054587542169,
-7.69388835880274)) ;
#33657 = CARTESIAN_POINT('Ctrl Pts',(-22.1414709101615,0.288411287534252,
-7.71105209490964)) ;
#33658 = CARTESIAN_POINT('Ctrl Pts',(-22.0826013294025,1.51203279496765,-7.73837942155627)) ;
#33659 = CARTESIAN_POINT('Ctrl Pts',(-22.0473696948826,1.95984942025784,-7.74844500470503)) ;
#33660 = CARTESIAN_POINT('Ctrl Pts',(-21.9609429326348,2.74997446835613,-7.76653427809586)) ;
#33661 = CARTESIAN_POINT('Ctrl Pts',(-21.9152994632171,3.09273639080316,-7.77450458383363)) ;
#33662 = CARTESIAN_POINT('Ctrl Pts',(-21.784995354661,3.92221402986284,-7.79400337979991)) ;
#33663 = CARTESIAN_POINT('Ctrl Pts',(-21.6920321323498,4.40743980225663,-7.80558128802677)) ;
#33664 = CARTESIAN_POINT('Ctrl Pts',(-21.3875054419404,5.751758839279,-7.8378826566359)) ;
#33665 = CARTESIAN_POINT('Ctrl Pts',(-21.140558805694,6.60188719486739,-7.85854191729972)) ;
#33666 = CARTESIAN_POINT('Ctrl Pts',(-20.6562308893538,7.95966809178261,-7.89164180624271)) ;
#33667 = CARTESIAN_POINT('Ctrl Pts',(-20.4493151968511,8.47712834705992,-7.90429166485741)) ;
#33668 = CARTESIAN_POINT('Ctrl Pts',(-19.9094391876684,9.69209408409439,-7.93420761934462)) ;
#33669 = CARTESIAN_POINT('Ctrl Pts',(-19.5590447922406,10.3810513237097,-7.95133765729493)) ;
#33670 = CARTESIAN_POINT('Ctrl Pts',(-18.8944035734317,11.5342710713653,-7.98095466431243)) ;
#33671 = CARTESIAN_POINT('Ctrl Pts',(-18.5972354215638,12.0075277654691,-7.99340979918347)) ;
#33672 = CARTESIAN_POINT('Ctrl Pts',(-18.1015042952759,12.7343843025311,-8.01337550591042)) ;
#33673 = CARTESIAN_POINT('Ctrl Pts',(-17.9147735950181,12.9957640875306,-8.02074922902676)) ;
#33674 = CARTESIAN_POINT('Ctrl Pts',(-17.2083533153364,13.9404175073009,-8.04805931127953)) ;
#33675 = CARTESIAN_POINT('Ctrl Pts',(-16.6547241497918,14.5973569020333,-8.06828974708615)) ;
#33676 = CARTESIAN_POINT('Ctrl Pts',(-15.588134674716,15.723081010033,-8.10452055545454)) ;
#33677 = CARTESIAN_POINT('Ctrl Pts',(-15.0886024132755,16.2030647774855,-8.12056901467968)) ;
#33678 = CARTESIAN_POINT('Ctrl Pts',(-14.1186236484521,17.0512664924444,-8.15004102090566)) ;
#33679 = CARTESIAN_POINT('Ctrl Pts',(-13.6541827924535,17.4253987664595,-8.16351020975757)) ;
#33680 = CARTESIAN_POINT('Ctrl Pts',(-12.5599456325401,18.2362273687018,-8.19402414598921)) ;
#33681 = CARTESIAN_POINT('Ctrl Pts',(-11.9214422105821,18.6598884682918,-8.21096779052898)) ;
#33682 = CARTESIAN_POINT('Ctrl Pts',(-10.856148315205,19.2896982458853,-8.23856327101693)) ;
#33683 = CARTESIAN_POINT('Ctrl Pts',(-10.4424585024676,19.5167484475727,-8.24913142098146)) ;
#33684 = CARTESIAN_POINT('Ctrl Pts',(-9.7098270817612,19.8888801978601,-8.26783904235382)) ;
#33685 = CARTESIAN_POINT('Ctrl Pts',(-9.39411082606535,20.0399344840325,-8.27591022471452)) ;
#33686 = CARTESIAN_POINT('Ctrl Pts',(-8.61204959735149,20.3915676438154,-8.29583040065005)) ;
#33687 = CARTESIAN_POINT('Ctrl Pts',(-8.14212790196691,20.5837115376729,-8.30773206508639)) ;
#33688 = CARTESIAN_POINT('Ctrl Pts',(-6.86195215515994,21.0564510866412,-8.33971086358471)) ;
#33689 = CARTESIAN_POINT('Ctrl Pts',(-6.04130908828061,21.3064104108324,-8.35972230418106)) ;
#33690 = CARTESIAN_POINT('Ctrl Pts',(-4.66773502174942,21.6390239407721,-8.39217752456532)) ;
#33691 = CARTESIAN_POINT('Ctrl Pts',(-4.12248992523782,21.749487131587,-8.40480777695205)) ;
#33692 = CARTESIAN_POINT('Ctrl Pts',(-2.80561696346871,21.9649729147315,-8.43483858252193)) ;
#33693 = CARTESIAN_POINT('Ctrl Pts',(-2.03147827827453,22.050048096241,-8.45209790799911)) ;
#33694 = CARTESIAN_POINT('Ctrl Pts',(-0.696393312061845,22.1258519331186,
-8.48185293993438)) ;
#33695 = CARTESIAN_POINT('Ctrl Pts',(-0.137320563919265,22.1363823437349,
-8.49431609272986)) ;
#33696 = CARTESIAN_POINT('Ctrl Pts',(0.742980542592581,22.1196105906853,-8.51429755452301)) ;
#33697 = CARTESIAN_POINT('Ctrl Pts',(1.06423893510949,22.1064828522234,-8.52167867267012)) ;
#33698 = CARTESIAN_POINT('Ctrl Pts',(2.25263268205027,22.0319554861014,-8.54924843143638)) ;
#33699 = CARTESIAN_POINT('Ctrl Pts',(3.11621067896902,21.9264828235127,-8.5697382211251)) ;
#33700 = CARTESIAN_POINT('Ctrl Pts',(4.64553740269503,21.6475052213926,-8.60604961950149)) ;
#33701 = CARTESIAN_POINT('Ctrl Pts',(5.31365952255052,21.4932671810344,-8.6219293971111)) ;
#33702 = CARTESIAN_POINT('Ctrl Pts',(6.55027511474448,21.1465950943765,-8.65129903202456)) ;
#33703 = CARTESIAN_POINT('Ctrl Pts',(7.12020155330308,20.9615678145442,-8.66482837190709)) ;
#33704 = CARTESIAN_POINT('Ctrl Pts',(8.41003049428063,20.4841401775169,-8.6956369788407)) ;
#33705 = CARTESIAN_POINT('Ctrl Pts',(9.12345027044491,20.1765028036385,-8.7128103966964)) ;
#33706 = CARTESIAN_POINT('Ctrl Pts',(10.2214844461911,19.6328442146709,-8.74014301963547)) ;
#33707 = CARTESIAN_POINT('Ctrl Pts',(10.6175902287654,19.4214852558423,-8.75020371231221)) ;
#33708 = CARTESIAN_POINT('Ctrl Pts',(11.3073047997766,19.0260486529937,-8.76829806559389)) ;
#33709 = CARTESIAN_POINT('Ctrl Pts',(11.6035334716215,18.846847880448,-8.77627861929453)) ;
#33710 = CARTESIAN_POINT('Ctrl Pts',(12.3130898457904,18.3945364964279,-8.79582021880085)) ;
#33711 = CARTESIAN_POINT('Ctrl Pts',(12.7216895063439,18.1143525614546,-8.80743101771404)) ;
#33712 = CARTESIAN_POINT('Ctrl Pts',(13.8305142969275,17.2979769088126,-8.83969854471356)) ;
#33713 = CARTESIAN_POINT('Ctrl Pts',(14.5086199203236,16.7332931912151,-8.86029083925275)) ;
#33714 = CARTESIAN_POINT('Ctrl Pts',(15.5572016390319,15.7483188943685,-8.89332398568439)) ;
#33715 = CARTESIAN_POINT('Ctrl Pts',(15.9486320401761,15.3517820863979,-8.90597167225456)) ;
#33716 = CARTESIAN_POINT('Ctrl Pts',(16.8466097990481,14.3706359252785,-8.93590006812211)) ;
#33717 = CARTESIAN_POINT('Ctrl Pts',(17.3382935025537,13.7734171618568,-8.95304416028605)) ;
#33718 = CARTESIAN_POINT('Ctrl Pts',(18.1297296635925,12.702395101905,-8.98267618853019)) ;
#33719 = CARTESIAN_POINT('Ctrl Pts',(18.4446078398806,12.2406851707781,-8.99513221240245)) ;
#33720 = CARTESIAN_POINT('Ctrl Pts',(18.9124885823397,11.4955120718219,-9.01509965227807)) ;
#33721 = CARTESIAN_POINT('Ctrl Pts',(19.0773561754003,11.2197816105119,-9.02247418162574)) ;
#33722 = CARTESIAN_POINT('Ctrl Pts',(19.6605606607886,10.1943666345315,-9.04978642258402)) ;
#33723 = CARTESIAN_POINT('Ctrl Pts',(20.0411805103896,9.42410957393968,-9.07001815227267)) ;
#33724 = CARTESIAN_POINT('Ctrl Pts',(20.6461747934665,7.99628283619559,-9.10624763174809)) ;
#33725 = CARTESIAN_POINT('Ctrl Pts',(20.8861999727258,7.34654581265738,-9.12229356527503)) ;
#33726 = CARTESIAN_POINT('Ctrl Pts',(21.2755160488762,6.11830756564737,-9.15176399458842)) ;
#33727 = CARTESIAN_POINT('Ctrl Pts',(21.4326174251605,5.54294038379523,-9.16523404087562)) ;
#33728 = CARTESIAN_POINT('Ctrl Pts',(21.7380275216957,4.21552056883294,-9.19575216608417)) ;
#33729 = CARTESIAN_POINT('Ctrl Pts',(21.8708940617532,3.46070025076321,-9.21269907513111)) ;
#33730 = CARTESIAN_POINT('Ctrl Pts',(22.0219047515762,2.23247017538734,-9.24029328718479)) ;
#33731 = CARTESIAN_POINT('Ctrl Pts',(22.0644751850135,1.76270861735612,-9.25085672297905)) ;
#33732 = CARTESIAN_POINT('Ctrl Pts',(22.1124378593305,0.942559353198248,-9.26956044830227)) ;
#33733 = CARTESIAN_POINT('Ctrl Pts',(22.124578721879,0.592737252509702,-9.27763261525578)) ;
#33734 = CARTESIAN_POINT('Ctrl Pts',(22.1339877264747,-0.264861580769144,
-9.29755690629313)) ;
#33735 = CARTESIAN_POINT('Ctrl Pts',(22.1220871878167,-0.772541899546286,
-9.309461732517)) ;
#33736 = CARTESIAN_POINT('Ctrl Pts',(22.0432003575448,-2.13480431721731,-9.34143750197635)) ;
#33737 = CARTESIAN_POINT('Ctrl Pts',(21.944019437397,-2.98665410439585,-9.36144274564382)) ;
#33738 = CARTESIAN_POINT('Ctrl Pts',(21.6994321916444,-4.37832621090559,-9.39389181081161)) ;
#33739 = CARTESIAN_POINT('Ctrl Pts',(21.5825580273603,-4.9222244130592,-9.40652189167091)) ;
#33740 = CARTESIAN_POINT('Ctrl Pts',(21.2532493491615,-6.21538375154405,-9.43655372852578)) ;
#33741 = CARTESIAN_POINT('Ctrl Pts',(21.0215226547319,-6.95896484435627,-9.45381421032134)) ;
#33742 = CARTESIAN_POINT('Ctrl Pts',(20.5568925925635,-8.2129445255478,-9.4835704752353)) ;
#33743 = CARTESIAN_POINT('Ctrl Pts',(20.3428919822577,-8.72954921137408,-9.4960336982369)) ;
#33744 = CARTESIAN_POINT('Ctrl Pts',(19.9753639382984,-9.5296395531761,-9.51601529924318)) ;
#33745 = CARTESIAN_POINT('Ctrl Pts',(19.8348154343114,-9.81882309668112,-9.52339648340031)) ;
#33746 = CARTESIAN_POINT('Ctrl Pts',(19.291104226313,-10.8781764230762,-9.5509664236352)) ;
#33747 = CARTESIAN_POINT('Ctrl Pts',(18.8489713727653,-11.6274547608296,-9.57145632400323)) ;
#33748 = CARTESIAN_POINT('Ctrl Pts',(17.9815001347149,-12.9174742628897,-9.6077676215876)) ;
#33749 = CARTESIAN_POINT('Ctrl Pts',(17.5728714777409,-13.4680989014952,-9.62364719604295)) ;
#33750 = CARTESIAN_POINT('Ctrl Pts',(16.7604564827969,-14.4627691304093,-9.65301671142507)) ;
#33751 = CARTESIAN_POINT('Ctrl Pts',(16.3628843516324,-14.9110903479753,-9.66654612743632)) ;
#33752 = CARTESIAN_POINT('Ctrl Pts',(15.4093292983237,-15.9022389385818,-9.69735510837264)) ;
#33753 = CARTESIAN_POINT('Ctrl Pts',(14.8419742276548,-16.4330286984593,-9.71452881803797)) ;
#33754 = CARTESIAN_POINT('Ctrl Pts',(13.9044494279254,-17.2218929280114,-9.74186159953693)) ;
#33755 = CARTESIAN_POINT('Ctrl Pts',(13.5522867834835,-17.5003665225471,-9.75192214371125)) ;
#33756 = CARTESIAN_POINT('Ctrl Pts',(12.9139521521488,-17.974301597064,-9.77001664921732)) ;
#33757 = CARTESIAN_POINT('Ctrl Pts',(12.6312011347797,-18.1741143073738,-9.77799751205913)) ;
#33758 = CARTESIAN_POINT('Ctrl Pts',(11.9327619114834,-18.6435079581784,-9.79754040273362)) ;
#33759 = CARTESIAN_POINT('Ctrl Pts',(11.5124812431647,-18.9059241931282,-9.8091521937653)) ;
#33760 = CARTESIAN_POINT('Ctrl Pts',(10.3207332205491,-19.59554660422,-9.84141870352719)) ;
#33761 = CARTESIAN_POINT('Ctrl Pts',(9.53200825225841,-19.9910935608971,-9.86200898195824)) ;
#33762 = CARTESIAN_POINT('Ctrl Pts',(8.23297262702736,-20.5481600776479,-9.89446345009149)) ;
#33763 = CARTESIAN_POINT('Ctrl Pts',(7.73675276523366,-20.740091202289,-9.906547564853)) ;
#33764 = CARTESIAN_POINT('Ctrl Pts',(6.15822503191993,-21.2861009289065,-9.94416301132018)) ;
#33765 = CARTESIAN_POINT('Ctrl Pts',(5.05524770027415,-21.5746674791876,-9.9691798774967)) ;
#33766 = CARTESIAN_POINT('Ctrl Pts',(3.58489124272495,-21.840351533277,-10.0027077280322)) ;
#33767 = CARTESIAN_POINT('Ctrl Pts',(3.23332624718334,-21.8951593151537,-10.010747562498)) ;
#33768 = CARTESIAN_POINT('Ctrl Pts',(2.69870303513949,-21.9653475116313,-10.0230997815463)) ;
#33769 = CARTESIAN_POINT('Ctrl Pts',(2.51652329890662,-21.9869643082306,-10.0273283249198)) ;
#33770 = CARTESIAN_POINT('Ctrl Pts',(1.55896316255078,-22.0885277856535,-10.0496218691874)) ;
#33771 = CARTESIAN_POINT('Ctrl Pts',(0.780029229939695,-22.1297305952072,
-10.0679688232123)) ;
#33772 = CARTESIAN_POINT('Ctrl Pts',(0.000550716358238557,-22.1297499931475,
-10.0862038529432)) ;
#33773 = CARTESIAN_POINT('Origin',(0.,0.,-10.)) ;
#33774 = CARTESIAN_POINT('',(-0.000186678706946326,-22.1297499992126,-13.7265753322825)) ;
#33775 = CARTESIAN_POINT('',(-0.000174491033434178,-22.1297499993121,-13.2609246410094)) ;
#33776 = CARTESIAN_POINT('',(-2.71011275034311E-15,-22.12975,-10.)) ;
#33777 = CARTESIAN_POINT('Ctrl Pts',(-0.000186678706946326,-22.1297499992126,
-13.7265753322825)) ;
#33778 = CARTESIAN_POINT('Ctrl Pts',(0.443811682544672,-22.129753744625,-13.7164336904268)) ;
#33779 = CARTESIAN_POINT('Ctrl Pts',(0.887869351187652,-22.1163909616294,
-13.706292048571)) ;
#33780 = CARTESIAN_POINT('Ctrl Pts',(1.33116660457718,-22.08967701288,-13.6961504067153)) ;
#33781 = CARTESIAN_POINT('Ctrl Pts',(1.77439794946708,-22.0629670359041,-13.6860102726974)) ;
#33782 = CARTESIAN_POINT('Ctrl Pts',(2.21686887397983,-22.0229098716419,-13.6758701386796)) ;
#33783 = CARTESIAN_POINT('Ctrl Pts',(2.65776220351048,-21.9695729392287,-13.6657300046617)) ;
#33784 = CARTESIAN_POINT('Ctrl Pts',(3.09861081635288,-21.9162414164029,-13.6555908990858)) ;
#33785 = CARTESIAN_POINT('Ctrl Pts',(3.53788192410997,-21.8496328434984,-13.64545179351)) ;
#33786 = CARTESIAN_POINT('Ctrl Pts',(3.97476424351366,-21.7698664274953,-13.6353126879341)) ;
#33787 = CARTESIAN_POINT('Ctrl Pts',(4.41162289108153,-21.6901043335198,-13.625174131731)) ;
#33788 = CARTESIAN_POINT('Ctrl Pts',(4.84609278126068,-21.5971858623802,-13.6150355755279)) ;
#33789 = CARTESIAN_POINT('Ctrl Pts',(5.27737184086928,-21.4912815233457,-13.6048970193247)) ;
#33790 = CARTESIAN_POINT('Ctrl Pts',(5.70869218708943,-21.3853670460232,-13.5947574925514)) ;
#33791 = CARTESIAN_POINT('Ctrl Pts',(6.13682086686759,-21.266464269091,-13.584617965778)) ;
#33792 = CARTESIAN_POINT('Ctrl Pts',(6.56096805462135,-21.1347943744134,-13.5744784390046)) ;
#33793 = CARTESIAN_POINT('Ctrl Pts',(6.98512129467272,-21.0031226008943,-13.5643387675469)) ;
#33794 = CARTESIAN_POINT('Ctrl Pts',(7.40529270873749,-20.8586834162419,-13.5541990960893)) ;
#33795 = CARTESIAN_POINT('Ctrl Pts',(7.82070825561196,-20.7017476905478,-13.5440594246316)) ;
#33796 = CARTESIAN_POINT('Ctrl Pts',(8.23620925994095,-20.5447796807283,-13.5339176672854)) ;
#33797 = CARTESIAN_POINT('Ctrl Pts',(8.64695222465578,-20.3753100725641,-13.5237759099392)) ;
#33798 = CARTESIAN_POINT('Ctrl Pts',(9.05218172659114,-20.1936584365308,-13.5136341525931)) ;
#33799 = CARTESIAN_POINT('Ctrl Pts',(9.3824336728765,-20.045616879686,-13.5053688730753)) ;
#33800 = CARTESIAN_POINT('Ctrl Pts',(9.70902397047871,-19.8894851375713,-13.4971035935576)) ;
#33801 = CARTESIAN_POINT('Ctrl Pts',(10.0315545694457,-19.7254593858478,-13.4888383140399)) ;
#33802 = CARTESIAN_POINT('Ctrl Pts',(10.4387353476837,-19.5183840464794,-13.478403760056)) ;
#33803 = CARTESIAN_POINT('Ctrl Pts',(10.839554832239,-19.2986698255881,-13.467969206072)) ;
#33804 = CARTESIAN_POINT('Ctrl Pts',(11.2332271499225,-19.0667365550779,-13.4575346520881)) ;
#33805 = CARTESIAN_POINT('Ctrl Pts',(11.6165832589122,-18.840881111009,-13.4473735362702)) ;
#33806 = CARTESIAN_POINT('Ctrl Pts',(11.9931617844149,-18.6034389500622,-13.4372124204522)) ;
#33807 = CARTESIAN_POINT('Ctrl Pts',(12.3622630052698,-18.3548437326782,-13.4270513046342)) ;
#33808 = CARTESIAN_POINT('Ctrl Pts',(12.7313262730158,-18.1062740772833,-13.4168912336406)) ;
#33809 = CARTESIAN_POINT('Ctrl Pts',(13.0929135815744,-17.8465537843947,-13.4067311626469)) ;
#33810 = CARTESIAN_POINT('Ctrl Pts',(13.4463540225345,-17.5761599492941,-13.3965710916533)) ;
#33811 = CARTESIAN_POINT('Ctrl Pts',(13.7997733772339,-17.3057822458928,-13.3864116268096)) ;
#33812 = CARTESIAN_POINT('Ctrl Pts',(14.1450466531115,-17.0247324119128,-13.3762521619659)) ;
#33813 = CARTESIAN_POINT('Ctrl Pts',(14.4815344736949,-16.7335290464888,-13.3660926971222)) ;
#33814 = CARTESIAN_POINT('Ctrl Pts',(14.8339480721597,-16.4285431907863,-13.3554523905642)) ;
#33815 = CARTESIAN_POINT('Ctrl Pts',(15.17672440761,-16.1124197650166,-13.3448120840061)) ;
#33816 = CARTESIAN_POINT('Ctrl Pts',(15.5091690889543,-15.785800873973,-13.3341717774481)) ;
#33817 = CARTESIAN_POINT('Ctrl Pts',(15.8266211638622,-15.4739118575909,-13.3240113279537)) ;
#33818 = CARTESIAN_POINT('Ctrl Pts',(16.1346525681014,-15.1524531520895,-13.3138508784592)) ;
#33819 = CARTESIAN_POINT('Ctrl Pts',(16.432696261367,-14.8220217461774,-13.3036904289648)) ;
#33820 = CARTESIAN_POINT('Ctrl Pts',(16.7307532993377,-14.4915755454221,-13.2935295245431)) ;
#33821 = CARTESIAN_POINT('Ctrl Pts',(17.0188215808823,-14.1521560135859,-13.2833686201214)) ;
#33822 = CARTESIAN_POINT('Ctrl Pts',(17.2963730898947,-13.8043946987062,-13.2732077156997)) ;
#33823 = CARTESIAN_POINT('Ctrl Pts',(17.5739707213121,-13.4565755942353,-13.2630451227793)) ;
#33824 = CARTESIAN_POINT('Ctrl Pts',(17.8410479450515,-13.100412116321,-13.2528825298589)) ;
#33825 = CARTESIAN_POINT('Ctrl Pts',(18.0971177761887,-12.7365679544081,-13.2427199369386)) ;
#33826 = CARTESIAN_POINT('Ctrl Pts',(18.1333256017635,-12.6851210272459,-13.2412829641011)) ;
#33827 = CARTESIAN_POINT('Ctrl Pts',(18.1693134208187,-12.6335205858924,-13.2398459912636)) ;
#33828 = CARTESIAN_POINT('Ctrl Pts',(18.2050799256723,-12.5817685546342,-13.2384090184261)) ;
#33829 = CARTESIAN_POINT('Ctrl Pts',(18.4647977964425,-12.2059720539304,-13.2279744644421)) ;
#33830 = CARTESIAN_POINT('Ctrl Pts',(18.7129092937484,-11.822082378419,-13.2175399104582)) ;
#33831 = CARTESIAN_POINT('Ctrl Pts',(18.9489227444543,-11.4308425711844,-13.2071053564743)) ;
#33832 = CARTESIAN_POINT('Ctrl Pts',(19.1787514472871,-11.0498552286227,-13.1969442406583)) ;
#33833 = CARTESIAN_POINT('Ctrl Pts',(19.39710792746,-10.6618982552937,-13.1867831248423)) ;
#33834 = CARTESIAN_POINT('Ctrl Pts',(19.6035828749807,-10.2676858895402,-13.1766220090263)) ;
#33835 = CARTESIAN_POINT('Ctrl Pts',(19.8100365915602,-9.87351405896871,-13.1664619380346)) ;
#33836 = CARTESIAN_POINT('Ctrl Pts',(20.0046111094016,-9.47308832405769,-13.1563018670429)) ;
#33837 = CARTESIAN_POINT('Ctrl Pts',(20.1869431201869,-9.06714743041258,-13.1461417960513)) ;
#33838 = CARTESIAN_POINT('Ctrl Pts',(20.3692642530432,-8.66123075520413,-13.1359823312095)) ;
#33839 = CARTESIAN_POINT('Ctrl Pts',(20.5393442440229,-8.24979978795752,-13.1258228663677)) ;
#33840 = CARTESIAN_POINT('Ctrl Pts',(20.6968672602428,-7.83361478976272,-13.115663401526)) ;
#33841 = CARTESIAN_POINT('Ctrl Pts',(20.8618457516162,-7.39773199128597,-13.1050230949665)) ;
#33842 = CARTESIAN_POINT('Ctrl Pts',(21.0130499833048,-6.95663459065067,-13.094382788407)) ;
#33843 = CARTESIAN_POINT('Ctrl Pts',(21.150174459723,-6.51121765768752,-13.0837424818475)) ;
#33844 = CARTESIAN_POINT('Ctrl Pts',(21.2811148897792,-6.08588815940987,-13.073582032355)) ;
#33845 = CARTESIAN_POINT('Ctrl Pts',(21.3992171990292,-5.65662030618157,-13.0634215828626)) ;
#33846 = CARTESIAN_POINT('Ctrl Pts',(21.5042664660398,-5.22420891810953,-13.0532611333701)) ;
#33847 = CARTESIAN_POINT('Ctrl Pts',(21.6093204365609,-4.79177816910761,-13.0431002289503)) ;
#33848 = CARTESIAN_POINT('Ctrl Pts',(21.7013201452544,-4.3562038276328,-13.0329393245305)) ;
#33849 = CARTESIAN_POINT('Ctrl Pts',(21.7801014345156,-3.91829255731518,-13.0227784201107)) ;
#33850 = CARTESIAN_POINT('Ctrl Pts',(21.8588958153373,-3.48030851664874,-13.0126158271923)) ;
#33851 = CARTESIAN_POINT('Ctrl Pts',(21.9244673470658,-3.03998699708508,-13.002453234274)) ;
#33852 = CARTESIAN_POINT('Ctrl Pts',(21.9767032516041,-2.59814342433856,-12.9922906413556)) ;
#33853 = CARTESIAN_POINT('Ctrl Pts',(21.9840893170606,-2.53566751665238,-12.9908536685078)) ;
#33854 = CARTESIAN_POINT('Ctrl Pts',(21.9912088416097,-2.47316118821051,-12.98941669566)) ;
#33855 = CARTESIAN_POINT('Ctrl Pts',(21.9980615899916,-2.41062675365442,-12.9879797228121)) ;
#33856 = CARTESIAN_POINT('Ctrl Pts',(22.047822706242,-1.95653401681598,-12.9775451688282)) ;
#33857 = CARTESIAN_POINT('Ctrl Pts',(22.0835251186466,-1.50084120821694,-12.9671106148443)) ;
#33858 = CARTESIAN_POINT('Ctrl Pts',(22.1050896615229,-1.04443578957034,-12.9566760608604)) ;
#33859 = CARTESIAN_POINT('Ctrl Pts',(22.1260891041486,-0.599990504643697,
-12.9465149450432)) ;
#33860 = CARTESIAN_POINT('Ctrl Pts',(22.1336821546946,-0.154869721914559,
-12.936353829226)) ;
#33861 = CARTESIAN_POINT('Ctrl Pts',(22.1278484033474,0.290103603867267,-12.9261927134089)) ;
#33862 = CARTESIAN_POINT('Ctrl Pts',(22.12201525186,0.735031174931935,-12.9160326424161)) ;
#33863 = CARTESIAN_POINT('Ctrl Pts',(22.1027580592561,1.17981108988913,-12.9058725714232)) ;
#33864 = CARTESIAN_POINT('Ctrl Pts',(22.0701085373036,1.62362071129283,-12.8957125004304)) ;
#33865 = CARTESIAN_POINT('Ctrl Pts',(22.0374609632219,2.06740385501081,-12.8855530355876)) ;
#33866 = CARTESIAN_POINT('Ctrl Pts',(21.9914226728818,2.51021659196284,-12.8753935707447)) ;
#33867 = CARTESIAN_POINT('Ctrl Pts',(21.9320773733454,2.95123993468679,-12.8652341059018)) ;
#33868 = CARTESIAN_POINT('Ctrl Pts',(21.8699232944008,3.41313666238461,-12.8545937993432)) ;
#33869 = CARTESIAN_POINT('Ctrl Pts',(21.7931723497383,3.8730702760558,-12.8439534927845)) ;
#33870 = CARTESIAN_POINT('Ctrl Pts',(21.7019814482537,4.33010811437246,-12.8333131862259)) ;
#33871 = CARTESIAN_POINT('Ctrl Pts',(21.6149030784992,4.76653443792858,-12.8231527367323)) ;
#33872 = CARTESIAN_POINT('Ctrl Pts',(21.5146582727688,5.20032012721874,-12.8129922872387)) ;
#33873 = CARTESIAN_POINT('Ctrl Pts',(21.4014359433373,5.63066378198242,-12.8028318377451)) ;
#33874 = CARTESIAN_POINT('Ctrl Pts',(21.2882085444514,6.06102670509671,-12.7926709333241)) ;
#33875 = CARTESIAN_POINT('Ctrl Pts',(21.1620025216004,6.48794706440571,-12.7825100289031)) ;
#33876 = CARTESIAN_POINT('Ctrl Pts',(21.0230570756204,6.91063718174438,-12.7723491244821)) ;
#33877 = CARTESIAN_POINT('Ctrl Pts',(20.8840885402411,7.33339754003844,-12.7621865315627)) ;
#33878 = CARTESIAN_POINT('Ctrl Pts',(20.732376423431,7.75192603371615,-12.7520239386432)) ;
#33879 = CARTESIAN_POINT('Ctrl Pts',(20.5682092908173,8.16545171020179,-12.7418613457237)) ;
#33880 = CARTESIAN_POINT('Ctrl Pts',(20.5449963457602,8.22392351667803,-12.7404243728819)) ;
#33881 = CARTESIAN_POINT('Ctrl Pts',(20.5215344610334,8.28229533056822,-12.7389874000401)) ;
#33882 = CARTESIAN_POINT('Ctrl Pts',(20.4978245304077,8.3405650038301,-12.7375504271984)) ;
#33883 = CARTESIAN_POINT('Ctrl Pts',(20.3256552702268,8.76368925058057,-12.7271158732144)) ;
#33884 = CARTESIAN_POINT('Ctrl Pts',(20.1403578099894,9.18153545349456,-12.7166813192305)) ;
#33885 = CARTESIAN_POINT('Ctrl Pts',(19.9422845404748,9.59328527508905,-12.7062467652466)) ;
#33886 = CARTESIAN_POINT('Ctrl Pts',(19.7494017938981,9.9942451657711,-12.69608564943)) ;
#33887 = CARTESIAN_POINT('Ctrl Pts',(19.5444043594006,10.3894238816228,-12.6859245336133)) ;
#33888 = CARTESIAN_POINT('Ctrl Pts',(19.3276656383988,10.7780877725485,-12.6757634177967)) ;
#33889 = CARTESIAN_POINT('Ctrl Pts',(19.1109492037187,11.1667116988178,-12.6656033468044)) ;
#33890 = CARTESIAN_POINT('Ctrl Pts',(18.8824940058694,11.548821937848,-12.6554432758121)) ;
#33891 = CARTESIAN_POINT('Ctrl Pts',(18.6427191461546,11.9237099050632,-12.6452832048198)) ;
#33892 = CARTESIAN_POINT('Ctrl Pts',(18.402958591408,12.2985755064621,-12.6351237399774)) ;
#33893 = CARTESIAN_POINT('Ctrl Pts',(18.1518798476512,12.6662195035583,-12.6249642751349)) ;
#33894 = CARTESIAN_POINT('Ctrl Pts',(17.8899460201268,13.0259612489617,-12.6148048102925)) ;
#33895 = CARTESIAN_POINT('Ctrl Pts',(17.6156150129077,13.4027293674133,-12.6041645037335)) ;
#33896 = CARTESIAN_POINT('Ctrl Pts',(17.3293768617193,13.7708290241797,-12.5935241971745)) ;
#33897 = CARTESIAN_POINT('Ctrl Pts',(17.0318131241977,14.129514385318,-12.5828838906155)) ;
#33898 = CARTESIAN_POINT('Ctrl Pts',(16.7476689306716,14.4720237364879,-12.5727234411223)) ;
#33899 = CARTESIAN_POINT('Ctrl Pts',(16.4531981208485,14.8059488590116,-12.5625629916292)) ;
#33900 = CARTESIAN_POINT('Ctrl Pts',(16.1489479842514,15.1306746070505,-12.5524025421361)) ;
#33901 = CARTESIAN_POINT('Ctrl Pts',(15.8446842250619,15.4554148944634,-12.5422416377157)) ;
#33902 = CARTESIAN_POINT('Ctrl Pts',(15.5306404229071,15.7709548185611,-12.5320807332954)) ;
#33903 = CARTESIAN_POINT('Ctrl Pts',(15.2074015800676,16.0767152193804,-12.5219198288751)) ;
#33904 = CARTESIAN_POINT('Ctrl Pts',(14.8841090226808,16.382526430249,-12.511757235956)) ;
#33905 = CARTESIAN_POINT('Ctrl Pts',(14.5516185382453,16.6785547129367,-12.5015946430369)) ;
#33906 = CARTESIAN_POINT('Ctrl Pts',(14.2105506008589,16.9642590961977,-12.4914320501178)) ;
#33907 = CARTESIAN_POINT('Ctrl Pts',(14.1623241917089,17.0046571957339,-12.4899950772734)) ;
#33908 = CARTESIAN_POINT('Ctrl Pts',(14.1139263444979,17.0448489497629,-12.4885581044289)) ;
#33909 = CARTESIAN_POINT('Ctrl Pts',(14.0653588669669,17.0848328937082,-12.4871211315845)) ;
#33910 = CARTESIAN_POINT('Ctrl Pts',(13.7126869510626,17.3751756257886,-12.4766865776005)) ;
#33911 = CARTESIAN_POINT('Ctrl Pts',(13.3509762733302,17.6546322121746,-12.4662520236166)) ;
#33912 = CARTESIAN_POINT('Ctrl Pts',(12.9809259880184,17.9226503496578,-12.4558174696327)) ;
#33913 = CARTESIAN_POINT('Ctrl Pts',(12.6205728945467,18.1836450543834,-12.4456563538159)) ;
#33914 = CARTESIAN_POINT('Ctrl Pts',(12.2523118783805,18.4337929897971,-12.4354952379991)) ;
#33915 = CARTESIAN_POINT('Ctrl Pts',(11.8768203035513,18.6726263428488,-12.4253341221823)) ;
#33916 = CARTESIAN_POINT('Ctrl Pts',(11.5013673389252,18.9114351376817,-12.4151740511898)) ;
#33917 = CARTESIAN_POINT('Ctrl Pts',(11.1186854943598,19.1389315509339,-12.4050139801974)) ;
#33918 = CARTESIAN_POINT('Ctrl Pts',(10.7294804156782,19.3546915519746,-12.3948539092049)) ;
#33919 = CARTESIAN_POINT('Ctrl Pts',(10.3402985569723,19.5704386807733,-12.3846944443623)) ;
#33920 = CARTESIAN_POINT('Ctrl Pts',(9.94459444236979,19.7744506849794,-12.3745349795197)) ;
#33921 = CARTESIAN_POINT('Ctrl Pts',(9.54309914195966,19.9663490360463,-12.3643755146771)) ;
#33922 = CARTESIAN_POINT('Ctrl Pts',(9.12260129640409,20.1673298273704,-12.3537352081183)) ;
#33923 = CARTESIAN_POINT('Ctrl Pts',(8.69575115004648,20.3550226323908,-12.3430949015594)) ;
#33924 = CARTESIAN_POINT('Ctrl Pts',(8.26341497367153,20.529047908644,-12.3324545950005)) ;
#33925 = CARTESIAN_POINT('Ctrl Pts',(7.85057631532528,20.6952249844768,-12.3222941455073)) ;
#33926 = CARTESIAN_POINT('Ctrl Pts',(7.43273567196483,20.8489397919958,-12.312133696014)) ;
#33927 = CARTESIAN_POINT('Ctrl Pts',(7.01066702043379,20.9899114574384,-12.3019732465208)) ;
#33928 = CARTESIAN_POINT('Ctrl Pts',(6.58857947106427,21.1308894347919,-12.2918123421003)) ;
#33929 = CARTESIAN_POINT('Ctrl Pts',(6.16226375373612,21.2591230596214,-12.2816514376798)) ;
#33930 = CARTESIAN_POINT('Ctrl Pts',(5.73250990772562,21.374381048824,-12.2714905332593)) ;
#33931 = CARTESIAN_POINT('Ctrl Pts',(5.30268464692803,21.4896581911415,-12.2613279403401)) ;
#33932 = CARTESIAN_POINT('Ctrl Pts',(4.86942033754504,21.5919553299681,-12.2511653474208)) ;
#33933 = CARTESIAN_POINT('Ctrl Pts',(4.43352006239451,21.681091644999,-12.2410027545016)) ;
#33934 = CARTESIAN_POINT('Ctrl Pts',(4.37188452676789,21.6936953638629,-12.239565781658)) ;
#33935 = CARTESIAN_POINT('Ctrl Pts',(4.3101963064683,21.7060360355789,-12.2381288088143)) ;
#33936 = CARTESIAN_POINT('Ctrl Pts',(4.2484576882242,21.7181132314451,-12.2366918359707)) ;
#33937 = CARTESIAN_POINT('Ctrl Pts',(3.80014375674978,21.8058115848247,-12.2262572819867)) ;
#33938 = CARTESIAN_POINT('Ctrl Pts',(3.349055427096,21.8796351373696,-12.2158227280028)) ;
#33939 = CARTESIAN_POINT('Ctrl Pts',(2.89607038505077,21.9394305164772,-12.2053881740189)) ;
#33940 = CARTESIAN_POINT('Ctrl Pts',(2.45495584555064,21.9976589537788,-12.1952270582021)) ;
#33941 = CARTESIAN_POINT('Ctrl Pts',(2.01204296917008,22.0425849991785,-12.1850659423853)) ;
#33942 = CARTESIAN_POINT('Ctrl Pts',(1.568150093832,22.0741192428082,-12.1749048265685)) ;
#33943 = CARTESIAN_POINT('Ctrl Pts',(1.12430286211199,22.1056502439056,-12.1647447555761)) ;
#33944 = CARTESIAN_POINT('Ctrl Pts',(0.679476061608808,22.1237921775522,-12.1545846845836)) ;
#33945 = CARTESIAN_POINT('Ctrl Pts',(0.234492088719243,22.1285075981827,-12.1444246135912)) ;
#33946 = CARTESIAN_POINT('Ctrl Pts',(-0.210465336426893,22.1332227374911,
-12.1342651487485)) ;
#33947 = CARTESIAN_POINT('Ctrl Pts',(-0.65557968575692,22.1245129616793,-12.1241056839059)) ;
#33948 = CARTESIAN_POINT('Ctrl Pts',(-1.10002783592053,22.1023929433602,-12.1139462190633)) ;
#33949 = CARTESIAN_POINT('Ctrl Pts',(-1.56551146527747,22.0792259971038,-12.1033059125044)) ;
#33950 = CARTESIAN_POINT('Ctrl Pts',(-2.03026404861439,22.0413489224589,-12.0926656059455)) ;
#33951 = CARTESIAN_POINT('Ctrl Pts',(-2.49334304585184,21.9888397947277,-12.0820252993867)) ;
#33952 = CARTESIAN_POINT('Ctrl Pts',(-2.93553808382328,21.9386987262071,-12.0718648498934)) ;
#33953 = CARTESIAN_POINT('Ctrl Pts',(-3.37620688762659,21.8752160462819,-12.0617044004001)) ;
#33954 = CARTESIAN_POINT('Ctrl Pts',(-3.81453502899431,21.7985127376864,-12.0515439509068)) ;
#33955 = CARTESIAN_POINT('Ctrl Pts',(-4.25288279619944,21.7218059947537,-12.0413830464865)) ;
#33956 = CARTESIAN_POINT('Ctrl Pts',(-4.68888946590498,21.6318774823466,-12.0312221420661)) ;
#33957 = CARTESIAN_POINT('Ctrl Pts',(-5.12175006271124,21.5288994460381,-12.0210612376458)) ;
#33958 = CARTESIAN_POINT('Ctrl Pts',(-5.55468259057673,21.4259042972473,-12.0108986447266)) ;
#33959 = CARTESIAN_POINT('Ctrl Pts',(-5.98446777763594,21.3098553447335,-12.0007360518074)) ;
#33960 = CARTESIAN_POINT('Ctrl Pts',(-6.41031317178666,21.1809754284858,-11.9905734588883)) ;
#33961 = CARTESIAN_POINT('Ctrl Pts',(-6.47052696485443,21.1627520340001,-11.9891364860444)) ;
#33962 = CARTESIAN_POINT('Ctrl Pts',(-6.53066201211327,21.1442721856697,-11.9876995132006)) ;
#33963 = CARTESIAN_POINT('Ctrl Pts',(-6.5907160980845,21.1255365938229,-11.9862625403567)) ;
#33964 = CARTESIAN_POINT('Ctrl Pts',(-7.02679782691396,20.9894884107383,-11.9758279863728)) ;
#33965 = CARTESIAN_POINT('Ctrl Pts',(-7.45872200889061,20.839915354729,-11.9653934323889)) ;
#33966 = CARTESIAN_POINT('Ctrl Pts',(-7.88564361724271,20.677099888629,-11.954958878405)) ;
#33967 = CARTESIAN_POINT('Ctrl Pts',(-8.30137771702621,20.5185510124284,-11.9447977625883)) ;
#33968 = CARTESIAN_POINT('Ctrl Pts',(-8.71236784836556,20.3474449705746,-11.9346366467715)) ;
#33969 = CARTESIAN_POINT('Ctrl Pts',(-9.11785160959659,20.1640922703671,-11.9244755309547)) ;
#33970 = CARTESIAN_POINT('Ctrl Pts',(-9.52329367665906,19.980758423537,-11.9143154599623)) ;
#33971 = CARTESIAN_POINT('Ctrl Pts',(-9.92323029549759,19.7851805282727,-11.9041553889698)) ;
#33972 = CARTESIAN_POINT('Ctrl Pts',(-10.3169202058506,19.5777167343031,-11.8939953179773)) ;
#33973 = CARTESIAN_POINT('Ctrl Pts',(-10.7105866286583,19.3702653176263,-11.8838358531348)) ;
#33974 = CARTESIAN_POINT('Ctrl Pts',(-11.0980068845182,19.1509295259284,-11.8736763882923)) ;
#33975 = CARTESIAN_POINT('Ctrl Pts',(-11.4784638584483,18.9201137024278,-11.8635169234497)) ;
#33976 = CARTESIAN_POINT('Ctrl Pts',(-11.8769276454528,18.6783734967416,-11.8528766168909)) ;
#33977 = CARTESIAN_POINT('Ctrl Pts',(-12.2677529454088,18.4240406018629,-11.842236310332)) ;
#33978 = CARTESIAN_POINT('Ctrl Pts',(-12.6501477448703,18.15763192422,-11.8315960037731)) ;
#33979 = CARTESIAN_POINT('Ctrl Pts',(-13.0152972849629,17.9032377581514,-11.8214355542798)) ;
#33980 = CARTESIAN_POINT('Ctrl Pts',(-13.3727596173026,17.637832923503,-11.8112751047865)) ;
#33981 = CARTESIAN_POINT('Ctrl Pts',(-13.7218758315993,17.3619111483924,-11.8011146552932)) ;
#33982 = CARTESIAN_POINT('Ctrl Pts',(-14.0710076773342,17.0859770190742,-11.7909537508728)) ;
#33983 = CARTESIAN_POINT('Ctrl Pts',(-14.4117924797961,16.7995251526353,-11.7807928464523)) ;
#33984 = CARTESIAN_POINT('Ctrl Pts',(-14.7436040222943,16.5030898772408,-11.7706319420319)) ;
#33985 = CARTESIAN_POINT('Ctrl Pts',(-15.075470703917,16.2066053414094,-11.7604693491127)) ;
#33986 = CARTESIAN_POINT('Ctrl Pts',(-15.3983609749454,15.9001342346632,-11.7503067561935)) ;
#33987 = CARTESIAN_POINT('Ctrl Pts',(-15.7116836954442,15.5842494370699,-11.7401441632744)) ;
#33988 = CARTESIAN_POINT('Ctrl Pts',(-15.7559869794864,15.5395838798128,-11.7387071904306)) ;
#33989 = CARTESIAN_POINT('Ctrl Pts',(-15.800099035216,15.4947301704647,-11.7372702175868)) ;
#33990 = CARTESIAN_POINT('Ctrl Pts',(-15.844018251497,15.4496899874635,-11.735833244743)) ;
#33991 = CARTESIAN_POINT('Ctrl Pts',(-16.1629368971697,15.1226314609247,-11.725398690759)) ;
#33992 = CARTESIAN_POINT('Ctrl Pts',(-16.4717664484133,14.7856523720499,-11.7149641367751)) ;
#33993 = CARTESIAN_POINT('Ctrl Pts',(-16.7698978695481,14.4394030523228,-11.7045295827912)) ;
#33994 = CARTESIAN_POINT('Ctrl Pts',(-17.0602167373648,14.1022272185817,-11.6943684669744)) ;
#33995 = CARTESIAN_POINT('Ctrl Pts',(-17.3403908348353,13.7562609764049,-11.6842073511576)) ;
#33996 = CARTESIAN_POINT('Ctrl Pts',(-17.609897147207,13.402140035356,-11.6740462353408)) ;
#33997 = CARTESIAN_POINT('Ctrl Pts',(-17.8793757473911,13.0480555070571,-11.6638861643483)) ;
#33998 = CARTESIAN_POINT('Ctrl Pts',(-18.138188614594,12.685818137402,-11.6537260933558)) ;
#33999 = CARTESIAN_POINT('Ctrl Pts',(-18.3858539882545,12.3160954926911,-11.6435660223633)) ;
#34000 = CARTESIAN_POINT('Ctrl Pts',(-18.6335045861991,11.9463949056329,-11.6334065575206)) ;
#34001 = CARTESIAN_POINT('Ctrl Pts',(-18.8700088915731,11.569210126359,-11.6232470926779)) ;
#34002 = CARTESIAN_POINT('Ctrl Pts',(-19.0949283514416,11.1852378747979,-11.6130876278352)) ;
#34003 = CARTESIAN_POINT('Ctrl Pts',(-19.3304931219399,10.7830924340715,-11.6024473212764)) ;
#34004 = CARTESIAN_POINT('Ctrl Pts',(-19.5533499527906,10.3735018220648,-11.5918070147175)) ;
#34005 = CARTESIAN_POINT('Ctrl Pts',(-19.7630479330817,9.95729739724672,-11.5811667081587)) ;
#34006 = CARTESIAN_POINT('Ctrl Pts',(-19.9632889436028,9.55986297993257,-11.5710062586654)) ;
#34007 = CARTESIAN_POINT('Ctrl Pts',(-20.1515314844915,9.15639824653307,-11.560845809172)) ;
#34008 = CARTESIAN_POINT('Ctrl Pts',(-20.3274307117808,8.74765086867624,-11.5506853596787)) ;
#34009 = CARTESIAN_POINT('Ctrl Pts',(-20.5033378148358,8.33888518943948,-11.5405244552583)) ;
#34010 = CARTESIAN_POINT('Ctrl Pts',(-20.6669004115264,7.9248366049264,-11.530363550838)) ;
#34011 = CARTESIAN_POINT('Ctrl Pts',(-20.8178217254164,7.50627295475458,-11.5202026464176)) ;
#34012 = CARTESIAN_POINT('Ctrl Pts',(-20.9687681188101,7.08763974934033,-11.5100400534985)) ;
#34013 = CARTESIAN_POINT('Ctrl Pts',(-21.1070689541603,6.66449019500752,-11.4998774605794)) ;
#34014 = CARTESIAN_POINT('Ctrl Pts',(-21.2324766450028,6.23760936432466,-11.4897148676604)) ;
#34015 = CARTESIAN_POINT('Ctrl Pts',(-21.2502090728956,6.17724916234625,-11.4882778948166)) ;
#34016 = CARTESIAN_POINT('Ctrl Pts',(-21.267683803721,6.11681438357297,-11.4868409219728)) ;
#34017 = CARTESIAN_POINT('Ctrl Pts',(-21.2849002183608,6.05630727068284,-11.4854039491291)) ;
#34018 = CARTESIAN_POINT('Ctrl Pts',(-21.4099169218747,5.61693589453045,-11.4749693951451)) ;
#34019 = CARTESIAN_POINT('Ctrl Pts',(-21.5213406419892,5.17363537269906,-11.4645348411612)) ;
#34020 = CARTESIAN_POINT('Ctrl Pts',(-21.618944881532,4.72726742122561,-11.4541002871773)) ;
#34021 = CARTESIAN_POINT('Ctrl Pts',(-21.7139913956172,4.29259657100826,-11.4439391713605)) ;
#34022 = CARTESIAN_POINT('Ctrl Pts',(-21.7959333929137,3.85501723569015,-11.4337780555437)) ;
#34023 = CARTESIAN_POINT('Ctrl Pts',(-21.8646130944639,3.41533736135931,-11.423616939727)) ;
#34024 = CARTESIAN_POINT('Ctrl Pts',(-21.9332857339723,2.97570269744167,-11.4134568687345)) ;
#34025 = CARTESIAN_POINT('Ctrl Pts',(-21.9886987663005,2.53396815266412,-11.4032967977421)) ;
#34026 = CARTESIAN_POINT('Ctrl Pts',(-22.0307458528026,2.09095007872548,-11.3931367267497)) ;
#34027 = CARTESIAN_POINT('Ctrl Pts',(-22.0727904307749,1.64795843525155,-11.3829772619072)) ;
#34028 = CARTESIAN_POINT('Ctrl Pts',(-22.1014706343473,1.20368364405753,-11.3728177970648)) ;
#34029 = CARTESIAN_POINT('Ctrl Pts',(-22.1167319981389,0.758947155603138,
-11.3626583322224)) ;
#34030 = CARTESIAN_POINT('Ctrl Pts',(-22.1327156736345,0.293161541057203,
-11.3520180256634)) ;
#34031 = CARTESIAN_POINT('Ctrl Pts',(-22.1339797673999,-0.17313025446473,
-11.3413777191045)) ;
#34032 = CARTESIAN_POINT('Ctrl Pts',(-22.1205229701666,-0.638982463634,-11.3307374125456)) ;
#34033 = CARTESIAN_POINT('Ctrl Pts',(-22.1076730482332,-1.08382564708693,
-11.3205769630523)) ;
#34034 = CARTESIAN_POINT('Ctrl Pts',(-22.0814004911738,-1.52826776709898,
-11.3104165135591)) ;
#34035 = CARTESIAN_POINT('Ctrl Pts',(-22.041757498408,-1.97148711481321,-11.3002560640658)) ;
#34036 = CARTESIAN_POINT('Ctrl Pts',(-22.0021127306535,-2.41472630738025,
-11.2900951596452)) ;
#34037 = CARTESIAN_POINT('Ctrl Pts',(-21.9490963538971,-2.85674238987022,
-11.2799342552245)) ;
#34038 = CARTESIAN_POINT('Ctrl Pts',(-21.8828124429122,-3.2967187703575,-11.2697733508038)) ;
#34039 = CARTESIAN_POINT('Ctrl Pts',(-21.8165175171327,-3.73676826435554,
-11.2596107578848)) ;
#34040 = CARTESIAN_POINT('Ctrl Pts',(-21.7369506859879,-4.17477715213099,
-11.2494481649658)) ;
#34041 = CARTESIAN_POINT('Ctrl Pts',(-21.6442674912479,-4.60993707438697,
-11.2392855720468)) ;
#34042 = CARTESIAN_POINT('Ctrl Pts',(-21.6311622498018,-4.67146792542045,
-11.2378485992029)) ;
#34043 = CARTESIAN_POINT('Ctrl Pts',(-21.6177948501307,-4.73294183313134,
-11.2364116263591)) ;
#34044 = CARTESIAN_POINT('Ctrl Pts',(-21.6041658141075,-4.79435653023914,
-11.2349746535153)) ;
#34045 = CARTESIAN_POINT('Ctrl Pts',(-21.5051987997055,-5.24031831380347,
-11.2245400995313)) ;
#34046 = CARTESIAN_POINT('Ctrl Pts',(-21.3924056844949,-5.68327238729325,
-11.2141055455474)) ;
#34047 = CARTESIAN_POINT('Ctrl Pts',(-21.2659970100249,-6.12235299799939,
-11.2036709915635)) ;
#34048 = CARTESIAN_POINT('Ctrl Pts',(-21.1429008831067,-6.54992747268951,
-11.1935098757467)) ;
#34049 = CARTESIAN_POINT('Ctrl Pts',(-21.0068937286801,-6.97382866349173,
-11.1833487599299)) ;
#34050 = CARTESIAN_POINT('Ctrl Pts',(-20.8582209686787,-7.39327079743941,
-11.1731876441131)) ;
#34051 = CARTESIAN_POINT('Ctrl Pts',(-20.7095634960657,-7.81266980193434,
-11.1630275731207)) ;
#34052 = CARTESIAN_POINT('Ctrl Pts',(-20.5482430959642,-8.22761044915114,
-11.1528675021283)) ;
#34053 = CARTESIAN_POINT('Ctrl Pts',(-20.3745544390668,-8.63732403421366,
-11.1427074311358)) ;
#34054 = CARTESIAN_POINT('Ctrl Pts',(-20.2008761444342,-9.04701317576482,
-11.1325479662932)) ;
#34055 = CARTESIAN_POINT('Ctrl Pts',(-20.0148311567656,-9.45147566690294,
-11.1223885014506)) ;
#34056 = CARTESIAN_POINT('Ctrl Pts',(-19.8167622038062,-9.84996298573239,
-11.112229036608)) ;
#34057 = CARTESIAN_POINT('Ctrl Pts',(-19.6093187594976,-10.2673104836424,
-11.1015887300491)) ;
#34058 = CARTESIAN_POINT('Ctrl Pts',(-19.38868594734,-10.6781033739189,-11.0909484234902)) ;
#34059 = CARTESIAN_POINT('Ctrl Pts',(-19.1553123747469,-11.0815090528488,
-11.0803081169313)) ;
#34060 = CARTESIAN_POINT('Ctrl Pts',(-18.9324634949436,-11.4667219227418,
-11.070147667438)) ;
#34061 = CARTESIAN_POINT('Ctrl Pts',(-18.6979975965305,-11.8451988543758,
-11.0599872179446)) ;
#34062 = CARTESIAN_POINT('Ctrl Pts',(-18.452351361982,-12.2162418229365,-11.0498267684513)) ;
#34063 = CARTESIAN_POINT('Ctrl Pts',(-18.2066941287932,-12.5873014046895,
-11.0396658640309)) ;
#34064 = CARTESIAN_POINT('Ctrl Pts',(-17.9498556879653,-12.9509261682689,
-11.0295049596105)) ;
#34065 = CARTESIAN_POINT('Ctrl Pts',(-17.6823159227956,-13.306447259466,-11.01934405519)) ;
#34066 = CARTESIAN_POINT('Ctrl Pts',(-17.4147316989321,-13.6620274297435,
-11.0091814622709)) ;
#34067 = CARTESIAN_POINT('Ctrl Pts',(-17.1364427354867,-14.0095010535141,
-10.9990188693518)) ;
#34068 = CARTESIAN_POINT('Ctrl Pts',(-16.8479702756838,-14.3482309938256,
-10.9888562764327)) ;
#34069 = CARTESIAN_POINT('Ctrl Pts',(-16.8071807749903,-14.3961268142608,
-10.9874193035889)) ;
#34070 = CARTESIAN_POINT('Ctrl Pts',(-16.7661877359645,-14.4438478730751,
-10.9859823307451)) ;
#34071 = CARTESIAN_POINT('Ctrl Pts',(-16.7249926958962,-14.4913924239432,
-10.9845453579013)) ;
#34072 = CARTESIAN_POINT('Ctrl Pts',(-16.4258556096824,-14.8366363753617,
-10.9741108039174)) ;
#34073 = CARTESIAN_POINT('Ctrl Pts',(-16.115986170001,-15.1726594823227,-10.9636762499335)) ;
#34074 = CARTESIAN_POINT('Ctrl Pts',(-15.7959812961833,-15.4988002746383,
-10.9532416959496)) ;
#34075 = CARTESIAN_POINT('Ctrl Pts',(-15.4843621709359,-15.8163945262395,
-10.9430805801328)) ;
#34076 = CARTESIAN_POINT('Ctrl Pts',(-15.163132185395,-16.1246175980715,-10.932919464316)) ;
#34077 = CARTESIAN_POINT('Ctrl Pts',(-14.8328809084565,-16.4228949645928,
-10.9227583484991)) ;
#34078 = CARTESIAN_POINT('Ctrl Pts',(-14.502663589852,-16.7211416605213,-10.9125982775066)) ;
#34079 = CARTESIAN_POINT('Ctrl Pts',(-14.1634270030494,-17.009444540111,-10.9024382065141)) ;
#34080 = CARTESIAN_POINT('Ctrl Pts',(-13.8157959238133,-17.2872675126535,
-10.8922781355216)) ;
#34081 = CARTESIAN_POINT('Ctrl Pts',(-13.4681855842518,-17.5650739102738,
-10.882118670679)) ;
#34082 = CARTESIAN_POINT('Ctrl Pts',(-13.1121819320761,-17.8324015066964,
-10.8719592058365)) ;
#34083 = CARTESIAN_POINT('Ctrl Pts',(-12.7484424203036,-18.0887548194646,
-10.8617997409939)) ;
#34084 = CARTESIAN_POINT('Ctrl Pts',(-12.3674873234739,-18.3572411893184,
-10.8511594344351)) ;
#34085 = CARTESIAN_POINT('Ctrl Pts',(-11.9780467254352,-18.6136893460692,
-10.8405191278762)) ;
#34086 = CARTESIAN_POINT('Ctrl Pts',(-11.5809112054464,-18.8575801924337,
-10.8298788213173)) ;
#34087 = CARTESIAN_POINT('Ctrl Pts',(-11.201685722563,-19.0904720374795,-10.8197183718241)) ;
#34088 = CARTESIAN_POINT('Ctrl Pts',(-10.8154441484443,-19.3119138847356,
-10.8095579223309)) ;
#34089 = CARTESIAN_POINT('Ctrl Pts',(-10.4229025731864,-19.5214993535938,
-10.7993974728376)) ;
#34090 = CARTESIAN_POINT('Ctrl Pts',(-10.0303434221401,-19.7310942065023,
-10.789236568417)) ;
#34091 = CARTESIAN_POINT('Ctrl Pts',(-9.63148390994459,-19.9288315143467,
-10.7790756639964)) ;
#34092 = CARTESIAN_POINT('Ctrl Pts',(-9.22706425791738,-20.1143511017075,
-10.7689147595758)) ;
#34093 = CARTESIAN_POINT('Ctrl Pts',(-8.82257740104682,-20.2999015179728,
-10.7587521666567)) ;
#34094 = CARTESIAN_POINT('Ctrl Pts',(-8.41252876678408,-20.4732300613035,
-10.7485895737375)) ;
#34095 = CARTESIAN_POINT('Ctrl Pts',(-7.99767987719359,-20.6340241262928,
-10.7384269808184)) ;
#34096 = CARTESIAN_POINT('Ctrl Pts',(-7.93902097062444,-20.6567601255247,
-10.7369900079748)) ;
#34097 = CARTESIAN_POINT('Ctrl Pts',(-7.88026612142671,-20.6792455963373,
-10.7355530351312)) ;
#34098 = CARTESIAN_POINT('Ctrl Pts',(-7.82141751240148,-20.7014797335649,
-10.7341160622875)) ;
#34099 = CARTESIAN_POINT('Ctrl Pts',(-7.40624151015085,-20.8583412186629,
-10.7239782416927)) ;
#34100 = CARTESIAN_POINT('Ctrl Pts',(-6.98628722558425,-21.0027307383675,
-10.7138404210978)) ;
#34101 = CARTESIAN_POINT('Ctrl Pts',(-6.56232615274566,-21.1343727261419,
-10.703702600503)) ;
#34102 = CARTESIAN_POINT('Ctrl Pts',(-6.13843308668183,-21.26599359748,-10.6935664060963)) ;
#34103 = CARTESIAN_POINT('Ctrl Pts',(-5.71053473731159,-21.3848709522725,
-10.6834302116896)) ;
#34104 = CARTESIAN_POINT('Ctrl Pts',(-5.27941863444923,-21.4907788119633,
-10.673294017283)) ;
#34105 = CARTESIAN_POINT('Ctrl Pts',(-4.84800360564933,-21.5967601057152,
-10.6631507946735)) ;
#34106 = CARTESIAN_POINT('Ctrl Pts',(-4.41336658261689,-21.6897538469575,
-10.6530075720639)) ;
#34107 = CARTESIAN_POINT('Ctrl Pts',(-3.97630984636663,-21.7695841730656,
-10.6428643494544)) ;
#34108 = CARTESIAN_POINT('Ctrl Pts',(-3.53961532798087,-21.8493483384951,
-10.6327295332053)) ;
#34109 = CARTESIAN_POINT('Ctrl Pts',(-3.10050533466276,-21.915970861745,-10.6225947169562)) ;
#34110 = CARTESIAN_POINT('Ctrl Pts',(-2.65978984330864,-21.9693275512004,
-10.612459900707)) ;
#34111 = CARTESIAN_POINT('Ctrl Pts',(-2.21852602234166,-22.0227506260074,
-10.6023124749173)) ;
#34112 = CARTESIAN_POINT('Ctrl Pts',(-1.77565293561,-22.0628747976657,-10.5921650491276)) ;
#34113 = CARTESIAN_POINT('Ctrl Pts',(-1.331989863321,-22.0896273863212,-10.5820176233379)) ;
#34114 = CARTESIAN_POINT('Ctrl Pts',(-0.888326791031996,-22.1163799749766,
-10.5718701975482)) ;
#34115 = CARTESIAN_POINT('Ctrl Pts',(-0.443873966088516,-22.1297609690224,
-10.5617227717585)) ;
#34116 = CARTESIAN_POINT('Ctrl Pts',(0.000546534359808369,-22.1297499932512,
-10.5515753459688)) ;
#34117 = CARTESIAN_POINT('Ctrl Pts',(0.000544184811332343,-22.1297499933091,
-10.0859246540312)) ;
#34118 = CARTESIAN_POINT('Ctrl Pts',(-0.443392383725113,-22.1297609099953,
-10.0960609647218)) ;
#34119 = CARTESIAN_POINT('Ctrl Pts',(-0.887360401803858,-22.1164090174797,
-10.1061972754123)) ;
#34120 = CARTESIAN_POINT('Ctrl Pts',(-1.3305405724524,-22.0897147298818,-10.1163335861029)) ;
#34121 = CARTESIAN_POINT('Ctrl Pts',(-1.77369351406842,-22.0630220823836,
-10.1264692740175)) ;
#34122 = CARTESIAN_POINT('Ctrl Pts',(-2.21605847372859,-22.0229886914173,
-10.1366049619322)) ;
#34123 = CARTESIAN_POINT('Ctrl Pts',(-2.65681909988972,-21.969687010355,-10.1467406498468)) ;
#34124 = CARTESIAN_POINT('Ctrl Pts',(-3.09762117372998,-21.916380316978,-10.1568772908882)) ;
#34125 = CARTESIAN_POINT('Ctrl Pts',(-3.53681838216302,-21.8498028649715,
-10.1670139319296)) ;
#34126 = CARTESIAN_POINT('Ctrl Pts',(-3.97360040099842,-21.7700788908925,
-10.177150572971)) ;
#34127 = CARTESIAN_POINT('Ctrl Pts',(-4.41038596564575,-21.6903542696116,
-10.187287296302)) ;
#34128 = CARTESIAN_POINT('Ctrl Pts',(-4.844756073909,-21.5974829566014,-10.197424019633)) ;
#34129 = CARTESIAN_POINT('Ctrl Pts',(-5.27591007353012,-21.491640420371,-10.207560742964)) ;
#34130 = CARTESIAN_POINT('Ctrl Pts',(-5.70715822137385,-21.385774772012,-10.2176996797837)) ;
#34131 = CARTESIAN_POINT('Ctrl Pts',(-6.13518863136855,-21.2669322928212,
-10.2278386166034)) ;
#34132 = CARTESIAN_POINT('Ctrl Pts',(-6.55921321524739,-21.13533905712,-10.237977553423)) ;
#34133 = CARTESIAN_POINT('Ctrl Pts',(-6.97217961022537,-21.0071776574816,
-10.2478520756713)) ;
#34134 = CARTESIAN_POINT('Ctrl Pts',(-7.38134625824425,-20.8669221562401,
-10.2577265979196)) ;
#34135 = CARTESIAN_POINT('Ctrl Pts',(-7.78600007850508,-20.7148265220836,
-10.2676011201678)) ;
#34136 = CARTESIAN_POINT('Ctrl Pts',(-8.21360376667814,-20.5541048116635,
-10.2780356741518)) ;
#34137 = CARTESIAN_POINT('Ctrl Pts',(-8.63628456897859,-20.3801176356223,
-10.2884702281357)) ;
#34138 = CARTESIAN_POINT('Ctrl Pts',(-9.05321496226866,-20.1931952377392,
-10.2989047821196)) ;
#34139 = CARTESIAN_POINT('Ctrl Pts',(-9.45921966743386,-20.0111711534733,
-10.3090658979364)) ;
#34140 = CARTESIAN_POINT('Ctrl Pts',(-9.85977126683292,-19.8168812107641,
-10.3192270137532)) ;
#34141 = CARTESIAN_POINT('Ctrl Pts',(-10.254126328709,-19.610678935146,-10.32938812957)) ;
#34142 = CARTESIAN_POINT('Ctrl Pts',(-10.6484408407306,-19.4044978624312,
-10.3395482005625)) ;
#34143 = CARTESIAN_POINT('Ctrl Pts',(-11.0365598846075,-19.1864070098415,
-10.3497082715549)) ;
#34144 = CARTESIAN_POINT('Ctrl Pts',(-11.4177638553577,-18.9568062607019,
-10.3598683425474)) ;
#34145 = CARTESIAN_POINT('Ctrl Pts',(-11.7989450834734,-18.7272192095464,
-10.3700278073899)) ;
#34146 = CARTESIAN_POINT('Ctrl Pts',(-12.1732118661025,-18.4861237521248,
-10.3801872722323)) ;
#34147 = CARTESIAN_POINT('Ctrl Pts',(-12.5398713412977,-18.2339645114879,
-10.3903467370748)) ;
#34148 = CARTESIAN_POINT('Ctrl Pts',(-12.9238846017689,-17.969870716821,-10.4009870436337)) ;
#34149 = CARTESIAN_POINT('Ctrl Pts',(-13.2995529305382,-17.6936408428704,
-10.4116273501926)) ;
#34150 = CARTESIAN_POINT('Ctrl Pts',(-13.6661151154515,-17.4058361681859,
-10.4222676567515)) ;
#34151 = CARTESIAN_POINT('Ctrl Pts',(-14.01614606102,-17.1310109227976,-10.4324281062448)) ;
#34152 = CARTESIAN_POINT('Ctrl Pts',(-14.3578737493921,-16.8456318200322,
-10.442588555738)) ;
#34153 = CARTESIAN_POINT('Ctrl Pts',(-14.6906685312681,-16.5502293992232,
-10.4527490052313)) ;
#34154 = CARTESIAN_POINT('Ctrl Pts',(-15.0234782138073,-16.2548137519687,
-10.4629099096519)) ;
#34155 = CARTESIAN_POINT('Ctrl Pts',(-15.3473540206489,-15.9493740441314,
-10.4730708140725)) ;
#34156 = CARTESIAN_POINT('Ctrl Pts',(-15.6617012605832,-15.6344794824371,
-10.483231718493)) ;
#34157 = CARTESIAN_POINT('Ctrl Pts',(-15.9761007374898,-15.3195325928188,
-10.4933943114122)) ;
#34158 = CARTESIAN_POINT('Ctrl Pts',(-16.2809683214846,-14.9951278724074,
-10.5035569043314)) ;
#34159 = CARTESIAN_POINT('Ctrl Pts',(-16.5757465417907,-14.6618710144652,
-10.5137194972506)) ;
#34160 = CARTESIAN_POINT('Ctrl Pts',(-16.6174276659735,-14.6147490782983,
-10.5151564700943)) ;
#34161 = CARTESIAN_POINT('Ctrl Pts',(-16.6589071323296,-14.5674502139036,
-10.516593442938)) ;
#34162 = CARTESIAN_POINT('Ctrl Pts',(-16.7001834281708,-14.5199761889595,
-10.5180304157816)) ;
#34163 = CARTESIAN_POINT('Ctrl Pts',(-16.999910551831,-14.175244360313,-10.5284649697656)) ;
#34164 = CARTESIAN_POINT('Ctrl Pts',(-17.2889986817735,-13.8211841236492,
-10.5388995237495)) ;
#34165 = CARTESIAN_POINT('Ctrl Pts',(-17.5668769022766,-13.4584795189784,
-10.5493340777334)) ;
#34166 = CARTESIAN_POINT('Ctrl Pts',(-17.8374733059035,-13.1052796121086,
-10.5594951935502)) ;
#34167 = CARTESIAN_POINT('Ctrl Pts',(-18.0974396498937,-12.7438827864294,
-10.569656309367)) ;
#34168 = CARTESIAN_POINT('Ctrl Pts',(-18.3462900644125,-12.3749535730418,
-10.5798174251838)) ;
#34169 = CARTESIAN_POINT('Ctrl Pts',(-18.5951148907004,-12.0060622950777,
-10.5899774961762)) ;
#34170 = CARTESIAN_POINT('Ctrl Pts',(-18.8328259423312,-11.6296403667387,
-10.6001375671687)) ;
#34171 = CARTESIAN_POINT('Ctrl Pts',(-19.0589803550444,-11.2463817687526,
-10.6102976381611)) ;
#34172 = CARTESIAN_POINT('Ctrl Pts',(-19.2851212753845,-10.863146035976,-10.6204571030037)) ;
#34173 = CARTESIAN_POINT('Ctrl Pts',(-19.4997068176385,-10.4730746460644,
-10.6306165678462)) ;
#34174 = CARTESIAN_POINT('Ctrl Pts',(-19.7023389190521,-10.076888219153,-10.6407760326888)) ;
#34175 = CARTESIAN_POINT('Ctrl Pts',(-19.914561483048,-9.66195051306934,-10.6514163392477)) ;
#34176 = CARTESIAN_POINT('Ctrl Pts',(-20.1136717964291,-9.24030525979585,
-10.6620566458066)) ;
#34177 = CARTESIAN_POINT('Ctrl Pts',(-20.2992671449799,-8.81280820392919,
-10.6726969523655)) ;
#34178 = CARTESIAN_POINT('Ctrl Pts',(-20.4764925054238,-8.40459043119787,
-10.6828574018587)) ;
#34179 = CARTESIAN_POINT('Ctrl Pts',(-20.6413947006628,-7.99103715615273,
-10.693017851352)) ;
#34180 = CARTESIAN_POINT('Ctrl Pts',(-20.7936721328555,-7.57291451779358,
-10.7031783008453)) ;
#34181 = CARTESIAN_POINT('Ctrl Pts',(-20.9459563831685,-7.15477315827262,
-10.7133392052659)) ;
#34182 = CARTESIAN_POINT('Ctrl Pts',(-21.085614664725,-6.73206224313735,-10.7235001096865)) ;
#34183 = CARTESIAN_POINT('Ctrl Pts',(-21.2123945201883,-6.30556530236464,
-10.7336610141071)) ;
#34184 = CARTESIAN_POINT('Ctrl Pts',(-21.3391954434224,-5.8789974880314,-10.7438236070262)) ;
#34185 = CARTESIAN_POINT('Ctrl Pts',(-21.4531135990334,-5.44864261096266,
-10.7539861999454)) ;
#34186 = CARTESIAN_POINT('Ctrl Pts',(-21.5539466232426,-5.01529859778159,
-10.7641487928646)) ;
#34187 = CARTESIAN_POINT('Ctrl Pts',(-21.568204236303,-4.95402451312071,-10.7655857657082)) ;
#34188 = CARTESIAN_POINT('Ctrl Pts',(-21.5822003150699,-4.8926906849236,-10.7670227385519)) ;
#34189 = CARTESIAN_POINT('Ctrl Pts',(-21.5959343694665,-4.83129938755548,
-10.7684597113956)) ;
#34190 = CARTESIAN_POINT('Ctrl Pts',(-21.6956639730229,-4.38550752074539,
-10.7788942653795)) ;
#34191 = CARTESIAN_POINT('Ctrl Pts',(-21.7815984515182,-3.93656892420253,
-10.7893288193634)) ;
#34192 = CARTESIAN_POINT('Ctrl Pts',(-21.8535608715591,-3.48535683905719,
-10.7997633733473)) ;
#34193 = CARTESIAN_POINT('Ctrl Pts',(-21.9236375116933,-3.04596879600585,
-10.8099244891641)) ;
#34194 = CARTESIAN_POINT('Ctrl Pts',(-21.980464965085,-2.60442513320454,-10.8200856049809)) ;
#34195 = CARTESIAN_POINT('Ctrl Pts',(-22.023931834818,-2.16154148648363,-10.8302467207977)) ;
#34196 = CARTESIAN_POINT('Ctrl Pts',(-22.0673942350375,-1.71870337960595,
-10.8404067917901)) ;
#34197 = CARTESIAN_POINT('Ctrl Pts',(-22.0974987733527,-1.27452579240092,
-10.8505668627826)) ;
#34198 = CARTESIAN_POINT('Ctrl Pts',(-22.1141858891321,-0.829829815932281,
-10.860726933775)) ;
#34199 = CARTESIAN_POINT('Ctrl Pts',(-22.1308720093581,-0.385160370027927,
-10.8708863986176)) ;
#34200 = CARTESIAN_POINT('Ctrl Pts',(-22.1341422976873,0.0600271740320306,
-10.8810458634601)) ;
#34201 = CARTESIAN_POINT('Ctrl Pts',(-22.1239892732356,0.504909596124077,
-10.8912053283027)) ;
#34202 = CARTESIAN_POINT('Ctrl Pts',(-22.1133557118875,0.970848051257177,
-10.9018456348616)) ;
#34203 = CARTESIAN_POINT('Ctrl Pts',(-22.0879976776636,1.43645153771628,-10.9124859414205)) ;
#34204 = CARTESIAN_POINT('Ctrl Pts',(-22.0479678562076,1.90077575587892,-10.9231262479794)) ;
#34205 = CARTESIAN_POINT('Ctrl Pts',(-22.0097433015976,2.34415985773987,-10.9332866974726)) ;
#34206 = CARTESIAN_POINT('Ctrl Pts',(-21.9581408990753,2.7863772673351,-10.9434471469659)) ;
#34207 = CARTESIAN_POINT('Ctrl Pts',(-21.893259673349,3.22661059593695,-10.9536075964591)) ;
#34208 = CARTESIAN_POINT('Ctrl Pts',(-21.8283755426094,3.66686363568972,-10.9637685008797)) ;
#34209 = CARTESIAN_POINT('Ctrl Pts',(-21.7502114365678,4.10513219023872,-10.9739294053002)) ;
#34210 = CARTESIAN_POINT('Ctrl Pts',(-21.6589178785627,4.54060694094708,-10.9840903097208)) ;
#34211 = CARTESIAN_POINT('Ctrl Pts',(-21.5676091497579,4.97615405711429,-10.9942529026399)) ;
#34212 = CARTESIAN_POINT('Ctrl Pts',(-21.4631666566022,5.40890621715232,-11.0044154955591)) ;
#34213 = CARTESIAN_POINT('Ctrl Pts',(-21.3457918355023,5.83806525981865,-11.0145780884782)) ;
#34214 = CARTESIAN_POINT('Ctrl Pts',(-21.3291952413263,5.89874759697905,-11.0160150613219)) ;
#34215 = CARTESIAN_POINT('Ctrl Pts',(-21.3123401673082,5.95935811737186,-11.0174520341656)) ;
#34216 = CARTESIAN_POINT('Ctrl Pts',(-21.2952272639061,6.01989458720738,-11.0188890070094)) ;
#34217 = CARTESIAN_POINT('Ctrl Pts',(-21.1709622054873,6.4594791383414,-11.0293235609933)) ;
#34218 = CARTESIAN_POINT('Ctrl Pts',(-21.0330653019663,6.89527156835765,-11.0397581149772)) ;
#34219 = CARTESIAN_POINT('Ctrl Pts',(-20.8817961763543,7.32641955607873,-11.0501926689611)) ;
#34220 = CARTESIAN_POINT('Ctrl Pts',(-20.7344910680365,7.74626928268595,-11.0603537847779)) ;
#34221 = CARTESIAN_POINT('Ctrl Pts',(-20.5745056923739,8.16171464033577,-11.0705149005947)) ;
#34222 = CARTESIAN_POINT('Ctrl Pts',(-20.4021299299239,8.57198514843583,-11.0806760164115)) ;
#34223 = CARTESIAN_POINT('Ctrl Pts',(-20.2297718921408,8.98221347016345,-11.0908360874039)) ;
#34224 = CARTESIAN_POINT('Ctrl Pts',(-20.0450261013507,9.38726779366562,-11.1009961583964)) ;
#34225 = CARTESIAN_POINT('Ctrl Pts',(-19.848230632152,9.78639749015959,-11.1111562293888)) ;
#34226 = CARTESIAN_POINT('Ctrl Pts',(-19.6514469037722,10.1855033745736,-11.1213156942314)) ;
#34227 = CARTESIAN_POINT('Ctrl Pts',(-19.4426150346879,10.5786851323224,-11.131475159074)) ;
#34228 = CARTESIAN_POINT('Ctrl Pts',(-19.2221199259505,10.9652150282097,-11.1416346239165)) ;
#34229 = CARTESIAN_POINT('Ctrl Pts',(-18.9911889086123,11.370039165126,-11.1522749304754)) ;
#34230 = CARTESIAN_POINT('Ctrl Pts',(-18.7474642290177,11.7675664183543,-11.1629152370343)) ;
#34231 = CARTESIAN_POINT('Ctrl Pts',(-18.4914412953425,12.1569911525592,-11.1735555435932)) ;
#34232 = CARTESIAN_POINT('Ctrl Pts',(-18.2469644964523,12.5288535910541,-11.1837159930865)) ;
#34233 = CARTESIAN_POINT('Ctrl Pts',(-17.9912741721608,12.893327874591,-11.1938764425798)) ;
#34234 = CARTESIAN_POINT('Ctrl Pts',(-17.7248461421975,13.2497420464674,-11.2040368920731)) ;
#34235 = CARTESIAN_POINT('Ctrl Pts',(-17.458406183098,13.6061721765492,-11.2141977964937)) ;
#34236 = CARTESIAN_POINT('Ctrl Pts',(-17.1812276970607,13.9545412915113,-11.2243587009142)) ;
#34237 = CARTESIAN_POINT('Ctrl Pts',(-16.893827968865,14.2942090239683,-11.2345196053348)) ;
#34238 = CARTESIAN_POINT('Ctrl Pts',(-16.6063804817296,14.6339332010532,-11.244682198254)) ;
#34239 = CARTESIAN_POINT('Ctrl Pts',(-16.3087085068463,14.9649529312239,-11.2548447911731)) ;
#34240 = CARTESIAN_POINT('Ctrl Pts',(-16.0013688107662,15.2866618738147,-11.2650073840922)) ;
#34241 = CARTESIAN_POINT('Ctrl Pts',(-15.9579115159039,15.3321509549725,-11.2664443569359)) ;
#34242 = CARTESIAN_POINT('Ctrl Pts',(-15.9142609916012,15.3774539397569,-11.2678813297796)) ;
#34243 = CARTESIAN_POINT('Ctrl Pts',(-15.8704188723364,15.4225691724527,-11.2693183026233)) ;
#34244 = CARTESIAN_POINT('Ctrl Pts',(-15.5520600653141,15.7501726711075,-11.2797528566072)) ;
#34245 = CARTESIAN_POINT('Ctrl Pts',(-15.2235128156921,16.0679576657595,-11.2901874105911)) ;
#34246 = CARTESIAN_POINT('Ctrl Pts',(-14.8854108318645,16.375297842455,-11.300621964575)) ;
#34247 = CARTESIAN_POINT('Ctrl Pts',(-14.556168832556,16.6745841497919,-11.3107830803918)) ;
#34248 = CARTESIAN_POINT('Ctrl Pts',(-14.2178666372514,16.9639658877613,-11.3209441962086)) ;
#34249 = CARTESIAN_POINT('Ctrl Pts',(-13.8711256523269,17.24290312563,-11.3311053120254)) ;
#34250 = CARTESIAN_POINT('Ctrl Pts',(-13.5244203213032,17.5218116815687,-11.3412653830178)) ;
#34251 = CARTESIAN_POINT('Ctrl Pts',(-13.1692781127201,17.7902777388003,-11.3514254540103)) ;
#34252 = CARTESIAN_POINT('Ctrl Pts',(-12.8063533882028,18.0478017486609,-11.3615855250028)) ;
#34253 = CARTESIAN_POINT('Ctrl Pts',(-12.4434503157737,18.3053103946397,-11.3717449898454)) ;
#34254 = CARTESIAN_POINT('Ctrl Pts',(-12.0727658421736,18.5518781646479,-11.381904454688)) ;
#34255 = CARTESIAN_POINT('Ctrl Pts',(-11.6949846347086,18.7870479175529,-11.3920639195307)) ;
#34256 = CARTESIAN_POINT('Ctrl Pts',(-11.2993232566861,19.0333481216525,-11.4027042260896)) ;
#34257 = CARTESIAN_POINT('Ctrl Pts',(-10.8958774642939,19.2671453181775,-11.4133445326484)) ;
#34258 = CARTESIAN_POINT('Ctrl Pts',(-10.4854661821076,19.4879663897077,-11.4239848392073)) ;
#34259 = CARTESIAN_POINT('Ctrl Pts',(-10.0935636479973,19.6988288617544,-11.4341452887006)) ;
#34260 = CARTESIAN_POINT('Ctrl Pts',(-9.69531013249103,19.8978594691585,-11.4443057381939)) ;
#34261 = CARTESIAN_POINT('Ctrl Pts',(-9.29144375761979,20.0846933748436,-11.4544661876872)) ;
#34262 = CARTESIAN_POINT('Ctrl Pts',(-8.88755929990611,20.2715356458899,-11.4646270921077)) ;
#34263 = CARTESIAN_POINT('Ctrl Pts',(-8.47806169000838,20.4461800299017,-11.4747879965283)) ;
#34264 = CARTESIAN_POINT('Ctrl Pts',(-8.06371050402149,20.6083091972591,-11.4849489009488)) ;
#34265 = CARTESIAN_POINT('Ctrl Pts',(-7.6492904628022,20.7704653065968,-11.495111493868)) ;
#34266 = CARTESIAN_POINT('Ctrl Pts',(-7.23001544766253,20.9201019601147,-11.5052740867872)) ;
#34267 = CARTESIAN_POINT('Ctrl Pts',(-6.80666358498739,21.0569505366591,-11.5154366797064)) ;
#34268 = CARTESIAN_POINT('Ctrl Pts',(-6.74680237291455,21.076300685754,-11.51687365255)) ;
#34269 = CARTESIAN_POINT('Ctrl Pts',(-6.68685967706741,21.0953952377611,-11.5183106253936)) ;
#34270 = CARTESIAN_POINT('Ctrl Pts',(-6.62683772265301,21.1142335134412,-11.5197475982372)) ;
#34271 = CARTESIAN_POINT('Ctrl Pts',(-6.19098931650444,21.2510273334671,-11.5301821522211)) ;
#34272 = CARTESIAN_POINT('Ctrl Pts',(-5.75084743422553,21.3743388151877,-11.540616706205)) ;
#34273 = CARTESIAN_POINT('Ctrl Pts',(-5.30726738537913,21.4839183568219,-11.5510512601889)) ;
#34274 = CARTESIAN_POINT('Ctrl Pts',(-4.87531138061828,21.590626359427,-11.5612123760057)) ;
#34275 = CARTESIAN_POINT('Ctrl Pts',(-4.44009533416375,21.6843128500613,-11.5713734918225)) ;
#34276 = CARTESIAN_POINT('Ctrl Pts',(-4.00242265413292,21.7647983670923,-11.5815346076393)) ;
#34277 = CARTESIAN_POINT('Ctrl Pts',(-3.56479497812494,21.8452756081394,-11.5916946786317)) ;
#34278 = CARTESIAN_POINT('Ctrl Pts',(-3.12471139879775,21.9125545454665,-11.6018547496242)) ;
#34279 = CARTESIAN_POINT('Ctrl Pts',(-2.68298511096576,21.9665069129535,-11.6120148206166)) ;
#34280 = CARTESIAN_POINT('Ctrl Pts',(-2.24128517652377,22.0204560616424,-11.6221742854592)) ;
#34281 = CARTESIAN_POINT('Ctrl Pts',(-1.79794295716301,22.0610802010845,-11.6323337503018)) ;
#34282 = CARTESIAN_POINT('Ctrl Pts',(-1.35377814039208,22.0883027824479,-11.6424932151443)) ;
#34283 = CARTESIAN_POINT('Ctrl Pts',(-0.888591254434927,22.1168137931674,
-11.6531335217032)) ;
#34284 = CARTESIAN_POINT('Ctrl Pts',(-0.42250230375543,22.130624171767,-11.6637738282621)) ;
#34285 = CARTESIAN_POINT('Ctrl Pts',(0.0435433219828738,22.1297071612259,
-11.674414134821)) ;
#34286 = CARTESIAN_POINT('Ctrl Pts',(0.48857119929579,22.1288315060709,-11.6845745843143)) ;
#34287 = CARTESIAN_POINT('Ctrl Pts',(0.93355932782238,22.1145272841406,-11.6947350338075)) ;
#34288 = CARTESIAN_POINT('Ctrl Pts',(1.37768489166807,22.0868245658304,-11.7048954833007)) ;
#34289 = CARTESIAN_POINT('Ctrl Pts',(1.82183034094231,22.0591206071493,-11.7150563877214)) ;
#34290 = CARTESIAN_POINT('Ctrl Pts',(2.26511291944918,22.018016970129,-11.725217292142)) ;
#34291 = CARTESIAN_POINT('Ctrl Pts',(2.70671353053708,21.9635957194196,-11.7353781965627)) ;
#34292 = CARTESIAN_POINT('Ctrl Pts',(3.14838752505139,21.9091654252041,-11.7455407894819)) ;
#34293 = CARTESIAN_POINT('Ctrl Pts',(3.58837876587045,21.8414131234149,-11.7557033824011)) ;
#34294 = CARTESIAN_POINT('Ctrl Pts',(4.02587500114296,21.7604725485839,-11.7658659753202)) ;
#34295 = CARTESIAN_POINT('Ctrl Pts',(4.08773620273373,21.7490276930336,-11.7673029481638)) ;
#34296 = CARTESIAN_POINT('Ctrl Pts',(4.14954753563977,21.7373192419766,-11.7687399210074)) ;
#34297 = CARTESIAN_POINT('Ctrl Pts',(4.21130671935913,21.7253476560901,-11.770176893851)) ;
#34298 = CARTESIAN_POINT('Ctrl Pts',(4.65976998670447,21.6384161877862,-11.7806114478349)) ;
#34299 = CARTESIAN_POINT('Ctrl Pts',(5.10559865867327,21.5375826947857,-11.7910460018188)) ;
#34300 = CARTESIAN_POINT('Ctrl Pts',(5.54792163087631,21.423034347173,-11.8014805558027)) ;
#34301 = CARTESIAN_POINT('Ctrl Pts',(5.97865350076954,21.3114877464739,-11.8116416716195)) ;
#34302 = CARTESIAN_POINT('Ctrl Pts',(6.40606082013145,21.186935954134,-11.8218027874363)) ;
#34303 = CARTESIAN_POINT('Ctrl Pts',(6.82935149681334,21.0496031600473,-11.8319639032532)) ;
#34304 = CARTESIAN_POINT('Ctrl Pts',(7.25259864831268,20.9122844873086,-11.8421239742456)) ;
#34305 = CARTESIAN_POINT('Ctrl Pts',(7.67172978439449,20.7621875087635,-11.852284045238)) ;
#34306 = CARTESIAN_POINT('Ctrl Pts',(8.0859685496601,20.5995861044927,-11.8624441162304)) ;
#34307 = CARTESIAN_POINT('Ctrl Pts',(8.50018260144122,20.4369944010216,-11.872603581073)) ;
#34308 = CARTESIAN_POINT('Ctrl Pts',(8.90950465192139,20.2618998460975,-11.8827630459156)) ;
#34309 = CARTESIAN_POINT('Ctrl Pts',(9.31317722828008,20.0746249025267,-11.8929225107582)) ;
#34310 = CARTESIAN_POINT('Ctrl Pts',(9.73595539902207,19.8784863419565,-11.9035628173171)) ;
#34311 = CARTESIAN_POINT('Ctrl Pts',(10.1525362281744,19.6689868209902,-11.914203123876)) ;
#34312 = CARTESIAN_POINT('Ctrl Pts',(10.5620753425864,19.4465523813356,-11.9248434304349)) ;
#34313 = CARTESIAN_POINT('Ctrl Pts',(10.9531450419859,19.2341493009199,-11.9350038799281)) ;
#34314 = CARTESIAN_POINT('Ctrl Pts',(11.3377938268513,19.0099521608913,-11.9451643294214)) ;
#34315 = CARTESIAN_POINT('Ctrl Pts',(11.7153121750737,18.7743787035169,-11.9553247789147)) ;
#34316 = CARTESIAN_POINT('Ctrl Pts',(12.0928474264256,18.5387946984998,-11.9654856833352)) ;
#34317 = CARTESIAN_POINT('Ctrl Pts',(12.4632514097936,18.2918334819398,-11.9756465877557)) ;
#34318 = CARTESIAN_POINT('Ctrl Pts',(12.8258426006866,18.0339567661929,-11.9858074921763)) ;
#34319 = CARTESIAN_POINT('Ctrl Pts',(13.1884940455382,17.7760371975213,-11.9959700850954)) ;
#34320 = CARTESIAN_POINT('Ctrl Pts',(13.5433299167266,17.5071986383238,-12.0061326780146)) ;
#34321 = CARTESIAN_POINT('Ctrl Pts',(13.8896992826413,17.2279449993403,-12.0162952709337)) ;
#34322 = CARTESIAN_POINT('Ctrl Pts',(13.9386753044767,17.1884590237709,-12.0177322437774)) ;
#34323 = CARTESIAN_POINT('Ctrl Pts',(13.9874821046735,17.148764881168,-12.0191692166211)) ;
#34324 = CARTESIAN_POINT('Ctrl Pts',(14.0361178961741,17.1088640612754,-12.0206061894648)) ;
#34325 = CARTESIAN_POINT('Ctrl Pts',(14.3892858729975,16.8191249329445,-12.0310407434487)) ;
#34326 = CARTESIAN_POINT('Ctrl Pts',(14.7335251246837,16.5184092272378,-12.0414752974326)) ;
#34327 = CARTESIAN_POINT('Ctrl Pts',(15.0681583589428,16.2072958488553,-12.0519098514165)) ;
#34328 = CARTESIAN_POINT('Ctrl Pts',(15.3940225074922,15.9043352168266,-12.0620709672334)) ;
#34329 = CARTESIAN_POINT('Ctrl Pts',(15.7107774734568,15.5915150493888,-12.0722320830502)) ;
#34330 = CARTESIAN_POINT('Ctrl Pts',(16.0178330754948,15.2694092429303,-12.082393198867)) ;
#34331 = CARTESIAN_POINT('Ctrl Pts',(16.3248571043089,14.9473365572442,-12.0925532698594)) ;
#34332 = CARTESIAN_POINT('Ctrl Pts',(16.6221836030454,14.6159803058319,-12.1027133408518)) ;
#34333 = CARTESIAN_POINT('Ctrl Pts',(16.9092598639506,14.2759506133878,-12.1128734118442)) ;
#34334 = CARTESIAN_POINT('Ctrl Pts',(17.1963189978866,13.9359412071146,-12.1230328766868)) ;
#34335 = CARTESIAN_POINT('Ctrl Pts',(17.4731289676943,13.5872595689571,-12.1331923415294)) ;
#34336 = CARTESIAN_POINT('Ctrl Pts',(17.7391767799057,13.2305495816974,-12.143351806372)) ;
#34337 = CARTESIAN_POINT('Ctrl Pts',(18.0178164843697,12.8569567127946,-12.1539921129309)) ;
#34338 = CARTESIAN_POINT('Ctrl Pts',(18.2846506579833,12.474557496929,-12.1646324194898)) ;
#34339 = CARTESIAN_POINT('Ctrl Pts',(18.5391391189094,12.0841282595074,-12.1752727260487)) ;
#34340 = CARTESIAN_POINT('Ctrl Pts',(18.782150646777,11.7113066189316,-12.1854331755419)) ;
#34341 = CARTESIAN_POINT('Ctrl Pts',(19.0139051079951,11.3311633367331,-12.1955936250352)) ;
#34342 = CARTESIAN_POINT('Ctrl Pts',(19.2339770009059,10.944403309049,-12.2057540745284)) ;
#34343 = CARTESIAN_POINT('Ctrl Pts',(19.4540587473879,10.5576259644446,-12.215914978949)) ;
#34344 = CARTESIAN_POINT('Ctrl Pts',(19.6624567690063,10.164231483083,-12.2260758833696)) ;
#34345 = CARTESIAN_POINT('Ctrl Pts',(19.8587911032522,9.76495012685115,-12.2362367877901)) ;
#34346 = CARTESIAN_POINT('Ctrl Pts',(20.0551580635548,9.36560241963596,-12.2463993807092)) ;
#34347 = CARTESIAN_POINT('Ctrl Pts',(20.2394572295999,8.96036608885079,-12.2565619736284)) ;
#34348 = CARTESIAN_POINT('Ctrl Pts',(20.411355618518,8.54999396940693,-12.2667245665475)) ;
#34349 = CARTESIAN_POINT('Ctrl Pts',(20.4356617497113,8.49196807029265,-12.2681615393912)) ;
#34350 = CARTESIAN_POINT('Ctrl Pts',(20.4597200247701,8.43383952219665,-12.269598512235)) ;
#34351 = CARTESIAN_POINT('Ctrl Pts',(20.4835295800864,8.3756104854646,-12.2710354850787)) ;
#34352 = CARTESIAN_POINT('Ctrl Pts',(20.6564222630383,7.9527813207642,-12.2814700390626)) ;
#34353 = CARTESIAN_POINT('Ctrl Pts',(20.8162405392581,7.52454223258302,-12.2919045930465)) ;
#34354 = CARTESIAN_POINT('Ctrl Pts',(20.9626639000163,7.09172456299961,-12.3023391470304)) ;
#34355 = CARTESIAN_POINT('Ctrl Pts',(21.1052502270643,6.67024890865189,-12.3125002628472)) ;
#34356 = CARTESIAN_POINT('Ctrl Pts',(21.2351346096812,6.24443179677039,-12.322661378664)) ;
#34357 = CARTESIAN_POINT('Ctrl Pts',(21.3520707879779,5.8150587381111,-12.3328224944809)) ;
#34358 = CARTESIAN_POINT('Ctrl Pts',(21.4689949422243,5.3857298300585,-12.3429825654733)) ;
#34359 = CARTESIAN_POINT('Ctrl Pts',(21.5729734913214,4.95284592699653,-12.3531426364658)) ;
#34360 = CARTESIAN_POINT('Ctrl Pts',(21.6638103688342,4.51720658877718,-12.3633027074582)) ;
#34361 = CARTESIAN_POINT('Ctrl Pts',(21.7546418270177,4.08159324080682,-12.3734621723007)) ;
#34362 = CARTESIAN_POINT('Ctrl Pts',(21.8323331331515,3.64322501075395,-12.3836216371431)) ;
#34363 = CARTESIAN_POINT('Ctrl Pts',(21.8967392106614,3.20291226898011,-12.3937811019856)) ;
#34364 = CARTESIAN_POINT('Ctrl Pts',(21.9641935913388,2.74175977454134,-12.4044214085445)) ;
#34365 = CARTESIAN_POINT('Ctrl Pts',(22.0170749229654,2.27847454785169,-12.4150617151035)) ;
#34366 = CARTESIAN_POINT('Ctrl Pts',(22.0552771946797,1.81399639700398,-12.4257020216624)) ;
#34367 = CARTESIAN_POINT('Ctrl Pts',(22.0917566184751,1.37046530452788,-12.4358624711555)) ;
#34368 = CARTESIAN_POINT('Ctrl Pts',(22.1148515219845,0.925846736851711,-12.4460229206486)) ;
#34369 = CARTESIAN_POINT('Ctrl Pts',(22.1245228090838,0.480963130427781,-12.4561833701418)) ;
#34370 = CARTESIAN_POINT('Ctrl Pts',(22.1341945292086,0.0360596046334728,
-12.4663442745624)) ;
#34371 = CARTESIAN_POINT('Ctrl Pts',(22.130441429444,-0.409108754106105,-12.4765051789829)) ;
#34372 = CARTESIAN_POINT('Ctrl Pts',(22.113276536622,-0.853718851487109,-12.4866660834035)) ;
#34373 = CARTESIAN_POINT('Ctrl Pts',(22.0961087914068,-1.2984028323929,-12.4968286763225)) ;
#34374 = CARTESIAN_POINT('Ctrl Pts',(22.06552480876,-1.74252813722489,-12.5069912692414)) ;
#34375 = CARTESIAN_POINT('Ctrl Pts',(22.0215896775743,-2.18527415558157,-12.5171538621604)) ;
#34376 = CARTESIAN_POINT('Ctrl Pts',(22.015377326955,-2.24787766732996,-12.5185908350045)) ;
#34377 = CARTESIAN_POINT('Ctrl Pts',(22.0088981253569,-2.31045361039959,-12.5200278078485)) ;
#34378 = CARTESIAN_POINT('Ctrl Pts',(22.0021523404249,-2.37299967366979,-12.5214647806926)) ;
#34379 = CARTESIAN_POINT('Ctrl Pts',(21.9531679373253,-2.82717685340531,-12.5318993346765)) ;
#34380 = CARTESIAN_POINT('Ctrl Pts',(21.890109436478,-3.27989555583653,-12.5423338886604)) ;
#34381 = CARTESIAN_POINT('Ctrl Pts',(21.8130902341816,-3.73027204074327,-12.5527684426443)) ;
#34382 = CARTESIAN_POINT('Ctrl Pts',(21.7380893251005,-4.1688463805134,-12.5629295584611)) ;
#34383 = CARTESIAN_POINT('Ctrl Pts',(21.6498500776779,-4.60519944952066,-12.5730906742779)) ;
#34384 = CARTESIAN_POINT('Ctrl Pts',(21.5485294090372,-5.03852313385167,-12.5832517900946)) ;
#34385 = CARTESIAN_POINT('Ctrl Pts',(21.4472191587707,-5.47180226134795,-12.593411861087)) ;
#34386 = CARTESIAN_POINT('Ctrl Pts',(21.332830226361,-5.9020524029421,-12.6035719320794)) ;
#34387 = CARTESIAN_POINT('Ctrl Pts',(21.2055703646003,-6.32847695535699,-12.6137320030718)) ;
#34388 = CARTESIAN_POINT('Ctrl Pts',(21.078318095163,-6.75487606728283,-12.6238914679143)) ;
#34389 = CARTESIAN_POINT('Ctrl Pts',(20.9381964961067,-7.17744982610941,-12.6340509327568)) ;
#34390 = CARTESIAN_POINT('Ctrl Pts',(20.7854633163735,-7.59541636687505,-12.6442103975994)) ;
#34391 = CARTESIAN_POINT('Ctrl Pts',(20.6255013617559,-8.03316502726702,-12.6548507041583)) ;
#34392 = CARTESIAN_POINT('Ctrl Pts',(20.4517054368565,-8.46585962278698,-12.6654910107172)) ;
#34393 = CARTESIAN_POINT('Ctrl Pts',(20.2644292103402,-8.89262300120791,-12.6761313172761)) ;
#34394 = CARTESIAN_POINT('Ctrl Pts',(20.0855987762474,-9.30014018391493,-12.6862917667694)) ;
#34395 = CARTESIAN_POINT('Ctrl Pts',(19.8944769789702,-9.70224900488492,-12.6964522162627)) ;
#34396 = CARTESIAN_POINT('Ctrl Pts',(19.6914205353077,-10.0982073836975,-12.706612665756)) ;
#34397 = CARTESIAN_POINT('Ctrl Pts',(19.4883549999242,-10.4941834912906,-12.7167735701768)) ;
#34398 = CARTESIAN_POINT('Ctrl Pts',(19.2733538573369,-10.8840084033699,-12.7269344745977)) ;
#34399 = CARTESIAN_POINT('Ctrl Pts',(19.0468199891755,-11.2669642478551,-12.7370953790185)) ;
#34400 = CARTESIAN_POINT('Ctrl Pts',(18.8202484765266,-11.6499837304029,-12.7472579719376)) ;
#34401 = CARTESIAN_POINT('Ctrl Pts',(18.5821405258547,-12.0261316670165,-12.7574205648567)) ;
#34402 = CARTESIAN_POINT('Ctrl Pts',(18.3329436359918,-12.3947171287629,-12.7675831577758)) ;
#34403 = CARTESIAN_POINT('Ctrl Pts',(18.2977076321218,-12.4468344676417,-12.7690201306194)) ;
#34404 = CARTESIAN_POINT('Ctrl Pts',(18.2622499926592,-12.4988006538132,-12.7704571034629)) ;
#34405 = CARTESIAN_POINT('Ctrl Pts',(18.2265720521004,-12.5506137814887,-12.7718940763064)) ;
#34406 = CARTESIAN_POINT('Ctrl Pts',(17.9674972905483,-12.9268539312153,-12.7823286302903)) ;
#34407 = CARTESIAN_POINT('Ctrl Pts',(17.6967352785155,-13.2951181446547,-12.7927631842742)) ;
#34408 = CARTESIAN_POINT('Ctrl Pts',(17.4148060316788,-13.6546829308302,-12.8031977382582)) ;
#34409 = CARTESIAN_POINT('Ctrl Pts',(17.1402647591279,-14.0048252983522,-12.8133588540749)) ;
#34410 = CARTESIAN_POINT('Ctrl Pts',(16.8551341904644,-14.3467181535442,-12.8235199698917)) ;
#34411 = CARTESIAN_POINT('Ctrl Pts',(16.5599366621038,-14.6797252293635,-12.8336810857085)) ;
#34412 = CARTESIAN_POINT('Ctrl Pts',(16.2647694876492,-15.0126980634819,-12.8438411567009)) ;
#34413 = CARTESIAN_POINT('Ctrl Pts',(15.9595375733945,-15.3367867715904,-12.8540012276934)) ;
#34414 = CARTESIAN_POINT('Ctrl Pts',(15.6448025014556,-15.651389387302,-12.8641612986859)) ;
#34415 = CARTESIAN_POINT('Ctrl Pts',(15.3300862066105,-15.965973233822,-12.8743207635285)) ;
#34416 = CARTESIAN_POINT('Ctrl Pts',(15.0058680490801,-16.2710719563738,-12.8844802283712)) ;
#34417 = CARTESIAN_POINT('Ctrl Pts',(14.6727465832436,-16.5661203293472,-12.8946396932138)) ;
#34418 = CARTESIAN_POINT('Ctrl Pts',(14.323858667124,-16.875133174685,-12.9052799997727)) ;
#34419 = CARTESIAN_POINT('Ctrl Pts',(13.9652046178105,-17.1731212774895,-12.9159203063315)) ;
#34420 = CARTESIAN_POINT('Ctrl Pts',(13.597512683015,-17.4594812035681,-12.9265606128904)) ;
#34421 = CARTESIAN_POINT('Ctrl Pts',(13.2464029370764,-17.7329268556963,-12.9367210623838)) ;
#34422 = CARTESIAN_POINT('Ctrl Pts',(12.887052558089,-17.9957696802504,-12.9468815118771)) ;
#34423 = CARTESIAN_POINT('Ctrl Pts',(12.5201282418468,-18.2475265137555,-12.9570419613704)) ;
#34424 = CARTESIAN_POINT('Ctrl Pts',(12.1531874968068,-18.4992946195093,-12.9672028657913)) ;
#34425 = CARTESIAN_POINT('Ctrl Pts',(11.7786723275488,-18.7399756145782,-12.9773637702121)) ;
#34426 = CARTESIAN_POINT('Ctrl Pts',(11.3972785282958,-18.9691295849585,-12.987524674633)) ;
#34427 = CARTESIAN_POINT('Ctrl Pts',(11.0158213505471,-19.1983216352288,-12.9976872675523)) ;
#34428 = CARTESIAN_POINT('Ctrl Pts',(10.6274834555761,-19.4159827151883,-13.0078498604716)) ;
#34429 = CARTESIAN_POINT('Ctrl Pts',(10.2329870740668,-19.6217178301106,-13.0180124533909)) ;
#34430 = CARTESIAN_POINT('Ctrl Pts',(10.1772059765213,-19.6508084150993,-13.019449426234)) ;
#34431 = CARTESIAN_POINT('Ctrl Pts',(10.1213017891803,-19.6796606340271,-13.0208863990771)) ;
#34432 = CARTESIAN_POINT('Ctrl Pts',(10.0652765922826,-19.7082734450116,-13.0223233719203)) ;
#34433 = CARTESIAN_POINT('Ctrl Pts',(9.66981891971409,-19.910238922406,-13.0324663427184)) ;
#34434 = CARTESIAN_POINT('Ctrl Pts',(9.26822673759724,-20.100325336545,-13.0426093135165)) ;
#34435 = CARTESIAN_POINT('Ctrl Pts',(8.86123712984376,-20.2781732804308,-13.0527522843147)) ;
#34436 = CARTESIAN_POINT('Ctrl Pts',(8.45430968843143,-20.4559940586207,-13.0628937058069)) ;
#34437 = CARTESIAN_POINT('Ctrl Pts',(8.04198667986045,-20.6215800075577,-13.0730351272992)) ;
#34438 = CARTESIAN_POINT('Ctrl Pts',(7.62502660957808,-20.7746192327495,-13.0831765487915)) ;
#34439 = CARTESIAN_POINT('Ctrl Pts',(7.20811061852015,-20.927642279293,-13.0933168981763)) ;
#34440 = CARTESIAN_POINT('Ctrl Pts',(6.786558762008,-21.0681211717514,-13.1034572475611)) ;
#34441 = CARTESIAN_POINT('Ctrl Pts',(6.36114786884429,-21.1957928102064,-13.1135975969459)) ;
#34442 = CARTESIAN_POINT('Ctrl Pts',(5.93576194770578,-21.3234569542144,-13.1237373510826)) ;
#34443 = CARTESIAN_POINT('Ctrl Pts',(5.50651766400403,-21.4383152797041,-13.1338771052192)) ;
#34444 = CARTESIAN_POINT('Ctrl Pts',(5.07420699489083,-21.5401545592296,-13.1440168593559)) ;
#34445 = CARTESIAN_POINT('Ctrl Pts',(4.64185758808263,-21.642002964181,-13.1541575220769)) ;
#34446 = CARTESIAN_POINT('Ctrl Pts',(4.20644147134835,-21.7308299361701,-13.1642981847978)) ;
#34447 = CARTESIAN_POINT('Ctrl Pts',(3.7687627767461,-21.8064729425717,-13.1744388475188)) ;
#34448 = CARTESIAN_POINT('Ctrl Pts',(3.33107979540985,-21.8821166898398,-13.18457960956)) ;
#34449 = CARTESIAN_POINT('Ctrl Pts',(2.89113442025274,-21.9445761760917,-13.1947203716011)) ;
#34450 = CARTESIAN_POINT('Ctrl Pts',(2.44973934653467,-21.9937402957419,-13.2048611336423)) ;
#34451 = CARTESIAN_POINT('Ctrl Pts',(2.0082552664889,-22.0429143292266,-13.2150039405454)) ;
#34452 = CARTESIAN_POINT('Ctrl Pts',(1.56532113348893,-22.0787876108243,-13.2251467474485)) ;
#34453 = CARTESIAN_POINT('Ctrl Pts',(1.12175523603032,-22.1013008724133,-13.2352895543516)) ;
#34454 = CARTESIAN_POINT('Ctrl Pts',(0.748063471728612,-22.1202676606439,
-13.2438345832375)) ;
#34455 = CARTESIAN_POINT('Ctrl Pts',(0.373923466354012,-22.1297529490399,
-13.2523796121235)) ;
#34456 = CARTESIAN_POINT('Ctrl Pts',(-0.000174491033434178,-22.1297499993121,
-13.2609246410094)) ;
#34457 = CARTESIAN_POINT('Origin',(0.,0.,-10.)) ;
#34458 = CARTESIAN_POINT('',(-0.000385679535181172,-22.1297499966392,-16.9015753636525)) ;
#34459 = CARTESIAN_POINT('',(-0.000394050632519626,-22.1297499964917,-16.4359246717926)) ;
#34460 = CARTESIAN_POINT('',(-2.71011275034311E-15,-22.12975,-10.)) ;
#34461 = CARTESIAN_POINT('Ctrl Pts',(-0.000398697885898679,-22.1294066254737,
-16.900980646995)) ;
#34462 = CARTESIAN_POINT('Ctrl Pts',(0.445515082507069,-22.129342469394,-16.8906755313063)) ;
#34463 = CARTESIAN_POINT('Ctrl Pts',(0.891431958115295,-22.1158270854489,
-16.8804240694696)) ;
#34464 = CARTESIAN_POINT('Ctrl Pts',(1.33653233619602,-22.0888918978169,-16.870238980174)) ;
#34465 = CARTESIAN_POINT('Ctrl Pts',(1.79786390062111,-22.0609744821951,-16.8596824778435)) ;
#34466 = CARTESIAN_POINT('Ctrl Pts',(2.25831851995547,-22.0186423035969,-16.8491963171386)) ;
#34467 = CARTESIAN_POINT('Ctrl Pts',(2.71698571375422,-21.9619713359938,-16.8387691144879)) ;
#34468 = CARTESIAN_POINT('Ctrl Pts',(3.15957854718771,-21.9072864479878,-16.8287073415328)) ;
#34469 = CARTESIAN_POINT('Ctrl Pts',(3.60050714112743,-21.8392512117159,-16.8186997539423)) ;
#34470 = CARTESIAN_POINT('Ctrl Pts',(4.03895502150918,-21.7579752470251,-16.808711591363)) ;
#34471 = CARTESIAN_POINT('Ctrl Pts',(4.47742742234612,-21.6766947369282,-16.7987228701899)) ;
#34472 = CARTESIAN_POINT('Ctrl Pts',(4.91341883197495,-21.5821718771262,-16.788753457181)) ;
#34473 = CARTESIAN_POINT('Ctrl Pts',(5.34611384725787,-21.4745565329947,-16.7787470699779)) ;
#34474 = CARTESIAN_POINT('Ctrl Pts',(5.77888324139644,-21.3669226901381,-16.7687389627095)) ;
#34475 = CARTESIAN_POINT('Ctrl Pts',(6.20835506704735,-21.2461916635369,-16.7586936895793)) ;
#34476 = CARTESIAN_POINT('Ctrl Pts',(6.63371499978502,-21.112556176669,-16.7485356440111)) ;
#34477 = CARTESIAN_POINT('Ctrl Pts',(6.67992922727902,-21.0980370357813,-16.7474319993265)) ;
#34478 = CARTESIAN_POINT('Ctrl Pts',(6.72609491888823,-21.0833656108719,-16.7463270063693)) ;
#34479 = CARTESIAN_POINT('Ctrl Pts',(6.77221103175265,-21.0685421811914,-16.7452205560158)) ;
#34480 = CARTESIAN_POINT('Ctrl Pts',(7.20711644354217,-20.928747445926,-16.7347859981845)) ;
#34481 = CARTESIAN_POINT('Ctrl Pts',(7.6377212435629,-20.7753936054156,-16.7242215297243)) ;
#34482 = CARTESIAN_POINT('Ctrl Pts',(8.06319260124452,-20.6088199087664,-16.7136124369833)) ;
#34483 = CARTESIAN_POINT('Ctrl Pts',(8.4775141851523,-20.4466113920542,-16.7032813629195)) ;
#34484 = CARTESIAN_POINT('Ctrl Pts',(8.88696805208349,-20.2718671255665,-16.6929080437768)) ;
#34485 = CARTESIAN_POINT('Ctrl Pts',(9.29080806907081,-20.0849356837908,-16.6825508059184)) ;
#34486 = CARTESIAN_POINT('Ctrl Pts',(9.69460655854542,-19.8980234644733,-16.6721946331112)) ;
#34487 = CARTESIAN_POINT('Ctrl Pts',(10.0927924334806,-19.6989266563173,-16.6618546330045)) ;
#34488 = CARTESIAN_POINT('Ctrl Pts',(10.4846410750577,-19.4880268263416,-16.651567069552)) ;
#34489 = CARTESIAN_POINT('Ctrl Pts',(10.8764663371707,-19.2771395796047,-16.641280119902)) ;
#34490 = CARTESIAN_POINT('Ctrl Pts',(11.2619552371151,-19.054450703537,-16.6310456413425)) ;
#34491 = CARTESIAN_POINT('Ctrl Pts',(11.6404015585227,-18.8203712583942,-16.6208788072008)) ;
#34492 = CARTESIAN_POINT('Ctrl Pts',(12.0367599774297,-18.5752126889297,-16.6102307705368)) ;
#34493 = CARTESIAN_POINT('Ctrl Pts',(12.4254010070655,-18.3175714676348,-16.5996488710798)) ;
#34494 = CARTESIAN_POINT('Ctrl Pts',(12.8055292672146,-18.0479464061951,-16.5891310273476)) ;
#34495 = CARTESIAN_POINT('Ctrl Pts',(13.1685140729281,-17.7904812008885,-16.5790875292342)) ;
#34496 = CARTESIAN_POINT('Ctrl Pts',(13.5237401762096,-17.5220942682271,-16.5690985128436)) ;
#34497 = CARTESIAN_POINT('Ctrl Pts',(13.8705432665648,-17.2432669395589,-16.5591300729815)) ;
#34498 = CARTESIAN_POINT('Ctrl Pts',(14.2173618847343,-16.9644271266335,-16.549161186791)) ;
#34499 = CARTESIAN_POINT('Ctrl Pts',(14.5557566675438,-16.675145864195,-16.539212762678)) ;
#34500 = CARTESIAN_POINT('Ctrl Pts',(14.8850834384798,-16.3759393909295,-16.5292295000744)) ;
#34501 = CARTESIAN_POINT('Ctrl Pts',(15.2144649363044,-16.0766831961085,-16.5192445784714)) ;
#34502 = CARTESIAN_POINT('Ctrl Pts',(15.5347752782515,-15.7674983418902,-16.5092246313089)) ;
#34503 = CARTESIAN_POINT('Ctrl Pts',(15.8453916701938,-15.4489382005339,-16.4990951144533)) ;
#34504 = CARTESIAN_POINT('Ctrl Pts',(15.8893133897355,-15.4038932204594,-16.4976627824516)) ;
#34505 = CARTESIAN_POINT('Ctrl Pts',(15.9330413214005,-15.3586608489135,-16.496228231026)) ;
#34506 = CARTESIAN_POINT('Ctrl Pts',(15.9765737421392,-15.3132427127179,-16.4947912219427)) ;
#34507 = CARTESIAN_POINT('Ctrl Pts',(16.2926759308042,-14.9834477687908,-16.4843566605601)) ;
#34508 = CARTESIAN_POINT('Ctrl Pts',(16.5985468894886,-14.6437701875884,-16.4737921907038)) ;
#34509 = CARTESIAN_POINT('Ctrl Pts',(16.8936153172396,-14.2949044544625,-16.4631830980188)) ;
#34510 = CARTESIAN_POINT('Ctrl Pts',(17.1809515893413,-13.955180614862,-16.4528520125627)) ;
#34511 = CARTESIAN_POINT('Ctrl Pts',(17.4580443900343,-13.606744039089,-16.4424786833142)) ;
#34512 = CARTESIAN_POINT('Ctrl Pts',(17.7244031181186,-13.250256189044,-16.4321214362433)) ;
#34513 = CARTESIAN_POINT('Ctrl Pts',(17.9907344586636,-12.8938049937956,-16.4217652541253)) ;
#34514 = CARTESIAN_POINT('Ctrl Pts',(18.2463340431563,-12.5293042118981,-16.4114252456008)) ;
#34515 = CARTESIAN_POINT('Ctrl Pts',(18.4907458857281,-12.1574340973639,-16.4011376742207)) ;
#34516 = CARTESIAN_POINT('Ctrl Pts',(18.7351431473738,-11.7855861675594,-16.3908507165682)) ;
#34517 = CARTESIAN_POINT('Ctrl Pts',(18.9683540956518,-11.4063697154289,-16.3806162304964)) ;
#34518 = CARTESIAN_POINT('Ctrl Pts',(19.1899529460168,-11.0204821823412,-16.3704493970263)) ;
#34519 = CARTESIAN_POINT('Ctrl Pts',(19.4220397597607,-10.6163311325035,-16.3598013815604)) ;
#34520 = CARTESIAN_POINT('Ctrl Pts',(19.6414016093852,-10.2048692691444,-16.3492194780429)) ;
#34521 = CARTESIAN_POINT('Ctrl Pts',(19.8475759560782,-9.78691359598903,-16.3387016462685)) ;
#34522 = CARTESIAN_POINT('Ctrl Pts',(20.0444523991574,-9.38780658963541,-16.3286581401685)) ;
#34523 = CARTESIAN_POINT('Ctrl Pts',(20.229309747748,-8.98278149620444,-16.318669115497)) ;
#34524 = CARTESIAN_POINT('Ctrl Pts',(20.4017925113281,-8.5725776517286,-16.3087006667177)) ;
#34525 = CARTESIAN_POINT('Ctrl Pts',(20.5742829976723,-8.16235544073625,-16.2987317716098)) ;
#34526 = CARTESIAN_POINT('Ctrl Pts',(20.7343976745234,-7.74695394304696,-16.2887833379422)) ;
#34527 = CARTESIAN_POINT('Ctrl Pts',(20.8818153631735,-7.32713362764678,-16.2788000648346)) ;
#34528 = CARTESIAN_POINT('Ctrl Pts',(21.0292575488269,-6.90724354897934,-16.2688151327655)) ;
#34529 = CARTESIAN_POINT('Ctrl Pts',(21.1639983406575,-6.48293311409231,-16.2587951741862)) ;
#34530 = CARTESIAN_POINT('Ctrl Pts',(21.2857530286841,-6.05498528965268,-16.2486656447027)) ;
#34531 = CARTESIAN_POINT('Ctrl Pts',(21.3029686234128,-5.99447528851859,-16.2472333723425)) ;
#34532 = CARTESIAN_POINT('Ctrl Pts',(21.3199246528324,-5.93389260301837,-16.2457988807246)) ;
#34533 = CARTESIAN_POINT('Ctrl Pts',(21.3366203749226,-5.87323948335914,-16.2443619316455)) ;
#34534 = CARTESIAN_POINT('Ctrl Pts',(21.4578581694875,-5.43280028455092,-16.2339273702463)) ;
#34535 = CARTESIAN_POINT('Ctrl Pts',(21.5653959819834,-4.98853289155693,-16.223362899899)) ;
#34536 = CARTESIAN_POINT('Ctrl Pts',(21.6590615068585,-4.5413199178888,-16.2127538065303)) ;
#34537 = CARTESIAN_POINT('Ctrl Pts',(21.7502724984438,-4.10582629488816,-16.2024227276486)) ;
#34538 = CARTESIAN_POINT('Ctrl Pts',(21.8283291030326,-3.66753945279771,-16.1920494048484)) ;
#34539 = CARTESIAN_POINT('Ctrl Pts',(21.8931143018501,-3.22727457632972,-16.181692164185)) ;
#34540 = CARTESIAN_POINT('Ctrl Pts',(21.9578928389617,-2.78705497123813,-16.1713359885318)) ;
#34541 = CARTESIAN_POINT('Ctrl Pts',(22.009402810843,-2.344857714738,-16.1609959864312)) ;
#34542 = CARTESIAN_POINT('Ctrl Pts',(22.0475665860202,-1.90149806147783,-16.15070842152)) ;
#34543 = CARTESIAN_POINT('Ctrl Pts',(22.0857280842954,-1.45816485964926,-16.1404214703788)) ;
#34544 = CARTESIAN_POINT('Ctrl Pts',(22.110545028001,-1.01366929450376,-16.130186990863)) ;
#34545 = CARTESIAN_POINT('Ctrl Pts',(22.1219745248157,-0.568827378077672,
-16.1200201652694)) ;
#34546 = CARTESIAN_POINT('Ctrl Pts',(22.1339449782719,-0.102931149895318,
-16.1093721451036)) ;
#34547 = CARTESIAN_POINT('Ctrl Pts',(22.1312447587415,0.363344973380265,-16.098790233538)) ;
#34548 = CARTESIAN_POINT('Ctrl Pts',(22.1138554908743,0.829062320497137,-16.0882723965198)) ;
#34549 = CARTESIAN_POINT('Ctrl Pts',(22.0972504520552,1.27377653656697,-16.0782288976609)) ;
#34550 = CARTESIAN_POINT('Ctrl Pts',(22.0672580237881,1.71798115666027,-16.0682398804317)) ;
#34551 = CARTESIAN_POINT('Ctrl Pts',(22.0239170757187,2.16085674282196,-16.0582714393598)) ;
#34552 = CARTESIAN_POINT('Ctrl Pts',(21.9805741870779,2.6037521585392,-16.0483025519555)) ;
#34553 = CARTESIAN_POINT('Ctrl Pts',(21.9238814467325,3.04531842922831,-16.0383541262568)) ;
#34554 = CARTESIAN_POINT('Ctrl Pts',(21.8539179578104,3.48473384348501,-16.0283708614441)) ;
#34555 = CARTESIAN_POINT('Ctrl Pts',(21.7839428425521,3.92422227856224,-16.0183859376406)) ;
#34556 = CARTESIAN_POINT('Ctrl Pts',(21.7006923714283,4.36155911551283,-16.0083659876531)) ;
#34557 = CARTESIAN_POINT('Ctrl Pts',(21.6042884274474,4.7959201946728,-15.998236467137)) ;
#34558 = CARTESIAN_POINT('Ctrl Pts',(21.5906569511857,4.85733866465523,-15.9968041572879)) ;
#34559 = CARTESIAN_POINT('Ctrl Pts',(21.5767625593062,4.91869763501853,-15.9953696280684)) ;
#34560 = CARTESIAN_POINT('Ctrl Pts',(21.5626056691803,4.97999477322625,-15.9939326412558)) ;
#34561 = CARTESIAN_POINT('Ctrl Pts',(21.4598065866317,5.42509885432025,-15.9834980807941)) ;
#34562 = CARTESIAN_POINT('Ctrl Pts',(21.3431352851995,5.86705553464502,-15.9729336112498)) ;
#34563 = CARTESIAN_POINT('Ctrl Pts',(21.2128599161341,6.30500644933931,-15.9623245184797)) ;
#34564 = CARTESIAN_POINT('Ctrl Pts',(21.0859984091412,6.73148087367288,-15.951993436662)) ;
#34565 = CARTESIAN_POINT('Ctrl Pts',(20.9462368104512,7.15415689631851,-15.9416201107047)) ;
#34566 = CARTESIAN_POINT('Ctrl Pts',(20.7938598409848,7.57226175957971,-15.9312628666886)) ;
#34567 = CARTESIAN_POINT('Ctrl Pts',(20.6414985396916,7.9903236311775,-15.920906687657)) ;
#34568 = CARTESIAN_POINT('Ctrl Pts',(20.4765245484738,8.40381535729372,-15.9105666819826)) ;
#34569 = CARTESIAN_POINT('Ctrl Pts',(20.2992572700811,8.81198284934143,-15.9002791133298)) ;
#34570 = CARTESIAN_POINT('Ctrl Pts',(20.1220005673712,9.22012599030738,-15.8899921584286)) ;
#34571 = CARTESIAN_POINT('Ctrl Pts',(19.9324520379643,9.622945648585,-15.8797576749853)) ;
#34572 = CARTESIAN_POINT('Ctrl Pts',(19.7309620091718,10.0197035923024,-15.8695908421538)) ;
#34573 = CARTESIAN_POINT('Ctrl Pts',(19.5199356073603,10.4352397940418,-15.8589428206953)) ;
#34574 = CARTESIAN_POINT('Ctrl Pts',(19.2958229094729,10.8441335486082,-15.848360917402)) ;
#34575 = CARTESIAN_POINT('Ctrl Pts',(19.0590541601682,11.2455503929158,-15.8378430819796)) ;
#34576 = CARTESIAN_POINT('Ctrl Pts',(18.8329631809739,11.6288641860625,-15.8277995787021)) ;
#34577 = CARTESIAN_POINT('Ctrl Pts',(18.5953377935072,12.0053633218949,-15.8178105569502)) ;
#34578 = CARTESIAN_POINT('Ctrl Pts',(18.3466018745999,12.3743454338818,-15.8078421112832)) ;
#34579 = CARTESIAN_POINT('Ctrl Pts',(18.0978548187502,12.7433440667337,-15.7978732192874)) ;
#34580 = CARTESIAN_POINT('Ctrl Pts',(17.8379961126401,13.1048249446298,-15.7879247889248)) ;
#34581 = CARTESIAN_POINT('Ctrl Pts',(17.5674861071872,13.4581028341233,-15.7779415194025)) ;
#34582 = CARTESIAN_POINT('Ctrl Pts',(17.2969311496136,13.8114394297275,-15.767956590906)) ;
#34583 = CARTESIAN_POINT('Ctrl Pts',(17.0157211924628,14.1565701935021,-15.75793663618)) ;
#34584 = CARTESIAN_POINT('Ctrl Pts',(16.7243553839128,14.4928280822395,-15.7478071109031)) ;
#34585 = CARTESIAN_POINT('Ctrl Pts',(16.6831569244332,14.5403741792672,-15.7463748191776)) ;
#34586 = CARTESIAN_POINT('Ctrl Pts',(16.6417554811955,14.5877429102753,-15.7449403081396)) ;
#34587 = CARTESIAN_POINT('Ctrl Pts',(16.6001525305366,14.6349324219095,-15.7435033395758)) ;
#34588 = CARTESIAN_POINT('Ctrl Pts',(16.2980522969234,14.9775995227523,-15.7330687782776)) ;
#34589 = CARTESIAN_POINT('Ctrl Pts',(15.9852455699344,15.3109009638877,-15.7225043081408)) ;
#34590 = CARTESIAN_POINT('Ctrl Pts',(15.6623764342191,15.6342091702737,-15.7118952150116)) ;
#34591 = CARTESIAN_POINT('Ctrl Pts',(15.3479681131464,15.9490450561309,-15.7015641341187)) ;
#34592 = CARTESIAN_POINT('Ctrl Pts',(15.0240180537662,16.2544049007209,-15.6911908093172)) ;
#34593 = CARTESIAN_POINT('Ctrl Pts',(14.6911442062324,16.5497443165883,-15.680833566643)) ;
#34594 = CARTESIAN_POINT('Ctrl Pts',(14.3583045867446,16.8450533639207,-15.6704773889614)) ;
#34595 = CARTESIAN_POINT('Ctrl Pts',(14.0165430552721,17.1303441493424,-15.6601373848229)) ;
#34596 = CARTESIAN_POINT('Ctrl Pts',(13.6664991931125,17.4051052013234,-15.6498498178448)) ;
#34597 = CARTESIAN_POINT('Ctrl Pts',(13.3164762145977,17.679849861038,-15.6395628646238)) ;
#34598 = CARTESIAN_POINT('Ctrl Pts',(12.95817183278,17.9440661428831,-15.6293283829993)) ;
#34599 = CARTESIAN_POINT('Ctrl Pts',(12.5922452900304,18.1972712266993,-15.6191615546121)) ;
#34600 = CARTESIAN_POINT('Ctrl Pts',(12.2089996346471,18.4624603752217,-15.608513535534)) ;
#34601 = CARTESIAN_POINT('Ctrl Pts',(11.8174009269038,18.7155830642744,-15.5979316269133)) ;
#34602 = CARTESIAN_POINT('Ctrl Pts',(11.4182244644345,18.9561098095404,-15.5874137914221)) ;
#34603 = CARTESIAN_POINT('Ctrl Pts',(11.0370500981217,19.1857892579249,-15.5773702902258)) ;
#34604 = CARTESIAN_POINT('Ctrl Pts',(10.6489697482767,19.4039887484891,-15.5673812705962)) ;
#34605 = CARTESIAN_POINT('Ctrl Pts',(10.2546903045263,19.6102919916142,-15.5574128270476)) ;
#34606 = CARTESIAN_POINT('Ctrl Pts',(9.86039320715561,19.8166044718404,-15.5474439371681)) ;
#34607 = CARTESIAN_POINT('Ctrl Pts',(9.45989637934238,20.0110195294185,-15.5374955089177)) ;
#34608 = CARTESIAN_POINT('Ctrl Pts',(9.05393064893995,20.1931532917484,-15.527512241464)) ;
#34609 = CARTESIAN_POINT('Ctrl Pts',(8.64789745668619,20.3753173203787,-15.5175273150286)) ;
#34610 = CARTESIAN_POINT('Ctrl Pts',(8.23639345897018,20.5451957927667,-15.5075073623198)) ;
#34611 = CARTESIAN_POINT('Ctrl Pts',(7.8201749628121,20.7024392880846,-15.4973778389826)) ;
#34612 = CARTESIAN_POINT('Ctrl Pts',(7.76132233973509,20.7246732643415,-15.495945540744)) ;
#34613 = CARTESIAN_POINT('Ctrl Pts',(7.70237549952867,20.7466546825148,-15.4945110231702)) ;
#34614 = CARTESIAN_POINT('Ctrl Pts',(7.6433366223019,20.7683826142873,-15.4930740480446)) ;
#34615 = CARTESIAN_POINT('Ctrl Pts',(7.21462721564321,20.9261594754961,-15.482639487253)) ;
#34616 = CARTESIAN_POINT('Ctrl Pts',(6.7809532594462,21.0706060016275,-15.4720750174389)) ;
#34617 = CARTESIAN_POINT('Ctrl Pts',(6.34317979086824,21.2014764159842,-15.4614659244762)) ;
#34618 = CARTESIAN_POINT('Ctrl Pts',(5.91687820583473,21.328917362224,-15.4511348435168)) ;
#34619 = CARTESIAN_POINT('Ctrl Pts',(5.4866891851808,21.4434847700754,-15.440761518499)) ;
#34620 = CARTESIAN_POINT('Ctrl Pts',(5.05341521606951,21.5449936137857,-15.4304042754925)) ;
#34621 = CARTESIAN_POINT('Ctrl Pts',(4.62018579870428,21.646492019767,-15.4200480974779)) ;
#34622 = CARTESIAN_POINT('Ctrl Pts',(4.18387205289975,21.7349346599373,-15.4097080928905)) ;
#34623 = CARTESIAN_POINT('Ctrl Pts',(3.74527984134167,21.8101757510026,-15.3994205253827)) ;
#34624 = CARTESIAN_POINT('Ctrl Pts',(3.30671379622569,21.8854123531791,-15.3891335716319)) ;
#34625 = CARTESIAN_POINT('Ctrl Pts',(2.86586945657449,21.9474490397433,-15.3788990893969)) ;
#34626 = CARTESIAN_POINT('Ctrl Pts',(2.4235563556766,21.9961745840213,-15.3687322589047)) ;
#34627 = CARTESIAN_POINT('Ctrl Pts',(1.96030882380211,22.0472062809803,-15.3580842380277)) ;
#34628 = CARTESIAN_POINT('Ctrl Pts',(1.49545140178371,22.0836509495794,-15.3475023320353)) ;
#34629 = CARTESIAN_POINT('Ctrl Pts',(1.02991790758809,22.1054115135611,-15.3369844961912)) ;
#34630 = CARTESIAN_POINT('Ctrl Pts',(0.585379068081297,22.1261907184518,-15.3269409942765)) ;
#34631 = CARTESIAN_POINT('Ctrl Pts',(0.140224399000022,22.1335869935488,-15.3169519739188)) ;
#34632 = CARTESIAN_POINT('Ctrl Pts',(-0.304726290300343,22.1275702944762,
-15.3069835296644)) ;
#34633 = CARTESIAN_POINT('Ctrl Pts',(-0.74969690195301,22.1215533260101,-15.2970146390799)) ;
#34634 = CARTESIAN_POINT('Ctrl Pts',(-1.19446353490935,22.1021220468533,-15.2870662101471)) ;
#34635 = CARTESIAN_POINT('Ctrl Pts',(-1.63820073751772,22.0692863133329,-15.2770829420619)) ;
#34636 = CARTESIAN_POINT('Ctrl Pts',(-2.08201167859416,22.036445123302,-15.2670980149973)) ;
#34637 = CARTESIAN_POINT('Ctrl Pts',(-2.52479283694592,21.9901948256536,-15.2570780617106)) ;
#34638 = CARTESIAN_POINT('Ctrl Pts',(-2.9657127307059,21.93058770016,-15.2469485378707)) ;
#34639 = CARTESIAN_POINT('Ctrl Pts',(-3.02805803913257,21.9221593559734,-15.2455162407643)) ;
#34640 = CARTESIAN_POINT('Ctrl Pts',(-3.09036612552438,21.913464034756,-15.2440817243279)) ;
#34641 = CARTESIAN_POINT('Ctrl Pts',(-3.15263463060782,21.9045019566268,-15.2426447503456)) ;
#34642 = CARTESIAN_POINT('Ctrl Pts',(-3.60479627335464,21.8394239856061,-15.232210189317)) ;
#34643 = CARTESIAN_POINT('Ctrl Pts',(-4.05498594158336,21.7602585768977,-15.2216457193675)) ;
#34644 = CARTESIAN_POINT('Ctrl Pts',(-4.5023257926841,21.6672008914192,-15.2110366263487)) ;
#34645 = CARTESIAN_POINT('Ctrl Pts',(-4.93794307784933,21.576581787818,-15.2007055452086)) ;
#34646 = CARTESIAN_POINT('Ctrl Pts',(-5.37085809264521,21.472789306177,-15.1903322200844)) ;
#34647 = CARTESIAN_POINT('Ctrl Pts',(-5.80027690904801,21.3560423037386,-15.1799749770272)) ;
#34648 = CARTESIAN_POINT('Ctrl Pts',(-6.22965157017806,21.2393073058875,-15.1696187989604)) ;
#34649 = CARTESIAN_POINT('Ctrl Pts',(-6.65553081823553,21.1096205437445,-15.1592787943764)) ;
#34650 = CARTESIAN_POINT('Ctrl Pts',(-7.07713641751565,20.9672370009374,-15.1489912269084)) ;
#34651 = CARTESIAN_POINT('Ctrl Pts',(-7.49871686383038,20.8248619527241,-15.1387042731961)) ;
#34652 = CARTESIAN_POINT('Ctrl Pts',(-7.91602428757526,20.6697916422236,-15.128469791036)) ;
#34653 = CARTESIAN_POINT('Ctrl Pts',(-8.32829365695817,20.5023131966915,-15.1183029612768)) ;
#34654 = CARTESIAN_POINT('Ctrl Pts',(-8.76007549515082,20.3269080940089,-15.1076549413947)) ;
#34655 = CARTESIAN_POINT('Ctrl Pts',(-9.18633668357024,20.1379053643401,-15.0970730344294)) ;
#34656 = CARTESIAN_POINT('Ctrl Pts',(-9.60620958610337,19.9356636821395,-15.0865551989198)) ;
#34657 = CARTESIAN_POINT('Ctrl Pts',(-10.0071470463981,19.7425427021048,-15.0765116971086)) ;
#34658 = CARTESIAN_POINT('Ctrl Pts',(-10.4022619996847,19.5373560485768,-15.0665226768525)) ;
#34659 = CARTESIAN_POINT('Ctrl Pts',(-10.7908189811037,19.3204671517673,-15.0565542326806)) ;
#34660 = CARTESIAN_POINT('Ctrl Pts',(-11.1793933598962,19.1035685439055,-15.0465853421784)) ;
#34661 = CARTESIAN_POINT('Ctrl Pts',(-11.561409132193,18.8749665165229,-15.0366369133088)) ;
#34662 = CARTESIAN_POINT('Ctrl Pts',(-11.9361448444259,18.6350622832329,-15.0266536452525)) ;
#34663 = CARTESIAN_POINT('Ctrl Pts',(-12.3109428287427,18.3951181836155,-15.0166687182166)) ;
#34664 = CARTESIAN_POINT('Ctrl Pts',(-12.678458230161,18.1438679522468,-15.006648764924)) ;
#34665 = CARTESIAN_POINT('Ctrl Pts',(-13.0379844648463,17.8817529898452,-14.9965192410308)) ;
#34666 = CARTESIAN_POINT('Ctrl Pts',(-13.0888208267137,17.8446904063839,-14.9950869446015)) ;
#34667 = CARTESIAN_POINT('Ctrl Pts',(-13.1394974841268,17.8074106672942,-14.9936524288434)) ;
#34668 = CARTESIAN_POINT('Ctrl Pts',(-13.190012466339,17.7699150881616,-14.9922154555409)) ;
#34669 = CARTESIAN_POINT('Ctrl Pts',(-13.556826282387,17.4976414801302,-14.9817808945932)) ;
#34670 = CARTESIAN_POINT('Ctrl Pts',(-13.9152061005742,17.2139130798917,-14.9712164246814)) ;
#34671 = CARTESIAN_POINT('Ctrl Pts',(-14.2644725010906,16.9193190259568,-14.9606073316696)) ;
#34672 = CARTESIAN_POINT('Ctrl Pts',(-14.6045863502757,16.6324448305496,-14.9502762507089)) ;
#34673 = CARTESIAN_POINT('Ctrl Pts',(-14.9360584492507,16.3352672232955,-14.9399029257363)) ;
#34674 = CARTESIAN_POINT('Ctrl Pts',(-15.2582944657499,16.028356282535,-14.929545682811)) ;
#34675 = CARTESIAN_POINT('Ctrl Pts',(-15.5804973480705,15.7214769001399,-14.9191895048776)) ;
#34676 = CARTESIAN_POINT('Ctrl Pts',(-15.8934661496102,15.4048662356502,-14.9088495004071)) ;
#34677 = CARTESIAN_POINT('Ctrl Pts',(-16.1966375223475,15.0791186849163,-14.8985619330411)) ;
#34678 = CARTESIAN_POINT('Ctrl Pts',(-16.4997908078651,14.7533905682978,-14.8882749794318)) ;
#34679 = CARTESIAN_POINT('Ctrl Pts',(-16.7931479375089,14.4185266033491,-14.878040497363)) ;
#34680 = CARTESIAN_POINT('Ctrl Pts',(-17.0761724647569,14.0751431834048,-14.8678736674933)) ;
#34681 = CARTESIAN_POINT('Ctrl Pts',(-17.3725923864151,13.7155076160272,-14.8572256471864)) ;
#34682 = CARTESIAN_POINT('Ctrl Pts',(-17.6576895078092,13.3465357073017,-14.8466437404107)) ;
#34683 = CARTESIAN_POINT('Ctrl Pts',(-17.9308711478129,12.9689555842401,-14.8361259046928)) ;
#34684 = CARTESIAN_POINT('Ctrl Pts',(-18.191732825452,12.6084035927385,-14.8260824029755)) ;
#34685 = CARTESIAN_POINT('Ctrl Pts',(-18.4417346834897,12.2400064517195,-14.8160933828175)) ;
#34686 = CARTESIAN_POINT('Ctrl Pts',(-18.6804025706626,11.864433616645,-14.806124938755)) ;
#34687 = CARTESIAN_POINT('Ctrl Pts',(-18.9190811440305,11.4888439655482,-14.796156048362)) ;
#34688 = CARTESIAN_POINT('Ctrl Pts',(-19.1464246288981,11.1060778874681,-14.7862076196129)) ;
#34689 = CARTESIAN_POINT('Ctrl Pts',(-19.3619891674588,10.7168314124428,-14.7762243516947)) ;
#34690 = CARTESIAN_POINT('Ctrl Pts',(-19.5775895276811,10.3275202539795,-14.7662394247966)) ;
#34691 = CARTESIAN_POINT('Ctrl Pts',(-19.781406855353,9.93172644478167,-14.7562194716594)) ;
#34692 = CARTESIAN_POINT('Ctrl Pts',(-19.9730294843648,9.53017429574671,-14.7460899479446)) ;
#34693 = CARTESIAN_POINT('Ctrl Pts',(-20.00012459641,9.47339550857423,-14.744657650614)) ;
#34694 = CARTESIAN_POINT('Ctrl Pts',(-20.0269759496543,9.41650163921464,-14.7432231339523)) ;
#34695 = CARTESIAN_POINT('Ctrl Pts',(-20.053582436078,9.35949478216512,-14.7417861597431)) ;
#34696 = CARTESIAN_POINT('Ctrl Pts',(-20.2467849324901,8.9455405711805,-14.7313515987845)) ;
#34697 = CARTESIAN_POINT('Ctrl Pts',(-20.427120813459,8.52552048915342,-14.7207871288741)) ;
#34698 = CARTESIAN_POINT('Ctrl Pts',(-20.594272565392,8.10027589246691,-14.7101780358706)) ;
#34699 = CARTESIAN_POINT('Ctrl Pts',(-20.7570440954759,7.68617485635989,-14.699846954796)) ;
#34700 = CARTESIAN_POINT('Ctrl Pts',(-20.9073137907143,7.26711960221349,-14.6894736297151)) ;
#34701 = CARTESIAN_POINT('Ctrl Pts',(-21.0448299240249,6.84389425607836,-14.6791163866848)) ;
#34702 = CARTESIAN_POINT('Ctrl Pts',(-21.18233191714,6.42071242839394,-14.6687602086454)) ;
#34703 = CARTESIAN_POINT('Ctrl Pts',(-21.3070830847419,5.99336136141939,-14.6584202040724)) ;
#34704 = CARTESIAN_POINT('Ctrl Pts',(-21.4188705204252,5.56263183850919,-14.6481326366048)) ;
#34705 = CARTESIAN_POINT('Ctrl Pts',(-21.5306512868717,5.13192801291597,-14.6378456828932)) ;
#34706 = CARTESIAN_POINT('Ctrl Pts',(-21.6294699347588,4.69784603908703,-14.6276112007232)) ;
#34707 = CARTESIAN_POINT('Ctrl Pts',(-21.7151476835065,4.26118325832356,-14.6174443707622)) ;
#34708 = CARTESIAN_POINT('Ctrl Pts',(-21.8048805109009,3.80385347890562,-14.6067963505777)) ;
#34709 = CARTESIAN_POINT('Ctrl Pts',(-21.8802129037667,3.34369517484707,-14.5962144438847)) ;
#34710 = CARTESIAN_POINT('Ctrl Pts',(-21.9409697473836,2.88163072060197,-14.5856966082665)) ;
#34711 = CARTESIAN_POINT('Ctrl Pts',(-21.9989865763307,2.44040446840396,-14.5756531064382)) ;
#34712 = CARTESIAN_POINT('Ctrl Pts',(-22.0437193846154,1.99744130624142,-14.5656640861658)) ;
#34713 = CARTESIAN_POINT('Ctrl Pts',(-22.0750694257953,1.5535556291076,-14.5556956419838)) ;
#34714 = CARTESIAN_POINT('Ctrl Pts',(-22.1064208706525,1.10965007728892,-14.5457267514713)) ;
#34715 = CARTESIAN_POINT('Ctrl Pts',(-22.12438821669,0.664821897241222,-14.5357783225975)) ;
#34716 = CARTESIAN_POINT('Ctrl Pts',(-22.1289120038117,0.219894455284174,
-14.5257950545478)) ;
#34717 = CARTESIAN_POINT('Ctrl Pts',(-22.1334365426781,-0.225106922927372,
-14.5158101275186)) ;
#34718 = CARTESIAN_POINT('Ctrl Pts',(-22.1245128562186,-0.670207602470856,
-14.5057901742436)) ;
#34719 = CARTESIAN_POINT('Ctrl Pts',(-22.1021232519658,-1.11457464741053,
-14.4956606503828)) ;
#34720 = CARTESIAN_POINT('Ctrl Pts',(-22.0989574016564,-1.17740735900297,
-14.4942283536844)) ;
#34721 = CARTESIAN_POINT('Ctrl Pts',(-22.0955223923823,-1.2402253877673,-14.4927938376568)) ;
#34722 = CARTESIAN_POINT('Ctrl Pts',(-22.0918182454677,-1.30302636428287,
-14.491356864084)) ;
#34723 = CARTESIAN_POINT('Ctrl Pts',(-22.064920640979,-1.75905466627196,-14.4809223031142)) ;
#34724 = CARTESIAN_POINT('Ctrl Pts',(-22.0238197949282,-2.21430033586412,
-14.4703578331927)) ;
#34725 = CARTESIAN_POINT('Ctrl Pts',(-21.9686365006969,-2.66787224769554,
-14.4597487401799)) ;
#34726 = CARTESIAN_POINT('Ctrl Pts',(-21.9148992883904,-3.10955827717089,
-14.4494176591608)) ;
#34727 = CARTESIAN_POINT('Ctrl Pts',(-21.8478083741637,-3.54965723659662,
-14.4390443341377)) ;
#34728 = CARTESIAN_POINT('Ctrl Pts',(-21.7675152072097,-3.98735963025754,
-14.4286870911672)) ;
#34729 = CARTESIAN_POINT('Ctrl Pts',(-21.6872302964613,-4.42501701683854,
-14.4183309131881)) ;
#34730 = CARTESIAN_POINT('Ctrl Pts',(-21.5937459456807,-4.86027838884591,
-14.4079909086775)) ;
#34731 = CARTESIAN_POINT('Ctrl Pts',(-21.4872509200593,-5.29234685536064,
-14.3977033412744)) ;
#34732 = CARTESIAN_POINT('Ctrl Pts',(-21.3807622479327,-5.7243895446642,-14.3874163876277)) ;
#34733 = CARTESIAN_POINT('Ctrl Pts',(-21.2612644665466,-6.15323982502812,
-14.3771819055247)) ;
#34734 = CARTESIAN_POINT('Ctrl Pts',(-21.1289794797663,-6.5781112650732,-14.3670150756742)) ;
#34735 = CARTESIAN_POINT('Ctrl Pts',(-20.9904335190314,-7.0230916311942,-14.3563670554903)) ;
#34736 = CARTESIAN_POINT('Ctrl Pts',(-20.8378745514713,-7.46371210013524,
-14.345785148674)) ;
#34737 = CARTESIAN_POINT('Ctrl Pts',(-20.6715871649445,-7.89907799341329,
-14.3352673130205)) ;
#34738 = CARTESIAN_POINT('Ctrl Pts',(-20.5127990156401,-8.31480973295033,
-14.3252238112674)) ;
#34739 = CARTESIAN_POINT('Ctrl Pts',(-20.3414990733482,-8.7257522039684,-14.3152347910721)) ;
#34740 = CARTESIAN_POINT('Ctrl Pts',(-20.1579877570251,-9.13114203336038,
-14.3052663469689)) ;
#34741 = CARTESIAN_POINT('Ctrl Pts',(-19.9744682241009,-9.5365500138209,-14.295297456535)) ;
#34742 = CARTESIAN_POINT('Ctrl Pts',(-19.7787360917902,-9.93640481898993,
-14.2853490277415)) ;
#34743 = CARTESIAN_POINT('Ctrl Pts',(-19.5711306051236,-10.3299538663865,
-14.2753657597736)) ;
#34744 = CARTESIAN_POINT('Ctrl Pts',(-19.3634906194045,-10.7235683121954,
-14.265380832826)) ;
#34745 = CARTESIAN_POINT('Ctrl Pts',(-19.1439731555917,-11.110874815802,-14.2553608796341)) ;
#34746 = CARTESIAN_POINT('Ctrl Pts',(-18.9129587520637,-11.491132239014,-14.2452313558577)) ;
#34747 = CARTESIAN_POINT('Ctrl Pts',(-18.8802937175048,-11.5448999767862,
-14.243799058827)) ;
#34748 = CARTESIAN_POINT('Ctrl Pts',(-18.8473988890757,-11.5985267997651,
-14.2423645424659)) ;
#34749 = CARTESIAN_POINT('Ctrl Pts',(-18.814275412313,-11.6520106337357,-14.2409275685585)) ;
#34750 = CARTESIAN_POINT('Ctrl Pts',(-18.5737498637265,-12.0403825609475,
-14.2304930076016)) ;
#34751 = CARTESIAN_POINT('Ctrl Pts',(-18.3211020605776,-12.4213116708992,
-14.2199285376896)) ;
#34752 = CARTESIAN_POINT('Ctrl Pts',(-18.0568620376773,-12.7940714936667,
-14.2093194446831)) ;
#34753 = CARTESIAN_POINT('Ctrl Pts',(-17.7995464416389,-13.1570631212096,
-14.1989883636437)) ;
#34754 = CARTESIAN_POINT('Ctrl Pts',(-17.5312384715473,-13.5123082746593,
-14.1886150385969)) ;
#34755 = CARTESIAN_POINT('Ctrl Pts',(-17.252456310858,-13.8591668711441,-14.1782577956)) ;
#34756 = CARTESIAN_POINT('Ctrl Pts',(-16.9737028161546,-14.2059898016321,
-14.1679016175944)) ;
#34757 = CARTESIAN_POINT('Ctrl Pts',(-16.6844773430316,-14.5444279976077,
-14.1575616130545)) ;
#34758 = CARTESIAN_POINT('Ctrl Pts',(-16.3853249072146,-14.873870210102,-14.1472740456199)) ;
#34759 = CARTESIAN_POINT('Ctrl Pts',(-16.0861903188295,-15.2032927680765,
-14.1369870919415)) ;
#34760 = CARTESIAN_POINT('Ctrl Pts',(-15.77712990884,-15.5237205238918,-14.1267526098046)) ;
#34761 = CARTESIAN_POINT('Ctrl Pts',(-15.4587128707131,-15.8345671888533,
-14.1165857798786)) ;
#34762 = CARTESIAN_POINT('Ctrl Pts',(-15.1252253348865,-16.1601260500491,
-14.1059377596624)) ;
#34763 = CARTESIAN_POINT('Ctrl Pts',(-14.781484058204,-16.4751856795172,-14.0953558529352)) ;
#34764 = CARTESIAN_POINT('Ctrl Pts',(-14.4281648535965,-16.7790943743333,
-14.0848380172876)) ;
#34765 = CARTESIAN_POINT('Ctrl Pts',(-14.090779655408,-17.0692973802685,-14.0747945154959)) ;
#34766 = CARTESIAN_POINT('Ctrl Pts',(-13.7446655050044,-17.3493373427742,
-14.0648054952612)) ;
#34767 = CARTESIAN_POINT('Ctrl Pts',(-13.3904496993175,-17.6186855950221,
-14.0548370511184)) ;
#34768 = CARTESIAN_POINT('Ctrl Pts',(-13.0362180338587,-17.8880459071547,
-14.0448681606453)) ;
#34769 = CARTESIAN_POINT('Ctrl Pts',(-12.67388388897,-18.1467134568534,-14.0349197318125)) ;
#34770 = CARTESIAN_POINT('Ctrl Pts',(-12.3041035849764,-18.3941875334039,
-14.0249364638055)) ;
#34771 = CARTESIAN_POINT('Ctrl Pts',(-11.9342618323657,-18.6417027342102,
-14.0149515368189)) ;
#34772 = CARTESIAN_POINT('Ctrl Pts',(-11.5569713318479,-18.8780205792078,
-14.0049315835884)) ;
#34773 = CARTESIAN_POINT('Ctrl Pts',(-11.1729192867255,-19.1026700621272,
-13.9948020597743)) ;
#34774 = CARTESIAN_POINT('Ctrl Pts',(-11.1186150012861,-19.1344351049104,
-13.9933697628771)) ;
#34775 = CARTESIAN_POINT('Ctrl Pts',(-11.0641755806956,-19.1659669081917,
-13.9919352466501)) ;
#34776 = CARTESIAN_POINT('Ctrl Pts',(-11.0096030190606,-19.1972641920671,
-13.9904982728772)) ;
#34777 = CARTESIAN_POINT('Ctrl Pts',(-10.613325277484,-19.4245288943289,-13.9800637119116)) ;
#34778 = CARTESIAN_POINT('Ctrl Pts',(-10.2099231501165,-19.6394815004455,
-13.969499241994)) ;
#34779 = CARTESIAN_POINT('Ctrl Pts',(-9.80020837513221,-19.8417350006139,
-13.9588901489843)) ;
#34780 = CARTESIAN_POINT('Ctrl Pts',(-9.40123020254088,-20.0386884346229,
-13.9485590679486)) ;
#34781 = CARTESIAN_POINT('Ctrl Pts',(-8.99626599144153,-20.2235999630236,
-13.938185742908)) ;
#34782 = CARTESIAN_POINT('Ctrl Pts',(-8.58607597318324,-20.3961529338449,
-13.9278284999193)) ;
#34783 = CARTESIAN_POINT('Ctrl Pts',(-8.17592813301714,-20.5686881617793,
-13.9174723219217)) ;
#34784 = CARTESIAN_POINT('Ctrl Pts',(-7.76055556505427,-20.7288674873255,
-13.9071323173917)) ;
#34785 = CARTESIAN_POINT('Ctrl Pts',(-7.34072839274776,-20.8764123834507,
-13.8968447499685)) ;
#34786 = CARTESIAN_POINT('Ctrl Pts',(-6.92092626733406,-21.023948477046,-13.8865577963017)) ;
#34787 = CARTESIAN_POINT('Ctrl Pts',(-6.49666997960255,-21.1588517230617,
-13.8763233141777)) ;
#34788 = CARTESIAN_POINT('Ctrl Pts',(-6.06873905204388,-21.2808770494131,
-13.8661564842907)) ;
#34789 = CARTESIAN_POINT('Ctrl Pts',(-5.62055439605247,-21.4086777653488,
-13.8555084641033)) ;
#34790 = CARTESIAN_POINT('Ctrl Pts',(-5.16834254152024,-21.5223662618714,
-13.8449265573283)) ;
#34791 = CARTESIAN_POINT('Ctrl Pts',(-4.71300791056191,-21.6216906253759,
-13.8344087216846)) ;
#34792 = CARTESIAN_POINT('Ctrl Pts',(-4.2782079830875,-21.7165356538712,-13.8243652199078)) ;
#34793 = CARTESIAN_POINT('Ctrl Pts',(-3.84056232262998,-21.7982893164388,
-13.8143761996884)) ;
#34794 = CARTESIAN_POINT('Ctrl Pts',(-3.40087416261841,-21.866784861429,-13.8044077555605)) ;
#34795 = CARTESIAN_POINT('Ctrl Pts',(-2.96116631586805,-21.9352834732607,
-13.7944388651022)) ;
#34796 = CARTESIAN_POINT('Ctrl Pts',(-2.51941574493279,-21.9905226500052,
-13.7844904362839)) ;
#34797 = CARTESIAN_POINT('Ctrl Pts',(-2.07643792028521,-22.0323740347578,
-13.7745071682909)) ;
#34798 = CARTESIAN_POINT('Ctrl Pts',(-1.63338648334986,-22.0742323742065,
-13.7645222413182)) ;
#34799 = CARTESIAN_POINT('Ctrl Pts',(-1.18910736175828,-22.1026982750266,
-13.7545022881008)) ;
#34800 = CARTESIAN_POINT('Ctrl Pts',(-0.744429067465207,-22.11768419737,-13.7443727642986)) ;
#34801 = CARTESIAN_POINT('Ctrl Pts',(-0.681552335208617,-22.1198031805515,
-13.7429404673681)) ;
#34802 = CARTESIAN_POINT('Ctrl Pts',(-0.61866764297327,-22.1216527220511,
-13.7415059511075)) ;
#34803 = CARTESIAN_POINT('Ctrl Pts',(-0.55577735361064,-22.1232326442476,
-13.7400689773009)) ;
#34804 = CARTESIAN_POINT('Ctrl Pts',(-0.37061492733742,-22.1278842721889,
-13.7358382199103)) ;
#34805 = CARTESIAN_POINT('Ctrl Pts',(-0.185394205576265,-22.1301988329937,
-13.7315860326588)) ;
#34806 = CARTESIAN_POINT('Ctrl Pts',(-0.000170111177784315,-22.1301789835866,
-13.7273184261236)) ;
#34807 = CARTESIAN_POINT('Ctrl Pts',(-0.000192018545400235,-22.1301832392792,
-13.2601742013415)) ;
#34808 = CARTESIAN_POINT('Ctrl Pts',(-0.17280475386243,-22.1302004171725,
-13.2640845203255)) ;
#34809 = CARTESIAN_POINT('Ctrl Pts',(-0.34541413006999,-22.1281900578278,
-13.2680085775377)) ;
#34810 = CARTESIAN_POINT('Ctrl Pts',(-0.517975506591968,-22.1241500110886,
-13.2719512513423)) ;
#34811 = CARTESIAN_POINT('Ctrl Pts',(-0.974671214221961,-22.1134577458689,
-13.2823858123052)) ;
#34812 = CARTESIAN_POINT('Ctrl Pts',(-1.43108897853208,-22.0885434086334,
-13.2929502822213)) ;
#34813 = CARTESIAN_POINT('Ctrl Pts',(-1.8863339478131,-22.0494960828901,-13.3035593752302)) ;
#34814 = CARTESIAN_POINT('Ctrl Pts',(-2.3296491930147,-22.0114719948618,-13.3138904562656)) ;
#34815 = CARTESIAN_POINT('Ctrl Pts',(-2.77185240675326,-21.9600462825204,
-13.3242637813067)) ;
#34816 = CARTESIAN_POINT('Ctrl Pts',(-3.21212922727595,-21.8953415636052,
-13.3346210242967)) ;
#34817 = CARTESIAN_POINT('Ctrl Pts',(-3.65236077600423,-21.8306434980013,
-13.3449772022954)) ;
#34818 = CARTESIAN_POINT('Ctrl Pts',(-4.09066638251384,-21.7526692563123,
-13.3553172068271)) ;
#34819 = CARTESIAN_POINT('Ctrl Pts',(-4.5262429572339,-21.6615791962104,-13.3656047742524)) ;
#34820 = CARTESIAN_POINT('Ctrl Pts',(-4.96179354545244,-21.570494570542,-13.3758917279215)) ;
#34821 = CARTESIAN_POINT('Ctrl Pts',(-5.39461557736581,-21.4662956991814,
-13.3861262100481)) ;
#34822 = CARTESIAN_POINT('Ctrl Pts',(-5.82391466313536,-21.3491747257555,
-13.3962920035461)) ;
#34823 = CARTESIAN_POINT('Ctrl Pts',(-6.27353223145597,-21.2265104830011,
-13.4069389382919)) ;
#34824 = CARTESIAN_POINT('Ctrl Pts',(-6.71929162805928,-21.0896926339765,
-13.417522966905)) ;
#34825 = CARTESIAN_POINT('Ctrl Pts',(-7.16028609751094,-20.9389649531089,
-13.4280408025512)) ;
#34826 = CARTESIAN_POINT('Ctrl Pts',(-7.58139257681946,-20.795034796562,-13.4380843043312)) ;
#34827 = CARTESIAN_POINT('Ctrl Pts',(-7.99815695782829,-20.6384307203011,
-13.4480733245541)) ;
#34828 = CARTESIAN_POINT('Ctrl Pts',(-8.40980568409793,-20.4694258552265,
-13.4580417686853)) ;
#34829 = CARTESIAN_POINT('Ctrl Pts',(-8.82147284165773,-20.3004134230746,
-13.4680106591467)) ;
#34830 = CARTESIAN_POINT('Ctrl Pts',(-9.22802385464807,-20.1189989585829,
-13.4779590879682)) ;
#34831 = CARTESIAN_POINT('Ctrl Pts',(-9.62869457218019,-19.9254947773076,
-13.4879423559642)) ;
#34832 = CARTESIAN_POINT('Ctrl Pts',(-10.0294318715792,-19.7319584402767,
-13.4979272829399)) ;
#34833 = CARTESIAN_POINT('Ctrl Pts',(-10.4242868388537,-19.5263281877794,
-13.5079472361601)) ;
#34834 = CARTESIAN_POINT('Ctrl Pts',(-10.8125052943334,-19.3089580089504,
-13.5180767599648)) ;
#34835 = CARTESIAN_POINT('Ctrl Pts',(-10.86739870413,-19.2782222463004,-13.519509056893)) ;
#34836 = CARTESIAN_POINT('Ctrl Pts',(-10.922159445338,-19.2472518323632,-13.5209435731512)) ;
#34837 = CARTESIAN_POINT('Ctrl Pts',(-10.9767854043858,-19.2160478383213,
-13.5223805469554)) ;
#34838 = CARTESIAN_POINT('Ctrl Pts',(-11.3734508816389,-18.9894605636156,
-13.5328151079184)) ;
#34839 = CARTESIAN_POINT('Ctrl Pts',(-11.7631085562476,-18.7504944647731,
-13.5433795778345)) ;
#34840 = CARTESIAN_POINT('Ctrl Pts',(-12.1450136006463,-18.4996534538397,
-13.5539886708435)) ;
#34841 = CARTESIAN_POINT('Ctrl Pts',(-12.5169107984637,-18.2553857479478,
-13.5643197518786)) ;
#34842 = CARTESIAN_POINT('Ctrl Pts',(-12.881456618974,-17.9998576069013,-13.5746930769196)) ;
#34843 = CARTESIAN_POINT('Ctrl Pts',(-13.2379929879246,-17.7335641654828,
-13.5850503199094)) ;
#34844 = CARTESIAN_POINT('Ctrl Pts',(-13.5944926957544,-17.4672981058882,
-13.5954064979078)) ;
#34845 = CARTESIAN_POINT('Ctrl Pts',(-13.942984694799,-17.1902690214,-13.6057465024393)) ;
#34846 = CARTESIAN_POINT('Ctrl Pts',(-14.2828387740266,-16.9029998857225,
-13.6160340698645)) ;
#34847 = CARTESIAN_POINT('Ctrl Pts',(-14.6226725775584,-16.6157478885228,
-13.6263210235333)) ;
#34848 = CARTESIAN_POINT('Ctrl Pts',(-14.9538696274581,-16.3182569975224,
-13.6365555056598)) ;
#34849 = CARTESIAN_POINT('Ctrl Pts',(-15.2758224815446,-16.0110740110271,
-13.6467212991572)) ;
#34850 = CARTESIAN_POINT('Ctrl Pts',(-15.613013181862,-15.6893522277684,-13.657368233903)) ;
#34851 = CARTESIAN_POINT('Ctrl Pts',(-15.9400791509408,-15.3570144246928,
-13.6679522625174)) ;
#34852 = CARTESIAN_POINT('Ctrl Pts',(-16.2563386528229,-15.0147062545501,
-13.678470098164)) ;
#34853 = CARTESIAN_POINT('Ctrl Pts',(-16.5583354682104,-14.6878355150181,
-13.6885135999438)) ;
#34854 = CARTESIAN_POINT('Ctrl Pts',(-16.8504855116544,-14.3518805506525,
-13.6985026201664)) ;
#34855 = CARTESIAN_POINT('Ctrl Pts',(-17.1322381813423,-14.0074494960581,
-13.7084710642973)) ;
#34856 = CARTESIAN_POINT('Ctrl Pts',(-17.4140034663123,-13.6630030197999,
-13.7184399547584)) ;
#34857 = CARTESIAN_POINT('Ctrl Pts',(-17.6853703552699,-13.3100795923354,
-13.7283883835796)) ;
#34858 = CARTESIAN_POINT('Ctrl Pts',(-17.9458151546047,-12.9493173457743,
-13.7383716515752)) ;
#34859 = CARTESIAN_POINT('Ctrl Pts',(-18.2063032336216,-12.5884951491763,
-13.7483565785506)) ;
#34860 = CARTESIAN_POINT('Ctrl Pts',(-18.4558654347015,-12.2198314084818,
-13.7583765317704)) ;
#34861 = CARTESIAN_POINT('Ctrl Pts',(-18.6940066536534,-11.8439961737811,
-13.7685060555746)) ;
#34862 = CARTESIAN_POINT('Ctrl Pts',(-18.7276794050476,-11.7908537296509,
-13.7699383525045)) ;
#34863 = CARTESIAN_POINT('Ctrl Pts',(-18.761123861049,-11.7375679558486,-13.7713728687645)) ;
#34864 = CARTESIAN_POINT('Ctrl Pts',(-18.7943386717719,-11.6841407997898,
-13.7728098425704)) ;
#34865 = CARTESIAN_POINT('Ctrl Pts',(-19.0355274574803,-11.2961804106372,
-13.7832444035333)) ;
#34866 = CARTESIAN_POINT('Ctrl Pts',(-19.2646648130735,-10.9006630632944,
-13.7938088734492)) ;
#34867 = CARTESIAN_POINT('Ctrl Pts',(-19.4813351570666,-10.4983862459944,
-13.804417966458)) ;
#34868 = CARTESIAN_POINT('Ctrl Pts',(-19.6923276405839,-10.1066511188915,
-13.8147490474935)) ;
#34869 = CARTESIAN_POINT('Ctrl Pts',(-19.8914983044428,-9.70850625480636,
-13.8251223725349)) ;
#34870 = CARTESIAN_POINT('Ctrl Pts',(-20.0785037090679,-9.30470016521747,
-13.835479615525)) ;
#34871 = CARTESIAN_POINT('Ctrl Pts',(-20.2654898847221,-8.90093559729271,
-13.8458357935238)) ;
#34872 = CARTESIAN_POINT('Ctrl Pts',(-20.4403134163448,-8.49151097680173,
-13.8561757980556)) ;
#34873 = CARTESIAN_POINT('Ctrl Pts',(-20.6026686141136,-8.07718605447576,
-13.8664633654812)) ;
#34874 = CARTESIAN_POINT('Ctrl Pts',(-20.7650141257705,-7.66288585077699,
-13.8767503191504)) ;
#34875 = CARTESIAN_POINT('Ctrl Pts',(-20.914892879849,-7.2436858088065,-13.8869848012772)) ;
#34876 = CARTESIAN_POINT('Ctrl Pts',(-21.0520305458122,-6.82035580981904,
-13.8971505947757)) ;
#34877 = CARTESIAN_POINT('Ctrl Pts',(-21.1956588598171,-6.37698984179532,
-13.9077975295215)) ;
#34878 = CARTESIAN_POINT('Ctrl Pts',(-21.3253321166679,-5.92909988888031,
-13.918381558134)) ;
#34879 = CARTESIAN_POINT('Ctrl Pts',(-21.4407576405948,-5.47757812386213,
-13.92889939378)) ;
#34880 = CARTESIAN_POINT('Ctrl Pts',(-21.5509776986048,-5.04641910946049,
-13.9389428955603)) ;
#34881 = CARTESIAN_POINT('Ctrl Pts',(-21.6482156614984,-4.61195142992625,
-13.9489319157834)) ;
#34882 = CARTESIAN_POINT('Ctrl Pts',(-21.7322763690278,-4.1749718929724,-13.9589003599148)) ;
#34883 = CARTESIAN_POINT('Ctrl Pts',(-21.8163408403181,-3.73797279055698,
-13.9688692503766)) ;
#34884 = CARTESIAN_POINT('Ctrl Pts',(-21.8872267475388,-3.29846155946272,
-13.9788176791983)) ;
#34885 = CARTESIAN_POINT('Ctrl Pts',(-21.9447768665892,-2.85724859969611,
-13.9888009471946)) ;
#34886 = CARTESIAN_POINT('Ctrl Pts',(-22.0023365490894,-2.41596232091478,
-13.9987858741707)) ;
#34887 = CARTESIAN_POINT('Ctrl Pts',(-22.0465558150088,-1.97297371783978,
-14.0088058273912)) ;
#34888 = CARTESIAN_POINT('Ctrl Pts',(-22.0773177686225,-1.52910767268793,
-14.0189353511962)) ;
#34889 = CARTESIAN_POINT('Ctrl Pts',(-22.0816674549924,-1.46634579121217,
-14.0203676481231)) ;
#34890 = CARTESIAN_POINT('Ctrl Pts',(-22.0857481520724,-1.40356638996004,
-14.0218021643801)) ;
#34891 = CARTESIAN_POINT('Ctrl Pts',(-22.0895595984754,-1.34077182398876,
-14.0232391381831)) ;
#34892 = CARTESIAN_POINT('Ctrl Pts',(-22.1172363520578,-0.884790145393343,
-14.0336736991461)) ;
#34893 = CARTESIAN_POINT('Ctrl Pts',(-22.1307178879002,-0.427891745342189,
-14.0442381690622)) ;
#34894 = CARTESIAN_POINT('Ctrl Pts',(-22.1300178686683,0.0290242049999805,
-14.0548472620713)) ;
#34895 = CARTESIAN_POINT('Ctrl Pts',(-22.129336193486,0.47396664305618,-14.0651783431059)) ;
#34896 = CARTESIAN_POINT('Ctrl Pts',(-22.1152068468041,0.918925795854455,
-14.0755516681463)) ;
#34897 = CARTESIAN_POINT('Ctrl Pts',(-22.0876836628607,1.36307988358833,-14.0859089111354)) ;
#34898 = CARTESIAN_POINT('Ctrl Pts',(-22.0601633090093,1.80718830084565,-14.0962650891334)) ;
#34899 = CARTESIAN_POINT('Ctrl Pts',(-22.0192519762506,2.25049186487643,-14.1066050936642)) ;
#34900 = CARTESIAN_POINT('Ctrl Pts',(-21.9650420516846,2.69217686070395,-14.1168926610888)) ;
#34901 = CARTESIAN_POINT('Ctrl Pts',(-21.910835361283,3.13383550560166,-14.127179614757)) ;
#34902 = CARTESIAN_POINT('Ctrl Pts',(-21.8433316861536,3.57387592410145,-14.1374140968829)) ;
#34903 = CARTESIAN_POINT('Ctrl Pts',(-21.7626558173783,4.01149040240759,-14.1475798903798)) ;
#34904 = CARTESIAN_POINT('Ctrl Pts',(-21.6781616054206,4.46981692615091,-14.1582268251261)) ;
#34905 = CARTESIAN_POINT('Ctrl Pts',(-21.5792399048857,4.92548682932996,-14.1688108537404)) ;
#34906 = CARTESIAN_POINT('Ctrl Pts',(-21.4660575244286,5.3775760955686,-14.1793286893873)) ;
#34907 = CARTESIAN_POINT('Ctrl Pts',(-21.3579794485149,5.80927701791184,-14.1893721911665)) ;
#34908 = CARTESIAN_POINT('Ctrl Pts',(-21.236907732684,6.23771490789214,-14.1993612113885)) ;
#34909 = CARTESIAN_POINT('Ctrl Pts',(-21.1030496181128,6.66209601419537,-14.2093296555187)) ;
#34910 = CARTESIAN_POINT('Ctrl Pts',(-20.9691855101354,7.08649612187432,-14.2192985459793)) ;
#34911 = CARTESIAN_POINT('Ctrl Pts',(-20.8225337231665,7.5068390621459,-14.2292469747998)) ;
#34912 = CARTESIAN_POINT('Ctrl Pts',(-20.663341334201,7.92233716722134,-14.2392302427949)) ;
#34913 = CARTESIAN_POINT('Ctrl Pts',(-20.5041224912775,8.33790431811922,-14.2492151697698)) ;
#34914 = CARTESIAN_POINT('Ctrl Pts',(-20.332358691548,8.74862495674422,-14.259235122989)) ;
#34915 = CARTESIAN_POINT('Ctrl Pts',(-20.1483393754432,9.15371785360323,-14.2693646467927)) ;
#34916 = CARTESIAN_POINT('Ctrl Pts',(-20.1223193662966,9.21099728004941,-14.2707969437254)) ;
#34917 = CARTESIAN_POINT('Ctrl Pts',(-20.0960543987149,9.26816420073129,-14.2722314599881)) ;
#34918 = CARTESIAN_POINT('Ctrl Pts',(-20.0695453627053,9.32521641962857,-14.2736684337969)) ;
#34919 = CARTESIAN_POINT('Ctrl Pts',(-19.8770504469171,9.73950014040196,-14.2841029947598)) ;
#34920 = CARTESIAN_POINT('Ctrl Pts',(-19.6716322081881,10.1478397624984,-14.2946674646759)) ;
#34921 = CARTESIAN_POINT('Ctrl Pts',(-19.4537302657956,10.5494507922323,-14.305276557685)) ;
#34922 = CARTESIAN_POINT('Ctrl Pts',(-19.2415384579781,10.9405375788069,-14.3156076387216)) ;
#34923 = CARTESIAN_POINT('Ctrl Pts',(-19.0175089331266,11.3252440359465,-14.325980963764)) ;
#34924 = CARTESIAN_POINT('Ctrl Pts',(-18.7820798455872,11.7028728538607,-14.3363382067553)) ;
#34925 = CARTESIAN_POINT('Ctrl Pts',(-18.5466749662204,12.0804628418083,-14.3466943847554)) ;
#34926 = CARTESIAN_POINT('Ctrl Pts',(-18.2998729378895,12.4509767361701,-14.3570343892884)) ;
#34927 = CARTESIAN_POINT('Ctrl Pts',(-18.0421419942429,12.8137426554905,-14.3673219567152)) ;
#34928 = CARTESIAN_POINT('Ctrl Pts',(-17.7844264268254,13.1764869321948,-14.3776089103856)) ;
#34929 = CARTESIAN_POINT('Ctrl Pts',(-17.5157831952769,13.5314842987859,-14.3878433925137)) ;
#34930 = CARTESIAN_POINT('Ctrl Pts',(-17.2367061848117,13.8780835626764,-14.3980091860119)) ;
#34931 = CARTESIAN_POINT('Ctrl Pts',(-16.9444206175783,14.2410871733287,-14.408656120756)) ;
#34932 = CARTESIAN_POINT('Ctrl Pts',(-16.6407067022616,14.5948927994589,-14.4192401493713)) ;
#34933 = CARTESIAN_POINT('Ctrl Pts',(-16.3261505940965,14.9387669198136,-14.4297579850172)) ;
#34934 = CARTESIAN_POINT('Ctrl Pts',(-16.0257803526236,15.267132988334,-14.4398014867987)) ;
#34935 = CARTESIAN_POINT('Ctrl Pts',(-15.7155314827287,15.5864494845368,-14.4497905070229)) ;
#34936 = CARTESIAN_POINT('Ctrl Pts',(-15.3959637602158,15.896116707577,-14.4597589511553)) ;
#34937 = CARTESIAN_POINT('Ctrl Pts',(-15.0763817292767,16.2057977957552,-14.469727841618)) ;
#34938 = CARTESIAN_POINT('Ctrl Pts',(-14.7474799019799,16.5058286643848,-14.4796762704406)) ;
#34939 = CARTESIAN_POINT('Ctrl Pts',(-14.4098502042424,16.7956339081327,-14.4896595384377)) ;
#34940 = CARTESIAN_POINT('Ctrl Pts',(-14.0721644005434,17.0854873105644,-14.4996444654145)) ;
#34941 = CARTESIAN_POINT('Ctrl Pts',(-13.7257476930588,17.3651115418814,-14.5096644186357)) ;
#34942 = CARTESIAN_POINT('Ctrl Pts',(-13.3712262126238,17.6339570063594,-14.5197939424411)) ;
#34943 = CARTESIAN_POINT('Ctrl Pts',(-13.3210974962862,17.6719712841147,-14.5212262393639)) ;
#34944 = CARTESIAN_POINT('Ctrl Pts',(-13.270806794774,17.7097701019362,-14.5226607556166)) ;
#34945 = CARTESIAN_POINT('Ctrl Pts',(-13.2203559353334,17.7473519512511,-14.5240977294154)) ;
#34946 = CARTESIAN_POINT('Ctrl Pts',(-12.8540078718454,18.0202519151262,-14.5345322903779)) ;
#34947 = CARTESIAN_POINT('Ctrl Pts',(-12.4791180167024,18.2817772414142,-14.5450967602933)) ;
#34948 = CARTESIAN_POINT('Ctrl Pts',(-12.096446163701,18.5314468803889,-14.5557058533015)) ;
#34949 = CARTESIAN_POINT('Ctrl Pts',(-11.7238022515889,18.7745739101754,-14.5660369343347)) ;
#34950 = CARTESIAN_POINT('Ctrl Pts',(-11.3437789926822,19.0064588143181,-14.5764102593736)) ;
#34951 = CARTESIAN_POINT('Ctrl Pts',(-10.9570934318374,19.2266965411546,-14.5867675023611)) ;
#34952 = CARTESIAN_POINT('Ctrl Pts',(-10.5704476322249,19.446911621882,-14.5971236803574)) ;
#34953 = CARTESIAN_POINT('Ctrl Pts',(-10.1771409189719,19.6554820328309,-14.6074636848866)) ;
#34954 = CARTESIAN_POINT('Ctrl Pts',(-9.77790470493387,19.8520393955615,-14.6177512523094)) ;
#34955 = CARTESIAN_POINT('Ctrl Pts',(-9.37869230932992,20.0485850316789,-14.628038205976)) ;
#34956 = CARTESIAN_POINT('Ctrl Pts',(-8.97355100716818,20.233119151384,-14.6382726881001)) ;
#34957 = CARTESIAN_POINT('Ctrl Pts',(-8.56322493812592,20.4053037746043,-14.6484384815999)) ;
#34958 = CARTESIAN_POINT('Ctrl Pts',(-8.13347836857059,20.5856377985473,-14.6590854163499)) ;
#34959 = CARTESIAN_POINT('Ctrl Pts',(-7.69805250397178,20.7524457118887,-14.6696694449544)) ;
#34960 = CARTESIAN_POINT('Ctrl Pts',(-7.25781180429722,20.9053609899327,-14.6801872806006)) ;
#34961 = CARTESIAN_POINT('Ctrl Pts',(-6.83742510131523,21.0513800872584,-14.6902307823785)) ;
#34962 = CARTESIAN_POINT('Ctrl Pts',(-6.41265179725684,21.1847405989812,-14.7002198025993)) ;
#34963 = CARTESIAN_POINT('Ctrl Pts',(-5.98426950815016,21.3051811759733,-14.7101882467287)) ;
#34964 = CARTESIAN_POINT('Ctrl Pts',(-5.55586803851677,21.4256271456107,-14.7201571371884)) ;
#34965 = CARTESIAN_POINT('Ctrl Pts',(-5.12385720369097,21.5331518991969,-14.7301055660084)) ;
#34966 = CARTESIAN_POINT('Ctrl Pts',(-4.68903134808266,21.627530749068,-14.7400888340033)) ;
#34967 = CARTESIAN_POINT('Ctrl Pts',(-4.2541332348432,21.721925282441,-14.7500737609779)) ;
#34968 = CARTESIAN_POINT('Ctrl Pts',(-3.81641911883025,21.8031693500113,-14.7600937141973)) ;
#34969 = CARTESIAN_POINT('Ctrl Pts',(-3.37670116039764,21.871077234674,-14.7702232380016)) ;
#34970 = CARTESIAN_POINT('Ctrl Pts',(-3.31452581075605,21.8806792906995,-14.7716555349368)) ;
#34971 = CARTESIAN_POINT('Ctrl Pts',(-3.2523104264018,21.8900147770267,-14.7730900512021)) ;
#34972 = CARTESIAN_POINT('Ctrl Pts',(-3.19005733214379,21.8990832355265,-14.7745270250134)) ;
#34973 = CARTESIAN_POINT('Ctrl Pts',(-2.73800754381034,21.9649336931498,-14.7849615859776)) ;
#34974 = CARTESIAN_POINT('Ctrl Pts',(-2.28385283854564,22.0167159629141,-14.7955260558956)) ;
#34975 = CARTESIAN_POINT('Ctrl Pts',(-1.82849036152256,22.0543681902254,-14.8061351489068)) ;
#34976 = CARTESIAN_POINT('Ctrl Pts',(-1.38506068790057,22.0910337384651,-14.8164662299439)) ;
#34977 = CARTESIAN_POINT('Ctrl Pts',(-0.94048567128749,22.1143004681896,-14.8268395549872)) ;
#34978 = CARTESIAN_POINT('Ctrl Pts',(-0.495588710245009,22.1241530502275,
-14.8371967979794)) ;
#34979 = CARTESIAN_POINT('Ctrl Pts',(-0.0507374960671489,22.1340046191662,
-14.8475529759804)) ;
#34980 = CARTESIAN_POINT('Ctrl Pts',(0.394435633723673,22.130444906467,-14.8578929805146)) ;
#34981 = CARTESIAN_POINT('Ctrl Pts',(0.839112081126021,22.1134976766824,-14.8681805479425)) ;
#34982 = CARTESIAN_POINT('Ctrl Pts',(1.28376199912979,22.0965514579695,-14.878467501614)) ;
#34983 = CARTESIAN_POINT('Ctrl Pts',(1.72791544045982,22.0662193522683,-14.8887019837431)) ;
#34984 = CARTESIAN_POINT('Ctrl Pts',(2.17075706739576,22.022557917448,-14.8988677772327)) ;
#34985 = CARTESIAN_POINT('Ctrl Pts',(2.63455813772609,21.9768300116459,-14.9095147119707)) ;
#34986 = CARTESIAN_POINT('Ctrl Pts',(3.09692288641447,21.9165025497567,-14.9200987406087)) ;
#34987 = CARTESIAN_POINT('Ctrl Pts',(3.55691655691509,21.8416641974045,-14.9306165762575)) ;
#34988 = CARTESIAN_POINT('Ctrl Pts',(3.99616541033259,21.7702009087324,-14.940660078039)) ;
#34989 = CARTESIAN_POINT('Ctrl Pts',(4.43325332453221,21.6855159560118,-14.9506490982629)) ;
#34990 = CARTESIAN_POINT('Ctrl Pts',(4.86737195482524,21.587749228196,-14.9606175423944)) ;
#34991 = CARTESIAN_POINT('Ctrl Pts',(5.30151002248591,21.4899781229412,-14.9705864328562)) ;
#34992 = CARTESIAN_POINT('Ctrl Pts',(5.73267853131744,21.3791239346503,-14.9805348616774)) ;
#34993 = CARTESIAN_POINT('Ctrl Pts',(6.16007185520018,21.2553667581344,-14.9905181296721)) ;
#34994 = CARTESIAN_POINT('Ctrl Pts',(6.5875362016034,21.1315890161439,-15.0005030566466)) ;
#34995 = CARTESIAN_POINT('Ctrl Pts',(7.0112240574055,20.9949038057253,-15.0105230098646)) ;
#34996 = CARTESIAN_POINT('Ctrl Pts',(7.43033265642514,20.8455339760244,-15.0206525336659)) ;
#34997 = CARTESIAN_POINT('Ctrl Pts',(7.48959387855016,20.8244133436218,-15.0220848305966)) ;
#34998 = CARTESIAN_POINT('Ctrl Pts',(7.54876355168885,20.8030391743093,-15.0235193468573)) ;
#34999 = CARTESIAN_POINT('Ctrl Pts',(7.60783941286998,20.7814121706377,-15.024956320664)) ;
#35000 = CARTESIAN_POINT('Ctrl Pts',(8.03681777829409,20.6243680497633,-15.0353908816239)) ;
#35001 = CARTESIAN_POINT('Ctrl Pts',(8.46095769649285,20.4539473069933,-15.0459553515357)) ;
#35002 = CARTESIAN_POINT('Ctrl Pts',(8.87944054383028,20.2705221664442,-15.0565644445398)) ;
#35003 = CARTESIAN_POINT('Ctrl Pts',(9.28695702112645,20.0919036935493,-15.0668955255765)) ;
#35004 = CARTESIAN_POINT('Ctrl Pts',(9.68910924282036,19.9009537604632,-15.0772688506184)) ;
#35005 = CARTESIAN_POINT('Ctrl Pts',(10.0851655844955,19.6980504490424,-15.0876260936088)) ;
#35006 = CARTESIAN_POINT('Ctrl Pts',(10.4811812013808,19.4951680013064,-15.097982271608)) ;
#35007 = CARTESIAN_POINT('Ctrl Pts',(10.8711022758455,19.2803347101707,-15.1083222761399)) ;
#35008 = CARTESIAN_POINT('Ctrl Pts',(11.254219997474,19.053960764905,-15.1186098435656)) ;
#35009 = CARTESIAN_POINT('Ctrl Pts',(11.6373148622978,18.8276003251097,-15.128896797235)) ;
#35010 = CARTESIAN_POINT('Ctrl Pts',(12.0136073304412,18.589700567336,-15.1391312793621)) ;
#35011 = CARTESIAN_POINT('Ctrl Pts',(12.3824070543977,18.3406989783901,-15.1492970728808)) ;
#35012 = CARTESIAN_POINT('Ctrl Pts',(12.7686618599914,18.0799122855504,-15.1599440076376)) ;
#35013 = CARTESIAN_POINT('Ctrl Pts',(13.1467103378622,17.8069655660871,-15.1705280362015)) ;
#35014 = CARTESIAN_POINT('Ctrl Pts',(13.5157723580305,17.5223813413833,-15.18104587184)) ;
#35015 = CARTESIAN_POINT('Ctrl Pts',(13.8681904015218,17.250631309687,-15.1910893736226)) ;
#35016 = CARTESIAN_POINT('Ctrl Pts',(14.2124199351184,16.9682779594212,-15.201078393849)) ;
#35017 = CARTESIAN_POINT('Ctrl Pts',(14.5478163910286,16.675828757253,-15.211046837985)) ;
#35018 = CARTESIAN_POINT('Ctrl Pts',(14.8832278640873,16.3833664608704,-15.2210157284513)) ;
#35019 = CARTESIAN_POINT('Ctrl Pts',(15.2098053956224,16.0808072927439,-15.2309641572789)) ;
#35020 = CARTESIAN_POINT('Ctrl Pts',(15.526925929212,15.7686927953774,-15.2409474252827)) ;
#35021 = CARTESIAN_POINT('Ctrl Pts',(15.844099160628,15.4565264320678,-15.2509323522662)) ;
#35022 = CARTESIAN_POINT('Ctrl Pts',(16.1518121149721,15.1348014192352,-15.2609523054958)) ;
#35023 = CARTESIAN_POINT('Ctrl Pts',(16.4494645834814,14.8040955498571,-15.2710818293117)) ;
#35024 = CARTESIAN_POINT('Ctrl Pts',(16.4915521203773,14.7573343200617,-15.2725141262098)) ;
#35025 = CARTESIAN_POINT('Ctrl Pts',(16.5334385533032,14.7103935927233,-15.2739486424378)) ;
#35026 = CARTESIAN_POINT('Ctrl Pts',(16.5751222256453,14.6632750620232,-15.2753856162117)) ;
#35027 = CARTESIAN_POINT('Ctrl Pts',(16.8778075135283,14.3211246412901,-15.2858201771801)) ;
#35028 = CARTESIAN_POINT('Ctrl Pts',(17.1698752271347,13.9695078748294,-15.2963846471033)) ;
#35029 = CARTESIAN_POINT('Ctrl Pts',(17.4507822432622,13.6091415001395,-15.3069937401202)) ;
#35030 = CARTESIAN_POINT('Ctrl Pts',(17.7243280722034,13.2582185504531,-15.3173248211435)) ;
#35031 = CARTESIAN_POINT('Ctrl Pts',(17.9872908051944,12.8989987202108,-15.3276981461732)) ;
#35032 = CARTESIAN_POINT('Ctrl Pts',(18.2392066369358,12.5321625274619,-15.3380553891518)) ;
#35033 = CARTESIAN_POINT('Ctrl Pts',(18.4910965652423,12.1653640549205,-15.3484115671391)) ;
#35034 = CARTESIAN_POINT('Ctrl Pts',(18.7319419744567,11.7909508137328,-15.3587515716595)) ;
#35035 = CARTESIAN_POINT('Ctrl Pts',(18.9613143971691,11.4096207172977,-15.3690391390733)) ;
#35036 = CARTESIAN_POINT('Ctrl Pts',(19.1906731355211,11.0283133710189,-15.3793260927307)) ;
#35037 = CARTESIAN_POINT('Ctrl Pts',(19.4085603638977,10.6400898901897,-15.3895605748454)) ;
#35038 = CARTESIAN_POINT('Ctrl Pts',(19.6145768377597,10.245663421493,-15.3997263683028)) ;
#35039 = CARTESIAN_POINT('Ctrl Pts',(19.8303439553452,9.83256897008963,-15.4103733030414)) ;
#35040 = CARTESIAN_POINT('Ctrl Pts',(20.033109362744,9.41267999232148,-15.4209573317316)) ;
#35041 = CARTESIAN_POINT('Ctrl Pts',(20.2224352726086,8.98682713471104,-15.4314751673962)) ;
#35042 = CARTESIAN_POINT('Ctrl Pts',(20.4032229527388,8.58017941143189,-15.4415186691607)) ;
#35043 = CARTESIAN_POINT('Ctrl Pts',(20.5717648884173,8.16809810738047,-15.4515076893666)) ;
#35044 = CARTESIAN_POINT('Ctrl Pts',(20.7277353859778,7.7513361592637,-15.4614761334789)) ;
#35045 = CARTESIAN_POINT('Ctrl Pts',(20.883712867013,7.33455555090941,-15.4714450239216)) ;
#35046 = CARTESIAN_POINT('Ctrl Pts',(21.027117665037,6.91309381214329,-15.4813934527224)) ;
#35047 = CARTESIAN_POINT('Ctrl Pts',(21.1576592144443,6.48772362609034,-15.4913767206954)) ;
#35048 = CARTESIAN_POINT('Ctrl Pts',(21.2882224567299,6.06228275370249,-15.5013616476484)) ;
#35049 = CARTESIAN_POINT('Ctrl Pts',(21.4059179868281,5.63293207259755,-15.5113816008435)) ;
#35050 = CARTESIAN_POINT('Ctrl Pts',(21.510492576861,5.20046528985004,-15.5215111246202)) ;
#35051 = CARTESIAN_POINT('Ctrl Pts',(21.5252792418472,5.13931523961193,-15.5229434216487)) ;
#35052 = CARTESIAN_POINT('Ctrl Pts',(21.5398036378763,5.07810292224206,-15.5243779380074)) ;
#35053 = CARTESIAN_POINT('Ctrl Pts',(21.5540651133108,5.01683061589433,-15.5258149119125)) ;
#35054 = CARTESIAN_POINT('Ctrl Pts',(21.6576245685067,4.5719028317288,-15.5362494728682)) ;
#35055 = CARTESIAN_POINT('Ctrl Pts',(21.7473421448813,4.12369678955954,-15.5468139427755)) ;
#35056 = CARTESIAN_POINT('Ctrl Pts',(21.8230809070896,3.67310127741325,-15.5574230357757)) ;
#35057 = CARTESIAN_POINT('Ctrl Pts',(21.8968349304165,3.23431364813468,-15.567754116847)) ;
#35058 = CARTESIAN_POINT('Ctrl Pts',(21.9573335435185,2.79326013028553,-15.5781274419242)) ;
#35059 = CARTESIAN_POINT('Ctrl Pts',(22.0044923619925,2.35075993046879,-15.5884846849508)) ;
#35060 = CARTESIAN_POINT('Ctrl Pts',(22.0516463313258,1.90830523106504,-15.5988408629862)) ;
#35061 = CARTESIAN_POINT('Ctrl Pts',(22.085463359548,1.46440411896152,-15.609180867555)) ;
#35062 = CARTESIAN_POINT('Ctrl Pts',(22.1058984209575,1.0198742983453,-15.6194684350184)) ;
#35063 = CARTESIAN_POINT('Ctrl Pts',(22.1263322632109,0.575370998383557,-15.6297553887254)) ;
#35064 = CARTESIAN_POINT('Ctrl Pts',(22.1333857802633,0.130238921738118,-15.6399898708908)) ;
#35065 = CARTESIAN_POINT('Ctrl Pts',(22.1270468977107,-0.314704723780525,
-15.6501556644476)) ;
#35066 = CARTESIAN_POINT('Ctrl Pts',(22.1204079994866,-0.780707296565286,
-15.6608025991765)) ;
#35067 = CARTESIAN_POINT('Ctrl Pts',(22.0991005065641,-1.24650398272563,-15.6713866277163)) ;
#35068 = CARTESIAN_POINT('Ctrl Pts',(22.0631343161778,-1.71115588215796,-15.6819044633305)) ;
#35069 = CARTESIAN_POINT('Ctrl Pts',(22.0287901305526,-2.1548528907594,-15.6919479651533)) ;
#35070 = CARTESIAN_POINT('Ctrl Pts',(21.9810895618747,-2.59750630302009,-15.7019369854204)) ;
#35071 = CARTESIAN_POINT('Ctrl Pts',(21.9201041596768,-3.03829888535571,-15.7119054295972)) ;
#35072 = CARTESIAN_POINT('Ctrl Pts',(21.8591160269008,-3.47911120386594,-15.721874320104)) ;
#35073 = CARTESIAN_POINT('Ctrl Pts',(21.7848417342053,-3.91806252827625,-15.7318227489723)) ;
#35074 = CARTESIAN_POINT('Ctrl Pts',(21.6973931232892,-4.35433495942962,-15.7418060170167)) ;
#35075 = CARTESIAN_POINT('Ctrl Pts',(21.6099299805154,-4.79067988857734,-15.7517909440404)) ;
#35076 = CARTESIAN_POINT('Ctrl Pts',(21.5092879455416,-5.22434499945482,-15.7618108973102)) ;
#35077 = CARTESIAN_POINT('Ctrl Pts',(21.3956217035828,-5.65451165430317,-15.7719404211659)) ;
#35078 = CARTESIAN_POINT('Ctrl Pts',(21.3795494986091,-5.7153364562003,-15.7733727178698)) ;
#35079 = CARTESIAN_POINT('Ctrl Pts',(21.3632169675423,-5.77609131197269,-15.774807233903)) ;
#35080 = CARTESIAN_POINT('Ctrl Pts',(21.3466246205186,-5.83677390766786,-15.7762442074813)) ;
#35081 = CARTESIAN_POINT('Ctrl Pts',(21.2261395543992,-6.27741961886123,-15.7866787684481)) ;
#35082 = CARTESIAN_POINT('Ctrl Pts',(21.0919189661969,-6.71436667920628,-15.7972432383664)) ;
#35083 = CARTESIAN_POINT('Ctrl Pts',(20.9442650580843,-7.14676811213256,-15.8078523313749)) ;
#35084 = CARTESIAN_POINT('Ctrl Pts',(20.8004804313346,-7.56783843417188,-15.8181834123322)) ;
#35085 = CARTESIAN_POINT('Ctrl Pts',(20.6439576245207,-7.98459843006223,-15.8285567372921)) ;
#35086 = CARTESIAN_POINT('Ctrl Pts',(20.47501197888,-8.39628732384464,-15.8389139801985)) ;
#35087 = CARTESIAN_POINT('Ctrl Pts',(20.3060837052022,-8.80793388540734,-15.8492701581137)) ;
#35088 = CARTESIAN_POINT('Ctrl Pts',(20.1247352309551,-9.21451046497884,-15.8596101625594)) ;
#35089 = CARTESIAN_POINT('Ctrl Pts',(19.9313158063182,-9.61527632526949,-15.8698977298976)) ;
#35090 = CARTESIAN_POINT('Ctrl Pts',(19.7379079210824,-10.0160182758726,-15.8801846834797)) ;
#35091 = CARTESIAN_POINT('Ctrl Pts',(19.5324304971458,-10.4109503478303,-15.8904191655179)) ;
#35092 = CARTESIAN_POINT('Ctrl Pts',(19.3152615355607,-10.7993479105026,-15.9005849589674)) ;
#35093 = CARTESIAN_POINT('Ctrl Pts',(19.0878140871097,-11.2061281150475,-15.9112318937997)) ;
#35094 = CARTESIAN_POINT('Ctrl Pts',(18.8475607465869,-11.6057515606328,-15.9218159223724)) ;
#35095 = CARTESIAN_POINT('Ctrl Pts',(18.594956714121,-11.9973970138781,-15.93233375806)) ;
#35096 = CARTESIAN_POINT('Ctrl Pts',(18.3537446337449,-12.371380016544,-15.9423772597511)) ;
#35097 = CARTESIAN_POINT('Ctrl Pts',(18.1012793724234,-12.7380933581479,-15.952366279886)) ;
#35098 = CARTESIAN_POINT('Ctrl Pts',(17.83801250649,-13.0968521526768,-15.9623347239313)) ;
#35099 = CARTESIAN_POINT('Ctrl Pts',(17.5747338529472,-13.4556270104065,-15.9723036143074)) ;
#35100 = CARTESIAN_POINT('Ctrl Pts',(17.3006525060449,-13.8064465458687,-15.9822520430458)) ;
#35101 = CARTESIAN_POINT('Ctrl Pts',(17.0162558032043,-14.1486444484711,-15.992235310962)) ;
#35102 = CARTESIAN_POINT('Ctrl Pts',(16.7318118404237,-14.4908992161926,-16.0022202378589)) ;
#35103 = CARTESIAN_POINT('Ctrl Pts',(16.4370489379124,-14.8245293621743,-16.0122401910037)) ;
#35104 = CARTESIAN_POINT('Ctrl Pts',(16.1324924733015,-15.1488883002968,-16.0223697147375)) ;
#35105 = CARTESIAN_POINT('Ctrl Pts',(16.0894287103524,-15.1947520991151,-16.0238020120602)) ;
#35106 = CARTESIAN_POINT('Ctrl Pts',(16.0461692040839,-15.2404305689993,-16.0252365287142)) ;
#35107 = CARTESIAN_POINT('Ctrl Pts',(16.0027155036575,-15.2859219169845,-16.0266735029158)) ;
#35108 = CARTESIAN_POINT('Ctrl Pts',(15.6871772801474,-15.6162564796911,-16.0371080638932)) ;
#35109 = CARTESIAN_POINT('Ctrl Pts',(15.3613149608306,-15.9368054596001,-16.0476725338348)) ;
#35110 = CARTESIAN_POINT('Ctrl Pts',(15.025797168888,-16.2469674928623,-16.0582816268791)) ;
#35111 = CARTESIAN_POINT('Ctrl Pts',(14.6990716395051,-16.5490017126434,-16.068612708045)) ;
#35112 = CARTESIAN_POINT('Ctrl Pts',(14.3631902466487,-16.8411865507727,-16.0789860332267)) ;
#35113 = CARTESIAN_POINT('Ctrl Pts',(14.0187921791655,-17.1230027213753,-16.0893432763632)) ;
#35114 = CARTESIAN_POINT('Ctrl Pts',(13.6744295246733,-17.4047899140176,-16.0996994545084)) ;
#35115 = CARTESIAN_POINT('Ctrl Pts',(13.3215519837295,-17.67621067911,-16.1100394591926)) ;
#35116 = CARTESIAN_POINT('Ctrl Pts',(12.9608190451236,-17.9367794839549,-16.120327026772)) ;
#35117 = CARTESIAN_POINT('Ctrl Pts',(12.6001076278555,-18.1973327432572,-16.1306139805949)) ;
#35118 = CARTESIAN_POINT('Ctrl Pts',(12.2315416550019,-18.4470354531436,-16.1408484628769)) ;
#35119 = CARTESIAN_POINT('Ctrl Pts',(11.8557982474563,-18.6854299218368,-16.151014256314)) ;
#35120 = CARTESIAN_POINT('Ctrl Pts',(11.4622711235392,-18.935107461718,-16.1616611908266)) ;
#35121 = CARTESIAN_POINT('Ctrl Pts',(11.0608821915056,-19.1723994457757,-16.1722452198653)) ;
#35122 = CARTESIAN_POINT('Ctrl Pts',(10.6524224217679,-19.3967999123517,-16.1827630554936)) ;
#35123 = CARTESIAN_POINT('Ctrl Pts',(10.2623833845461,-19.6110803590934,-16.1928065574148)) ;
#35124 = CARTESIAN_POINT('Ctrl Pts',(9.86590213146238,-19.8136143204186,-16.2027955777705)) ;
#35125 = CARTESIAN_POINT('Ctrl Pts',(9.4637016064469,-20.0040140565321,-16.2127640220214)) ;
#35126 = CARTESIAN_POINT('Ctrl Pts',(9.06148307321215,-20.1944223176474,-16.2227329126018)) ;
#35127 = CARTESIAN_POINT('Ctrl Pts',(8.65354467893047,-20.3726951538725,-16.2326813415289)) ;
#35128 = CARTESIAN_POINT('Ctrl Pts',(8.2406319926359,-20.5384781721711,-16.2426646096125)) ;
#35129 = CARTESIAN_POINT('Ctrl Pts',(7.82765069020417,-20.704288739612,-16.2526495366748)) ;
#35130 = CARTESIAN_POINT('Ctrl Pts',(7.40969336449929,-20.8576051555763,-16.2626694899634)) ;
#35131 = CARTESIAN_POINT('Ctrl Pts',(6.98752966814416,-20.9981084684307,-16.2727990138138)) ;
#35132 = CARTESIAN_POINT('Ctrl Pts',(6.92783648149656,-21.0179753839217,-16.2742313102502)) ;
#35133 = CARTESIAN_POINT('Ctrl Pts',(6.86805923479046,-21.0375861822736,-16.2756658260145)) ;
#35134 = CARTESIAN_POINT('Ctrl Pts',(6.80820014344603,-21.0569400229394,-16.2771027993227)) ;
#35135 = CARTESIAN_POINT('Ctrl Pts',(6.3840662249976,-21.1940724132621,-16.2872845295527)) ;
#35136 = CARTESIAN_POINT('Ctrl Pts',(5.95571662068674,-21.3183340351005,-16.2975900166844)) ;
#35137 = CARTESIAN_POINT('Ctrl Pts',(5.52396187406269,-21.4295287131257,-16.3079398138918)) ;
#35138 = CARTESIAN_POINT('Ctrl Pts',(5.07349743468953,-21.5455419097137,-16.318738109992)) ;
#35139 = CARTESIAN_POINT('Ctrl Pts',(4.6193263349758,-21.6473310109628,-16.3295842934684)) ;
#35140 = CARTESIAN_POINT('Ctrl Pts',(4.16237135896441,-21.734721310978,-16.3404117032938)) ;
#35141 = CARTESIAN_POINT('Ctrl Pts',(3.72451307507802,-21.81845946638,-16.3507866227802)) ;
#35142 = CARTESIAN_POINT('Ctrl Pts',(3.28409872649029,-21.8889775702143,-16.3611443679875)) ;
#35143 = CARTESIAN_POINT('Ctrl Pts',(2.84194227547393,-21.9461619586397,-16.3714489886679)) ;
#35144 = CARTESIAN_POINT('Ctrl Pts',(2.39982355247863,-22.003341467675,-16.3817527300827)) ;
#35145 = CARTESIAN_POINT('Ctrl Pts',(1.95596293810181,-22.0471895885666,-16.3920033160626)) ;
#35146 = CARTESIAN_POINT('Ctrl Pts',(1.51117670721767,-22.0776282696489,-16.4021866747302)) ;
#35147 = CARTESIAN_POINT('Ctrl Pts',(1.06639929112509,-22.1080663474962,-16.4123698315837)) ;
#35148 = CARTESIAN_POINT('Ctrl Pts',(0.620696708842184,-22.1251049600064,
-16.4224912401162)) ;
#35149 = CARTESIAN_POINT('Ctrl Pts',(0.174887699130083,-22.1286943106416,
-16.4325548170702)) ;
#35150 = CARTESIAN_POINT('Ctrl Pts',(0.116466280787281,-22.1291646801283,
-16.4338736070149)) ;
#35151 = CARTESIAN_POINT('Ctrl Pts',(0.0580430444652074,-22.1294042197614,
-16.4351914834666)) ;
#35152 = CARTESIAN_POINT('Ctrl Pts',(-0.000380161200413355,-22.1294128925051,
-16.4365085000897)) ;
#35153 = CARTESIAN_POINT('Origin',(0.,0.,-10.)) ;
#35154 = CARTESIAN_POINT('',(-2.71011275034311E-15,-22.12975,-20.)) ;
#35155 = CARTESIAN_POINT('',(0.00050934658643668,-22.1297499941383,-19.6109246391395)) ;
#35156 = CARTESIAN_POINT('',(-2.71011275034311E-15,-22.12975,-10.)) ;
#35157 = CARTESIAN_POINT('',(3.34070509846219,-21.8761405304411,-20.)) ;
#35158 = CARTESIAN_POINT('Origin',(0.,0.,-20.)) ;
#35159 = CARTESIAN_POINT('Ctrl Pts',(3.3407050984622,-21.8761405304411,-20.)) ;
#35160 = CARTESIAN_POINT('Ctrl Pts',(3.79243697068971,-21.8071565628812,-19.9895654460161)) ;
#35161 = CARTESIAN_POINT('Ctrl Pts',(4.24205501176312,-21.7241722534374,-19.9791308920322)) ;
#35162 = CARTESIAN_POINT('Ctrl Pts',(4.6886871030314,-21.6273449205483,-19.9686963380483)) ;
#35163 = CARTESIAN_POINT('Ctrl Pts',(5.12615421837869,-21.5325045030461,-19.9584759031075)) ;
#35164 = CARTESIAN_POINT('Ctrl Pts',(5.56075648282984,-21.4243835827313,-19.9482554681667)) ;
#35165 = CARTESIAN_POINT('Ctrl Pts',(5.99168520350615,-21.3031815343292,-19.9380350332259)) ;
#35166 = CARTESIAN_POINT('Ctrl Pts',(6.42260071072155,-21.1819832023156,-19.9278149116718)) ;
#35167 = CARTESIAN_POINT('Ctrl Pts',(6.84984268386217,-21.0477046044914,-19.9175947901176)) ;
#35168 = CARTESIAN_POINT('Ctrl Pts',(7.27261650517739,-20.9005953080557,-19.9073746685635)) ;
#35169 = CARTESIAN_POINT('Ctrl Pts',(7.69539013295677,-20.7534860789633,-19.8971545516879)) ;
#35170 = CARTESIAN_POINT('Ctrl Pts',(8.11369540181686,-20.5935462370468,-19.8869344348123)) ;
#35171 = CARTESIAN_POINT('Ctrl Pts',(8.52675489776927,-20.4210745548776,-19.8767143179368)) ;
#35172 = CARTESIAN_POINT('Ctrl Pts',(8.9549779599098,-20.2422713737505,-19.8661190168075)) ;
#35173 = CARTESIAN_POINT('Ctrl Pts',(9.37756266132238,-20.0499991455787,-19.8555237156783)) ;
#35174 = CARTESIAN_POINT('Ctrl Pts',(9.79366589611002,-19.8446452066514,-19.8449284145491)) ;
#35175 = CARTESIAN_POINT('Ctrl Pts',(10.1951078639102,-19.646526849363,-19.8347064355325)) ;
#35176 = CARTESIAN_POINT('Ctrl Pts',(10.5905169982379,-19.4362327966258,-19.8244844565158)) ;
#35177 = CARTESIAN_POINT('Ctrl Pts',(10.9791601023046,-19.2141582826431,-19.8142624774992)) ;
#35178 = CARTESIAN_POINT('Ctrl Pts',(11.3678262810571,-18.9920705835567,-19.8040398915789)) ;
#35179 = CARTESIAN_POINT('Ctrl Pts',(11.7497254337773,-18.7582011388228,-19.7938173056585)) ;
#35180 = CARTESIAN_POINT('Ctrl Pts',(12.1241506717191,-18.5129901839749,-19.7835947197381)) ;
#35181 = CARTESIAN_POINT('Ctrl Pts',(12.498637489504,-18.2677389005099,-19.7733704525603)) ;
#35182 = CARTESIAN_POINT('Ctrl Pts',(12.8656477491244,-18.0111425023592,-19.7631461853824)) ;
#35183 = CARTESIAN_POINT('Ctrl Pts',(13.2245034898344,-17.7436845809955,-19.7529219182046)) ;
#35184 = CARTESIAN_POINT('Ctrl Pts',(13.2637109393324,-17.7144629697599,-19.7518048469318)) ;
#35185 = CARTESIAN_POINT('Ctrl Pts',(13.3028210782212,-17.6851117451297,-19.7506877756589)) ;
#35186 = CARTESIAN_POINT('Ctrl Pts',(13.3418330449212,-17.6556315679714,-19.7495707043861)) ;
#35187 = CARTESIAN_POINT('Ctrl Pts',(13.7062435193986,-17.3802574647239,-19.7391361504022)) ;
#35188 = CARTESIAN_POINT('Ctrl Pts',(14.0621855564206,-17.093551993444,-19.7287015964183)) ;
#35189 = CARTESIAN_POINT('Ctrl Pts',(14.4089555524661,-16.7960660557631,-19.7182670424344)) ;
#35190 = CARTESIAN_POINT('Ctrl Pts',(14.7456256827497,-16.5072445586938,-19.7081364005413)) ;
#35191 = CARTESIAN_POINT('Ctrl Pts',(15.07365025053,-16.2082617802615,-19.6980057586482)) ;
#35192 = CARTESIAN_POINT('Ctrl Pts',(15.3924188474478,-15.8996627979097,-19.6878751167551)) ;
#35193 = CARTESIAN_POINT('Ctrl Pts',(15.7111459282296,-15.5911040072124,-19.6777457942677)) ;
#35194 = CARTESIAN_POINT('Ctrl Pts',(16.0206192789643,-15.2729316755362,-19.6676164717803)) ;
#35195 = CARTESIAN_POINT('Ctrl Pts',(16.320264375849,-14.9457286796226,-19.6574871492929)) ;
#35196 = CARTESIAN_POINT('Ctrl Pts',(16.6198851681435,-14.618552223555,-19.6473586484075)) ;
#35197 = CARTESIAN_POINT('Ctrl Pts',(16.9096791421221,-14.2823467377391,-19.6372301475222)) ;
#35198 = CARTESIAN_POINT('Ctrl Pts',(17.1891100231423,-13.9377305066072,-19.6271016466369)) ;
#35199 = CARTESIAN_POINT('Ctrl Pts',(17.4685319635363,-13.5931253017616,-19.6169734698214)) ;
#35200 = CARTESIAN_POINT('Ctrl Pts',(17.7375913273382,-13.2401100698593,-19.606845293006)) ;
#35201 = CARTESIAN_POINT('Ctrl Pts',(17.9957922924994,-12.8793359622194,-19.5967171161906)) ;
#35202 = CARTESIAN_POINT('Ctrl Pts',(18.2540199317834,-12.5185245838713,-19.5865878930575)) ;
#35203 = CARTESIAN_POINT('Ctrl Pts',(18.5013867940576,-12.1499529159039,-19.5764586699244)) ;
#35204 = CARTESIAN_POINT('Ctrl Pts',(18.7374394273198,-11.7743024748823,-19.5663294467913)) ;
#35205 = CARTESIAN_POINT('Ctrl Pts',(18.9735016270929,-11.3986368098661,-19.556199813151)) ;
#35206 = CARTESIAN_POINT('Ctrl Pts',(19.1982485601447,-11.0158919966168,-19.5460701795106)) ;
#35207 = CARTESIAN_POINT('Ctrl Pts',(19.411271159721,-10.6267768879508,-19.5359405458703)) ;
#35208 = CARTESIAN_POINT('Ctrl Pts',(19.6243313335516,-10.2375931447357,-19.525809125502)) ;
#35209 = CARTESIAN_POINT('Ctrl Pts',(19.8256629301047,-9.84203706470778,-19.5156777051336)) ;
#35210 = CARTESIAN_POINT('Ctrl Pts',(20.0149028339713,-9.4408421027569,-19.5055462847653)) ;
#35211 = CARTESIAN_POINT('Ctrl Pts',(20.054780694894,-9.35629969616782,-19.503411326101)) ;
#35212 = CARTESIAN_POINT('Ctrl Pts',(20.0941217827245,-9.27150697063714,-19.5012763674367)) ;
#35213 = CARTESIAN_POINT('Ctrl Pts',(20.1329229677406,-9.18647091311582,-19.4991414087723)) ;
#35214 = CARTESIAN_POINT('Ctrl Pts',(20.322562732882,-8.77085943191464,-19.4887068547884)) ;
#35215 = CARTESIAN_POINT('Ctrl Pts',(20.4993499633938,-8.34932714801769,-19.4782723008045)) ;
#35216 = CARTESIAN_POINT('Ctrl Pts',(20.6629329963277,-7.92269114958888,-19.4678377468206)) ;
#35217 = CARTESIAN_POINT('Ctrl Pts',(20.8224877607088,-7.50656115746839,-19.4576601460483)) ;
#35218 = CARTESIAN_POINT('Ctrl Pts',(20.9694807490619,-7.0855760176988,-19.447482545276)) ;
#35219 = CARTESIAN_POINT('Ctrl Pts',(21.1036346104306,-6.66051359070265,-19.4373049445037)) ;
#35220 = CARTESIAN_POINT('Ctrl Pts',(21.2377764380265,-6.23548929234978,-19.4271282566752)) ;
#35221 = CARTESIAN_POINT('Ctrl Pts',(21.359081370659,-5.80638865474412,-19.4169515688467)) ;
#35222 = CARTESIAN_POINT('Ctrl Pts',(21.467321673352,-5.37400551128574,-19.4067748810181)) ;
#35223 = CARTESIAN_POINT('Ctrl Pts',(21.5755565743006,-4.94164394595661,-19.3965987010584)) ;
#35224 = CARTESIAN_POINT('Ctrl Pts',(21.670728092663,-4.5060004232084,-19.3864225210986)) ;
#35225 = CARTESIAN_POINT('Ctrl Pts',(21.7526590257418,-4.06788155829462,-19.3762463411389)) ;
#35226 = CARTESIAN_POINT('Ctrl Pts',(21.8382264844152,-3.61031667457137,-19.3656184888072)) ;
#35227 = CARTESIAN_POINT('Ctrl Pts',(21.9093514285122,-3.15005201733719,-19.3549906364754)) ;
#35228 = CARTESIAN_POINT('Ctrl Pts',(21.9658916693059,-2.68801752874067,-19.3443627841437)) ;
#35229 = CARTESIAN_POINT('Ctrl Pts',(22.0200346956006,-2.24557255302133,-19.3341855355121)) ;
#35230 = CARTESIAN_POINT('Ctrl Pts',(22.0608038992464,-1.80150492822418,-19.3240082868804)) ;
#35231 = CARTESIAN_POINT('Ctrl Pts',(22.0881273500749,-1.35663747160816,-19.3138310382488)) ;
#35232 = CARTESIAN_POINT('Ctrl Pts',(22.1154519954715,-0.911750565602043,
-19.3036533446727)) ;
#35233 = CARTESIAN_POINT('Ctrl Pts',(22.1293297018622,-0.466063985600068,
-19.2934756510967)) ;
#35234 = CARTESIAN_POINT('Ctrl Pts',(22.1297405942435,-0.0204032838767659,
-19.2832979575206)) ;
#35235 = CARTESIAN_POINT('Ctrl Pts',(22.1301515519295,0.425328248427631,-19.2731186463643)) ;
#35236 = CARTESIAN_POINT('Ctrl Pts',(22.1170914187326,0.871033666252579,-19.262939335208)) ;
#35237 = CARTESIAN_POINT('Ctrl Pts',(22.0905924393186,1.31588781528603,-19.2527600240517)) ;
#35238 = CARTESIAN_POINT('Ctrl Pts',(22.0870799060446,1.374854803266,-19.2514107204206)) ;
#35239 = CARTESIAN_POINT('Ctrl Pts',(22.0833313212298,1.43380683812886,-19.2500614167895)) ;
#35240 = CARTESIAN_POINT('Ctrl Pts',(22.0793468285778,1.49274200244797,-19.2487121131585)) ;
#35241 = CARTESIAN_POINT('Ctrl Pts',(22.0485335981691,1.94850461915425,-19.2382775591745)) ;
#35242 = CARTESIAN_POINT('Ctrl Pts',(22.0035995302651,2.40337505914454,-19.2278430051906)) ;
#35243 = CARTESIAN_POINT('Ctrl Pts',(21.9446221721438,2.85646508544292,-19.2174084512067)) ;
#35244 = CARTESIAN_POINT('Ctrl Pts',(21.8872306192117,3.29737225822284,-19.2072544653999)) ;
#35245 = CARTESIAN_POINT('Ctrl Pts',(21.8165410911735,3.73659326317763,-19.197100479593)) ;
#35246 = CARTESIAN_POINT('Ctrl Pts',(21.7326775496694,4.17331541877621,-19.1869464937861)) ;
#35247 = CARTESIAN_POINT('Ctrl Pts',(21.6488230510757,4.60999048312111,-19.176793602872)) ;
#35248 = CARTESIAN_POINT('Ctrl Pts',(21.5517974198474,5.04416701032279,-19.1666407119579)) ;
#35249 = CARTESIAN_POINT('Ctrl Pts',(21.4417758771208,5.47504176219896,-19.1564878210438)) ;
#35250 = CARTESIAN_POINT('Ctrl Pts',(21.3317612926476,5.90588926363242,-19.1463355722438)) ;
#35251 = CARTESIAN_POINT('Ctrl Pts',(21.2087524956298,6.33343518393133,-19.1361833234439)) ;
#35252 = CARTESIAN_POINT('Ctrl Pts',(21.0729752571866,6.75688899364948,-19.1260310746439)) ;
#35253 = CARTESIAN_POINT('Ctrl Pts',(20.9305987099914,7.20092432693188,-19.1153853865523)) ;
#35254 = CARTESIAN_POINT('Ctrl Pts',(20.7741819950338,7.64045969298141,-19.1047396984607)) ;
#35255 = CARTESIAN_POINT('Ctrl Pts',(20.6040440446311,8.07460240936996,-19.0940940103691)) ;
#35256 = CARTESIAN_POINT('Ctrl Pts',(20.4417767872506,8.48866139934446,-19.0839407987813)) ;
#35257 = CARTESIAN_POINT('Ctrl Pts',(20.2670289301901,8.89781506380064,-19.0737875871935)) ;
#35258 = CARTESIAN_POINT('Ctrl Pts',(20.0801267919074,9.30130867584889,-19.0636343756057)) ;
#35259 = CARTESIAN_POINT('Ctrl Pts',(19.8932161178159,9.70482071542506,-19.0534807003214)) ;
#35260 = CARTESIAN_POINT('Ctrl Pts',(19.694150152377,10.1026719782809,-19.043327025037)) ;
#35261 = CARTESIAN_POINT('Ctrl Pts',(19.4833023080315,10.4941300847833,-19.0331733497527)) ;
#35262 = CARTESIAN_POINT('Ctrl Pts',(19.2724186442316,10.8856546933449,-19.023017949532)) ;
#35263 = CARTESIAN_POINT('Ctrl Pts',(19.0497492113925,11.2707837727805,-19.0128625493114)) ;
#35264 = CARTESIAN_POINT('Ctrl Pts',(18.8157130769916,11.6488100880231,-19.0027071490907)) ;
#35265 = CARTESIAN_POINT('Ctrl Pts',(18.7817261199756,11.7037074403484,-19.0012323719087)) ;
#35266 = CARTESIAN_POINT('Ctrl Pts',(18.747499525508,11.7584550484515,-18.9997575947267)) ;
#35267 = CARTESIAN_POINT('Ctrl Pts',(18.7130346544292,11.8130507949738,-18.9982828175446)) ;
#35268 = CARTESIAN_POINT('Ctrl Pts',(18.4691838800839,12.1993344121385,-18.9878482635607)) ;
#35269 = CARTESIAN_POINT('Ctrl Pts',(18.2133371812781,12.5781141300808,-18.9774137095768)) ;
#35270 = CARTESIAN_POINT('Ctrl Pts',(17.9459852961038,12.9486465244259,-18.9669791555929)) ;
#35271 = CARTESIAN_POINT('Ctrl Pts',(17.6855825221689,13.3095479007423,-18.9568158204797)) ;
#35272 = CARTESIAN_POINT('Ctrl Pts',(17.4142652102917,13.6626250534368,-18.9466524853664)) ;
#35273 = CARTESIAN_POINT('Ctrl Pts',(17.1325301821108,14.0072211598719,-18.9364891502532)) ;
#35274 = CARTESIAN_POINT('Ctrl Pts',(16.8508237559169,14.3517822826082,-18.9263268469306)) ;
#35275 = CARTESIAN_POINT('Ctrl Pts',(16.5587018711189,14.6878639014468,-18.9161645436081)) ;
#35276 = CARTESIAN_POINT('Ctrl Pts',(16.2567019280894,15.0148419067187,-18.9060022402855)) ;
#35277 = CARTESIAN_POINT('Ctrl Pts',(15.954719742825,15.3418006855013,-18.8958405345121)) ;
#35278 = CARTESIAN_POINT('Ctrl Pts',(15.6428608153228,15.6596567517417,-18.8856788287386)) ;
#35279 = CARTESIAN_POINT('Ctrl Pts',(15.3217009513977,15.9678212357992,-18.8755171229652)) ;
#35280 = CARTESIAN_POINT('Ctrl Pts',(14.985467828973,16.2904490555668,-18.8648784895456)) ;
#35281 = CARTESIAN_POINT('Ctrl Pts',(14.6390401032639,16.6024537021538,-18.8542398561261)) ;
#35282 = CARTESIAN_POINT('Ctrl Pts',(14.2831208788024,16.9032036319752,-18.8436012227066)) ;
#35283 = CARTESIAN_POINT('Ctrl Pts',(13.9431244897694,17.1904988470508,-18.8334385321344)) ;
#35284 = CARTESIAN_POINT('Ctrl Pts',(13.5944673083247,17.467523991423,-18.8232758415622)) ;
#35285 = CARTESIAN_POINT('Ctrl Pts',(13.2377964855047,17.7337694602941,-18.8131131509901)) ;
#35286 = CARTESIAN_POINT('Ctrl Pts',(12.8811098745721,18.0000267145796,-18.8029500105642)) ;
#35287 = CARTESIAN_POINT('Ctrl Pts',(12.5164090986917,18.2555032047083,-18.7927868701383)) ;
#35288 = CARTESIAN_POINT('Ctrl Pts',(12.1443721118082,18.4997313783859,-18.7826237297123)) ;
#35289 = CARTESIAN_POINT('Ctrl Pts',(11.7722738496555,18.7439997769541,-18.772458915396)) ;
#35290 = CARTESIAN_POINT('Ctrl Pts',(11.3928371539001,18.9770160314776,-18.7622941010796)) ;
#35291 = CARTESIAN_POINT('Ctrl Pts',(11.0067681889689,19.1983564165478,-18.7521292867632)) ;
#35292 = CARTESIAN_POINT('Ctrl Pts',(10.9526356997833,19.2293915607565,-18.7507040318191)) ;
#35293 = CARTESIAN_POINT('Ctrl Pts',(10.8983728613506,19.2601972283926,-18.7492787768749)) ;
#35294 = CARTESIAN_POINT('Ctrl Pts',(10.8439816606655,19.2907723226845,-18.7478535219308)) ;
#35295 = CARTESIAN_POINT('Ctrl Pts',(10.4457736613714,19.5146182200516,-18.7374189679468)) ;
#35296 = CARTESIAN_POINT('Ctrl Pts',(10.0405806954128,19.726158913574,-18.7269844139629)) ;
#35297 = CARTESIAN_POINT('Ctrl Pts',(9.62918811115828,19.9249735603947,-18.716549859979)) ;
#35298 = CARTESIAN_POINT('Ctrl Pts',(9.22858174703272,20.1185755256369,-18.7063888874852)) ;
#35299 = CARTESIAN_POINT('Ctrl Pts',(8.82209691497259,20.3001101209105,-18.6962279149914)) ;
#35300 = CARTESIAN_POINT('Ctrl Pts',(8.41048263201501,20.4692358665162,-18.6860669424976)) ;
#35301 = CARTESIAN_POINT('Ctrl Pts',(7.99891062035745,20.6383442435188,-18.675907013499)) ;
#35302 = CARTESIAN_POINT('Ctrl Pts',(7.58221042228983,20.7950462291208,-18.6657470845003)) ;
#35303 = CARTESIAN_POINT('Ctrl Pts',(7.16115120186113,20.9390484150207,-18.6555871555017)) ;
#35304 = CARTESIAN_POINT('Ctrl Pts',(6.74011703542317,21.0830420324599,-18.6454278310422)) ;
#35305 = CARTESIAN_POINT('Ctrl Pts',(6.31472458195684,21.2143372856418,-18.6352685065827)) ;
#35306 = CARTESIAN_POINT('Ctrl Pts',(5.88576003712376,21.3326900284024,-18.6251091821232)) ;
#35307 = CARTESIAN_POINT('Ctrl Pts',(5.43648214166529,21.4566472920729,-18.6144687691393)) ;
#35308 = CARTESIAN_POINT('Ctrl Pts',(4.98328597402742,21.5664067363189,-18.6038283561555)) ;
#35309 = CARTESIAN_POINT('Ctrl Pts',(4.52709106641022,21.6617469641515,-18.5931879431716)) ;
#35310 = CARTESIAN_POINT('Ctrl Pts',(4.09147980422567,21.7527854134847,-18.5830276286818)) ;
#35311 = CARTESIAN_POINT('Ctrl Pts',(3.65313463063065,21.8306768528102,-18.5728673141919)) ;
#35312 = CARTESIAN_POINT('Ctrl Pts',(3.21286681761231,21.8952808128781,-18.5627069997021)) ;
#35313 = CARTESIAN_POINT('Ctrl Pts',(2.77257919737902,21.9598876794144,-18.5525462281097)) ;
#35314 = CARTESIAN_POINT('Ctrl Pts',(2.33036899234188,22.011205841337,-18.5423854565173)) ;
#35315 = CARTESIAN_POINT('Ctrl Pts',(1.88705457087286,22.049146471214,-18.5322246849249)) ;
#35316 = CARTESIAN_POINT('Ctrl Pts',(1.4436663280189,22.0870934190217,-18.5220622213455)) ;
#35317 = CARTESIAN_POINT('Ctrl Pts',(0.999173730027711,22.1116583641229,-18.5118997577662)) ;
#35318 = CARTESIAN_POINT('Ctrl Pts',(0.554399116588597,22.1228044488493,-18.5017372941868)) ;
#35319 = CARTESIAN_POINT('Ctrl Pts',(0.491476608361625,22.1243812915618,-18.5002996048968)) ;
#35320 = CARTESIAN_POINT('Ctrl Pts',(0.42854845840298,22.1256896554998,-18.4988619156069)) ;
#35321 = CARTESIAN_POINT('Ctrl Pts',(0.365616996697635,22.1267295205194,-18.497424226317)) ;
#35322 = CARTESIAN_POINT('Ctrl Pts',(-0.0911310218380175,22.1342767198753,
-18.486989672333)) ;
#35323 = CARTESIAN_POINT('Ctrl Pts',(-0.548172161965109,22.1276775334204,
-18.4765551183491)) ;
#35324 = CARTESIAN_POINT('Ctrl Pts',(-1.00461540528293,22.106935177676,-18.4661205643652)) ;
#35325 = CARTESIAN_POINT('Ctrl Pts',(-1.44907797800853,22.0867372649376,-18.4559598953733)) ;
#35326 = CARTESIAN_POINT('Ctrl Pts',(-1.8929733966678,22.0531291368785,-18.4457992263815)) ;
#35327 = CARTESIAN_POINT('Ctrl Pts',(-2.33548041515253,22.0061665515132,-18.4356385573896)) ;
#35328 = CARTESIAN_POINT('Ctrl Pts',(-2.77794173212602,21.9592088163786,-18.4254789377775)) ;
#35329 = CARTESIAN_POINT('Ctrl Pts',(-3.21901470712191,21.8988994031436,-18.4153193181654)) ;
#35330 = CARTESIAN_POINT('Ctrl Pts',(-3.65788322850045,21.8253459388197,-18.4051596985533)) ;
#35331 = CARTESIAN_POINT('Ctrl Pts',(-4.09672540761267,21.7517968894057,-18.3950006887535)) ;
#35332 = CARTESIAN_POINT('Ctrl Pts',(-4.53336317109265,21.6650054150248,-18.3848416789537)) ;
#35333 = CARTESIAN_POINT('Ctrl Pts',(-4.96698884890711,21.5651305777946,-18.3746826691539)) ;
#35334 = CARTESIAN_POINT('Ctrl Pts',(-5.42117256714812,21.4605207097616,-18.364042024283)) ;
#35335 = CARTESIAN_POINT('Ctrl Pts',(-5.87205145844143,21.3415571265267,-18.3534013794121)) ;
#35336 = CARTESIAN_POINT('Ctrl Pts',(-6.31871123447953,21.2084823454617,-18.3427607345412)) ;
#35337 = CARTESIAN_POINT('Ctrl Pts',(-6.74519466056983,21.0814187691124,-18.3326007449388)) ;
#35338 = CARTESIAN_POINT('Ctrl Pts',(-7.16783141749581,20.9414905278016,-18.3224407553364)) ;
#35339 = CARTESIAN_POINT('Ctrl Pts',(-7.58584107653467,20.7889598158268,-18.312280765734)) ;
#35340 = CARTESIAN_POINT('Ctrl Pts',(-8.00386942639121,20.6364222836178,-18.3021203218394)) ;
#35341 = CARTESIAN_POINT('Ctrl Pts',(-8.41727005014962,20.4712812357829,-18.2919598779449)) ;
#35342 = CARTESIAN_POINT('Ctrl Pts',(-8.82528083322448,20.2938476705927,-18.2817994340503)) ;
#35343 = CARTESIAN_POINT('Ctrl Pts',(-9.2333594473503,20.1163846073949,-18.2716373010005)) ;
#35344 = CARTESIAN_POINT('Ctrl Pts',(-9.63604621986356,19.9266250350328,-18.2614751679506)) ;
#35345 = CARTESIAN_POINT('Ctrl Pts',(-10.0326002557977,19.7249275580385,-18.2513130349007)) ;
#35346 = CARTESIAN_POINT('Ctrl Pts',(-10.088768307615,19.6963590571215,-18.2498736668348)) ;
#35347 = CARTESIAN_POINT('Ctrl Pts',(-10.1448133629315,19.6675511343935,-18.2484342987689)) ;
#35348 = CARTESIAN_POINT('Ctrl Pts',(-10.2007333551877,19.6385048839992,-18.246994930703)) ;
#35349 = CARTESIAN_POINT('Ctrl Pts',(-10.6061197131374,19.427937014006,-18.2365603767191)) ;
#35350 = CARTESIAN_POINT('Ctrl Pts',(-11.0050361639793,19.204785476768,-18.2261258227352)) ;
#35351 = CARTESIAN_POINT('Ctrl Pts',(-11.3967005232772,18.9694768574474,-18.2156912687513)) ;
#35352 = CARTESIAN_POINT('Ctrl Pts',(-11.7781177315545,18.7403246393959,-18.2055297149727)) ;
#35353 = CARTESIAN_POINT('Ctrl Pts',(-12.1526572685521,18.4996434734602,-18.1953681611942)) ;
#35354 = CARTESIAN_POINT('Ctrl Pts',(-12.519623122867,18.2478730794543,-18.1852066074156)) ;
#35355 = CARTESIAN_POINT('Ctrl Pts',(-12.8865513804556,17.9961284800625,-18.1750460947179)) ;
#35356 = CARTESIAN_POINT('Ctrl Pts',(-13.2459073161222,17.7332970517887,-18.1648855820203)) ;
#35357 = CARTESIAN_POINT('Ctrl Pts',(-13.5970241052032,17.4598616989088,-18.1547250693226)) ;
#35358 = CARTESIAN_POINT('Ctrl Pts',(-13.9481200466894,17.1864425812806,-18.1445651599065)) ;
#35359 = CARTESIAN_POINT('Ctrl Pts',(-14.290977637916,16.9024209378865,-18.1344052504903)) ;
#35360 = CARTESIAN_POINT('Ctrl Pts',(-14.6249619430466,16.6083209032984,-18.1242453410741)) ;
#35361 = CARTESIAN_POINT('Ctrl Pts',(-14.9747273472437,16.3003243421072,-18.1136053655754)) ;
#35362 = CARTESIAN_POINT('Ctrl Pts',(-15.314760603478,15.9812742923543,-18.1029653900766)) ;
#35363 = CARTESIAN_POINT('Ctrl Pts',(-15.6443729734733,15.6518187227351,-18.0923254145779)) ;
#35364 = CARTESIAN_POINT('Ctrl Pts',(-15.9591441257327,15.3371973107145,-18.0821645175588)) ;
#35365 = CARTESIAN_POINT('Ctrl Pts',(-16.2644118172505,15.0130867972284,-18.0720036205397)) ;
#35366 = CARTESIAN_POINT('Ctrl Pts',(-16.559614118049,14.6800890775162,-18.0618427235205)) ;
#35367 = CARTESIAN_POINT('Ctrl Pts',(-16.8548296358653,14.3470764485816,-18.0516813715702)) ;
#35368 = CARTESIAN_POINT('Ctrl Pts',(-17.1399787121037,14.0051759916967,-18.0415200196198)) ;
#35369 = CARTESIAN_POINT('Ctrl Pts',(-17.4145387367278,13.6550238245675,-18.0313586676694)) ;
#35370 = CARTESIAN_POINT('Ctrl Pts',(-17.6891443441964,13.3048135246792,-18.0211956287169)) ;
#35371 = CARTESIAN_POINT('Ctrl Pts',(-17.9531572457499,12.9463489577964,-18.0110325897645)) ;
#35372 = CARTESIAN_POINT('Ctrl Pts',(-18.2060961372532,12.5802980292039,-18.0008695508121)) ;
#35373 = CARTESIAN_POINT('Ctrl Pts',(-18.2418015883866,12.5286254158486,-17.9994349122378)) ;
#35374 = CARTESIAN_POINT('Ctrl Pts',(-18.2772864393892,12.4768016790243,-17.9980002736635)) ;
#35375 = CARTESIAN_POINT('Ctrl Pts',(-18.3125494054851,12.4248287446615,-17.9965656350893)) ;
#35376 = CARTESIAN_POINT('Ctrl Pts',(-18.5690274689917,12.046814101087,-17.9861310811053)) ;
#35377 = CARTESIAN_POINT('Ctrl Pts',(-18.8138301175145,11.6608062419235,-17.9756965271214)) ;
#35378 = CARTESIAN_POINT('Ctrl Pts',(-19.0464720509751,11.2675524171811,-17.9652619731375)) ;
#35379 = CARTESIAN_POINT('Ctrl Pts',(-19.2730114206556,10.8846142587141,-17.9551011339146)) ;
#35380 = CARTESIAN_POINT('Ctrl Pts',(-19.4880197714198,10.4948056214014,-17.9449402946916)) ;
#35381 = CARTESIAN_POINT('Ctrl Pts',(-19.6910939541567,10.0988441888701,-17.9347794554686)) ;
#35382 = CARTESIAN_POINT('Ctrl Pts',(-19.8941472116954,9.70292355705174,-17.9246196632403)) ;
#35383 = CARTESIAN_POINT('Ctrl Pts',(-20.085268652827,9.30085160061508,-17.9144598710119)) ;
#35384 = CARTESIAN_POINT('Ctrl Pts',(-20.2641013384807,8.89337011521972,-17.9043000787835)) ;
#35385 = CARTESIAN_POINT('Ctrl Pts',(-20.4429233261946,8.48591300575116,-17.8941408943235)) ;
#35386 = CARTESIAN_POINT('Ctrl Pts',(-20.6094579348632,8.07304722399147,-17.8839817098635)) ;
#35387 = CARTESIAN_POINT('Ctrl Pts',(-20.763395883629,7.655535673106,-17.8738225254035)) ;
#35388 = CARTESIAN_POINT('Ctrl Pts',(-20.9246272438241,7.21824288217204,-17.8631820099095)) ;
#35389 = CARTESIAN_POINT('Ctrl Pts',(-21.0720395086345,6.77585376433237,-17.8525414944155)) ;
#35390 = CARTESIAN_POINT('Ctrl Pts',(-21.2053348525127,6.3292660597663,-17.8419009789215)) ;
#35391 = CARTESIAN_POINT('Ctrl Pts',(-21.3326128073726,5.90283878894843,-17.8317408111967)) ;
#35392 = CARTESIAN_POINT('Ctrl Pts',(-21.4470199752717,5.47258380592941,-17.821580643472)) ;
#35393 = CARTESIAN_POINT('Ctrl Pts',(-21.5483482822266,5.03929770606615,-17.8114204757472)) ;
#35394 = CARTESIAN_POINT('Ctrl Pts',(-21.6496811278202,4.60599219870317,-17.8012598529341)) ;
#35395 = CARTESIAN_POINT('Ctrl Pts',(-21.7379338920429,4.16965552728269,-17.791099230121)) ;
#35396 = CARTESIAN_POINT('Ctrl Pts',(-21.8129493646537,3.73109569396881,-17.7809386073079)) ;
#35397 = CARTESIAN_POINT('Ctrl Pts',(-21.8879773120214,3.29246293000324,-17.770776294826)) ;
#35398 = CARTESIAN_POINT('Ctrl Pts',(-21.9497635306201,2.85160649169889,-17.7606139823442)) ;
#35399 = CARTESIAN_POINT('Ctrl Pts',(-21.9982022631477,2.40934270126547,-17.7504516698623)) ;
#35400 = CARTESIAN_POINT('Ctrl Pts',(-22.005058613831,2.34674164868904,-17.7490132264)) ;
#35401 = CARTESIAN_POINT('Ctrl Pts',(-22.0116476255083,2.28411240874201,-17.7475747829376)) ;
#35402 = CARTESIAN_POINT('Ctrl Pts',(-22.017969082177,2.22145730519318,-17.7461363394753)) ;
#35403 = CARTESIAN_POINT('Ctrl Pts',(-22.0638253028726,1.76695347694492,-17.7357017854914)) ;
#35404 = CARTESIAN_POINT('Ctrl Pts',(-22.0956095704889,1.31097053574373,-17.7252672315075)) ;
#35405 = CARTESIAN_POINT('Ctrl Pts',(-22.1132503614142,0.854396579998724,
-17.7148326775236)) ;
#35406 = CARTESIAN_POINT('Ctrl Pts',(-22.1304291012946,0.409781298569257,
-17.7046714274177)) ;
#35407 = CARTESIAN_POINT('Ctrl Pts',(-22.1341957795088,-0.0353941912238496,
-17.6945101773119)) ;
#35408 = CARTESIAN_POINT('Ctrl Pts',(-22.1245370679452,-0.480306768243701,
-17.684348927206)) ;
#35409 = CARTESIAN_POINT('Ctrl Pts',(-22.1148793486058,-0.925173640091113,
-17.6741887209494)) ;
#35410 = CARTESIAN_POINT('Ctrl Pts',(-22.0917989993386,-1.36977742371452,
-17.6640285146929)) ;
#35411 = CARTESIAN_POINT('Ctrl Pts',(-22.0553348089614,-1.81329576382731,
-17.6538683084363)) ;
#35412 = CARTESIAN_POINT('Ctrl Pts',(-22.0188727914712,-2.25678767485438,
-17.6437087076225)) ;
#35413 = CARTESIAN_POINT('Ctrl Pts',(-21.969028545034,-2.69919404289627,-17.6335491068087)) ;
#35414 = CARTESIAN_POINT('Ctrl Pts',(-21.9058928204378,-3.13969660986405,
-17.6233895059949)) ;
#35415 = CARTESIAN_POINT('Ctrl Pts',(-21.8397704327511,-3.60103734359781,
-17.6127493008171)) ;
#35416 = CARTESIAN_POINT('Ctrl Pts',(-21.7590688864884,-4.06028956270628,
-17.6021090956393)) ;
#35417 = CARTESIAN_POINT('Ctrl Pts',(-21.6639530976092,-4.51652202995732,
-17.5914688904615)) ;
#35418 = CARTESIAN_POINT('Ctrl Pts',(-21.5731247600813,-4.9521893047067,-17.5813083045205)) ;
#35419 = CARTESIAN_POINT('Ctrl Pts',(-21.4691528313875,-5.38510277625743,
-17.5711477185795)) ;
#35420 = CARTESIAN_POINT('Ctrl Pts',(-21.3522331111678,-5.81446267756954,
-17.5609871326385)) ;
#35421 = CARTESIAN_POINT('Ctrl Pts',(-21.2353081576933,-6.24384179676661,
-17.5508260919159)) ;
#35422 = CARTESIAN_POINT('Ctrl Pts',(-21.1054343173727,-6.66966680711632,
-17.5406650511934)) ;
#35423 = CARTESIAN_POINT('Ctrl Pts',(-20.9628575586059,-7.09115209540037,
-17.5305040104708)) ;
#35424 = CARTESIAN_POINT('Ctrl Pts',(-20.8202571165975,-7.51270739606229,
-17.5203412819108)) ;
#35425 = CARTESIAN_POINT('Ctrl Pts',(-20.6649496135383,-7.9299213168805,-17.5101785533509)) ;
#35426 = CARTESIAN_POINT('Ctrl Pts',(-20.4972302370595,-8.34202539384011,
-17.5000158247909)) ;
#35427 = CARTESIAN_POINT('Ctrl Pts',(-20.4735270866502,-8.40026651734974,
-17.4985795644811)) ;
#35428 = CARTESIAN_POINT('Ctrl Pts',(-20.4495761114447,-8.45840561310341,
-17.4971433041712)) ;
#35429 = CARTESIAN_POINT('Ctrl Pts',(-20.4253782222638,-8.51644054402846,
-17.4957070438614)) ;
#35430 = CARTESIAN_POINT('Ctrl Pts',(-20.2495784878933,-8.93806928050909,
-17.4852724898775)) ;
#35431 = CARTESIAN_POINT('Ctrl Pts',(-20.060696399042,-9.35430734868467,-17.4748379358936)) ;
#35432 = CARTESIAN_POINT('Ctrl Pts',(-19.859091365861,-9.76433946485292,-17.4644033819097)) ;
#35433 = CARTESIAN_POINT('Ctrl Pts',(-19.6627703438885,-10.1636247545978,
-17.4542423146505)) ;
#35434 = CARTESIAN_POINT('Ctrl Pts',(-19.4543848809506,-10.5570250251441,
-17.4440812473913)) ;
#35435 = CARTESIAN_POINT('Ctrl Pts',(-19.2343146647519,-10.9438098685882,
-17.433920180132)) ;
#35436 = CARTESIAN_POINT('Ctrl Pts',(-19.0142670842641,-11.3305549285941,
-17.4237601580074)) ;
#35437 = CARTESIAN_POINT('Ctrl Pts',(-18.7825372646835,-11.7106857212213,
-17.4136001358827)) ;
#35438 = CARTESIAN_POINT('Ctrl Pts',(-18.5395503765572,-12.0834972957996,
-17.403440113758)) ;
#35439 = CARTESIAN_POINT('Ctrl Pts',(-18.2965779902041,-12.4562866204988,
-17.3932806979966)) ;
#35440 = CARTESIAN_POINT('Ctrl Pts',(-18.0423500028385,-12.8217574075939,
-17.3831212822352)) ;
#35441 = CARTESIAN_POINT('Ctrl Pts',(-17.777335347269,-13.1792330206746,-17.3729618664738)) ;
#35442 = CARTESIAN_POINT('Ctrl Pts',(-17.4997754018268,-13.5536308495433,
-17.3623215232883)) ;
#35443 = CARTESIAN_POINT('Ctrl Pts',(-17.2103831657475,-13.9192581433289,
-17.3516811801028)) ;
#35444 = CARTESIAN_POINT('Ctrl Pts',(-16.9097465941923,-14.2753740820583,
-17.3410408369173)) ;
#35445 = CARTESIAN_POINT('Ctrl Pts',(-16.6226705222947,-14.6154270712928,
-17.3308804365723)) ;
#35446 = CARTESIAN_POINT('Ctrl Pts',(-16.325342090823,-14.9468074772167,-17.3207200362273)) ;
#35447 = CARTESIAN_POINT('Ctrl Pts',(-16.0183138511908,-15.2689048863122,
-17.3105596358824)) ;
#35448 = CARTESIAN_POINT('Ctrl Pts',(-15.7112718618294,-15.5910167199836,
-17.3003987805214)) ;
#35449 = CARTESIAN_POINT('Ctrl Pts',(-15.3945293564791,-15.9038445617162,
-17.2902379251605)) ;
#35450 = CARTESIAN_POINT('Ctrl Pts',(-15.0686762885948,-16.2068143067057,
-17.2800770697995)) ;
#35451 = CARTESIAN_POINT('Ctrl Pts',(-14.7427690622244,-16.5098344068532,
-17.2699145256512)) ;
#35452 = CARTESIAN_POINT('Ctrl Pts',(-14.4077484158269,-16.8029929801262,
-17.2597519815029)) ;
#35453 = CARTESIAN_POINT('Ctrl Pts',(-14.064239445091,-17.0857544139452,-17.2495894373546)) ;
#35454 = CARTESIAN_POINT('Ctrl Pts',(-14.0156589628267,-17.1257437242425,
-17.2481522076522)) ;
#35455 = CARTESIAN_POINT('Ctrl Pts',(-13.9669087616435,-17.1655251488869,
-17.2467149779499)) ;
#35456 = CARTESIAN_POINT('Ctrl Pts',(-13.9179906627924,-17.205097238113,-17.2452777482476)) ;
#35457 = CARTESIAN_POINT('Ctrl Pts',(-13.562836199713,-17.4923979393284,-17.2348431942637)) ;
#35458 = CARTESIAN_POINT('Ctrl Pts',(-13.1987368800248,-17.7687352045356,
-17.2244086402798)) ;
#35459 = CARTESIAN_POINT('Ctrl Pts',(-12.8263965789861,-18.0335627611705,
-17.2139740862959)) ;
#35460 = CARTESIAN_POINT('Ctrl Pts',(-12.4638131708609,-18.2914507141593,
-17.2038129618213)) ;
#35461 = CARTESIAN_POINT('Ctrl Pts',(-12.0934153512721,-18.5384243082068,
-17.1936518373467)) ;
#35462 = CARTESIAN_POINT('Ctrl Pts',(-11.7158844814942,-18.7740215691466,
-17.1834907128721)) ;
#35463 = CARTESIAN_POINT('Ctrl Pts',(-11.338392430653,-19.0095946052194,-17.173330633197)) ;
#35464 = CARTESIAN_POINT('Ctrl Pts',(-10.9537689893333,-19.2337935232605,
-17.1631705535219)) ;
#35465 = CARTESIAN_POINT('Ctrl Pts',(-10.5627234232182,-19.446200373006,-17.1530104738468)) ;
#35466 = CARTESIAN_POINT('Ctrl Pts',(-10.1717011865675,-19.6585945507294,
-17.1428510003139)) ;
#35467 = CARTESIAN_POINT('Ctrl Pts',(-9.77425779222756,-19.8591979561205,
-17.132691526781)) ;
#35468 = CARTESIAN_POINT('Ctrl Pts',(-9.37112753809439,-20.0476383578533,
-17.1225320532481)) ;
#35469 = CARTESIAN_POINT('Ctrl Pts',(-8.9489179767631,-20.2449972475346,-17.1118917531969)) ;
#35470 = CARTESIAN_POINT('Ctrl Pts',(-8.52047057261104,-20.4290140579446,
-17.1012514531457)) ;
#35471 = CARTESIAN_POINT('Ctrl Pts',(-8.0866548242917,-20.5993167074847,-17.0906111530945)) ;
#35472 = CARTESIAN_POINT('Ctrl Pts',(-7.67240271472477,-20.7619392773433,
-17.0804506949744)) ;
#35473 = CARTESIAN_POINT('Ctrl Pts',(-7.25325591364203,-20.912057024724,-17.0702902368543)) ;
#35474 = CARTESIAN_POINT('Ctrl Pts',(-6.8299907847078,-21.0493957381989,-17.0601297787342)) ;
#35475 = CARTESIAN_POINT('Ctrl Pts',(-6.40670670611673,-21.186740600353,-17.0499688657286)) ;
#35476 = CARTESIAN_POINT('Ctrl Pts',(-5.97930415032894,-21.311305216929,-17.0398079527229)) ;
#35477 = CARTESIAN_POINT('Ctrl Pts',(-5.54857511661993,-21.4228651033826,
-17.0296470397173)) ;
#35478 = CARTESIAN_POINT('Ctrl Pts',(-5.1177745098352,-21.53444352744,-17.0194844383003)) ;
#35479 = CARTESIAN_POINT('Ctrl Pts',(-4.6836465428587,-21.6330128459855,-17.0093218368833)) ;
#35480 = CARTESIAN_POINT('Ctrl Pts',(-4.24699582430295,-21.7183991475167,
-16.9991592354663)) ;
#35481 = CARTESIAN_POINT('Ctrl Pts',(-4.18525617241255,-21.730472230896,-16.9977223078554)) ;
#35482 = CARTESIAN_POINT('Ctrl Pts',(-4.12346610193498,-21.7422818405832,
-16.9962853802446)) ;
#35483 = CARTESIAN_POINT('Ctrl Pts',(-4.06162790298059,-21.7538275675852,
-16.9948484526338)) ;
#35484 = CARTESIAN_POINT('Ctrl Pts',(-3.61186926570409,-21.8378013981717,
-16.984397459315)) ;
#35485 = CARTESIAN_POINT('Ctrl Pts',(-3.15947745055909,-21.9078281300336,
-16.9739464659962)) ;
#35486 = CARTESIAN_POINT('Ctrl Pts',(-2.70531145384119,-21.9637684608133,
-16.9634954726774)) ;
#35487 = CARTESIAN_POINT('Ctrl Pts',(-2.25124847500317,-22.0196961027208,
-16.9530468499438)) ;
#35488 = CARTESIAN_POINT('Ctrl Pts',(-1.7954123174551,-22.0615437046833,-16.9425982272102)) ;
#35489 = CARTESIAN_POINT('Ctrl Pts',(-1.33866864577018,-22.0892236468223,
-16.9321496044766)) ;
#35490 = CARTESIAN_POINT('Ctrl Pts',(-0.893168431085587,-22.1162222040653,
-16.9219581908686)) ;
#35491 = CARTESIAN_POINT('Ctrl Pts',(-0.44680503136645,-22.1297422163973,
-16.9117667772605)) ;
#35492 = CARTESIAN_POINT('Ctrl Pts',(-0.000385679535181172,-22.1297499966392,
-16.9015753636525)) ;
#35493 = CARTESIAN_POINT('Ctrl Pts',(-0.000394050632519626,-22.1297499964917,
-16.4359246717926)) ;
#35494 = CARTESIAN_POINT('Ctrl Pts',(-0.458270040802388,-22.12974184338,-16.4463776769714)) ;
#35495 = CARTESIAN_POINT('Ctrl Pts',(-0.91608658402974,-22.1155188134193,
-16.4568306821502)) ;
#35496 = CARTESIAN_POINT('Ctrl Pts',(-1.37297316201532,-22.0871179595457,
-16.467283687329)) ;
#35497 = CARTESIAN_POINT('Ctrl Pts',(-1.82999981297473,-22.0587083984956,
-16.4777398972058)) ;
#35498 = CARTESIAN_POINT('Ctrl Pts',(-2.28609572932389,-22.016112336254,-16.4881961070826)) ;
#35499 = CARTESIAN_POINT('Ctrl Pts',(-2.74039394844152,-21.9594188463594,
-16.4986523169594)) ;
#35500 = CARTESIAN_POINT('Ctrl Pts',(-3.17025376482808,-21.9057751116256,
-16.5085460481444)) ;
#35501 = CARTESIAN_POINT('Ctrl Pts',(-3.59850398566261,-21.8395102898116,
-16.5184397793293)) ;
#35502 = CARTESIAN_POINT('Ctrl Pts',(-4.02441617112775,-21.7607423941387,
-16.5283335105142)) ;
#35503 = CARTESIAN_POINT('Ctrl Pts',(-4.47361007063524,-21.6776687948833,
-16.5387680644981)) ;
#35504 = CARTESIAN_POINT('Ctrl Pts',(-4.92028896367183,-21.5806710394323,
-16.5492026184821)) ;
#35505 = CARTESIAN_POINT('Ctrl Pts',(-5.36358016922639,-21.4699288035797,
-16.559637172466)) ;
#35506 = CARTESIAN_POINT('Ctrl Pts',(-5.79525488918246,-21.3620885778997,
-16.5697982880316)) ;
#35507 = CARTESIAN_POINT('Ctrl Pts',(-6.22371696461821,-21.2412150662447,
-16.5799594035972)) ;
#35508 = CARTESIAN_POINT('Ctrl Pts',(-6.64817240571008,-21.1075256419708,
-16.5901205191629)) ;
#35509 = CARTESIAN_POINT('Ctrl Pts',(-7.07258420181503,-20.9738499644242,
-16.6002805899033)) ;
#35510 = CARTESIAN_POINT('Ctrl Pts',(-7.49298996764377,-20.827361075493,-16.6104406606437)) ;
#35511 = CARTESIAN_POINT('Ctrl Pts',(-7.90861102244079,-20.6683261721463,
-16.6206007313841)) ;
#35512 = CARTESIAN_POINT('Ctrl Pts',(-8.32420728126773,-20.5093007568288,
-16.6307601959742)) ;
#35513 = CARTESIAN_POINT('Ctrl Pts',(-8.73501918503367,-20.3377309044873,
-16.6409196605643)) ;
#35514 = CARTESIAN_POINT('Ctrl Pts',(-9.14028651728225,-20.1539325553225,
-16.6510791251545)) ;
#35515 = CARTESIAN_POINT('Ctrl Pts',(-9.56473494089009,-19.9614351262012,
-16.6617194319023)) ;
#35516 = CARTESIAN_POINT('Ctrl Pts',(-9.98310109258281,-19.7555239619668,
-16.6723597386501)) ;
#35517 = CARTESIAN_POINT('Ctrl Pts',(-10.3945369683939,-19.5366178310165,
-16.6830000453979)) ;
#35518 = CARTESIAN_POINT('Ctrl Pts',(-10.7874178722743,-19.3275839483412,
-16.6931604946402)) ;
#35519 = CARTESIAN_POINT('Ctrl Pts',(-11.1739794721254,-19.1067012528695,
-16.7033209438824)) ;
#35520 = CARTESIAN_POINT('Ctrl Pts',(-11.5535086814804,-18.8743813728942,
-16.7134813931247)) ;
#35521 = CARTESIAN_POINT('Ctrl Pts',(-11.9330548840379,-18.6420510909297,
-16.7236422972953)) ;
#35522 = CARTESIAN_POINT('Ctrl Pts',(-12.3055678724736,-18.3982827231497,
-16.7338032014659)) ;
#35523 = CARTESIAN_POINT('Ctrl Pts',(-12.6703621789704,-18.1435321069581,
-16.7439641056365)) ;
#35524 = CARTESIAN_POINT('Ctrl Pts',(-13.0352171056192,-17.8887391572628,
-16.7541266983081)) ;
#35525 = CARTESIAN_POINT('Ctrl Pts',(-13.3923505992489,-17.6229604440359,
-16.7642892909797)) ;
#35526 = CARTESIAN_POINT('Ctrl Pts',(-13.7411074210875,-17.3466942644596,
-16.7744518836513)) ;
#35527 = CARTESIAN_POINT('Ctrl Pts',(-13.7904210713462,-17.3076306737142,
-16.7758888578102)) ;
#35528 = CARTESIAN_POINT('Ctrl Pts',(-13.8395672951608,-17.2683574687375,
-16.7773258319691)) ;
#35529 = CARTESIAN_POINT('Ctrl Pts',(-13.8885442927298,-17.228876123862,-16.778762806128)) ;
#35530 = CARTESIAN_POINT('Ctrl Pts',(-14.2441896061347,-16.9421832686685,
-16.7891973601119)) ;
#35531 = CARTESIAN_POINT('Ctrl Pts',(-14.5910008705382,-16.6444374970597,
-16.7996319140958)) ;
#35532 = CARTESIAN_POINT('Ctrl Pts',(-14.9282958429325,-16.3362118708219,
-16.8100664680797)) ;
#35533 = CARTESIAN_POINT('Ctrl Pts',(-15.2567520107339,-16.0360632878367,
-16.8202275848908)) ;
#35534 = CARTESIAN_POINT('Ctrl Pts',(-15.5761840758257,-15.7259772360805,
-16.8303887017018)) ;
#35535 = CARTESIAN_POINT('Ctrl Pts',(-15.8859969457872,-15.406522518107,-16.8405498185128)) ;
#35536 = CARTESIAN_POINT('Ctrl Pts',(-16.1957779590629,-15.0871006482479,
-16.8507098905012)) ;
#35537 = CARTESIAN_POINT('Ctrl Pts',(-16.4959415931659,-14.7583122011488,
-16.8608699624896)) ;
#35538 = CARTESIAN_POINT('Ctrl Pts',(-16.7859299164886,-14.4207625284252,
-16.8710300344779)) ;
#35539 = CARTESIAN_POINT('Ctrl Pts',(-17.075900939101,-14.0832329939231,-16.8811895003162)) ;
#35540 = CARTESIAN_POINT('Ctrl Pts',(-17.3556977142044,-13.7369434521286,
-16.8913489661544)) ;
#35541 = CARTESIAN_POINT('Ctrl Pts',(-17.6248017328512,-13.3825333528516,
-16.9015084319926)) ;
#35542 = CARTESIAN_POINT('Ctrl Pts',(-17.9066422448772,-13.0113492867431,
-16.912148737805)) ;
#35543 = CARTESIAN_POINT('Ctrl Pts',(-18.1767533565653,-12.6312577288267,
-16.9227890436175)) ;
#35544 = CARTESIAN_POINT('Ctrl Pts',(-18.4345882334818,-12.24303033258,-16.9334293494299)) ;
#35545 = CARTESIAN_POINT('Ctrl Pts',(-18.6807953016649,-11.8723111724674,
-16.9435897999089)) ;
#35546 = CARTESIAN_POINT('Ctrl Pts',(-18.9158086482927,-11.4941738823983,
-16.9537502503878)) ;
#35547 = CARTESIAN_POINT('Ctrl Pts',(-19.1391967285628,-11.1093196752938,
-16.9639107008667)) ;
#35548 = CARTESIAN_POINT('Ctrl Pts',(-19.3625948107562,-10.7244482368212,
-16.9740716062672)) ;
#35549 = CARTESIAN_POINT('Ctrl Pts',(-19.5743664734542,-10.3328594801228,
-16.9842325116676)) ;
#35550 = CARTESIAN_POINT('Ctrl Pts',(-19.7741254912944,-9.93528037435493,
-16.9943934170681)) ;
#35551 = CARTESIAN_POINT('Ctrl Pts',(-19.973917704069,-9.53763520091962,-17.0045560109559)) ;
#35552 = CARTESIAN_POINT('Ctrl Pts',(-20.161693180309,-9.13399789449304,-17.0147186048438)) ;
#35553 = CARTESIAN_POINT('Ctrl Pts',(-20.3371124785335,-8.72511840022681,
-17.0248811987317)) ;
#35554 = CARTESIAN_POINT('Ctrl Pts',(-20.361916368469,-8.66730376936636,-17.0263181664017)) ;
#35555 = CARTESIAN_POINT('Ctrl Pts',(-20.3864732954977,-8.6093843636827,-17.0277551340718)) ;
#35556 = CARTESIAN_POINT('Ctrl Pts',(-20.4107823774842,-8.55136233599528,
-17.0291921017419)) ;
#35557 = CARTESIAN_POINT('Ctrl Pts',(-20.587303000441,-8.13003484702398,-17.0396266557258)) ;
#35558 = CARTESIAN_POINT('Ctrl Pts',(-20.7507961995129,-7.70318525587862,
-17.0500612097097)) ;
#35559 = CARTESIAN_POINT('Ctrl Pts',(-20.9009343320342,-7.27164211925304,
-17.0604957636936)) ;
#35560 = CARTESIAN_POINT('Ctrl Pts',(-21.0471380495211,-6.85140770064717,
-17.070656877044)) ;
#35561 = CARTESIAN_POINT('Ctrl Pts',(-21.180677613898,-6.42672281012036,-17.0808179903944)) ;
#35562 = CARTESIAN_POINT('Ctrl Pts',(-21.3013000227658,-5.99837081236371,
-17.0909791037448)) ;
#35563 = CARTESIAN_POINT('Ctrl Pts',(-21.4219100285112,-5.57006286033871,
-17.1011391722683)) ;
#35564 = CARTESIAN_POINT('Ctrl Pts',(-21.5296054696472,-5.13808877515966,
-17.1112992407919)) ;
#35565 = CARTESIAN_POINT('Ctrl Pts',(-21.6241834146182,-4.70324640152428,
-17.1214593093154)) ;
#35566 = CARTESIAN_POINT('Ctrl Pts',(-21.718755717089,-4.26842997049313,-17.1316187716914)) ;
#35567 = CARTESIAN_POINT('Ctrl Pts',(-21.8002120381128,-3.8307458171197,-17.1417782340674)) ;
#35568 = CARTESIAN_POINT('Ctrl Pts',(-21.8684003411913,-3.3910030344847,-17.1519376964434)) ;
#35569 = CARTESIAN_POINT('Ctrl Pts',(-21.9398159877889,-2.93044728312142,
-17.1625780048527)) ;
#35570 = CARTESIAN_POINT('Ctrl Pts',(-21.9966774498719,-2.46763361794661,
-17.1732183132621)) ;
#35571 = CARTESIAN_POINT('Ctrl Pts',(-22.0388706425406,-2.00350090188735,
-17.1838586216715)) ;
#35572 = CARTESIAN_POINT('Ctrl Pts',(-22.0791609878698,-1.56029984916074,
-17.1940190687272)) ;
#35573 = CARTESIAN_POINT('Ctrl Pts',(-22.1060766607646,-1.1158963185534,-17.204179515783)) ;
#35574 = CARTESIAN_POINT('Ctrl Pts',(-22.119571497574,-0.671112379720387,
-17.2143399628387)) ;
#35575 = CARTESIAN_POINT('Ctrl Pts',(-22.1330669386263,-0.226308525301396,
-17.2245008648373)) ;
#35576 = CARTESIAN_POINT('Ctrl Pts',(-22.133140338349,0.218875541893517,-17.2346617668358)) ;
#35577 = CARTESIAN_POINT('Ctrl Pts',(-22.1197976484675,0.663616646378586,
-17.2448226688344)) ;
#35578 = CARTESIAN_POINT('Ctrl Pts',(-22.1064527413112,1.10843165749302,-17.2549852593614)) ;
#35579 = CARTESIAN_POINT('Ctrl Pts',(-22.0796872966979,1.55280332939547,-17.2651478498885)) ;
#35580 = CARTESIAN_POINT('Ctrl Pts',(-22.0395593478398,1.99591052293076,-17.2753104404155)) ;
#35581 = CARTESIAN_POINT('Ctrl Pts',(-22.0338852742473,2.05856567718201,-17.2767474260622)) ;
#35582 = CARTESIAN_POINT('Ctrl Pts',(-22.0279441178173,2.12119555697544,-17.2781844117089)) ;
#35583 = CARTESIAN_POINT('Ctrl Pts',(-22.0217361263272,2.18379784891302,-17.2796213973557)) ;
#35584 = CARTESIAN_POINT('Ctrl Pts',(-21.9766573028303,2.63837928209217,-17.2900559513396)) ;
#35585 = CARTESIAN_POINT('Ctrl Pts',(-21.9174923657914,3.09162326122403,-17.3004905053235)) ;
#35586 = CARTESIAN_POINT('Ctrl Pts',(-21.8443471114585,3.54264510452476,-17.3109250593074)) ;
#35587 = CARTESIAN_POINT('Ctrl Pts',(-21.7731186004249,3.98184809363163,-17.3210861798114)) ;
#35588 = CARTESIAN_POINT('Ctrl Pts',(-21.688633135833,4.41894367839406,-17.3312473003155)) ;
#35589 = CARTESIAN_POINT('Ctrl Pts',(-21.5910406832882,4.8531224253148,-17.3414084208195)) ;
#35590 = CARTESIAN_POINT('Ctrl Pts',(-21.493458265736,5.2872565275897,-17.3515684965013)) ;
#35591 = CARTESIAN_POINT('Ctrl Pts',(-21.3827716026278,5.71847416723885,-17.361728572183)) ;
#35592 = CARTESIAN_POINT('Ctrl Pts',(-21.2591815922954,6.1459769840366,-17.3718886478648)) ;
#35593 = CARTESIAN_POINT('Ctrl Pts',(-21.1355989554263,6.57345429572838,-17.3820481173896)) ;
#35594 = CARTESIAN_POINT('Ctrl Pts',(-20.9991145730536,6.99721700689574,-17.3922075869144)) ;
#35595 = CARTESIAN_POINT('Ctrl Pts',(-20.8499794644913,7.41648106535637,-17.4023670564392)) ;
#35596 = CARTESIAN_POINT('Ctrl Pts',(-20.6937859992954,7.85558830679939,-17.4130073594834)) ;
#35597 = CARTESIAN_POINT('Ctrl Pts',(-20.5237156435815,8.28976057934957,-17.4236476625276)) ;
#35598 = CARTESIAN_POINT('Ctrl Pts',(-20.3401145130157,8.71811772459553,-17.4342879655718)) ;
#35599 = CARTESIAN_POINT('Ctrl Pts',(-20.164793297579,9.12715711947368,-17.4444484196854)) ;
#35600 = CARTESIAN_POINT('Ctrl Pts',(-19.9771346756949,9.53089399517996,-17.454608873799)) ;
#35601 = CARTESIAN_POINT('Ctrl Pts',(-19.7774889727994,9.92858323192686,-17.4647693279127)) ;
#35602 = CARTESIAN_POINT('Ctrl Pts',(-19.5778343315327,10.326290273685,-17.4749302369217)) ;
#35603 = CARTESIAN_POINT('Ctrl Pts',(-19.3661916420715,10.7179489314522,-17.4850911459307)) ;
#35604 = CARTESIAN_POINT('Ctrl Pts',(-19.14295760106,11.1028378960751,-17.4952520549397)) ;
#35605 = CARTESIAN_POINT('Ctrl Pts',(-18.9196864652342,11.4877908177207,-17.5054146523876)) ;
#35606 = CARTESIAN_POINT('Ctrl Pts',(-18.6848202443778,11.8659715999616,-17.5155772498355)) ;
#35607 = CARTESIAN_POINT('Ctrl Pts',(-18.4388004822799,12.2366854922881,-17.5257398472834)) ;
#35608 = CARTESIAN_POINT('Ctrl Pts',(-18.4040143220296,12.289102878418,-17.5271767958455)) ;
#35609 = CARTESIAN_POINT('Ctrl Pts',(-18.369005242705,12.3413710274821,-17.5286137444075)) ;
#35610 = CARTESIAN_POINT('Ctrl Pts',(-18.3337745623043,12.3934880223892,-17.5300506929695)) ;
#35611 = CARTESIAN_POINT('Ctrl Pts',(-18.0779432498685,12.7719410938493,-17.5404852469535)) ;
#35612 = CARTESIAN_POINT('Ctrl Pts',(-17.810356562303,13.1425189796053,-17.5509198009374)) ;
#35613 = CARTESIAN_POINT('Ctrl Pts',(-17.5315282776837,13.5044937450937,-17.5613543549213)) ;
#35614 = CARTESIAN_POINT('Ctrl Pts',(-17.2600068850294,13.8569827064104,-17.5715154640545)) ;
#35615 = CARTESIAN_POINT('Ctrl Pts',(-16.9778256938762,14.2013134889568,-17.5816765731877)) ;
#35616 = CARTESIAN_POINT('Ctrl Pts',(-16.6855015517371,14.5368453603069,-17.5918376823209)) ;
#35617 = CARTESIAN_POINT('Ctrl Pts',(-16.3932074679945,14.8723427304013,-17.6019977466322)) ;
#35618 = CARTESIAN_POINT('Ctrl Pts',(-16.0907726672864,15.1990428235145,-17.6121578109436)) ;
#35619 = CARTESIAN_POINT('Ctrl Pts',(-15.7787535362038,15.516338869277,-17.6223178752549)) ;
#35620 = CARTESIAN_POINT('Ctrl Pts',(-15.4667530197208,15.833615985627,-17.6324773334319)) ;
#35621 = CARTESIAN_POINT('Ctrl Pts',(-15.1451694761089,16.1414900118586,-17.6426367916089)) ;
#35622 = CARTESIAN_POINT('Ctrl Pts',(-14.8145965786543,16.4393905992352,-17.6527962497858)) ;
#35623 = CARTESIAN_POINT('Ctrl Pts',(-14.4683774631192,16.7513910042083,-17.6634365613523)) ;
#35624 = CARTESIAN_POINT('Ctrl Pts',(-14.1122978043987,17.0524510061868,-17.6740768729187)) ;
#35625 = CARTESIAN_POINT('Ctrl Pts',(-13.7470806382558,17.341960932599,-17.6847171844852)) ;
#35626 = CARTESIAN_POINT('Ctrl Pts',(-13.3983344431678,17.6184142174838,-17.6948776274144)) ;
#35627 = CARTESIAN_POINT('Ctrl Pts',(-13.0412567961562,17.8843359100162,-17.7050380703436)) ;
#35628 = CARTESIAN_POINT('Ctrl Pts',(-12.6765102147787,18.1392371349269,-17.7151985132728)) ;
#35629 = CARTESIAN_POINT('Ctrl Pts',(-12.3117473003179,18.3941497741267,-17.7253594111791)) ;
#35630 = CARTESIAN_POINT('Ctrl Pts',(-11.9393149548486,18.6380408301885,-17.7355203090854)) ;
#35631 = CARTESIAN_POINT('Ctrl Pts',(-11.5599051650042,18.8704644256205,-17.7456812069918)) ;
#35632 = CARTESIAN_POINT('Ctrl Pts',(-11.1804323228982,19.1029266463957,-17.7558437934882)) ;
#35633 = CARTESIAN_POINT('Ctrl Pts',(-10.7939799152298,19.3239174788007,-17.7660063799845)) ;
#35634 = CARTESIAN_POINT('Ctrl Pts',(-10.4012667501909,19.5330357357445,-17.7761689664809)) ;
#35635 = CARTESIAN_POINT('Ctrl Pts',(-10.3457364271116,19.5626054201954,-17.7776059738484)) ;
#35636 = CARTESIAN_POINT('Ctrl Pts',(-10.290080963963,19.5919377939813,-17.7790429812159)) ;
#35637 = CARTESIAN_POINT('Ctrl Pts',(-10.234302432103,19.6210317973024,-17.7804799885833)) ;
#35638 = CARTESIAN_POINT('Ctrl Pts',(-9.82927729791871,19.8322923343968,-17.7909145425673)) ;
#35639 = CARTESIAN_POINT('Ctrl Pts',(-9.41765613265564,20.0310348947837,-17.8013490965512)) ;
#35640 = CARTESIAN_POINT('Ctrl Pts',(-9.00023706922651,20.2168634501057,-17.8117836505351)) ;
#35641 = CARTESIAN_POINT('Ctrl Pts',(-8.59375629880124,20.3978224453988,-17.8219447713703)) ;
#35642 = CARTESIAN_POINT('Ctrl Pts',(-8.18177782754204,20.5665354915101,-17.8321058922055)) ;
#35643 = CARTESIAN_POINT('Ctrl Pts',(-7.76506102216589,20.7226847291691,-17.8422670130407)) ;
#35644 = CARTESIAN_POINT('Ctrl Pts',(-7.34838706667009,20.8788179104175,-17.8524270890349)) ;
#35645 = CARTESIAN_POINT('Ctrl Pts',(-6.9269759651681,21.0223897832525,-17.8625871650291)) ;
#35646 = CARTESIAN_POINT('Ctrl Pts',(-6.50160571582377,21.1531311672402,-17.8727472410233)) ;
#35647 = CARTESIAN_POINT('Ctrl Pts',(-6.07626084515955,21.2838647508616,-17.8829067108413)) ;
#35648 = CARTESIAN_POINT('Ctrl Pts',(-5.64695751792443,21.4017693075676,-17.8930661806593)) ;
#35649 = CARTESIAN_POINT('Ctrl Pts',(-5.21448921269231,21.5066254283004,-17.9032256504773)) ;
#35650 = CARTESIAN_POINT('Ctrl Pts',(-4.76155280893994,21.6164442373588,-17.9138659532873)) ;
#35651 = CARTESIAN_POINT('Ctrl Pts',(-4.30514490389635,21.7119497426604,-17.9245062560973)) ;
#35652 = CARTESIAN_POINT('Ctrl Pts',(-3.84619147011417,21.7929494616429,-17.9351465589073)) ;
#35653 = CARTESIAN_POINT('Ctrl Pts',(-3.4079355765569,21.8702963156102,-17.9453070132638)) ;
#35654 = CARTESIAN_POINT('Ctrl Pts',(-2.96735888389062,21.9344165972658,-17.9554674676203)) ;
#35655 = CARTESIAN_POINT('Ctrl Pts',(-2.52527668758332,21.9851953076075,-17.9656279219769)) ;
#35656 = CARTESIAN_POINT('Ctrl Pts',(-2.08317469951773,22.035976291282,-17.9757888312109)) ;
#35657 = CARTESIAN_POINT('Ctrl Pts',(-1.63956730143142,22.0734144864172,-17.985949740445)) ;
#35658 = CARTESIAN_POINT('Ctrl Pts',(-1.19527526488837,22.0974467326804,-17.996110649679)) ;
#35659 = CARTESIAN_POINT('Ctrl Pts',(-0.750909401426862,22.121482972323,-18.0062732473265)) ;
#35660 = CARTESIAN_POINT('Ctrl Pts',(-0.305858901380434,22.1321087996347,
-18.0164358449739)) ;
#35661 = CARTESIAN_POINT('Ctrl Pts',(0.139053121511222,22.1293131229123,-18.0265984426213)) ;
#35662 = CARTESIAN_POINT('Ctrl Pts',(0.201961750205417,22.1289178263596,-18.0280353898133)) ;
#35663 = CARTESIAN_POINT('Ctrl Pts',(0.264867610527304,22.1282542823854,-18.0294723370053)) ;
#35664 = CARTESIAN_POINT('Ctrl Pts',(0.327768376633555,22.1273225437191,-18.0309092841973)) ;
#35665 = CARTESIAN_POINT('Ctrl Pts',(0.784529378868009,22.1205566183833,-18.0413438381812)) ;
#35666 = CARTESIAN_POINT('Ctrl Pts',(1.24113991677261,22.0996420266961,-18.0517783921651)) ;
#35667 = CARTESIAN_POINT('Ctrl Pts',(1.69670955080554,22.0646099390564,-18.062212946149)) ;
#35668 = CARTESIAN_POINT('Ctrl Pts',(2.14034132093769,22.0304958412544,-18.0723740703957)) ;
#35669 = CARTESIAN_POINT('Ctrl Pts',(2.58298580001337,21.9829946786199,-18.0825351946423)) ;
#35670 = CARTESIAN_POINT('Ctrl Pts',(3.02382382315773,21.9221879507727,-18.092696318889)) ;
#35671 = CARTESIAN_POINT('Ctrl Pts',(3.46461651891799,21.861387475131,-18.1028563983592)) ;
#35672 = CARTESIAN_POINT('Ctrl Pts',(3.90360290244921,21.7872841983707,-18.1130164778295)) ;
#35673 = CARTESIAN_POINT('Ctrl Pts',(4.3399705682238,21.700011302519,-18.1231765572997)) ;
#35674 = CARTESIAN_POINT('Ctrl Pts',(4.7763122016556,21.6127436130978,-18.1333360306511)) ;
#35675 = CARTESIAN_POINT('Ctrl Pts',(5.21003520441906,21.5123079192163,-18.1434955040024)) ;
#35676 = CARTESIAN_POINT('Ctrl Pts',(5.64033722181922,21.3988885479284,-18.1536549773538)) ;
#35677 = CARTESIAN_POINT('Ctrl Pts',(6.09100454339223,21.2801012724663,-18.1642952775586)) ;
#35678 = CARTESIAN_POINT('Ctrl Pts',(6.53791902154512,21.1470718784239,-18.1749355777633)) ;
#35679 = CARTESIAN_POINT('Ctrl Pts',(6.98017455454659,21.0000713867968,-18.1855758779681)) ;
#35680 = CARTESIAN_POINT('Ctrl Pts',(7.40248583158888,20.8597001292037,-18.1957363359664)) ;
#35681 = CARTESIAN_POINT('Ctrl Pts',(7.82054879569433,20.7065899384987,-18.2058967939648)) ;
#35682 = CARTESIAN_POINT('Ctrl Pts',(8.23359155226314,20.5410273650809,-18.2160572519631)) ;
#35683 = CARTESIAN_POINT('Ctrl Pts',(8.64665280167992,20.3754573790564,-18.2262181648679)) ;
#35684 = CARTESIAN_POINT('Ctrl Pts',(9.0546931823239,20.1974339839893,-18.2363790777726)) ;
#35685 = CARTESIAN_POINT('Ctrl Pts',(9.45696063420162,20.0072919363331,-18.2465399906774)) ;
#35686 = CARTESIAN_POINT('Ctrl Pts',(9.85929493094365,19.8171182927343,-18.2567025920231)) ;
#35687 = CARTESIAN_POINT('Ctrl Pts',(10.2558541746451,19.614822070914,-18.2668651933688)) ;
#35688 = CARTESIAN_POINT('Ctrl Pts',(10.6459090061464,19.4007849453405,-18.2770277947145)) ;
#35689 = CARTESIAN_POINT('Ctrl Pts',(10.7010603234539,19.3705214324322,-18.27846472308)) ;
#35690 = CARTESIAN_POINT('Ctrl Pts',(10.7560816439118,19.3400232678949,-18.2799016514455)) ;
#35691 = CARTESIAN_POINT('Ctrl Pts',(10.8109709466575,19.3092916041223,-18.281338579811)) ;
#35692 = CARTESIAN_POINT('Ctrl Pts',(11.2095610269893,19.0861272402275,-18.291773133795)) ;
#35693 = CARTESIAN_POINT('Ctrl Pts',(11.6012903702668,18.8505879952913,-18.3022076877789)) ;
#35694 = CARTESIAN_POINT('Ctrl Pts',(11.9853904837859,18.6031247378948,-18.3126422417628)) ;
#35695 = CARTESIAN_POINT('Ctrl Pts',(12.3594234447549,18.362147420687,-18.3228033091138)) ;
#35696 = CARTESIAN_POINT('Ctrl Pts',(12.7262217752393,18.1098632747737,-18.3329643764648)) ;
#35697 = CARTESIAN_POINT('Ctrl Pts',(13.0851036283453,17.8467335414065,-18.3431254438158)) ;
#35698 = CARTESIAN_POINT('Ctrl Pts',(13.4439485754045,17.5836308673018,-18.3532854662412)) ;
#35699 = CARTESIAN_POINT('Ctrl Pts',(13.794878486179,17.309684969259,-18.3634454886666)) ;
#35700 = CARTESIAN_POINT('Ctrl Pts',(14.1372420373358,17.0253993386436,-18.373605511092)) ;
#35701 = CARTESIAN_POINT('Ctrl Pts',(14.4795851627889,16.7411306687532,-18.3837649273618)) ;
#35702 = CARTESIAN_POINT('Ctrl Pts',(14.8133627731231,16.4465236453209,-18.3939243436315)) ;
#35703 = CARTESIAN_POINT('Ctrl Pts',(15.1379567085441,16.1421219718085,-18.4040837599013)) ;
#35704 = CARTESIAN_POINT('Ctrl Pts',(15.4779162794496,15.8233105245892,-18.4147241028616)) ;
#35705 = CARTESIAN_POINT('Ctrl Pts',(15.8078016088646,15.4937550079356,-18.4253644458219)) ;
#35706 = CARTESIAN_POINT('Ctrl Pts',(16.1269444809372,15.1541247444803,-18.4360047887822)) ;
#35707 = CARTESIAN_POINT('Ctrl Pts',(16.4316921460637,14.8298137889445,-18.446165190148)) ;
#35708 = CARTESIAN_POINT('Ctrl Pts',(16.7266447332537,14.4963169159911,-18.4563255915139)) ;
#35709 = CARTESIAN_POINT('Ctrl Pts',(17.0112594907531,14.154253268921,-18.4664859928797)) ;
#35710 = CARTESIAN_POINT('Ctrl Pts',(17.2958869991246,13.8121742972422,-18.4766468494362)) ;
#35711 = CARTESIAN_POINT('Ctrl Pts',(17.5701756074771,13.4615279625757,-18.4868077059926)) ;
#35712 = CARTESIAN_POINT('Ctrl Pts',(17.8336229367823,13.1029663821279,-18.4969685625491)) ;
#35713 = CARTESIAN_POINT('Ctrl Pts',(18.0971140586121,12.7443451984307,-18.5071311081322)) ;
#35714 = CARTESIAN_POINT('Ctrl Pts',(18.34976016463,12.3778063249207,-18.5172936537154)) ;
#35715 = CARTESIAN_POINT('Ctrl Pts',(18.5911011573929,12.004032356591,-18.5274561992985)) ;
#35716 = CARTESIAN_POINT('Ctrl Pts',(18.6252325072704,11.9511718377786,-18.528893424674)) ;
#35717 = CARTESIAN_POINT('Ctrl Pts',(18.6591378185395,11.8981666586563,-18.5303306500495)) ;
#35718 = CARTESIAN_POINT('Ctrl Pts',(18.6928158607279,11.8450187952329,-18.5317678754249)) ;
#35719 = CARTESIAN_POINT('Ctrl Pts',(18.937325424281,11.4591542958431,-18.5422024294089)) ;
#35720 = CARTESIAN_POINT('Ctrl Pts',(19.1699147805733,11.0656664148644,-18.5526369833928)) ;
#35721 = CARTESIAN_POINT('Ctrl Pts',(19.3901223208208,10.6653172220102,-18.5630715373767)) ;
#35722 = CARTESIAN_POINT('Ctrl Pts',(19.6045621556333,10.2754540289221,-18.5732327881228)) ;
#35723 = CARTESIAN_POINT('Ctrl Pts',(19.8072603769393,9.87908456548571,-18.583394038869)) ;
#35724 = CARTESIAN_POINT('Ctrl Pts',(19.9978365056969,9.47693885988061,-18.5935552896152)) ;
#35725 = CARTESIAN_POINT('Ctrl Pts',(20.188393041677,9.07483449812786,-18.603715495702)) ;
#35726 = CARTESIAN_POINT('Ctrl Pts',(20.3668298762112,8.6669552877514,-18.6138757017889)) ;
#35727 = CARTESIAN_POINT('Ctrl Pts',(20.5328134736599,8.25405390813451,-18.6240359078758)) ;
#35728 = CARTESIAN_POINT('Ctrl Pts',(20.698787167029,7.84117716594067,-18.634195507713)) ;
#35729 = CARTESIAN_POINT('Ctrl Pts',(20.8523090222703,7.42327906610788,-18.6443551075503)) ;
#35730 = CARTESIAN_POINT('Ctrl Pts',(20.9930938002441,7.00113189110542,-18.6545147073876)) ;
#35731 = CARTESIAN_POINT('Ctrl Pts',(21.140538479695,6.55901481143818,-18.6651549126918)) ;
#35732 = CARTESIAN_POINT('Ctrl Pts',(21.2740119866376,6.1122372486611,-18.6757951179961)) ;
#35733 = CARTESIAN_POINT('Ctrl Pts',(21.3932448091053,5.66170571472859,-18.6864353233004)) ;
#35734 = CARTESIAN_POINT('Ctrl Pts',(21.5071030430424,5.23148252848763,-18.696595906264)) ;
#35735 = CARTESIAN_POINT('Ctrl Pts',(21.6079758403492,4.79783651864598,-18.7067564892277)) ;
#35736 = CARTESIAN_POINT('Ctrl Pts',(21.6956801712193,4.36157047067479,-18.7169170721913)) ;
#35737 = CARTESIAN_POINT('Ctrl Pts',(21.7833884217748,3.92528492508412,-18.7270781092521)) ;
#35738 = CARTESIAN_POINT('Ctrl Pts',(21.8579269871129,3.48637933287732,-18.7372391463129)) ;
#35739 = CARTESIAN_POINT('Ctrl Pts',(21.9191640334981,3.04566628754737,-18.7474001833738)) ;
#35740 = CARTESIAN_POINT('Ctrl Pts',(21.9804112462253,2.60488007671033,-18.7575629073314)) ;
#35741 = CARTESIAN_POINT('Ctrl Pts',(22.028352496046,2.16228604050916,-18.767725631289)) ;
#35742 = CARTESIAN_POINT('Ctrl Pts',(22.0629076375027,1.7187034769044,-18.7778883552466)) ;
#35743 = CARTESIAN_POINT('Ctrl Pts',(22.0677912277629,1.65601308132613,-18.7793246271773)) ;
#35744 = CARTESIAN_POINT('Ctrl Pts',(22.0724075360066,1.59330294842003,-18.780760899108)) ;
#35745 = CARTESIAN_POINT('Ctrl Pts',(22.0767564197453,1.53057539694607,-18.7821971710388)) ;
#35746 = CARTESIAN_POINT('Ctrl Pts',(22.1083511764002,1.07485805809132,-18.7926317250227)) ;
#35747 = CARTESIAN_POINT('Ctrl Pts',(22.1258345572466,0.618103055261106,-18.8030662790066)) ;
#35748 = CARTESIAN_POINT('Ctrl Pts',(22.1291628742813,0.161200328877062,-18.8135008329905)) ;
#35749 = CARTESIAN_POINT('Ctrl Pts',(22.1324038834859,-0.283717005133503,
-18.82366166958)) ;
#35750 = CARTESIAN_POINT('Ctrl Pts',(22.1222229435832,-0.728774169492671,
-18.8338225061696)) ;
#35751 = CARTESIAN_POINT('Ctrl Pts',(22.0986325054952,-1.17314809362323,-18.8439833427592)) ;
#35752 = CARTESIAN_POINT('Ctrl Pts',(22.0750444935956,-1.61747631555604,-18.8541431343446)) ;
#35753 = CARTESIAN_POINT('Ctrl Pts',(22.0380497504388,-2.0611212084516,-18.8643029259301)) ;
#35754 = CARTESIAN_POINT('Ctrl Pts',(21.987712794336,-2.50326209900041,-18.8744627175156)) ;
#35755 = CARTESIAN_POINT('Ctrl Pts',(21.9373788396031,-2.94537662664519,-18.8846219033177)) ;
#35756 = CARTESIAN_POINT('Ctrl Pts',(21.873704287247,-3.38598710307002,-18.8947810891198)) ;
#35757 = CARTESIAN_POINT('Ctrl Pts',(21.7968054637468,-3.82427857746736,-18.9049402749218)) ;
#35758 = CARTESIAN_POINT('Ctrl Pts',(21.7162632651838,-4.28333578215012,-18.9155807908994)) ;
#35759 = CARTESIAN_POINT('Ctrl Pts',(21.6212136012674,-4.7398486899698,-18.926221306877)) ;
#35760 = CARTESIAN_POINT('Ctrl Pts',(21.5118505074808,-5.19289156504341,-18.9368618228545)) ;
#35761 = CARTESIAN_POINT('Ctrl Pts',(21.4074243627027,-5.62548284629804,-18.947021996854)) ;
#35762 = CARTESIAN_POINT('Ctrl Pts',(21.2899483818142,-6.05491017847042,-18.9571821708534)) ;
#35763 = CARTESIAN_POINT('Ctrl Pts',(21.1596433130348,-6.48038038448689,-18.9673423448528)) ;
#35764 = CARTESIAN_POINT('Ctrl Pts',(21.0293323860427,-6.90586971865379,-18.97750297563)) ;
#35765 = CARTESIAN_POINT('Ctrl Pts',(20.8861912882732,-7.32740135243248,-18.9876636064072)) ;
#35766 = CARTESIAN_POINT('Ctrl Pts',(20.7304904684155,-7.74419782814426,-18.9978242371844)) ;
#35767 = CARTESIAN_POINT('Ctrl Pts',(20.5747637205468,-8.16106371070696,-19.0079865599562)) ;
#35768 = CARTESIAN_POINT('Ctrl Pts',(20.4064731518633,-8.57319264461813,-19.018148882728)) ;
#35769 = CARTESIAN_POINT('Ctrl Pts',(20.2259378685435,-8.9798258557902,-19.0283112054998)) ;
#35770 = CARTESIAN_POINT('Ctrl Pts',(20.200384101217,-9.0373825298899,-19.0297496258841)) ;
#35771 = CARTESIAN_POINT('Ctrl Pts',(20.1745850912025,-9.09482913238595,-19.0311880462684)) ;
#35772 = CARTESIAN_POINT('Ctrl Pts',(20.1485418203396,-9.15216354620723,-19.0326264666527)) ;
#35773 = CARTESIAN_POINT('Ctrl Pts',(19.9596193615738,-9.56807744919059,-19.0430610206366)) ;
#35774 = CARTESIAN_POINT('Ctrl Pts',(19.7577899213315,-9.97819337166521,-19.0534955746205)) ;
#35775 = CARTESIAN_POINT('Ctrl Pts',(19.5434382712976,-10.3817077399857,-19.0639301286044)) ;
#35776 = CARTESIAN_POINT('Ctrl Pts',(19.334694588316,-10.7746651786894,-19.0740916889587)) ;
#35777 = CARTESIAN_POINT('Ctrl Pts',(19.1140756649796,-11.1613618636978,-19.0842532493131)) ;
#35778 = CARTESIAN_POINT('Ctrl Pts',(18.8819839317268,-11.5410795796802,-19.0944148096674)) ;
#35779 = CARTESIAN_POINT('Ctrl Pts',(18.6499160627817,-11.9207582520469,-19.1045753251823)) ;
#35780 = CARTESIAN_POINT('Ctrl Pts',(18.406377859936,-12.2934591930215,-19.1147358406971)) ;
#35781 = CARTESIAN_POINT('Ctrl Pts',(18.1518164162402,-12.6584910575318,-19.124896356212)) ;
#35782 = CARTESIAN_POINT('Ctrl Pts',(17.897270181131,-13.0235011134814,-19.1350562646943)) ;
#35783 = CARTESIAN_POINT('Ctrl Pts',(17.6317021521492,-13.3808428201497,-19.1452161731766)) ;
#35784 = CARTESIAN_POINT('Ctrl Pts',(17.3556022759239,-13.7298545040522,-19.155376081659)) ;
#35785 = CARTESIAN_POINT('Ctrl Pts',(17.066456429831,-14.0953573069438,-19.1660160550429)) ;
#35786 = CARTESIAN_POINT('Ctrl Pts',(16.7657597501494,-14.4517237890874,-19.1766560284269)) ;
#35787 = CARTESIAN_POINT('Ctrl Pts',(16.4541230109498,-14.7982320228814,-19.1872960018108)) ;
#35788 = CARTESIAN_POINT('Ctrl Pts',(16.1565183554016,-15.1291380124246,-19.1974568885603)) ;
#35789 = CARTESIAN_POINT('Ctrl Pts',(15.8489371338289,-15.4510536424285,-19.2076177753097)) ;
#35790 = CARTESIAN_POINT('Ctrl Pts',(15.531950792724,-15.7633860459896,-19.2177786620592)) ;
#35791 = CARTESIAN_POINT('Ctrl Pts',(15.2149503591327,-16.0757323351338,-19.2279400005384)) ;
#35792 = CARTESIAN_POINT('Ctrl Pts',(14.8885441357062,-16.3784943872188,-19.2381013390176)) ;
#35793 = CARTESIAN_POINT('Ctrl Pts',(14.5533398161578,-16.6711167969616,-19.2482626774968)) ;
#35794 = CARTESIAN_POINT('Ctrl Pts',(14.2180799909986,-16.9637876612877,-19.2584256985656)) ;
#35795 = CARTESIAN_POINT('Ctrl Pts',(13.8740193316362,-17.2463153775312,-19.2685887196343)) ;
#35796 = CARTESIAN_POINT('Ctrl Pts',(13.5217994519541,-17.5181841137612,-19.2787517407031)) ;
#35797 = CARTESIAN_POINT('Ctrl Pts',(13.4720779519223,-17.5565627577755,-19.2801864145576)) ;
#35798 = CARTESIAN_POINT('Ctrl Pts',(13.4221939082105,-17.5947290580384,-19.281621088412)) ;
#35799 = CARTESIAN_POINT('Ctrl Pts',(13.3721491765175,-17.6326816299581,-19.2830557622665)) ;
#35800 = CARTESIAN_POINT('Ctrl Pts',(13.0081678766255,-17.908715210202,-19.2934903162504)) ;
#35801 = CARTESIAN_POINT('Ctrl Pts',(12.6355894894932,-18.1735105277762,-19.3039248702343)) ;
#35802 = CARTESIAN_POINT('Ctrl Pts',(12.2551346890656,-18.4265435938312,-19.3143594242182)) ;
#35803 = CARTESIAN_POINT('Ctrl Pts',(11.8846664628094,-18.6729347842174,-19.3245200811526)) ;
#35804 = CARTESIAN_POINT('Ctrl Pts',(11.506730223014,-18.908173171776,-19.334680738087)) ;
#35805 = CARTESIAN_POINT('Ctrl Pts',(11.122021406894,-19.1318183894551,-19.3448413950214)) ;
#35806 = CARTESIAN_POINT('Ctrl Pts',(10.7373521223267,-19.3554406260058,-19.3550010078765)) ;
#35807 = CARTESIAN_POINT('Ctrl Pts',(10.3459118499595,-19.5674719568917,-19.3651606207315)) ;
#35808 = CARTESIAN_POINT('Ctrl Pts',(9.94842253873426,-19.7675168914384,-19.3753202335865)) ;
#35809 = CARTESIAN_POINT('Ctrl Pts',(9.55095687890385,-19.9675499229186,-19.3854792419246)) ;
#35810 = CARTESIAN_POINT('Ctrl Pts',(9.14744310432309,-20.1555978797707,-19.3956382502627)) ;
#35811 = CARTESIAN_POINT('Ctrl Pts',(8.73862675140959,-20.3313117521238,-19.4057972586008)) ;
#35812 = CARTESIAN_POINT('Ctrl Pts',(8.31042829381307,-20.5153562713406,-19.4164379085408)) ;
#35813 = CARTESIAN_POINT('Ctrl Pts',(7.87641261126653,-20.6858689254489,-19.4270785584807)) ;
#35814 = CARTESIAN_POINT('Ctrl Pts',(7.43746056803071,-20.8425050164679,-19.4377192084207)) ;
#35815 = CARTESIAN_POINT('Ctrl Pts',(7.01833641904422,-20.992065701651,-19.4478792097682)) ;
#35816 = CARTESIAN_POINT('Ctrl Pts',(6.59471216982767,-21.1289754616445,-19.4580392111156)) ;
#35817 = CARTESIAN_POINT('Ctrl Pts',(6.16737233137084,-21.2529845807299,-19.4681992124631)) ;
#35818 = CARTESIAN_POINT('Ctrl Pts',(5.74001319418937,-21.3769993000837,-19.4783596726376)) ;
#35819 = CARTESIAN_POINT('Ctrl Pts',(5.30893835363587,-21.4881121528177,-19.4885201328121)) ;
#35820 = CARTESIAN_POINT('Ctrl Pts',(4.87494638901349,-21.586123616035,-19.4986805929866)) ;
#35821 = CARTESIAN_POINT('Ctrl Pts',(4.4408820067301,-21.6841514338429,-19.5088427485767)) ;
#35822 = CARTESIAN_POINT('Ctrl Pts',(4.0038997516947,-21.7690734433896,-19.5190049041668)) ;
#35823 = CARTESIAN_POINT('Ctrl Pts',(3.56480922029008,-21.8407410653905,-19.529167059757)) ;
#35824 = CARTESIAN_POINT('Ctrl Pts',(3.50261795014775,-21.8508918204661,-19.5306063924648)) ;
#35825 = CARTESIAN_POINT('Ctrl Pts',(3.44038440017182,-21.860776764644,-19.5320457251726)) ;
#35826 = CARTESIAN_POINT('Ctrl Pts',(3.37811088385319,-21.870395559269,-19.5334850578803)) ;
#35827 = CARTESIAN_POINT('Ctrl Pts',(2.92127077503222,-21.94095928271,-19.5440440394463)) ;
#35828 = CARTESIAN_POINT('Ctrl Pts',(2.46219788517309,-21.997207914348,-19.5546030210123)) ;
#35829 = CARTESIAN_POINT('Ctrl Pts',(2.00177361950542,-22.0390275973953,-19.5651620025783)) ;
#35830 = CARTESIAN_POINT('Ctrl Pts',(1.54146658847117,-22.0808366321871,-19.5757182955842)) ;
#35831 = CARTESIAN_POINT('Ctrl Pts',(1.07980905639184,-22.1082240440806,-19.58627458859)) ;
#35832 = CARTESIAN_POINT('Ctrl Pts',(0.617687415648591,-22.1211278491638,
-19.5968308815959)) ;
#35833 = CARTESIAN_POINT('Ctrl Pts',(0.412027140883022,-22.1268704932318,
-19.6015288007771)) ;
#35834 = CARTESIAN_POINT('Ctrl Pts',(0.206275004551934,-22.1297452581592,
-19.6062267199583)) ;
#35835 = CARTESIAN_POINT('Ctrl Pts',(0.00050934658643668,-22.1297499941383,
-19.6109246391395)) ;
#35836 = CARTESIAN_POINT('Origin',(0.,0.,5.8748638224677)) ;
#35837 = CARTESIAN_POINT('',(18.1314964472961,-9.20710716996868,-2.14394731085456)) ;
#35838 = CARTESIAN_POINT('',(18.1314964405175,-9.2071071833178,-1.50729947444597)) ;
#35839 = CARTESIAN_POINT('',(18.1314964405232,-9.20710718330643,5.8748638224677)) ;
#35840 = CARTESIAN_POINT('',(-16.4382148282779,-11.9710934804213,1.74782063822043E-13)) ;
#35841 = CARTESIAN_POINT('Ctrl Pts',(18.1314964473001,-9.20710716996079,-2.14394731121824)) ;
#35842 = CARTESIAN_POINT('Ctrl Pts',(18.4070604988656,-8.66444067007858,-2.12914163381511)) ;
#35843 = CARTESIAN_POINT('Ctrl Pts',(18.6581480245163,-8.10962743636976,-2.11424200137709)) ;
#35844 = CARTESIAN_POINT('Ctrl Pts',(19.1103747290994,-6.97767300525182,-2.08402031193033)) ;
#35845 = CARTESIAN_POINT('Ctrl Pts',(19.311139015107,-6.40111261666378,-2.0687139103353)) ;
#35846 = CARTESIAN_POINT('Ctrl Pts',(19.6449050680122,-5.28295493835131,-2.03918173204836)) ;
#35847 = CARTESIAN_POINT('Ctrl Pts',(19.7821641775101,-4.74319360546866,-2.0249931683764)) ;
#35848 = CARTESIAN_POINT('Ctrl Pts',(20.0076220225193,-3.67472276012286,-1.99722483133982)) ;
#35849 = CARTESIAN_POINT('Ctrl Pts',(20.097417547488,-3.14679846711533,-1.98365443331201)) ;
#35850 = CARTESIAN_POINT('Ctrl Pts',(20.215535744351,-2.23622729969757,-1.9607817254437)) ;
#35851 = CARTESIAN_POINT('Ctrl Pts',(20.25405783991,-1.8551927740339,-1.95138198287428)) ;
#35852 = CARTESIAN_POINT('Ctrl Pts',(20.328558793268,-0.829593349802003,-1.92629447398207)) ;
#35853 = CARTESIAN_POINT('Ctrl Pts',(20.3446471041896,-0.184026714065221,
-1.91071628859271)) ;
#35854 = CARTESIAN_POINT('Ctrl Pts',(20.3147745984406,1.13274267984035,-1.87868818779915)) ;
#35855 = CARTESIAN_POINT('Ctrl Pts',(20.2662770572425,1.80310203072013,-1.86224593843474)) ;
#35856 = CARTESIAN_POINT('Ctrl Pts',(20.1059766817548,3.1131594358071,-1.8294707549246)) ;
#35857 = CARTESIAN_POINT('Ctrl Pts',(19.9965465099027,3.75235604437061,-1.81317389417271)) ;
#35858 = CARTESIAN_POINT('Ctrl Pts',(19.6850285228298,5.16294251539185,-1.77654689194309)) ;
#35859 = CARTESIAN_POINT('Ctrl Pts',(19.4677347381169,5.92989250164944,-1.75616931465371)) ;
#35860 = CARTESIAN_POINT('Ctrl Pts',(19.0969913292527,6.99549883656332,-1.72772363405256)) ;
#35861 = CARTESIAN_POINT('Ctrl Pts',(18.9803055255759,7.30616789254893,-1.71942424390114)) ;
#35862 = CARTESIAN_POINT('Ctrl Pts',(18.6270344095751,8.18106127797865,-1.69610832322852)) ;
#35863 = CARTESIAN_POINT('Ctrl Pts',(18.3725214965132,8.73765636526242,-1.68128119906307)) ;
#35864 = CARTESIAN_POINT('Ctrl Pts',(17.692629506754,10.0629722209494,-1.64515670408829)) ;
#35865 = CARTESIAN_POINT('Ctrl Pts',(17.2418041688731,10.8172420572401,-1.62386139796713)) ;
#35866 = CARTESIAN_POINT('Ctrl Pts',(16.4142942665253,12.0178940801389,-1.58777800121821)) ;
#35867 = CARTESIAN_POINT('Ctrl Pts',(16.064626498684,12.481450277972,-1.57325807757352)) ;
#35868 = CARTESIAN_POINT('Ctrl Pts',(15.2355192782029,13.4879420754917,-1.54032775643703)) ;
#35869 = CARTESIAN_POINT('Ctrl Pts',(14.7459402570254,14.0215144549308,-1.52185763212307)) ;
#35870 = CARTESIAN_POINT('Ctrl Pts',(13.9156141079229,14.8347582832945,-1.49234182989152)) ;
#35871 = CARTESIAN_POINT('Ctrl Pts',(13.5924101608993,15.1314493493459,-1.48125018949377)) ;
#35872 = CARTESIAN_POINT('Ctrl Pts',(12.9806406249973,15.6576049047881,-1.4611340156327)) ;
#35873 = CARTESIAN_POINT('Ctrl Pts',(12.6949446197056,15.8901228458011,-1.45208134364914)) ;
#35874 = CARTESIAN_POINT('Ctrl Pts',(11.9365412565554,16.473845482997,-1.428711200507)) ;
#35875 = CARTESIAN_POINT('Ctrl Pts',(11.4546150392463,16.8125072556577,-1.41448677511618)) ;
#35876 = CARTESIAN_POINT('Ctrl Pts',(10.3614203648338,17.5118719554038,-1.38297106473484)) ;
#35877 = CARTESIAN_POINT('Ctrl Pts',(9.74459614002155,17.8624613848042,-1.36566102265593)) ;
#35878 = CARTESIAN_POINT('Ctrl Pts',(8.56695497260617,18.4526208173196,-1.33300576935575)) ;
#35879 = CARTESIAN_POINT('Ctrl Pts',(8.01123497730341,18.7005892071007,-1.31775132822014)) ;
#35880 = CARTESIAN_POINT('Ctrl Pts',(7.05069167603135,19.0785088641159,-1.29163120878163)) ;
#35881 = CARTESIAN_POINT('Ctrl Pts',(6.65138332692506,19.2213644644102,-1.28084508721137)) ;
#35882 = CARTESIAN_POINT('Ctrl Pts',(5.6476362773152,19.5454360459507,-1.25400172155765)) ;
#35883 = CARTESIAN_POINT('Ctrl Pts',(5.03867446859198,19.7112057522894,-1.23794767112378)) ;
#35884 = CARTESIAN_POINT('Ctrl Pts',(4.09048204034264,19.9224997528993,-1.21368061529707)) ;
#35885 = CARTESIAN_POINT('Ctrl Pts',(3.75616222978537,19.9882286622897,-1.20527986520689)) ;
#35886 = CARTESIAN_POINT('Ctrl Pts',(2.94049161212025,20.1274057392257,-1.18502727560605)) ;
#35887 = CARTESIAN_POINT('Ctrl Pts',(2.45784751184561,20.1920266813045,-1.17323622308097)) ;
#35888 = CARTESIAN_POINT('Ctrl Pts',(1.16539400332144,20.3180422333094,-1.1417423316886)) ;
#35889 = CARTESIAN_POINT('Ctrl Pts',(0.353452242653345,20.3483670971419,-1.12201771310095)) ;
#35890 = CARTESIAN_POINT('Ctrl Pts',(-1.03452166985655,20.3170902643203,-1.08767445272038)) ;
#35891 = CARTESIAN_POINT('Ctrl Pts',(-1.61010437925601,20.2795943532478,-1.07325669585217)) ;
#35892 = CARTESIAN_POINT('Ctrl Pts',(-2.887436311421,20.1416551426706,-1.04082413410225)) ;
#35893 = CARTESIAN_POINT('Ctrl Pts',(-3.58710714495018,20.0288845241005,-1.02275548667019)) ;
#35894 = CARTESIAN_POINT('Ctrl Pts',(-4.728583451408,19.783163105859,-0.993087957827959)) ;
#35895 = CARTESIAN_POINT('Ctrl Pts',(-5.17430308148158,19.6712896363558,-0.981459861869672)) ;
#35896 = CARTESIAN_POINT('Ctrl Pts',(-5.96207971388486,19.4449315258678,-0.96101602464987)) ;
#35897 = CARTESIAN_POINT('Ctrl Pts',(-6.30560267918617,19.3362646781196,-0.952154263379939)) ;
#35898 = CARTESIAN_POINT('Ctrl Pts',(-7.17410015107353,19.0359251514032,-0.929701075255005)) ;
#35899 = CARTESIAN_POINT('Ctrl Pts',(-7.69439392225628,18.8316346910951,-0.916193587012207)) ;
#35900 = CARTESIAN_POINT('Ctrl Pts',(-8.84950855944488,18.3222111373546,-0.885552539775624)) ;
#35901 = CARTESIAN_POINT('Ctrl Pts',(-9.47822329441879,18.0050130882924,-0.8684000658019)) ;
#35902 = CARTESIAN_POINT('Ctrl Pts',(-10.5924135477188,17.3683229020488,-0.836647666386695)) ;
#35903 = CARTESIAN_POINT('Ctrl Pts',(-11.083076537831,17.0594041772199,-0.822150128390012)) ;
#35904 = CARTESIAN_POINT('Ctrl Pts',(-12.1523009529982,16.3206037883209,-0.789333034621653)) ;
#35905 = CARTESIAN_POINT('Ctrl Pts',(-12.7225679017549,15.8800750951574,-0.770955141014419)) ;
#35906 = CARTESIAN_POINT('Ctrl Pts',(-13.6042674086005,15.1209289036687,-0.741404424010633)) ;
#35907 = CARTESIAN_POINT('Ctrl Pts',(-13.9307242687187,14.8207121330741,-0.730189714768981)) ;
#35908 = CARTESIAN_POINT('Ctrl Pts',(-14.5090111905555,14.2529051111629,-0.709983274671964)) ;
#35909 = CARTESIAN_POINT('Ctrl Pts',(-14.7639050642147,13.9887032134202,-0.700959695861528)) ;
#35910 = CARTESIAN_POINT('Ctrl Pts',(-15.4053784238701,13.2867306178644,-0.677735911140703)) ;
#35911 = CARTESIAN_POINT('Ctrl Pts',(-15.7805031862737,12.8389492488045,-0.663627217392614)) ;
#35912 = CARTESIAN_POINT('Ctrl Pts',(-16.5678199913945,11.8124156469433,-0.632212178287984)) ;
#35913 = CARTESIAN_POINT('Ctrl Pts',(-16.9700105384739,11.2269565957541,-0.614886334466801)) ;
#35914 = CARTESIAN_POINT('Ctrl Pts',(-17.6564842816621,10.1062311654097,-0.582311719678745)) ;
#35915 = CARTESIAN_POINT('Ctrl Pts',(-17.9490644994335,9.57697339141689,-0.567156569360043)) ;
#35916 = CARTESIAN_POINT('Ctrl Pts',(-18.5826511492801,8.29951432464586,-0.531081318129922)) ;
#35917 = CARTESIAN_POINT('Ctrl Pts',(-18.9027344600243,7.54211406716008,-0.51006273235971)) ;
#35918 = CARTESIAN_POINT('Ctrl Pts',(-19.2952777119488,6.42980821109379,-0.480241768079931)) ;
#35919 = CARTESIAN_POINT('Ctrl Pts',(-19.4054935741367,6.08908865801761,-0.471249831683759)) ;
#35920 = CARTESIAN_POINT('Ctrl Pts',(-19.6860582950359,5.1365600894882,-0.446641306907111)) ;
#35921 = CARTESIAN_POINT('Ctrl Pts',(-19.8368358112422,4.51941352605139,-0.431244421412695)) ;
#35922 = CARTESIAN_POINT('Ctrl Pts',(-20.1315721908958,3.00961929385165,-0.393939392305378)) ;
#35923 = CARTESIAN_POINT('Ctrl Pts',(-20.2453808210544,2.11247495945526,-0.372041340353589)) ;
#35924 = CARTESIAN_POINT('Ctrl Pts',(-20.3337181638462,0.631424936674302,
-0.335325976267399)) ;
#35925 = CARTESIAN_POINT('Ctrl Pts',(-20.3434557697033,0.0508955018989362,
-0.320806137541027)) ;
#35926 = CARTESIAN_POINT('Ctrl Pts',(-20.3094700081703,-1.25448810626689,
-0.287828656960079)) ;
#35927 = CARTESIAN_POINT('Ctrl Pts',(-20.2517912924953,-1.97819474295732,
-0.269310323623449)) ;
#35928 = CARTESIAN_POINT('Ctrl Pts',(-20.0942908791518,-3.15513204026942,
-0.239157653214394)) ;
#35929 = CARTESIAN_POINT('Ctrl Pts',(-20.0174332880666,-3.61078296201057,
-0.227480522918781)) ;
#35930 = CARTESIAN_POINT('Ctrl Pts',(-19.8421665466511,-4.47020919927205,
-0.205656060245955)) ;
#35931 = CARTESIAN_POINT('Ctrl Pts',(-19.7467703008463,-4.8743624684055,-0.195485321582215)) ;
#35932 = CARTESIAN_POINT('Ctrl Pts',(-19.3421533093001,-6.38068085310552,
-0.157484461189357)) ;
#35933 = CARTESIAN_POINT('Ctrl Pts',(-18.9524467025526,-7.45900487226203,
-0.129970419011596)) ;
#35934 = CARTESIAN_POINT('Ctrl Pts',(-18.33406171794,-8.80320602529759,-0.0933871600585856)) ;
#35935 = CARTESIAN_POINT('Ctrl Pts',(-18.1865243033531,-9.10409728854879,
-0.085051792049178)) ;
#35936 = CARTESIAN_POINT('Ctrl Pts',(-17.5649938141278,-10.2962000708724,
-0.0513967240819126)) ;
#35937 = CARTESIAN_POINT('Ctrl Pts',(-17.0323873926875,-11.1552000722871,
-0.025624345594017)) ;
#35938 = CARTESIAN_POINT('Ctrl Pts',(-16.4382148282779,-11.9710934804213,
1.86183533867901E-13)) ;
#35939 = CARTESIAN_POINT('',(-16.4251684725406,11.9889877181628,1.11022302462516E-15)) ;
#35940 = CARTESIAN_POINT('Origin',(0.,0.,1.11022302462516E-15)) ;
#35941 = CARTESIAN_POINT('Ctrl Pts',(-16.4251684725406,11.9889877181628,9.19403442267708E-16)) ;
#35942 = CARTESIAN_POINT('Ctrl Pts',(-15.7219712149796,12.952382935206,-0.0296386565568351)) ;
#35943 = CARTESIAN_POINT('Ctrl Pts',(-14.9353782007936,13.8520448586411,-0.0582115199547762)) ;
#35944 = CARTESIAN_POINT('Ctrl Pts',(-13.6865165338504,15.0495895201416,-0.100707837078664)) ;
#35945 = CARTESIAN_POINT('Ctrl Pts',(-13.2839741547818,15.4060671066688,-0.114015439948085)) ;
#35946 = CARTESIAN_POINT('Ctrl Pts',(-12.235534047229,16.2628530497365,-0.147905859106198)) ;
#35947 = CARTESIAN_POINT('Ctrl Pts',(-11.5727423153889,16.7409765741639,-0.168668796287312)) ;
#35948 = CARTESIAN_POINT('Ctrl Pts',(-10.4504160352174,17.4520211923301,-0.202612219255183)) ;
#35949 = CARTESIAN_POINT('Ctrl Pts',(-10.0076207859949,17.709651808454,-0.21571277353598)) ;
#35950 = CARTESIAN_POINT('Ctrl Pts',(-9.25245913876061,18.1116509552783,-0.237390996457211)) ;
#35951 = CARTESIAN_POINT('Ctrl Pts',(-8.94530316347661,18.2653074811295,-0.246030364109235)) ;
#35952 = CARTESIAN_POINT('Ctrl Pts',(-8.21650025089806,18.6070997266183,-0.266015168510672)) ;
#35953 = CARTESIAN_POINT('Ctrl Pts',(-7.79204552560557,18.7888016920705,-0.277285765206995)) ;
#35954 = CARTESIAN_POINT('Ctrl Pts',(-6.69110876728485,19.216364933913,-0.306000207822587)) ;
#35955 = CARTESIAN_POINT('Ctrl Pts',(-6.00709437540987,19.441050264074,-0.323367849376024)) ;
#35956 = CARTESIAN_POINT('Ctrl Pts',(-4.75371597153538,19.7802785394849,-0.355098077817085)) ;
#35957 = CARTESIAN_POINT('Ctrl Pts',(-4.18861647154059,19.9076045446856,-0.369366498788469)) ;
#35958 = CARTESIAN_POINT('Ctrl Pts',(-2.81094533615709,20.1567518224348,-0.404281146988823)) ;
#35959 = CARTESIAN_POINT('Ctrl Pts',(-1.99493103026704,20.2537968393659,-0.425087477408961)) ;
#35960 = CARTESIAN_POINT('Ctrl Pts',(-0.697887529780475,20.3288864237583,
-0.458140229404543)) ;
#35961 = CARTESIAN_POINT('Ctrl Pts',(-0.21964999526929,20.3396761523728,-0.470314421784974)) ;
#35962 = CARTESIAN_POINT('Ctrl Pts',(0.59746849952955,20.3292872467944,-0.490928594759438)) ;
#35963 = CARTESIAN_POINT('Ctrl Pts',(0.936256696337432,20.3165035783119,-0.49941434113361)) ;
#35964 = CARTESIAN_POINT('Ctrl Pts',(1.88052753388487,20.2572019990012,-0.522807492740379)) ;
#35965 = CARTESIAN_POINT('Ctrl Pts',(2.48447960409391,20.1920278333657,-0.537532244683842)) ;
#35966 = CARTESIAN_POINT('Ctrl Pts',(3.51328878711502,20.0341428410562,-0.562781070047226)) ;
#35967 = CARTESIAN_POINT('Ctrl Pts',(3.93975081945725,19.9546596075592,-0.573294782305604)) ;
#35968 = CARTESIAN_POINT('Ctrl Pts',(4.96485395431136,19.7294573611182,-0.59888790002866)) ;
#35969 = CARTESIAN_POINT('Ctrl Pts',(5.56004610352606,19.5700572545556,-0.614023173627694)) ;
#35970 = CARTESIAN_POINT('Ctrl Pts',(6.82786080761857,19.168003838611,-0.64713199168191)) ;
#35971 = CARTESIAN_POINT('Ctrl Pts',(7.49678808185005,18.9164005021167,-0.665155449979463)) ;
#35972 = CARTESIAN_POINT('Ctrl Pts',(8.68573499721003,18.3962105785484,-0.698126809632371)) ;
#35973 = CARTESIAN_POINT('Ctrl Pts',(9.21006803657225,18.1393826657444,-0.713013891681812)) ;
#35974 = CARTESIAN_POINT('Ctrl Pts',(10.0456123870918,17.684538166588,-0.737065327508699)) ;
#35975 = CARTESIAN_POINT('Ctrl Pts',(10.3637717111078,17.4999845891053,-0.746301370099693)) ;
#35976 = CARTESIAN_POINT('Ctrl Pts',(11.1369487134599,17.0230060573996,-0.768809774521529)) ;
#35977 = CARTESIAN_POINT('Ctrl Pts',(11.58563980657,16.7208648253939,-0.781961505553171)) ;
#35978 = CARTESIAN_POINT('Ctrl Pts',(12.5577503102278,16.0083269080645,-0.811211874784397)) ;
#35979 = CARTESIAN_POINT('Ctrl Pts',(13.0741611450178,15.5894172898652,-0.827284196837257)) ;
#35980 = CARTESIAN_POINT('Ctrl Pts',(13.9886805663289,14.7701083375025,-0.857329854589425)) ;
#35981 = CARTESIAN_POINT('Ctrl Pts',(14.3924270211163,14.3769719035031,-0.87123408282866)) ;
#35982 = CARTESIAN_POINT('Ctrl Pts',(15.4110846311364,13.2991137050321,-0.908266919871303)) ;
#35983 = CARTESIAN_POINT('Ctrl Pts',(15.9967555779025,12.5885557748925,-0.931658915679869)) ;
#35984 = CARTESIAN_POINT('Ctrl Pts',(16.878451015568,11.3575200483428,-0.970199293705423)) ;
#35985 = CARTESIAN_POINT('Ctrl Pts',(17.2032376720091,10.8592813464447,-0.985303589678979)) ;
#35986 = CARTESIAN_POINT('Ctrl Pts',(17.694621029346,10.0279694223595,-1.00937345260218)) ;
#35987 = CARTESIAN_POINT('Ctrl Pts',(17.8747258531264,9.7032963799115,-1.0184949619102)) ;
#35988 = CARTESIAN_POINT('Ctrl Pts',(18.4048995851386,8.68264789894119,-1.04657461776846)) ;
#35989 = CARTESIAN_POINT('Ctrl Pts',(18.7239452244203,7.97136031257796,-1.06533766762343)) ;
#35990 = CARTESIAN_POINT('Ctrl Pts',(19.2209235455291,6.66767422753229,-1.09934704103421)) ;
#35991 = CARTESIAN_POINT('Ctrl Pts',(19.4141517981003,6.08214457079392,-1.11448617868724)) ;
#35992 = CARTESIAN_POINT('Ctrl Pts',(19.7718753841205,4.80600620762275,-1.14746669668622)) ;
#35993 = CARTESIAN_POINT('Ctrl Pts',(19.927418170574,4.11372607210993,-1.16535440325119)) ;
#35994 = CARTESIAN_POINT('Ctrl Pts',(20.145793450775,2.83173967860662,-1.19839064679211)) ;
#35995 = CARTESIAN_POINT('Ctrl Pts',(20.2196230506528,2.24467981957297,-1.21348053536974)) ;
#35996 = CARTESIAN_POINT('Ctrl Pts',(20.2978287413328,1.28708130193953,-1.23777705679103)) ;
#35997 = CARTESIAN_POINT('Ctrl Pts',(20.3178592037096,0.918168610825223,-1.24705709300463)) ;
#35998 = CARTESIAN_POINT('Ctrl Pts',(20.3398770536836,0.102781692689801,-1.26727135936445)) ;
#35999 = CARTESIAN_POINT('Ctrl Pts',(20.3372340397449,-0.343626683938318,
-1.2781632442229)) ;
#36000 = CARTESIAN_POINT('Ctrl Pts',(20.2920426930773,-1.50661779239668,-1.30645425721975)) ;
#36001 = CARTESIAN_POINT('Ctrl Pts',(20.2262473093586,-2.2216691251496,-1.32377799590472)) ;
#36002 = CARTESIAN_POINT('Ctrl Pts',(20.03940846552,-3.5040868038042,-1.35544979326474)) ;
#36003 = CARTESIAN_POINT('Ctrl Pts',(19.9316425617138,-4.07260761472665,-1.36970457180588)) ;
#36004 = CARTESIAN_POINT('Ctrl Pts',(19.6427688522322,-5.30641667700451,-1.40131018670499)) ;
#36005 = CARTESIAN_POINT('Ctrl Pts',(19.4517739557115,-5.96866006951631,-1.4187176908526)) ;
#36006 = CARTESIAN_POINT('Ctrl Pts',(19.0422020257174,-7.15825970678939,-1.45070432997864)) ;
#36007 = CARTESIAN_POINT('Ctrl Pts',(18.8343309265916,-7.6885707034895,-1.4652318784316)) ;
#36008 = CARTESIAN_POINT('Ctrl Pts',(18.4579742636463,-8.5414796265195,-1.4888054269677)) ;
#36009 = CARTESIAN_POINT('Ctrl Pts',(18.3026026643531,-8.86952253996998,-1.49792082093674)) ;
#36010 = CARTESIAN_POINT('Ctrl Pts',(18.13618981682,-9.19786016798943,-1.50704257034263)) ;
#36011 = CARTESIAN_POINT('Ctrl Pts',(18.1338440092164,-9.20248413150992,-1.50717103379489)) ;
#36012 = CARTESIAN_POINT('Ctrl Pts',(18.1314964405117,-9.20710718332916,-1.50729947444597)) ;
#36013 = CARTESIAN_POINT('Origin',(0.,0.,5.8748638224677)) ;
#36014 = CARTESIAN_POINT('',(18.1314964416892,-9.20710718101026,-5.31929120111857)) ;
#36015 = CARTESIAN_POINT('',(18.1314964277575,-9.20710720844602,-4.68087293510305)) ;
#36016 = CARTESIAN_POINT('',(18.1314964405232,-9.20710718330643,5.8748638224677)) ;
#36017 = CARTESIAN_POINT('Ctrl Pts',(18.1314964428552,-9.20710717871412,-5.31929120111857)) ;
#36018 = CARTESIAN_POINT('Ctrl Pts',(18.1559821510112,-9.15888763247507,-5.31792774964532)) ;
#36019 = CARTESIAN_POINT('Ctrl Pts',(18.1802763413727,-9.1105687599884,-5.3165631336081)) ;
#36020 = CARTESIAN_POINT('Ctrl Pts',(18.5257542087327,-8.41656031266548,-5.29698693603004)) ;
#36021 = CARTESIAN_POINT('Ctrl Pts',(18.812559440899,-7.75433145747545,-5.27858124043252)) ;
#36022 = CARTESIAN_POINT('Ctrl Pts',(19.2173957433681,-6.66400522939126,-5.24904220623317)) ;
#36023 = CARTESIAN_POINT('Ctrl Pts',(19.3576696079644,-6.24482956744858,-5.23786576038616)) ;
#36024 = CARTESIAN_POINT('Ctrl Pts',(19.5891884193155,-5.46994018417184,-5.21770239003431)) ;
#36025 = CARTESIAN_POINT('Ctrl Pts',(19.6846715106068,-5.11568730207103,-5.20868442153962)) ;
#36026 = CARTESIAN_POINT('Ctrl Pts',(19.9070235798934,-4.1919693321225,-5.18548127515127)) ;
#36027 = CARTESIAN_POINT('Ctrl Pts',(20.01906597078,-3.61928115521873,-5.17138750943531)) ;
#36028 = CARTESIAN_POINT('Ctrl Pts',(20.2125403282271,-2.34073661212831,-5.1399886145783)) ;
#36029 = CARTESIAN_POINT('Ctrl Pts',(20.2819235790346,-1.63382978160729,-5.12266394850667)) ;
#36030 = CARTESIAN_POINT('Ctrl Pts',(20.341628685311,-0.322271658271764,-5.0901250649481)) ;
#36031 = CARTESIAN_POINT('Ctrl Pts',(20.3422387413483,0.281122441438539,-5.07500528495166)) ;
#36032 = CARTESIAN_POINT('Ctrl Pts',(20.2805486881811,1.69944790969356,-5.03909214548146)) ;
#36033 = CARTESIAN_POINT('Ctrl Pts',(20.1959593676048,2.51236867865972,-5.01820225209204)) ;
#36034 = CARTESIAN_POINT('Ctrl Pts',(20.003033753051,3.67892060385428,-4.98830116649707)) ;
#36035 = CARTESIAN_POINT('Ctrl Pts',(19.9336141555108,4.03817398281195,-4.97911105857734)) ;
#36036 = CARTESIAN_POINT('Ctrl Pts',(19.7169315789473,5.01696301556774,-4.95426715437512)) ;
#36037 = CARTESIAN_POINT('Ctrl Pts',(19.5502062721511,5.6317631709054,-4.93882867315064)) ;
#36038 = CARTESIAN_POINT('Ctrl Pts',(19.0789827810852,7.0939118971983,-4.90157021711408)) ;
#36039 = CARTESIAN_POINT('Ctrl Pts',(18.7465469335426,7.9308345030986,-4.87975936640964)) ;
#36040 = CARTESIAN_POINT('Ctrl Pts',(18.1096423233854,9.26829907880833,-4.8430982931057)) ;
#36041 = CARTESIAN_POINT('Ctrl Pts',(17.8370604409887,9.78262637817891,-4.82854004079058)) ;
#36042 = CARTESIAN_POINT('Ctrl Pts',(17.1739178738523,10.9137770434637,-4.79542382251435)) ;
#36043 = CARTESIAN_POINT('Ctrl Pts',(16.7714468156124,11.522697112974,-4.77680392585817)) ;
#36044 = CARTESIAN_POINT('Ctrl Pts',(16.0652550039059,12.4754979401561,-4.74669152458499)) ;
#36045 = CARTESIAN_POINT('Ctrl Pts',(15.7810933767637,12.8330652546081,-4.7351519394572)) ;
#36046 = CARTESIAN_POINT('Ctrl Pts',(15.2189472597664,13.4934904143528,-4.71357318973011)) ;
#36047 = CARTESIAN_POINT('Ctrl Pts',(14.9433454287944,13.7980821014407,-4.70351182668701)) ;
#36048 = CARTESIAN_POINT('Ctrl Pts',(13.7819594721497,15.005991399071,-4.66268786995385)) ;
#36049 = CARTESIAN_POINT('Ctrl Pts',(12.822039094026,15.8340616479812,-4.63230648977514)) ;
#36050 = CARTESIAN_POINT('Ctrl Pts',(11.2705226606738,16.9383022133271,-4.5850307035503)) ;
#36051 = CARTESIAN_POINT('Ctrl Pts',(10.7324344207221,17.284258819552,-4.56896247581451)) ;
#36052 = CARTESIAN_POINT('Ctrl Pts',(9.49726269523084,17.99844555663,-4.53279983291788)) ;
#36053 = CARTESIAN_POINT('Ctrl Pts',(8.79325973576812,18.3526734065808,-4.51265608620187)) ;
#36054 = CARTESIAN_POINT('Ctrl Pts',(7.75698817238502,18.8007388644242,-4.48416089966032)) ;
#36055 = CARTESIAN_POINT('Ctrl Pts',(7.44011275310201,18.9283748749947,-4.47560413940647)) ;
#36056 = CARTESIAN_POINT('Ctrl Pts',(6.52246470706421,19.2713935114325,-4.45136992208235)) ;
#36057 = CARTESIAN_POINT('Ctrl Pts',(5.9145711602534,19.4665614275168,-4.43590902175634)) ;
#36058 = CARTESIAN_POINT('Ctrl Pts',(4.46238337407389,19.8584778008896,-4.39943068161008)) ;
#36059 = CARTESIAN_POINT('Ctrl Pts',(3.61270560573872,20.0304855698857,-4.37841506745215)) ;
#36060 = CARTESIAN_POINT('Ctrl Pts',(2.18029147518007,20.2263288514101,-4.34264201396965)) ;
#36061 = CARTESIAN_POINT('Ctrl Pts',(1.60283395315019,20.2802604584607,-4.3281401286249)) ;
#36062 = CARTESIAN_POINT('Ctrl Pts',(0.303975372320136,20.3457402264736,-4.29530039101204)) ;
#36063 = CARTESIAN_POINT('Ctrl Pts',(-0.417335032413373,20.3437304944877,
-4.27690391106356)) ;
#36064 = CARTESIAN_POINT('Ctrl Pts',(-1.57868926258423,20.2786937551661,-4.24736157726332)) ;
#36065 = CARTESIAN_POINT('Ctrl Pts',(-2.01944860790256,20.2395531485828,-4.23617301754538)) ;
#36066 = CARTESIAN_POINT('Ctrl Pts',(-2.82252969581127,20.1417411123703,-4.21600245294478)) ;
#36067 = CARTESIAN_POINT('Ctrl Pts',(-3.18521255936294,20.0875790072685,-4.20698899832239)) ;
#36068 = CARTESIAN_POINT('Ctrl Pts',(-4.1198644264802,19.9220500231144,-4.18380767998688)) ;
#36069 = CARTESIAN_POINT('Ctrl Pts',(-4.68886700872009,19.7958553722445,-4.16973101253819)) ;
#36070 = CARTESIAN_POINT('Ctrl Pts',(-5.93742480729189,19.462087328627,-4.1383495640242)) ;
#36071 = CARTESIAN_POINT('Ctrl Pts',(-6.61310926607348,19.242989159634,-4.12102518045135)) ;
#36072 = CARTESIAN_POINT('Ctrl Pts',(-7.83847800144446,18.7734692246094,-4.08850431681238)) ;
#36073 = CARTESIAN_POINT('Ctrl Pts',(-8.39114766142448,18.5330384800905,-4.07340268560286)) ;
#36074 = CARTESIAN_POINT('Ctrl Pts',(-9.66340846286822,17.9109683531498,-4.03757887817461)) ;
#36075 = CARTESIAN_POINT('Ctrl Pts',(-10.3723728449488,17.5099435998261,-4.01676128458584)) ;
#36076 = CARTESIAN_POINT('Ctrl Pts',(-11.3644555938423,16.8673273129995,-3.986864930243)) ;
#36077 = CARTESIAN_POINT('Ctrl Pts',(-11.6680254241961,16.6587745831404,-3.97761235817111)) ;
#36078 = CARTESIAN_POINT('Ctrl Pts',(-12.4761743375731,16.0706424584172,-3.95283884329037)) ;
#36079 = CARTESIAN_POINT('Ctrl Pts',(-12.969012009516,15.6756248780064,-3.93752735238435)) ;
#36080 = CARTESIAN_POINT('Ctrl Pts',(-14.124125878444,14.6579622040014,-3.90018900818199)) ;
#36081 = CARTESIAN_POINT('Ctrl Pts',(-14.7645845484479,14.0126306882734,-3.87817348869706)) ;
#36082 = CARTESIAN_POINT('Ctrl Pts',(-15.7414024152423,12.8867905911197,-3.84128411561408)) ;
#36083 = CARTESIAN_POINT('Ctrl Pts',(-16.103972501381,12.430735397658,-3.82671197625354)) ;
#36084 = CARTESIAN_POINT('Ctrl Pts',(-16.8766837623956,11.3681406801463,-3.79352754605739)) ;
#36085 = CARTESIAN_POINT('Ctrl Pts',(-17.274663788893,10.7537463644558,-3.77485250637854)) ;
#36086 = CARTESIAN_POINT('Ctrl Pts',(-17.8643813866559,9.72582113497613,-3.74476532263966)) ;
#36087 = CARTESIAN_POINT('Ctrl Pts',(-18.0768666610458,9.32494587308614,-3.73330351633081)) ;
#36088 = CARTESIAN_POINT('Ctrl Pts',(-18.4564949196336,8.54690779082685,-3.7117648017382)) ;
#36089 = CARTESIAN_POINT('Ctrl Pts',(-18.6259193753762,8.17110568143938,-3.70166870844146)) ;
#36090 = CARTESIAN_POINT('Ctrl Pts',(-19.2656157557448,6.62870580523238,-3.6609904811159)) ;
#36091 = CARTESIAN_POINT('Ctrl Pts',(-19.6386135852726,5.42480940085267,-3.63078223882926)) ;
#36092 = CARTESIAN_POINT('Ctrl Pts',(-20.0288419676727,3.57349332928095,-3.58382219019039)) ;
#36093 = CARTESIAN_POINT('Ctrl Pts',(-20.1305592892701,2.94702166548093,-3.56788497202938)) ;
#36094 = CARTESIAN_POINT('Ctrl Pts',(-20.2919301335513,1.53986115124165,-3.53199399658883)) ;
#36095 = CARTESIAN_POINT('Ctrl Pts',(-20.336135819065,0.758404399295824,-3.51198995184768)) ;
#36096 = CARTESIAN_POINT('Ctrl Pts',(-20.3348212719647,-0.371850029604857,
-3.48344537174236)) ;
#36097 = CARTESIAN_POINT('Ctrl Pts',(-20.3254730830073,-0.719985144308301,
-3.47471456322468)) ;
#36098 = CARTESIAN_POINT('Ctrl Pts',(-20.2760620399025,-1.65975043878857,
-3.45142170283921)) ;
#36099 = CARTESIAN_POINT('Ctrl Pts',(-20.2190580112873,-2.2501481542125,-3.4370326667016)) ;
#36100 = CARTESIAN_POINT('Ctrl Pts',(-20.0068234580975,-3.75642445874931,
-3.40013501711456)) ;
#36101 = CARTESIAN_POINT('Ctrl Pts',(-19.8145176404088,-4.66568197339976,
-3.37764394821454)) ;
#36102 = CARTESIAN_POINT('Ctrl Pts',(-19.4012900804551,-6.11983084814863,
-3.34022694617133)) ;
#36103 = CARTESIAN_POINT('Ctrl Pts',(-19.2177301737652,-6.67392121870762,
-3.32562601743648)) ;
#36104 = CARTESIAN_POINT('Ctrl Pts',(-18.7493477397926,-7.90730586690761,
-3.29230002823761)) ;
#36105 = CARTESIAN_POINT('Ctrl Pts',(-18.4509419304834,-8.58057464067465,
-3.2735105166438)) ;
#36106 = CARTESIAN_POINT('Ctrl Pts',(-17.9246075092757,-9.61297600972349,
-3.24409445403031)) ;
#36107 = CARTESIAN_POINT('Ctrl Pts',(-17.7208015771778,-9.98368956859351,
-3.23340709515066)) ;
#36108 = CARTESIAN_POINT('Ctrl Pts',(-17.3144346144009,-10.6711501975291,
-3.21350673853816)) ;
#36109 = CARTESIAN_POINT('Ctrl Pts',(-17.114361987694,-10.989163170545,-3.20427955772466)) ;
#36110 = CARTESIAN_POINT('Ctrl Pts',(-16.562748791522,-11.8143093382929,-3.18005395100237)) ;
#36111 = CARTESIAN_POINT('Ctrl Pts',(-16.1967411976689,-12.3113009502041,
-3.16515691186729)) ;
#36112 = CARTESIAN_POINT('Ctrl Pts',(-15.3773813481496,-13.3239768187198,
-3.133503402729)) ;
#36113 = CARTESIAN_POINT('Ctrl Pts',(-14.9193693249711,-13.8349059995625,
-3.11674068766792)) ;
#36114 = CARTESIAN_POINT('Ctrl Pts',(-13.9983046704741,-14.7633478698724,
-3.08429713304078)) ;
#36115 = CARTESIAN_POINT('Ctrl Pts',(-13.5401522683127,-15.1846382880166,
-3.06867986646868)) ;
#36116 = CARTESIAN_POINT('Ctrl Pts',(-12.273494607637,-16.246406544396,-3.02682294982442)) ;
#36117 = CARTESIAN_POINT('Ctrl Pts',(-11.4343779880079,-16.847533591618,-3.00035128809016)) ;
#36118 = CARTESIAN_POINT('Ctrl Pts',(-10.2573202563203,-17.5621546356799,
-2.96597026664429)) ;
#36119 = CARTESIAN_POINT('Ctrl Pts',(-9.95678235336474,-17.7342713265434,
-2.95743783011756)) ;
#36120 = CARTESIAN_POINT('Ctrl Pts',(-9.20534756741494,-18.1394892450863,
-2.9365538209568)) ;
#36121 = CARTESIAN_POINT('Ctrl Pts',(-8.74983841907269,-18.3635460865105,
-2.92426988918525)) ;
#36122 = CARTESIAN_POINT('Ctrl Pts',(-7.57919642304287,-18.8859082291014,
-2.89317653789288)) ;
#36123 = CARTESIAN_POINT('Ctrl Pts',(-6.85452267548015,-19.1608260831607,
-2.874342072748)) ;
#36124 = CARTESIAN_POINT('Ctrl Pts',(-5.56729315337474,-19.5667622311266,
-2.84095791844988)) ;
#36125 = CARTESIAN_POINT('Ctrl Pts',(-5.01155363446369,-19.7164210453311,
-2.82657401849589)) ;
#36126 = CARTESIAN_POINT('Ctrl Pts',(-3.76434522106229,-19.9961441505205,
-2.79431156345238)) ;
#36127 = CARTESIAN_POINT('Ctrl Pts',(-3.07095541609495,-20.1143058864918,
-2.77638121592286)) ;
#36128 = CARTESIAN_POINT('Ctrl Pts',(-1.9109392768459,-20.2505950739922,-2.74669961807585)) ;
#36129 = CARTESIAN_POINT('Ctrl Pts',(-1.44730307479802,-20.2890021451473,
-2.73492410963611)) ;
#36130 = CARTESIAN_POINT('Ctrl Pts',(-0.626954948110609,-20.3286941224461,
-2.71443328580762)) ;
#36131 = CARTESIAN_POINT('Ctrl Pts',(-0.270762259295128,-20.3365573588638,
-2.70566650212191)) ;
#36132 = CARTESIAN_POINT('Ctrl Pts',(0.629321581591579,-20.3327749817555,
-2.6836673689249)) ;
#36133 = CARTESIAN_POINT('Ctrl Pts',(1.17288107122135,-20.3086714890162,-2.67051431989398)) ;
#36134 = CARTESIAN_POINT('Ctrl Pts',(2.43130969904529,-20.2021719751195,-2.63986861127068)) ;
#36135 = CARTESIAN_POINT('Ctrl Pts',(3.14407350940222,-20.1035770788437,-2.62235408269805)) ;
#36136 = CARTESIAN_POINT('Ctrl Pts',(4.41601894790743,-19.8583211785809,-2.59031105777517)) ;
#36137 = CARTESIAN_POINT('Ctrl Pts',(4.97702696327167,-19.7251954957874,-2.57589920033517)) ;
#36138 = CARTESIAN_POINT('Ctrl Pts',(6.21209824809652,-19.376064520588,-2.54350015905168)) ;
#36139 = CARTESIAN_POINT('Ctrl Pts',(6.88207995319268,-19.1483422019311,-2.52545957319964)) ;
#36140 = CARTESIAN_POINT('Ctrl Pts',(7.96696701704833,-18.7152859913309,-2.49577841572246)) ;
#36141 = CARTESIAN_POINT('Ctrl Pts',(8.38917057033345,-18.5298762748669,-2.48410975236042)) ;
#36142 = CARTESIAN_POINT('Ctrl Pts',(9.12911082110965,-18.1744556599384,-2.46363482643909)) ;
#36143 = CARTESIAN_POINT('Ctrl Pts',(9.44931891438479,-18.0100492850482,-2.45478133249999)) ;
#36144 = CARTESIAN_POINT('Ctrl Pts',(10.25391352465,-17.5695738505339,-2.43236865412459)) ;
#36145 = CARTESIAN_POINT('Ctrl Pts',(10.7316215597439,-17.2819261129632,-2.41889297829457)) ;
#36146 = CARTESIAN_POINT('Ctrl Pts',(11.7856830911829,-16.5866554654144,-2.38824614270176)) ;
#36147 = CARTESIAN_POINT('Ctrl Pts',(12.3538488586625,-16.1679273323465,-2.37105567099732)) ;
#36148 = CARTESIAN_POINT('Ctrl Pts',(13.3470239570827,-15.3530011744314,-2.33926772330736)) ;
#36149 = CARTESIAN_POINT('Ctrl Pts',(13.7790261411589,-14.9665000387234,-2.32477401215987)) ;
#36150 = CARTESIAN_POINT('Ctrl Pts',(14.7092110958243,-14.0598316175406,-2.29197434772223)) ;
#36151 = CARTESIAN_POINT('Ctrl Pts',(15.1974680285817,-13.5305844023817,-2.27361024388068)) ;
#36152 = CARTESIAN_POINT('Ctrl Pts',(15.9399896757244,-12.6347091686847,-2.24405621502609)) ;
#36153 = CARTESIAN_POINT('Ctrl Pts',(16.2120666867259,-12.2836494797824,-2.23282498533318)) ;
#36154 = CARTESIAN_POINT('Ctrl Pts',(16.6870212631333,-11.6275205233157,-2.21262927117704)) ;
#36155 = CARTESIAN_POINT('Ctrl Pts',(16.893567392919,-11.3253385544376,-2.20363190181635)) ;
#36156 = CARTESIAN_POINT('Ctrl Pts',(17.4061026073839,-10.5302419978033,-2.18052815892107)) ;
#36157 = CARTESIAN_POINT('Ctrl Pts',(17.6993580095662,-10.0295131625774,-2.16651221541519)) ;
#36158 = CARTESIAN_POINT('Ctrl Pts',(18.0252615792884,-9.41411009224698,-2.1496040846359)) ;
#36159 = CARTESIAN_POINT('Ctrl Pts',(18.078826114347,-9.31083051511026,-2.14677721575038)) ;
#36160 = CARTESIAN_POINT('Ctrl Pts',(18.1314964473001,-9.2071071699608,-2.14394731121824)) ;
#36161 = CARTESIAN_POINT('Ctrl Pts',(18.1314964405117,-9.20710718332915,-1.50729947444597)) ;
#36162 = CARTESIAN_POINT('Ctrl Pts',(17.931679960588,-9.60060448083557,-1.51823187387938)) ;
#36163 = CARTESIAN_POINT('Ctrl Pts',(17.7191046873647,-9.98749663233832,-1.5290015688187)) ;
#36164 = CARTESIAN_POINT('Ctrl Pts',(17.1281981947186,-10.9846234998532,-1.55717469977094)) ;
#36165 = CARTESIAN_POINT('Ctrl Pts',(16.7298560809444,-11.5822727656112,-1.57450204871407)) ;
#36166 = CARTESIAN_POINT('Ctrl Pts',(15.9545411699598,-12.6218042253867,-1.60619443826675)) ;
#36167 = CARTESIAN_POINT('Ctrl Pts',(15.5886620159045,-13.0709959220834,-1.62046639596972)) ;
#36168 = CARTESIAN_POINT('Ctrl Pts',(14.7558371702652,-14.0086739984771,-1.65174617509447)) ;
#36169 = CARTESIAN_POINT('Ctrl Pts',(14.2827086477002,-14.4907521949825,-1.66880058980069)) ;
#36170 = CARTESIAN_POINT('Ctrl Pts',(13.3631368055728,-15.3388471891994,-1.70059535045569)) ;
#36171 = CARTESIAN_POINT('Ctrl Pts',(12.9233906504269,-15.7111308707512,-1.71528951228431)) ;
#36172 = CARTESIAN_POINT('Ctrl Pts',(12.1801583387756,-16.28799860044,-1.73907935903575)) ;
#36173 = CARTESIAN_POINT('Ctrl Pts',(11.8859047649343,-16.5039519441112,-1.748245547445)) ;
#36174 = CARTESIAN_POINT('Ctrl Pts',(11.2171270537096,-16.9676017320783,-1.76841089369576)) ;
#36175 = CARTESIAN_POINT('Ctrl Pts',(10.8398896254436,-17.2110501102726,-1.7793635901593)) ;
#36176 = CARTESIAN_POINT('Ctrl Pts',(9.84075242908301,-17.8099489333762,-1.80767708616042)) ;
#36177 = CARTESIAN_POINT('Ctrl Pts',(9.20758678954942,-18.1453860492822,-1.82496471288984)) ;
#36178 = CARTESIAN_POINT('Ctrl Pts',(8.03323387083179,-18.6902074591705,-1.85660421164305)) ;
#36179 = CARTESIAN_POINT('Ctrl Pts',(7.49826929292229,-18.911177935506,-1.87086378527517)) ;
#36180 = CARTESIAN_POINT('Ctrl Pts',(6.32063693777119,-19.3397699396133,-1.90212207100057)) ;
#36181 = CARTESIAN_POINT('Ctrl Pts',(5.67557303286072,-19.5388078214488,-1.91916746525642)) ;
#36182 = CARTESIAN_POINT('Ctrl Pts',(4.46336522351739,-19.8477323571006,-1.95096385584129)) ;
#36183 = CARTESIAN_POINT('Ctrl Pts',(3.89911576652593,-19.966246663739,-1.96566886219092)) ;
#36184 = CARTESIAN_POINT('Ctrl Pts',(2.97056623354441,-20.1204104515116,-1.98947076388529)) ;
#36185 = CARTESIAN_POINT('Ctrl Pts',(2.60898812358905,-20.1704825854934,-1.99863835351361)) ;
#36186 = CARTESIAN_POINT('Ctrl Pts',(1.7704147312209,-20.2636827344797,-2.01954710877414)) ;
#36187 = CARTESIAN_POINT('Ctrl Pts',(1.29285219851626,-20.2997474260199,-2.03121840685039)) ;
#36188 = CARTESIAN_POINT('Ctrl Pts',(0.114827243913788,-20.3469671807111,
-2.0598584861084)) ;
#36189 = CARTESIAN_POINT('Ctrl Pts',(-0.585785981426001,-20.3388572127459,
-2.07677256901841)) ;
#36190 = CARTESIAN_POINT('Ctrl Pts',(-1.85799711370025,-20.2583305087049,
-2.10793922852146)) ;
#36191 = CARTESIAN_POINT('Ctrl Pts',(-2.42961215087073,-20.1977495076431,
-2.12210708924134)) ;
#36192 = CARTESIAN_POINT('Ctrl Pts',(-3.72189028244642,-20.0051328435108,
-2.15470718588174)) ;
#36193 = CARTESIAN_POINT('Ctrl Pts',(-4.43953009968398,-19.8582064770843,
-2.17322951128812)) ;
#36194 = CARTESIAN_POINT('Ctrl Pts',(-5.6633056996895,-19.5379894415735,-2.20540541298524)) ;
#36195 = CARTESIAN_POINT('Ctrl Pts',(-6.17343150103331,-19.3828482896351,
-2.21899493987718)) ;
#36196 = CARTESIAN_POINT('Ctrl Pts',(-7.01052651262709,-19.0918642557179,
-2.2413860423993)) ;
#36197 = CARTESIAN_POINT('Ctrl Pts',(-7.3411057299747,-18.9672068466635,-2.25024848035673)) ;
#36198 = CARTESIAN_POINT('Ctrl Pts',(-8.09973310493635,-18.658331277792,-2.27053048643341)) ;
#36199 = CARTESIAN_POINT('Ctrl Pts',(-8.52503137253512,-18.4678869402404,
-2.28188655391473)) ;
#36200 = CARTESIAN_POINT('Ctrl Pts',(-9.57283390191909,-17.9547767688043,
-2.31022903436473)) ;
#36201 = CARTESIAN_POINT('Ctrl Pts',(-10.1858964435259,-17.6142178533954,
-2.32715837737893)) ;
#36202 = CARTESIAN_POINT('Ctrl Pts',(-11.2675460356486,-16.937969215499,-2.35834655001133)) ;
#36203 = CARTESIAN_POINT('Ctrl Pts',(-11.7417986043157,-16.6127226077643,
-2.37252040053138)) ;
#36204 = CARTESIAN_POINT('Ctrl Pts',(-12.7896829377169,-15.826760197692,-2.40520335689515)) ;
#36205 = CARTESIAN_POINT('Ctrl Pts',(-13.353381014675,-15.3541371600193,-2.42380469731094)) ;
#36206 = CARTESIAN_POINT('Ctrl Pts',(-14.2781528882038,-14.4892519524119,
-2.45601194955388)) ;
#36207 = CARTESIAN_POINT('Ctrl Pts',(-14.651698515326,-14.111406879844,-2.46955314804877)) ;
#36208 = CARTESIAN_POINT('Ctrl Pts',(-15.2480086758211,-13.4589988018858,
-2.49188352326496)) ;
#36209 = CARTESIAN_POINT('Ctrl Pts',(-15.4791814507536,-13.1924738048849,
-2.50073309925654)) ;
#36210 = CARTESIAN_POINT('Ctrl Pts',(-15.9993633374509,-12.560234379475,-2.52100504250987)) ;
#36211 = CARTESIAN_POINT('Ctrl Pts',(-16.2829661866801,-12.1903294675225,
-2.53236368367608)) ;
#36212 = CARTESIAN_POINT('Ctrl Pts',(-16.9603847076335,-11.2408995733523,
-2.56069677309593)) ;
#36213 = CARTESIAN_POINT('Ctrl Pts',(-17.3374327804186,-10.6501594554693,
-2.57761453501714)) ;
#36214 = CARTESIAN_POINT('Ctrl Pts',(-17.9669902824396,-9.54145913085048,
-2.60878651550773)) ;
#36215 = CARTESIAN_POINT('Ctrl Pts',(-18.229420337493,-9.0299727804122,-2.62295595904236)) ;
#36216 = CARTESIAN_POINT('Ctrl Pts',(-18.7768009261932,-7.84168486601956,
-2.655599681445)) ;
#36217 = CARTESIAN_POINT('Ctrl Pts',(-19.0474751251439,-7.15918643759163,
-2.67416527045035)) ;
#36218 = CARTESIAN_POINT('Ctrl Pts',(-19.4497598633974,-5.95917948995069,
-2.706358581822)) ;
#36219 = CARTESIAN_POINT('Ctrl Pts',(-19.5989900371501,-5.44835479055282,
-2.71992188893821)) ;
#36220 = CARTESIAN_POINT('Ctrl Pts',(-19.8136287671889,-4.58984561078642,
-2.74227980842077)) ;
#36221 = CARTESIAN_POINT('Ctrl Pts',(-19.8903100757725,-4.2452489795954,-2.75113504185427)) ;
#36222 = CARTESIAN_POINT('Ctrl Pts',(-20.0473124236452,-3.44155844627817,
-2.77141131862243)) ;
#36223 = CARTESIAN_POINT('Ctrl Pts',(-20.1208997509695,-2.98135181708414,
-2.78276871851628)) ;
#36224 = CARTESIAN_POINT('Ctrl Pts',(-20.2654039335711,-1.82380183773396,
-2.81110713779146)) ;
#36225 = CARTESIAN_POINT('Ctrl Pts',(-20.3162055848214,-1.12456194766157,
-2.82803125954087)) ;
#36226 = CARTESIAN_POINT('Ctrl Pts',(-20.3428032991933,0.150504483196495,
-2.85921209444023)) ;
#36227 = CARTESIAN_POINT('Ctrl Pts',(-20.3304243301488,0.725352551259077,
-2.87338391920243)) ;
#36228 = CARTESIAN_POINT('Ctrl Pts',(-20.2468210857837,2.03155072083549,-2.90604166894579)) ;
#36229 = CARTESIAN_POINT('Ctrl Pts',(-20.1602868809396,2.7611193008484,-2.9246191867066)) ;
#36230 = CARTESIAN_POINT('Ctrl Pts',(-19.9433911357388,4.00821911015401,-2.95681697117818)) ;
#36231 = CARTESIAN_POINT('Ctrl Pts',(-19.8317802280077,4.5282628989769,-2.97037272203585)) ;
#36232 = CARTESIAN_POINT('Ctrl Pts',(-19.6123967152931,5.38520338436748,-2.9927213559517)) ;
#36233 = CARTESIAN_POINT('Ctrl Pts',(-19.5159902179828,5.72474037613498,-3.00157477901812)) ;
#36234 = CARTESIAN_POINT('Ctrl Pts',(-19.2719081461799,6.50635360558748,-3.02184972770117)) ;
#36235 = CARTESIAN_POINT('Ctrl Pts',(-19.1177750820932,6.946204880368,-3.03320759258375)) ;
#36236 = CARTESIAN_POINT('Ctrl Pts',(-18.6944326197623,8.03311120996374,-3.0615436430039)) ;
#36237 = CARTESIAN_POINT('Ctrl Pts',(-18.4066389319981,8.67227358385617,-3.07846502264682)) ;
#36238 = CARTESIAN_POINT('Ctrl Pts',(-17.8237475696155,9.80644029831512,-3.10964206395009)) ;
#36239 = CARTESIAN_POINT('Ctrl Pts',(-17.5395098600439,10.3062037006224,-3.12381288683432)) ;
#36240 = CARTESIAN_POINT('Ctrl Pts',(-16.8452234401258,11.4148288191342,-3.15645108432189)) ;
#36241 = CARTESIAN_POINT('Ctrl Pts',(-16.4226182843025,12.0148850578971,-3.17500951984659)) ;
#36242 = CARTESIAN_POINT('Ctrl Pts',(-15.6390393910186,13.0086748133683,-3.20720028692804)) ;
#36243 = CARTESIAN_POINT('Ctrl Pts',(-15.2932736843599,13.4134617064196,-3.22076826265459)) ;
#36244 = CARTESIAN_POINT('Ctrl Pts',(-14.6923896364129,14.0634382065645,-3.24313224922067)) ;
#36245 = CARTESIAN_POINT('Ctrl Pts',(-14.4460376142167,14.3163756175292,-3.25198891965484)) ;
#36246 = CARTESIAN_POINT('Ctrl Pts',(-13.8595737623538,14.8879570933692,-3.27226638233046)) ;
#36247 = CARTESIAN_POINT('Ctrl Pts',(-13.5148453314719,15.2015792748605,-3.28362356535633)) ;
#36248 = CARTESIAN_POINT('Ctrl Pts',(-12.625512279075,15.956481271788,-3.31196185955175)) ;
#36249 = CARTESIAN_POINT('Ctrl Pts',(-12.0683028909577,16.381969338984,-3.32888606359975)) ;
#36250 = CARTESIAN_POINT('Ctrl Pts',(-11.0160689380441,17.1025878764741,-3.36006674941463)) ;
#36251 = CARTESIAN_POINT('Ctrl Pts',(-10.5283403566255,17.4070769617992,-3.37423833645923)) ;
#36252 = CARTESIAN_POINT('Ctrl Pts',(-9.39716893216085,18.0483144709618,-3.40668178234294)) ;
#36253 = CARTESIAN_POINT('Ctrl Pts',(-8.74727002565604,18.3720900088539,-3.42503881544016)) ;
#36254 = CARTESIAN_POINT('Ctrl Pts',(-7.58854779621848,18.8739097072096,-3.45715533181558)) ;
#36255 = CARTESIAN_POINT('Ctrl Pts',(-7.08736400983769,19.067768565847,-3.47085224169067)) ;
#36256 = CARTESIAN_POINT('Ctrl Pts',(-6.24376845983031,19.3562116692087,-3.49337962385169)) ;
#36257 = CARTESIAN_POINT('Ctrl Pts',(-5.90549928457571,19.4620826003385,-3.5022719485616)) ;
#36258 = CARTESIAN_POINT('Ctrl Pts',(-5.1168192141225,19.6864652854163,-3.52257739844244)) ;
#36259 = CARTESIAN_POINT('Ctrl Pts',(-4.66475971933943,19.7984538934229,-3.53392759252148)) ;
#36260 = CARTESIAN_POINT('Ctrl Pts',(-3.52285661358665,20.0400523410299,-3.56228262981554)) ;
#36261 = CARTESIAN_POINT('Ctrl Pts',(-2.82940544657397,20.1496570844654,-3.57922972254332)) ;
#36262 = CARTESIAN_POINT('Ctrl Pts',(-1.55988901236768,20.2834738028633,-3.61043926899561)) ;
#36263 = CARTESIAN_POINT('Ctrl Pts',(-0.985803598136994,20.3194671830052,
-3.62461636408733)) ;
#36264 = CARTESIAN_POINT('Ctrl Pts',(0.34907381416042,20.3464501795615,-3.65792906066143)) ;
#36265 = CARTESIAN_POINT('Ctrl Pts',(1.10937474094696,20.3191820208798,-3.67717624096812)) ;
#36266 = CARTESIAN_POINT('Ctrl Pts',(2.56050338015072,20.1854339997927,-3.71425133826466)) ;
#36267 = CARTESIAN_POINT('Ctrl Pts',(3.25090648785058,20.0858043470427,-3.73203484978193)) ;
#36268 = CARTESIAN_POINT('Ctrl Pts',(4.24844578666855,19.8890642328277,-3.75748739774337)) ;
#36269 = CARTESIAN_POINT('Ctrl Pts',(4.56055729021179,19.8198255676919,-3.76539766653791)) ;
#36270 = CARTESIAN_POINT('Ctrl Pts',(5.65433088606337,19.5499777724197,-3.7930408743695)) ;
#36271 = CARTESIAN_POINT('Ctrl Pts',(6.42555507314387,19.3102393688022,-3.81246499702841)) ;
#36272 = CARTESIAN_POINT('Ctrl Pts',(7.79738916061737,18.7924845669388,-3.84813547191183)) ;
#36273 = CARTESIAN_POINT('Ctrl Pts',(8.40259026412085,18.5297927888828,-3.86428651998511)) ;
#36274 = CARTESIAN_POINT('Ctrl Pts',(9.58503196085372,17.946684428984,-3.89703783010886)) ;
#36275 = CARTESIAN_POINT('Ctrl Pts',(10.1615843856654,17.6266420549615,-3.91361863943306)) ;
#36276 = CARTESIAN_POINT('Ctrl Pts',(11.4240029594834,16.8433226018647,-3.95130391409726)) ;
#36277 = CARTESIAN_POINT('Ctrl Pts',(12.0992007970443,16.3650450229797,-3.97246317545991)) ;
#36278 = CARTESIAN_POINT('Ctrl Pts',(12.8553587923976,15.7569785546575,-3.99687002616268)) ;
#36279 = CARTESIAN_POINT('Ctrl Pts',(12.9663512222465,15.6657702985513,-4.00047068462399)) ;
#36280 = CARTESIAN_POINT('Ctrl Pts',(13.3504290834985,15.3432751705168,-4.01298161554906)) ;
#36281 = CARTESIAN_POINT('Ctrl Pts',(13.618367782473,15.1059626914056,-4.02178721215786)) ;
#36282 = CARTESIAN_POINT('Ctrl Pts',(14.4833505067786,14.2981227520694,-4.05071069258373)) ;
#36283 = CARTESIAN_POINT('Ctrl Pts',(15.051911897898,13.6983106067469,-4.0705832408216)) ;
#36284 = CARTESIAN_POINT('Ctrl Pts',(15.9716005878999,12.6014615600297,-4.10549367227418)) ;
#36285 = CARTESIAN_POINT('Ctrl Pts',(16.3398350154851,12.1201749904149,-4.12038340043091)) ;
#36286 = CARTESIAN_POINT('Ctrl Pts',(17.0915947667932,11.0409612257292,-4.15312801458585)) ;
#36287 = CARTESIAN_POINT('Ctrl Pts',(17.4664003687829,10.4379250757297,-4.17103695047986)) ;
#36288 = CARTESIAN_POINT('Ctrl Pts',(18.0918294018035,9.30328775361926,-4.20396119083834)) ;
#36289 = CARTESIAN_POINT('Ctrl Pts',(18.3524219535583,8.77804437935544,-4.21891726249764)) ;
#36290 = CARTESIAN_POINT('Ctrl Pts',(18.7389458071928,7.90626329195108,-4.24303579536137)) ;
#36291 = CARTESIAN_POINT('Ctrl Pts',(18.878790832447,7.56626408438369,-4.25227098886652)) ;
#36292 = CARTESIAN_POINT('Ctrl Pts',(19.165662910752,6.81124419867061,-4.2722892913204)) ;
#36293 = CARTESIAN_POINT('Ctrl Pts',(19.3085844787189,6.39486142599375,-4.28303329335084)) ;
#36294 = CARTESIAN_POINT('Ctrl Pts',(19.6501461161649,5.28353754798832,-4.31129854211033)) ;
#36295 = CARTESIAN_POINT('Ctrl Pts',(19.8254506778058,4.5820865525839,-4.3287387600465)) ;
#36296 = CARTESIAN_POINT('Ctrl Pts',(20.0735365754715,3.30328165574474,-4.36057039461972)) ;
#36297 = CARTESIAN_POINT('Ctrl Pts',(20.1595990429213,2.72930371006243,-4.37486635117816)) ;
#36298 = CARTESIAN_POINT('Ctrl Pts',(20.2941852977256,1.46493687931805,-4.40657679710737)) ;
#36299 = CARTESIAN_POINT('Ctrl Pts',(20.3322567287544,0.774157649557999,-4.42404857398858)) ;
#36300 = CARTESIAN_POINT('Ctrl Pts',(20.3373822022035,-0.484781177569453,
-4.45605319658284)) ;
#36301 = CARTESIAN_POINT('Ctrl Pts',(20.3159298056552,-1.05219992621706,-4.47053345588276)) ;
#36302 = CARTESIAN_POINT('Ctrl Pts',(20.2419180649595,-1.97945371830992,-4.49405182864441)) ;
#36303 = CARTESIAN_POINT('Ctrl Pts',(20.20340142889,-2.34009849004814,-4.50315872875805)) ;
#36304 = CARTESIAN_POINT('Ctrl Pts',(20.09513401912,-3.1484475524981,-4.52336630592519)) ;
#36305 = CARTESIAN_POINT('Ctrl Pts',(20.0200247136739,-3.59523975853926,-4.53441644919468)) ;
#36306 = CARTESIAN_POINT('Ctrl Pts',(19.7884420576793,-4.73791899084519,-4.56275156300918)) ;
#36307 = CARTESIAN_POINT('Ctrl Pts',(19.610174850103,-5.42875285913641,-4.57996688218247)) ;
#36308 = CARTESIAN_POINT('Ctrl Pts',(19.2224294398213,-6.65988090871565,-4.61151468807607)) ;
#36309 = CARTESIAN_POINT('Ctrl Pts',(19.0254576747953,-7.20331587378892,-4.6257563455703)) ;
#36310 = CARTESIAN_POINT('Ctrl Pts',(18.6004501997403,-8.23625949884474,-4.65361808332889)) ;
#36311 = CARTESIAN_POINT('Ctrl Pts',(18.3755607890832,-8.72647284682466,-4.66720239419565)) ;
#36312 = CARTESIAN_POINT('Ctrl Pts',(18.1314964277493,-9.20710720846217,-4.68087293438847)) ;
#36313 = CARTESIAN_POINT('Origin',(0.,0.,5.8748638224677)) ;
#36314 = CARTESIAN_POINT('',(18.1314964426296,-9.20710717915839,-8.49264489791374)) ;
#36315 = CARTESIAN_POINT('',(18.1314964397986,-9.2071071847335,-7.85560087779543)) ;
#36316 = CARTESIAN_POINT('',(18.1314964405232,-9.20710718330643,5.8748638224677)) ;
#36317 = CARTESIAN_POINT('Ctrl Pts',(18.131496444736,-9.20710717501038,-8.49264489791374)) ;
#36318 = CARTESIAN_POINT('Ctrl Pts',(18.1932674928183,-9.08546185065345,-8.48921597676009)) ;
#36319 = CARTESIAN_POINT('Ctrl Pts',(18.2538163712279,-8.96319091114333,-8.48579881785955)) ;
#36320 = CARTESIAN_POINT('Ctrl Pts',(18.4728147531323,-8.50952521834696,-8.4732394955958)) ;
#36321 = CARTESIAN_POINT('Ctrl Pts',(18.6235044093928,-8.17447174954134,-8.46421003414079)) ;
#36322 = CARTESIAN_POINT('Ctrl Pts',(18.9904852834932,-7.29560107995186,-8.44095127109311)) ;
#36323 = CARTESIAN_POINT('Ctrl Pts',(19.1925271143377,-6.74620138477858,-8.42681393123442)) ;
#36324 = CARTESIAN_POINT('Ctrl Pts',(19.5865814277305,-5.5128443631374,-8.39537318257033)) ;
#36325 = CARTESIAN_POINT('Ctrl Pts',(19.7670274914648,-4.82599611654746,-8.37805044530867)) ;
#36326 = CARTESIAN_POINT('Ctrl Pts',(20.0340665331976,-3.53892179136578,-8.3454695286419)) ;
#36327 = CARTESIAN_POINT('Ctrl Pts',(20.1304533551351,-2.941534835654,-8.33030467021252)) ;
#36328 = CARTESIAN_POINT('Ctrl Pts',(20.2948600824927,-1.52274471572167,-8.29416956240355)) ;
#36329 = CARTESIAN_POINT('Ctrl Pts',(20.3398733544353,-0.699744311822382,
-8.27309999793224)) ;
#36330 = CARTESIAN_POINT('Ctrl Pts',(20.3326732563183,0.483760817714732,-8.2431822172196)) ;
#36331 = CARTESIAN_POINT('Ctrl Pts',(20.3209206250887,0.843692761431439,-8.23414218048783)) ;
#36332 = CARTESIAN_POINT('Ctrl Pts',(20.2619672669607,1.83837644347612,-8.20945746357235)) ;
#36333 = CARTESIAN_POINT('Ctrl Pts',(20.1945184988773,2.47151386605704,-8.19402822491205)) ;
#36334 = CARTESIAN_POINT('Ctrl Pts',(19.9612492075238,3.9835945910032,-8.15692170200691)) ;
#36335 = CARTESIAN_POINT('Ctrl Pts',(19.7669429729029,4.85679412600449,-8.13525196739468)) ;
#36336 = CARTESIAN_POINT('Ctrl Pts',(19.3524424112644,6.27240414608569,-8.09874849696558)) ;
#36337 = CARTESIAN_POINT('Ctrl Pts',(19.1651896699438,6.82316474363552,-8.08420010532792)) ;
#36338 = CARTESIAN_POINT('Ctrl Pts',(18.690967904662,8.04360082058764,-8.05113229623419)) ;
#36339 = CARTESIAN_POINT('Ctrl Pts',(18.3911030964677,8.70741723048133,-8.03255152790795)) ;
#36340 = CARTESIAN_POINT('Ctrl Pts',(17.8452784204912,9.7610699717966,-8.00242067816574)) ;
#36341 = CARTESIAN_POINT('Ctrl Pts',(17.620533104815,10.1611646401539,-7.99082532445382)) ;
#36342 = CARTESIAN_POINT('Ctrl Pts',(17.1698355381235,10.9035120098911,-7.96921656654375)) ;
#36343 = CARTESIAN_POINT('Ctrl Pts',(16.9466879673368,11.2472039390264,-7.95917882762995)) ;
#36344 = CARTESIAN_POINT('Ctrl Pts',(15.9898515385722,12.6277299165048,-7.9182548591709)) ;
#36345 = CARTESIAN_POINT('Ctrl Pts',(15.1702019484581,13.6014667716605,-7.88775489658032)) ;
#36346 = CARTESIAN_POINT('Ctrl Pts',(13.8068741521705,14.9434136805402,-7.84025866223606)) ;
#36347 = CARTESIAN_POINT('Ctrl Pts',(13.327522494099,15.3724597544759,-7.82409645369742)) ;
#36348 = CARTESIAN_POINT('Ctrl Pts',(12.2147766604731,16.277198542221,-7.78774176398343)) ;
#36349 = CARTESIAN_POINT('Ctrl Pts',(11.5722923534326,16.7400719244327,-7.76750070324327)) ;
#36350 = CARTESIAN_POINT('Ctrl Pts',(10.6197969596022,17.345191026119,-7.73903165503595)) ;
#36351 = CARTESIAN_POINT('Ctrl Pts',(10.3306569328559,17.5189403838093,-7.73058763602346)) ;
#36352 = CARTESIAN_POINT('Ctrl Pts',(9.90571895203523,17.7601130953422,-7.71850594637521)) ;
#36353 = CARTESIAN_POINT('Ctrl Pts',(9.77328262245036,17.8333348573003,-7.71478237534946)) ;
#36354 = CARTESIAN_POINT('Ctrl Pts',(9.2597694124691,18.1098089481559,-7.70048200028835)) ;
#36355 = CARTESIAN_POINT('Ctrl Pts',(8.8730704250491,18.3023805470242,-7.68999991658958)) ;
#36356 = CARTESIAN_POINT('Ctrl Pts',(7.64276566526082,18.866895267784,-7.65716672155101)) ;
#36357 = CARTESIAN_POINT('Ctrl Pts',(6.77983813774774,19.1938893097623,-7.63483030379097)) ;
#36358 = CARTESIAN_POINT('Ctrl Pts',(5.33966402241091,19.6303335366024,-7.59758426882942)) ;
#36359 = CARTESIAN_POINT('Ctrl Pts',(4.77460210253822,19.7753678214987,-7.58299197760067)) ;
#36360 = CARTESIAN_POINT('Ctrl Pts',(3.48538919668097,20.0477841143969,-7.54970849235954)) ;
#36361 = CARTESIAN_POINT('Ctrl Pts',(2.75898443028803,20.1605948129092,-7.53095335906623)) ;
#36362 = CARTESIAN_POINT('Ctrl Pts',(1.60749515412967,20.2760107404773,-7.50157565350564)) ;
#36363 = CARTESIAN_POINT('Ctrl Pts',(1.18569852694703,20.3050430929132,-7.49089351167923)) ;
#36364 = CARTESIAN_POINT('Ctrl Pts',(0.391163179234408,20.334887761987,-7.47107658945271)) ;
#36365 = CARTESIAN_POINT('Ctrl Pts',(0.0187096304971401,20.3386410462601,
-7.46192636134628)) ;
#36366 = CARTESIAN_POINT('Ctrl Pts',(-0.957969681235675,20.3216536893527,
-7.43807945923731)) ;
#36367 = CARTESIAN_POINT('Ctrl Pts',(-1.56153474184536,20.2842038945325,-7.42348050899772)) ;
#36368 = CARTESIAN_POINT('Ctrl Pts',(-2.84926844815383,20.14647991131,-7.39201967694105)) ;
#36369 = CARTESIAN_POINT('Ctrl Pts',(-3.53180938168843,20.0380961108315,-7.37514712359831)) ;
#36370 = CARTESIAN_POINT('Ctrl Pts',(-4.80589160842951,19.7686486728442,-7.34285740243697)) ;
#36371 = CARTESIAN_POINT('Ctrl Pts',(-5.39825754073355,19.6151693824441,-7.32751406300869)) ;
#36372 = CARTESIAN_POINT('Ctrl Pts',(-6.79895095392575,19.1839900707252,-7.29042060741557)) ;
#36373 = CARTESIAN_POINT('Ctrl Pts',(-7.59846294567933,18.881593238979,-7.26855803393727)) ;
#36374 = CARTESIAN_POINT('Ctrl Pts',(-8.68544689161686,18.3902116635167,-7.2384580283756)) ;
#36375 = CARTESIAN_POINT('Ctrl Pts',(-8.99076791818554,18.2428882224929,-7.22996984157808)) ;
#36376 = CARTESIAN_POINT('Ctrl Pts',(-9.42613706030807,18.0192279668962,-7.21786500247111)) ;
#36377 = CARTESIAN_POINT('Ctrl Pts',(-9.55923899426645,17.9489717389519,-7.21416106077178)) ;
#36378 = CARTESIAN_POINT('Ctrl Pts',(-10.0674837841138,17.6734438538954,-7.19998303249942)) ;
#36379 = CARTESIAN_POINT('Ctrl Pts',(-10.4368979716341,17.4578352277467,-7.18960248119923)) ;
#36380 = CARTESIAN_POINT('Ctrl Pts',(-11.5875986240165,16.7366420037633,-7.15666140785297)) ;
#36381 = CARTESIAN_POINT('Ctrl Pts',(-12.3411126403601,16.1890257351276,-7.13412054761323)) ;
#36382 = CARTESIAN_POINT('Ctrl Pts',(-13.501895699122,15.2171388177069,-7.09664864954409)) ;
#36383 = CARTESIAN_POINT('Ctrl Pts',(-13.9329787510482,14.8234474888726,-7.08204510994786)) ;
#36384 = CARTESIAN_POINT('Ctrl Pts',(-14.8683485479531,13.8923117024224,-7.0487062932591)) ;
#36385 = CARTESIAN_POINT('Ctrl Pts',(-15.3615675319116,13.3448997181919,-7.02990641066344)) ;
#36386 = CARTESIAN_POINT('Ctrl Pts',(-16.0892022183127,12.4433854765112,-7.00049846000239)) ;
#36387 = CARTESIAN_POINT('Ctrl Pts',(-16.3441004827617,12.1066367480222,-6.98982903363529)) ;
#36388 = CARTESIAN_POINT('Ctrl Pts',(-16.8056078946816,11.4557686780552,-6.96994612776944)) ;
#36389 = CARTESIAN_POINT('Ctrl Pts',(-17.0143525322356,11.1433792677009,-6.96071894253681)) ;
#36390 = CARTESIAN_POINT('Ctrl Pts',(-17.5427302432451,10.3031630980202,-6.93649330215191)) ;
#36391 = CARTESIAN_POINT('Ctrl Pts',(-17.8472025903495,9.7662642678522,-6.9215962342594)) ;
#36392 = CARTESIAN_POINT('Ctrl Pts',(-18.4375850322338,8.60509571756327,-6.88994271837802)) ;
#36393 = CARTESIAN_POINT('Ctrl Pts',(-18.7172530796746,7.97851119947298,-6.87318002593854)) ;
#36394 = CARTESIAN_POINT('Ctrl Pts',(-19.189241589446,6.75884458700106,-6.84073651545719)) ;
#36395 = CARTESIAN_POINT('Ctrl Pts',(-19.3870100099025,6.16869558480859,-6.82511927024866)) ;
#36396 = CARTESIAN_POINT('Ctrl Pts',(-19.8397625058855,4.57910718211882,-6.78326233391622)) ;
#36397 = CARTESIAN_POINT('Ctrl Pts',(-20.0463315664789,3.5677699205246,-6.75679062883414)) ;
#36398 = CARTESIAN_POINT('Ctrl Pts',(-20.218677211945,2.20158745389991,-6.72240952422769)) ;
#36399 = CARTESIAN_POINT('Ctrl Pts',(-20.2532348093798,1.85698015649438,-6.71387704507936)) ;
#36400 = CARTESIAN_POINT('Ctrl Pts',(-20.3166990478875,1.00560412832394,-6.69299285041195)) ;
#36401 = CARTESIAN_POINT('Ctrl Pts',(-20.3354662319348,0.498313472598733,
-6.68070877754043)) ;
#36402 = CARTESIAN_POINT('Ctrl Pts',(-20.334889551072,-0.783581673061414,
-6.64961551101604)) ;
#36403 = CARTESIAN_POINT('Ctrl Pts',(-20.2903021214652,-1.55735749048991,
-6.63078127140845)) ;
#36404 = CARTESIAN_POINT('Ctrl Pts',(-20.1358720522922,-2.89820559516594,
-6.59739731442196)) ;
#36405 = CARTESIAN_POINT('Ctrl Pts',(-20.0458278439741,-3.4666578185139,-6.58301337638405)) ;
#36406 = CARTESIAN_POINT('Ctrl Pts',(-19.7924843776348,-4.71949604009386,
-6.5507507945064)) ;
#36407 = CARTESIAN_POINT('Ctrl Pts',(-19.6175340056101,-5.40078076590417,
-6.53282035727844)) ;
#36408 = CARTESIAN_POINT('Ctrl Pts',(-19.2687971071472,-6.51550049506038,
-6.5031387050621)) ;
#36409 = CARTESIAN_POINT('Ctrl Pts',(-19.1147465052204,-6.95447763417581,
-6.49136322954928)) ;
#36410 = CARTESIAN_POINT('Ctrl Pts',(-18.8163646253583,-7.71966982779728,
-6.47087234604565)) ;
#36411 = CARTESIAN_POINT('Ctrl Pts',(-18.6782510680693,-8.04809400935234,
-6.46210547202084)) ;
#36412 = CARTESIAN_POINT('Ctrl Pts',(-18.3076446776743,-8.86836772680735,
-6.44010590062631)) ;
#36413 = CARTESIAN_POINT('Ctrl Pts',(-18.063911901196,-9.3548324491682,-6.42695250827293)) ;
#36414 = CARTESIAN_POINT('Ctrl Pts',(-17.4533573106967,-10.4603689719171,
-6.39630676388711)) ;
#36415 = CARTESIAN_POINT('Ctrl Pts',(-17.0726065157728,-11.0709122222924,
-6.37879254438756)) ;
#36416 = CARTESIAN_POINT('Ctrl Pts',(-16.3298588994978,-12.1321826127183,
-6.34674976342576)) ;
#36417 = CARTESIAN_POINT('Ctrl Pts',(-15.9794738373463,-12.590097452661,-6.3323378287567)) ;
#36418 = CARTESIAN_POINT('Ctrl Pts',(-15.1569095298164,-13.5753509782339,
-6.29993835103382)) ;
#36419 = CARTESIAN_POINT('Ctrl Pts',(-14.6756963033449,-14.0941828888234,
-6.28189740023685)) ;
#36420 = CARTESIAN_POINT('Ctrl Pts',(-13.8377803886648,-14.9080618490359,
-6.25221642321969)) ;
#36421 = CARTESIAN_POINT('Ctrl Pts',(-13.4962940054707,-15.2179015218636,
-6.240548290746)) ;
#36422 = CARTESIAN_POINT('Ctrl Pts',(-12.8699771114681,-15.7484981462581,
-6.22007382416863)) ;
#36423 = CARTESIAN_POINT('Ctrl Pts',(-12.5892545875132,-15.9737964779749,
-6.21122027333049)) ;
#36424 = CARTESIAN_POINT('Ctrl Pts',(-11.8588835448729,-16.5287495145717,
-6.18880728908166)) ;
#36425 = CARTESIAN_POINT('Ctrl Pts',(-11.4013871290171,-16.8475830490838,
-6.17533136794391)) ;
#36426 = CARTESIAN_POINT('Ctrl Pts',(-10.3366323470895,-17.5263653729688,
-6.14468452283959)) ;
#36427 = CARTESIAN_POINT('Ctrl Pts',(-9.72257543638125,-17.8743103011633,
-6.12749428948782)) ;
#36428 = CARTESIAN_POINT('Ctrl Pts',(-8.57341777328908,-18.4486910524161,
-6.09570658249754)) ;
#36429 = CARTESIAN_POINT('Ctrl Pts',(-8.04431764871778,-18.6854659739644,
-6.08121286554617)) ;
#36430 = CARTESIAN_POINT('Ctrl Pts',(-6.83707999963106,-19.1649183674483,
-6.04841314798866)) ;
#36431 = CARTESIAN_POINT('Ctrl Pts',(-6.15470096420743,-19.3948294029144,
-6.03004899612453)) ;
#36432 = CARTESIAN_POINT('Ctrl Pts',(-5.03386769216678,-19.7073418079305,
-6.00049496899895)) ;
#36433 = CARTESIAN_POINT('Ctrl Pts',(-4.60236216404437,-19.8125569209369,
-5.98926378685334)) ;
#36434 = CARTESIAN_POINT('Ctrl Pts',(-3.80954984437051,-19.9785698825362,
-5.9690676990184)) ;
#36435 = CARTESIAN_POINT('Ctrl Pts',(-3.44938261443551,-20.0438939486088,
-5.9600699193788)) ;
#36436 = CARTESIAN_POINT('Ctrl Pts',(-2.51429977879769,-20.1875399508006,
-5.93696433519843)) ;
#36437 = CARTESIAN_POINT('Ctrl Pts',(-1.93744315322656,-20.2510441802163,
-5.92294697681138)) ;
#36438 = CARTESIAN_POINT('Ctrl Pts',(-0.635491093403947,-20.3382264991574,
-5.89126431651432)) ;
#36439 = CARTESIAN_POINT('Ctrl Pts',(0.0897453550806687,-20.3479542121509,
-5.8735748440604)) ;
#36440 = CARTESIAN_POINT('Ctrl Pts',(1.42352942581411,-20.2945248130426,-5.84047966504807)) ;
#36441 = CARTESIAN_POINT('Ctrl Pts',(2.0316997923572,-20.2426865635556,-5.8251769070561)) ;
#36442 = CARTESIAN_POINT('Ctrl Pts',(3.19842593928037,-20.0901241217493,-5.79539823306841)) ;
#36443 = CARTESIAN_POINT('Ctrl Pts',(3.7569215023495,-19.9932126866801,-5.78095573007756)) ;
#36444 = CARTESIAN_POINT('Ctrl Pts',(4.8247207349255,-19.7615984010064,-5.75317452714807)) ;
#36445 = CARTESIAN_POINT('Ctrl Pts',(5.33428659815078,-19.6301832425762,-5.73984266301656)) ;
#36446 = CARTESIAN_POINT('Ctrl Pts',(6.20531554825694,-19.3691233047096,-5.71719187551594)) ;
#36447 = CARTESIAN_POINT('Ctrl Pts',(6.56926329430078,-19.2487313784905,-5.70778343914778)) ;
#36448 = CARTESIAN_POINT('Ctrl Pts',(7.5377477943781,-18.8976926946415,-5.68265164402447)) ;
#36449 = CARTESIAN_POINT('Ctrl Pts',(8.13504068305113,-18.6483658256576,-5.66703828743495)) ;
#36450 = CARTESIAN_POINT('Ctrl Pts',(9.32515255716397,-18.0835025278383,-5.63500288632133)) ;
#36451 = CARTESIAN_POINT('Ctrl Pts',(9.91627795033413,-17.7662307555444,-5.61858951222894)) ;
#36452 = CARTESIAN_POINT('Ctrl Pts',(11.0466583143976,-17.0855081643718,-5.58582086193217)) ;
#36453 = CARTESIAN_POINT('Ctrl Pts',(11.5863165201075,-16.7242490655957,-5.56950011778613)) ;
#36454 = CARTESIAN_POINT('Ctrl Pts',(12.7483411379843,-15.8630853188755,-5.53282697474644)) ;
#36455 = CARTESIAN_POINT('Ctrl Pts',(13.3604378352449,-15.3511034160689,-5.51242739080587)) ;
#36456 = CARTESIAN_POINT('Ctrl Pts',(14.1818258335732,-14.5776310115413,-5.48398528020362)) ;
#36457 = CARTESIAN_POINT('Ctrl Pts',(14.4171882564254,-14.3449014606328,-5.47570885832489)) ;
#36458 = CARTESIAN_POINT('Ctrl Pts',(15.0760440458305,-13.660813311538,-5.45224112912472)) ;
#36459 = CARTESIAN_POINT('Ctrl Pts',(15.4847529342396,-13.1957327042059,-5.43724555280852)) ;
#36460 = CARTESIAN_POINT('Ctrl Pts',(16.4138990550934,-12.0357109092044,-5.40120091548751)) ;
#36461 = CARTESIAN_POINT('Ctrl Pts',(16.9123007715931,-11.3246849799612,-5.38015222413626)) ;
#36462 = CARTESIAN_POINT('Ctrl Pts',(17.6373946762965,-10.1351205510364,-5.34568057294485)) ;
#36463 = CARTESIAN_POINT('Ctrl Pts',(17.893492917947,-9.67580597644696,-5.33254408539732)) ;
#36464 = CARTESIAN_POINT('Ctrl Pts',(18.1314964428552,-9.20710717871412,-5.31929120111857)) ;
#36465 = CARTESIAN_POINT('Ctrl Pts',(18.1314964277493,-9.20710720846216,-4.68087293438847)) ;
#36466 = CARTESIAN_POINT('Ctrl Pts',(18.0523186452368,-9.36303150132383,-4.68530784267373)) ;
#36467 = CARTESIAN_POINT('Ctrl Pts',(17.9711228049512,-9.51794767764142,-4.6897511590617)) ;
#36468 = CARTESIAN_POINT('Ctrl Pts',(17.6266893201308,-10.1549739633927,-4.70816687118514)) ;
#36469 = CARTESIAN_POINT('Ctrl Pts',(17.3459827772761,-10.6273494016093,-4.7221755114788)) ;
#36470 = CARTESIAN_POINT('Ctrl Pts',(16.8514746170197,-11.3876126790035,-4.74509759838492)) ;
#36471 = CARTESIAN_POINT('Ctrl Pts',(16.6485719905417,-11.6822504765265,-4.75407572346182)) ;
#36472 = CARTESIAN_POINT('Ctrl Pts',(16.1645160437808,-12.3469113555224,-4.7744420263802)) ;
#36473 = CARTESIAN_POINT('Ctrl Pts',(15.8782408678854,-12.7129568319709,-4.78576912166363)) ;
#36474 = CARTESIAN_POINT('Ctrl Pts',(15.1272276196611,-13.6082552580042,-4.81416040569896)) ;
#36475 = CARTESIAN_POINT('Ctrl Pts',(14.6470714677209,-14.1237715717995,-4.83116467092485)) ;
#36476 = CARTESIAN_POINT('Ctrl Pts',(13.7275412161976,-15.0135893299879,-4.86244627437124)) ;
#36477 = CARTESIAN_POINT('Ctrl Pts',(13.2971302422379,-15.3960894973893,-4.87663709220211)) ;
#36478 = CARTESIAN_POINT('Ctrl Pts',(12.2923176824295,-16.2154471370018,-4.90898445864983)) ;
#36479 = CARTESIAN_POINT('Ctrl Pts',(11.7097251327719,-16.6410373002128,-4.92722230095032)) ;
#36480 = CARTESIAN_POINT('Ctrl Pts',(10.6522173054578,-17.3304759122839,-4.95932864520367)) ;
#36481 = CARTESIAN_POINT('Ctrl Pts',(10.1870366082399,-17.6079361468506,-4.97313551388248)) ;
#36482 = CARTESIAN_POINT('Ctrl Pts',(9.39895532900243,-18.0362978148204,-4.99580215751323)) ;
#36483 = CARTESIAN_POINT('Ctrl Pts',(9.08216866487118,-18.1978740154346,-5.00472479228085)) ;
#36484 = CARTESIAN_POINT('Ctrl Pts',(8.34142296047336,-18.5515264932037,-5.0250532362406)) ;
#36485 = CARTESIAN_POINT('Ctrl Pts',(7.91478173495953,-18.7375213898214,-5.03639671589767)) ;
#36486 = CARTESIAN_POINT('Ctrl Pts',(6.82898138842262,-19.1671699920706,-5.06476550979927)) ;
#36487 = CARTESIAN_POINT('Ctrl Pts',(6.16287660469016,-19.3916049762649,-5.08173233593433)) ;
#36488 = CARTESIAN_POINT('Ctrl Pts',(4.93266189503718,-19.7363027731233,-5.11296674033377)) ;
#36489 = CARTESIAN_POINT('Ctrl Pts',(4.37249641020224,-19.8679155362104,-5.12714855901422)) ;
#36490 = CARTESIAN_POINT('Ctrl Pts',(3.09846408611006,-20.1107562768848,-5.15950800860268)) ;
#36491 = CARTESIAN_POINT('Ctrl Pts',(2.3827303204123,-20.2080572831549,-5.17776777172363)) ;
#36492 = CARTESIAN_POINT('Ctrl Pts',(1.12488481625565,-20.3112903407755,-5.20986644447541)) ;
#36493 = CARTESIAN_POINT('Ctrl Pts',(0.584874102586749,-20.3340061177622,
-5.22364359864288)) ;
#36494 = CARTESIAN_POINT('Ctrl Pts',(-0.310632077300816,-20.3359702145692,
-5.24627261087276)) ;
#36495 = CARTESIAN_POINT('Ctrl Pts',(-0.665828451570617,-20.3274409486539,
-5.25518705775032)) ;
#36496 = CARTESIAN_POINT('Ctrl Pts',(-1.48540360645998,-20.2862546658499,
-5.27550939406321)) ;
#36497 = CARTESIAN_POINT('Ctrl Pts',(-1.94924850372538,-20.2469500918845,
-5.28685478750299)) ;
#36498 = CARTESIAN_POINT('Ctrl Pts',(-3.10858582711033,-20.1084998925431,
-5.31521995017413)) ;
#36499 = CARTESIAN_POINT('Ctrl Pts',(-3.80105142593879,-19.9891740977748,
-5.33218143203738)) ;
#36500 = CARTESIAN_POINT('Ctrl Pts',(-5.04689461541006,-19.7073993924063,
-5.36340910001509)) ;
#36501 = CARTESIAN_POINT('Ctrl Pts',(-5.60219651994496,-19.5567922296115,
-5.37758963507189)) ;
#36502 = CARTESIAN_POINT('Ctrl Pts',(-6.88185689440415,-19.1507438043911,
-5.41108617195795)) ;
#36503 = CARTESIAN_POINT('Ctrl Pts',(-7.59961829259005,-18.8774131380579,
-5.43051941813763)) ;
#36504 = CARTESIAN_POINT('Ctrl Pts',(-8.76716071463369,-18.3553947435915,
-5.46305851184877)) ;
#36505 = CARTESIAN_POINT('Ctrl Pts',(-9.22607405494234,-18.1290700920658,
-5.47609430972741)) ;
#36506 = CARTESIAN_POINT('Ctrl Pts',(-9.98149972271132,-17.7203928156439,
-5.49778391185284)) ;
#36507 = CARTESIAN_POINT('Ctrl Pts',(-10.2827520333698,-17.5472982222961,
-5.5064932719995)) ;
#36508 = CARTESIAN_POINT('Ctrl Pts',(-11.4618939357414,-16.8289845265552,
-5.54066571611911)) ;
#36509 = CARTESIAN_POINT('Ctrl Pts',(-12.3021110078318,-16.2249142478387,
-5.56541565375218)) ;
#36510 = CARTESIAN_POINT('Ctrl Pts',(-13.5683529946967,-15.1594227991939,
-5.6057400748679)) ;
#36511 = CARTESIAN_POINT('Ctrl Pts',(-14.0253292971861,-14.7376535327089,
-5.62100081478672)) ;
#36512 = CARTESIAN_POINT('Ctrl Pts',(-14.944566972909,-13.8077001509719,-5.653529486803)) ;
#36513 = CARTESIAN_POINT('Ctrl Pts',(-15.4018613095405,-13.2956880269988,
-5.67082389327669)) ;
#36514 = CARTESIAN_POINT('Ctrl Pts',(-16.2191211190515,-12.2817686118603,
-5.7038957899571)) ;
#36515 = CARTESIAN_POINT('Ctrl Pts',(-16.5838349768186,-11.7846572875102,
-5.71962798801488)) ;
#36516 = CARTESIAN_POINT('Ctrl Pts',(-17.1335305179989,-10.9592468818078,
-5.74472164879162)) ;
#36517 = CARTESIAN_POINT('Ctrl Pts',(-17.3329570886999,-10.6410321419026,
-5.75416185539592)) ;
#36518 = CARTESIAN_POINT('Ctrl Pts',(-17.7374233266058,-9.95407646846906,
-5.77392877806474)) ;
#36519 = CARTESIAN_POINT('Ctrl Pts',(-17.9400311561078,-9.58410721721756,
-5.78423300381752)) ;
#36520 = CARTESIAN_POINT('Ctrl Pts',(-18.4644945166908,-8.5514256546696,-5.81240688096996)) ;
#36521 = CARTESIAN_POINT('Ctrl Pts',(-18.7620766322954,-7.87711369197664,
-5.83017715348359)) ;
#36522 = CARTESIAN_POINT('Ctrl Pts',(-19.2287110709534,-6.64223127829799,
-5.86242550382837)) ;
#36523 = CARTESIAN_POINT('Ctrl Pts',(-19.4114029600428,-6.08769191180265,
-5.87680124775349)) ;
#36524 = CARTESIAN_POINT('Ctrl Pts',(-19.8231473315249,-4.62954228969047,
-5.914577844863)) ;
#36525 = CARTESIAN_POINT('Ctrl Pts',(-20.0143957853065,-3.71668696132871,
-5.93824202395825)) ;
#36526 = CARTESIAN_POINT('Ctrl Pts',(-20.2234612532234,-2.20947709836345,
-5.97696244300309)) ;
#36527 = CARTESIAN_POINT('Ctrl Pts',(-20.2790564039257,-1.62174353473886,
-5.99196018620084)) ;
#36528 = CARTESIAN_POINT('Ctrl Pts',(-20.3267009554494,-0.684518342453904,
-6.01538700183379)) ;
#36529 = CARTESIAN_POINT('Ctrl Pts',(-20.3354443265445,-0.336215972824135,
-6.02396830376446)) ;
#36530 = CARTESIAN_POINT('Ctrl Pts',(-20.3347696017134,0.794075410618914,
-6.05161225316834)) ;
#36531 = CARTESIAN_POINT('Ctrl Pts',(-20.2892024562884,1.57533590928818,-6.07044353448938)) ;
#36532 = CARTESIAN_POINT('Ctrl Pts',(-20.125404454939,2.98200010873307,-6.10492983665134)) ;
#36533 = CARTESIAN_POINT('Ctrl Pts',(-20.0226171098174,3.60818844230698,-6.12048853700425)) ;
#36534 = CARTESIAN_POINT('Ctrl Pts',(-19.6292478759167,5.45856606542675,-6.16752322739209)) ;
#36535 = CARTESIAN_POINT('Ctrl Pts',(-19.2542282705926,6.6616758845014,-6.1996678371757)) ;
#36536 = CARTESIAN_POINT('Ctrl Pts',(-18.61196560671,8.20284094613253,-6.24199141751562)) ;
#36537 = CARTESIAN_POINT('Ctrl Pts',(-18.4418872135962,8.57838358101396,-6.25238086663229)) ;
#36538 = CARTESIAN_POINT('Ctrl Pts',(-18.0609437410463,9.35574548362379,-6.27388110292608)) ;
#36539 = CARTESIAN_POINT('Ctrl Pts',(-17.847805435031,9.75620362594056,-6.28496129213293)) ;
#36540 = CARTESIAN_POINT('Ctrl Pts',(-17.2563467729632,10.7831180846691,-6.31378211727741)) ;
#36541 = CARTESIAN_POINT('Ctrl Pts',(-16.8572979835043,11.3968699716414,-6.33143517742053)) ;
#36542 = CARTESIAN_POINT('Ctrl Pts',(-16.0827391690205,12.4581955234338,-6.36353552931055)) ;
#36543 = CARTESIAN_POINT('Ctrl Pts',(-15.7193838906015,12.913639955258,-6.37788293923393)) ;
#36544 = CARTESIAN_POINT('Ctrl Pts',(-14.7405317272159,14.0379416997429,-6.41505324288756)) ;
#36545 = CARTESIAN_POINT('Ctrl Pts',(-14.0988491451116,14.6822854666767,-6.43811631393356)) ;
#36546 = CARTESIAN_POINT('Ctrl Pts',(-12.9467303015985,15.6937736613283,-6.47713198858411)) ;
#36547 = CARTESIAN_POINT('Ctrl Pts',(-12.458456000942,16.0841300303486,-6.49302121782243)) ;
#36548 = CARTESIAN_POINT('Ctrl Pts',(-11.6606791644631,16.6637659195397,-6.51761543908738)) ;
#36549 = CARTESIAN_POINT('Ctrl Pts',(-11.3627651222621,16.8683165221969,-6.52650274465454)) ;
#36550 = CARTESIAN_POINT('Ctrl Pts',(-10.3698062090231,17.5118444081389,-6.55541133735499)) ;
#36551 = CARTESIAN_POINT('Ctrl Pts',(-9.65358337859131,17.9166378537394,-6.5751955799527)) ;
#36552 = CARTESIAN_POINT('Ctrl Pts',(-8.37157240397254,18.541955280397,-6.60998648575256)) ;
#36553 = CARTESIAN_POINT('Ctrl Pts',(-7.81677440872748,18.7825812750195,-6.62484670724638)) ;
#36554 = CARTESIAN_POINT('Ctrl Pts',(-6.58903079019188,19.2512432320273,-6.65756666678475)) ;
#36555 = CARTESIAN_POINT('Ctrl Pts',(-5.91318352347607,19.4694616933211,-6.67548142331575)) ;
#36556 = CARTESIAN_POINT('Ctrl Pts',(-4.66227799181143,19.8021971452917,-6.7083763207331)) ;
#36557 = CARTESIAN_POINT('Ctrl Pts',(-4.09101684857812,19.9280563423746,-6.72329708712856)) ;
#36558 = CARTESIAN_POINT('Ctrl Pts',(-3.15345603968111,20.0925990500634,-6.747371142373)) ;
#36559 = CARTESIAN_POINT('Ctrl Pts',(-2.79012676745793,20.146265670974,-6.75659687764503)) ;
#36560 = CARTESIAN_POINT('Ctrl Pts',(-1.9877004539964,20.2426654098935,-6.77662748053633)) ;
#36561 = CARTESIAN_POINT('Ctrl Pts',(-1.54826285545236,20.2810094184567,-6.78739245042025)) ;
#36562 = CARTESIAN_POINT('Ctrl Pts',(-0.38714765283173,20.344364544381,-6.81566218836829)) ;
#36563 = CARTESIAN_POINT('Ctrl Pts',(0.335211131801346,20.3452865751508,-6.83308674848994)) ;
#36564 = CARTESIAN_POINT('Ctrl Pts',(1.63527276899067,20.2776781940589,-6.86489862269561)) ;
#36565 = CARTESIAN_POINT('Ctrl Pts',(2.21290108733795,20.2227943351447,-6.87919080054629)) ;
#36566 = CARTESIAN_POINT('Ctrl Pts',(3.47797413104281,20.0477360726295,-6.91104179026425)) ;
#36567 = CARTESIAN_POINT('Ctrl Pts',(4.16318287476264,19.9167246434693,-6.92866206780184)) ;
#36568 = CARTESIAN_POINT('Ctrl Pts',(5.38764960139512,19.6166459994107,-6.96071356446155)) ;
#36569 = CARTESIAN_POINT('Ctrl Pts',(5.92918512910822,19.459813287763,-6.9750900514938)) ;
#36570 = CARTESIAN_POINT('Ctrl Pts',(6.80629938240583,19.1657764570306,-6.99847733107374)) ;
#36571 = CARTESIAN_POINT('Ctrl Pts',(7.14597084944364,19.0417385068789,-7.00755602325346)) ;
#36572 = CARTESIAN_POINT('Ctrl Pts',(7.9061950747109,18.7409184964848,-7.02781200001761)) ;
#36573 = CARTESIAN_POINT('Ctrl Pts',(8.32447040222371,18.5589101101451,-7.03893602336652)) ;
#36574 = CARTESIAN_POINT('Ctrl Pts',(9.3780620912044,18.0576592430295,-7.06728932490813)) ;
#36575 = CARTESIAN_POINT('Ctrl Pts',(10.0034004445994,17.7188906304676,-7.08445150867794)) ;
#36576 = CARTESIAN_POINT('Ctrl Pts',(11.1021413708814,17.046924060357,-7.11593227583205)) ;
#36577 = CARTESIAN_POINT('Ctrl Pts',(11.5815164450668,16.7249404127619,-7.13016111803944)) ;
#36578 = CARTESIAN_POINT('Ctrl Pts',(12.7094391931464,15.8955706239743,-7.16508529626908)) ;
#36579 = CARTESIAN_POINT('Ctrl Pts',(13.3421363363681,15.3683566612708,-7.18594311988888)) ;
#36580 = CARTESIAN_POINT('Ctrl Pts',(14.4143475351795,14.3586581388065,-7.22342331023085)) ;
#36581 = CARTESIAN_POINT('Ctrl Pts',(14.8659146446333,13.8906107296394,-7.23998367067229)) ;
#36582 = CARTESIAN_POINT('Ctrl Pts',(15.510166803466,13.1553794517549,-7.26444036775844)) ;
#36583 = CARTESIAN_POINT('Ctrl Pts',(15.7200563570076,12.9038409519787,-7.27253713703068)) ;
#36584 = CARTESIAN_POINT('Ctrl Pts',(16.4219456576386,12.020118921661,-7.3002052098067)) ;
#36585 = CARTESIAN_POINT('Ctrl Pts',(16.8826186394949,11.3640115498233,-7.31948819747828)) ;
#36586 = CARTESIAN_POINT('Ctrl Pts',(17.6463459583452,10.1269282207857,-7.35486440420772)) ;
#36587 = CARTESIAN_POINT('Ctrl Pts',(17.9623464898602,9.5552236829556,-7.37086172866693)) ;
#36588 = CARTESIAN_POINT('Ctrl Pts',(18.5440448238941,8.371614000146,-7.40363032436401)) ;
#36589 = CARTESIAN_POINT('Ctrl Pts',(18.8082497509511,7.75984845441656,-7.42039169249166)) ;
#36590 = CARTESIAN_POINT('Ctrl Pts',(19.3308247553459,6.36543532668595,-7.45817300001808)) ;
#36591 = CARTESIAN_POINT('Ctrl Pts',(19.5726222530227,5.57781409248115,-7.47924057867345)) ;
#36592 = CARTESIAN_POINT('Ctrl Pts',(19.7993282149357,4.63990184905076,-7.50350100928927)) ;
#36593 = CARTESIAN_POINT('Ctrl Pts',(19.8311966017323,4.50174726995194,-7.50705295132518)) ;
#36594 = CARTESIAN_POINT('Ctrl Pts',(19.9399615148408,4.00664911744195,-7.51969236259956)) ;
#36595 = CARTESIAN_POINT('Ctrl Pts',(20.0086863129187,3.64798229709993,-7.52866996891407)) ;
#36596 = CARTESIAN_POINT('Ctrl Pts',(20.199868287735,2.48101672171897,-7.55755264345226)) ;
#36597 = CARTESIAN_POINT('Ctrl Pts',(20.2832635636153,1.66713831158843,-7.57722974781153)) ;
#36598 = CARTESIAN_POINT('Ctrl Pts',(20.3426798402346,0.247673027358125,-7.61188471003829)) ;
#36599 = CARTESIAN_POINT('Ctrl Pts',(20.3410735553585,-0.355925594235231,
-7.62671854096718)) ;
#36600 = CARTESIAN_POINT('Ctrl Pts',(20.2791764547102,-1.66758078837585,-7.65941473943478)) ;
#36601 = CARTESIAN_POINT('Ctrl Pts',(20.2086171861824,-2.3743630890629,-7.6773329384659)) ;
#36602 = CARTESIAN_POINT('Ctrl Pts',(20.0129875733312,-3.65277631698287,-7.71020049598997)) ;
#36603 = CARTESIAN_POINT('Ctrl Pts',(19.8999425410213,-4.22548623332871,-7.72509039010834)) ;
#36604 = CARTESIAN_POINT('Ctrl Pts',(19.6759621555885,-5.14908738348592,-7.74912554701932)) ;
#36605 = CARTESIAN_POINT('Ctrl Pts',(19.5798626614912,-5.50323287449455,-7.75834300526929)) ;
#36606 = CARTESIAN_POINT('Ctrl Pts',(19.3470476572957,-6.27765007180376,-7.77838462815951)) ;
#36607 = CARTESIAN_POINT('Ctrl Pts',(19.2061083955231,-6.69645792239567,-7.78916819527272)) ;
#36608 = CARTESIAN_POINT('Ctrl Pts',(18.7994464817941,-7.78607832377935,-7.81744195033205)) ;
#36609 = CARTESIAN_POINT('Ctrl Pts',(18.5114810466438,-8.44791532986397,-7.83485265313227)) ;
#36610 = CARTESIAN_POINT('Ctrl Pts',(18.1699267787802,-9.13113132033814,-7.85351834323284)) ;
#36611 = CARTESIAN_POINT('Ctrl Pts',(18.1507709233616,-9.16915006932015,-7.85455929226164)) ;
#36612 = CARTESIAN_POINT('Ctrl Pts',(18.1314964390739,-9.20710718616059,-7.85560087779543)) ;
#36613 = CARTESIAN_POINT('Origin',(0.,0.,5.8748638224677)) ;
#36614 = CARTESIAN_POINT('',(18.1314964616813,-9.20710714163998,-11.6687558734427)) ;
#36615 = CARTESIAN_POINT('',(18.1314964420815,-9.20710718023772,-11.0322347276753)) ;
#36616 = CARTESIAN_POINT('',(18.1314964405232,-9.20710718330643,5.8748638224677)) ;
#36617 = CARTESIAN_POINT('Ctrl Pts',(18.1314964616938,-9.20710714161542,-11.6687558745767)) ;
#36618 = CARTESIAN_POINT('Ctrl Pts',(18.2644739001709,-8.94523553328637,-11.6616247551653)) ;
#36619 = CARTESIAN_POINT('Ctrl Pts',(18.391785753033,-8.68046790628738,-11.6544792653389)) ;
#36620 = CARTESIAN_POINT('Ctrl Pts',(18.7543475034272,-7.88262674001481,-11.6330691624918)) ;
#36621 = CARTESIAN_POINT('Ctrl Pts',(18.9724551492615,-7.34215854648363,-11.6187174011085)) ;
#36622 = CARTESIAN_POINT('Ctrl Pts',(19.471581392229,-5.93384513506377,-11.5814618845947)) ;
#36623 = CARTESIAN_POINT('Ctrl Pts',(19.7179811697906,-5.0551151568954,-11.5583147733356)) ;
#36624 = CARTESIAN_POINT('Ctrl Pts',(20.0250982014908,-3.58663586093282,-11.5201361262327)) ;
#36625 = CARTESIAN_POINT('Ctrl Pts',(20.1205283548207,-3.00547161251361,-11.5051669123351)) ;
#36626 = CARTESIAN_POINT('Ctrl Pts',(20.2305155847466,-2.08819683527602,-11.4820760342017)) ;
#36627 = CARTESIAN_POINT('Ctrl Pts',(20.2621849322976,-1.75447676518937,-11.4738035306207)) ;
#36628 = CARTESIAN_POINT('Ctrl Pts',(20.3409804622817,-0.628929714393546,
-11.4461703104481)) ;
#36629 = CARTESIAN_POINT('Ctrl Pts',(20.3500339446608,0.164827882851609,-11.4270738833638)) ;
#36630 = CARTESIAN_POINT('Ctrl Pts',(20.2823537764486,1.60123956804531,-11.3920719691454)) ;
#36631 = CARTESIAN_POINT('Ctrl Pts',(20.2213791806036,2.24358135100497,-11.3762627454793)) ;
#36632 = CARTESIAN_POINT('Ctrl Pts',(19.9496333159388,4.14169546660323,-11.3286069890023)) ;
#36633 = CARTESIAN_POINT('Ctrl Pts',(19.651419904358,5.38173937783459,-11.2960738940596)) ;
#36634 = CARTESIAN_POINT('Ctrl Pts',(19.1067732956969,6.97284908097476,-11.2534486205041)) ;
#36635 = CARTESIAN_POINT('Ctrl Pts',(18.9626035307604,7.35588764401761,-11.2431363222837)) ;
#36636 = CARTESIAN_POINT('Ctrl Pts',(18.6320535515641,8.15966182634198,-11.2215538952151)) ;
#36637 = CARTESIAN_POINT('Ctrl Pts',(18.4427515604126,8.57895223271918,-11.2103208887694)) ;
#36638 = CARTESIAN_POINT('Ctrl Pts',(17.9179044953875,9.64361666003351,-11.181458000497)) ;
#36639 = CARTESIAN_POINT('Ctrl Pts',(17.5616689415133,10.2780556717329,-11.1639099260452)) ;
#36640 = CARTESIAN_POINT('Ctrl Pts',(16.8608830349276,11.3829028430115,-11.131942139304)) ;
#36641 = CARTESIAN_POINT('Ctrl Pts',(16.528643529125,11.860176595648,-11.1176201230084)) ;
#36642 = CARTESIAN_POINT('Ctrl Pts',(15.636803814885,13.030937675594,-11.0809191550807)) ;
#36643 = CARTESIAN_POINT('Ctrl Pts',(15.0512450284891,13.7031005982243,-11.0583171485039)) ;
#36644 = CARTESIAN_POINT('Ctrl Pts',(13.9984070067423,14.762462134288,-11.020307225313)) ;
#36645 = CARTESIAN_POINT('Ctrl Pts',(13.5544664991448,15.1710952507671,-11.0049643258568)) ;
#36646 = CARTESIAN_POINT('Ctrl Pts',(12.8382133778352,15.7738126559706,-10.9815614086281)) ;
#36647 = CARTESIAN_POINT('Ctrl Pts',(12.5781798297473,15.9819360770221,-10.9733388808027)) ;
#36648 = CARTESIAN_POINT('Ctrl Pts',(11.6802940609545,16.6650852530905,-10.9457000993399)) ;
#36649 = CARTESIAN_POINT('Ctrl Pts',(11.0197383572832,17.1090535624009,-10.9265544041125)) ;
#36650 = CARTESIAN_POINT('Ctrl Pts',(9.77772819691337,17.8419881207972,-10.8914546721904)) ;
#36651 = CARTESIAN_POINT('Ctrl Pts',(9.20520540511956,18.1439988032286,-10.8755968305895)) ;
#36652 = CARTESIAN_POINT('Ctrl Pts',(7.46415502869361,18.9587675303416,-10.8278252742946)) ;
#36653 = CARTESIAN_POINT('Ctrl Pts',(6.26075656118646,19.3894640284856,-10.7952218245531)) ;
#36654 = CARTESIAN_POINT('Ctrl Pts',(4.62903477404356,19.8055802561647,-10.7525417888207)) ;
#36655 = CARTESIAN_POINT('Ctrl Pts',(4.23011053522662,19.8946008433138,-10.7422433212736)) ;
#36656 = CARTESIAN_POINT('Ctrl Pts',(3.37587394598267,20.0583677539779,-10.720643854053)) ;
#36657 = CARTESIAN_POINT('Ctrl Pts',(2.92014939149677,20.1297634184969,-10.7093812246527)) ;
#36658 = CARTESIAN_POINT('Ctrl Pts',(1.74149529091752,20.273544401591,-10.6805098312542)) ;
#36659 = CARTESIAN_POINT('Ctrl Pts',(1.01640818719418,20.3228030401721,-10.662981794902)) ;
#36660 = CARTESIAN_POINT('Ctrl Pts',(-0.2907517079791,20.3414619205923,-10.6310393061773)) ;
#36661 = CARTESIAN_POINT('Ctrl Pts',(-0.871830604109229,20.3248496419359,
-10.6167221336598)) ;
#36662 = CARTESIAN_POINT('Ctrl Pts',(-2.33631900803327,20.2200568250381,-10.5801083433041)) ;
#36663 = CARTESIAN_POINT('Ctrl Pts',(-3.21614306287666,20.0988925386872,-10.5575917884417)) ;
#36664 = CARTESIAN_POINT('Ctrl Pts',(-4.69316381036904,19.79599277279,-10.5192202809965)) ;
#36665 = CARTESIAN_POINT('Ctrl Pts',(-5.29507781997509,19.6435555360137,-10.5034304755838)) ;
#36666 = CARTESIAN_POINT('Ctrl Pts',(-6.21642563714968,19.3647877362269,-10.4793874238207)) ;
#36667 = CARTESIAN_POINT('Ctrl Pts',(-6.54122155327408,19.2575017170481,-10.470955337764)) ;
#36668 = CARTESIAN_POINT('Ctrl Pts',(-7.6040364769991,18.8764424028527,-10.4433245169478)) ;
#36669 = CARTESIAN_POINT('Ctrl Pts',(-8.32887114586476,18.5680199236532,-10.42437196776)) ;
#36670 = CARTESIAN_POINT('Ctrl Pts',(-9.60648786267476,17.9344835961022,-10.389651975235)) ;
#36671 = CARTESIAN_POINT('Ctrl Pts',(-10.1652682088097,17.6237800621291,-10.373980887929)) ;
#36672 = CARTESIAN_POINT('Ctrl Pts',(-11.7834581811822,16.6214036752975,-10.326662299053)) ;
#36673 = CARTESIAN_POINT('Ctrl Pts',(-12.7939709280014,15.8567073858111,-10.2943377863863)) ;
#36674 = CARTESIAN_POINT('Ctrl Pts',(-14.0299467657592,14.7258722452353,-10.2518746451638)) ;
#36675 = CARTESIAN_POINT('Ctrl Pts',(-14.3245421419475,14.4394673595353,-10.2415210919698)) ;
#36676 = CARTESIAN_POINT('Ctrl Pts',(-14.927704807478,13.816435948504,-10.2199852021186)) ;
#36677 = CARTESIAN_POINT('Ctrl Pts',(-15.2340207895599,13.4779408469831,-10.2088364118082)) ;
#36678 = CARTESIAN_POINT('Ctrl Pts',(-15.9997083995505,12.5723318606258,-10.1799970917707)) ;
#36679 = CARTESIAN_POINT('Ctrl Pts',(-16.440407115086,11.9902965739383,-10.1623915064785)) ;
#36680 = CARTESIAN_POINT('Ctrl Pts',(-17.174666673047,10.9037323775427,-10.1303511097546)) ;
#36681 = CARTESIAN_POINT('Ctrl Pts',(-17.4796130868513,10.4078659365241,-10.1160151906014)) ;
#36682 = CARTESIAN_POINT('Ctrl Pts',(-18.2010772685386,9.11334243900613,-10.0790607033173)) ;
#36683 = CARTESIAN_POINT('Ctrl Pts',(-18.5865874435017,8.29885312023002,-10.0562099047307)) ;
#36684 = CARTESIAN_POINT('Ctrl Pts',(-19.0792013177351,7.04995072791319,-10.0220436999903)) ;
#36685 = CARTESIAN_POINT('Ctrl Pts',(-19.2280650107008,6.6331927567273,-10.0107900395202)) ;
#36686 = CARTESIAN_POINT('Ctrl Pts',(-19.4637722789977,5.89846700872934,-9.99134313324307)) ;
#36687 = CARTESIAN_POINT('Ctrl Pts',(-19.5567033174411,5.58262526534466,-9.98311377696789)) ;
#36688 = CARTESIAN_POINT('Ctrl Pts',(-19.8060872175668,4.65219891399434,-9.95931814270051)) ;
#36689 = CARTESIAN_POINT('Ctrl Pts',(-19.9415120356514,4.03238819383098,-9.94396128563841)) ;
#36690 = CARTESIAN_POINT('Ctrl Pts',(-20.1893981051791,2.57386814890178,-9.90808249181154)) ;
#36691 = CARTESIAN_POINT('Ctrl Pts',(-20.2789340505529,1.73245925534119,-9.88755883477629)) ;
#36692 = CARTESIAN_POINT('Ctrl Pts',(-20.341103048006,0.310028945555236,-9.85233272823169)) ;
#36693 = CARTESIAN_POINT('Ctrl Pts',(-20.341691015884,-0.268680190415014,
-9.83786436388446)) ;
#36694 = CARTESIAN_POINT('Ctrl Pts',(-20.2878109996761,-1.5617167766763,-9.80518880033128)) ;
#36695 = CARTESIAN_POINT('Ctrl Pts',(-20.2202816950277,-2.27473849227552,
-9.78692492533925)) ;
#36696 = CARTESIAN_POINT('Ctrl Pts',(-20.0494162186243,-3.42705074382047,
-9.75733344824936)) ;
#36697 = CARTESIAN_POINT('Ctrl Pts',(-19.9688233781693,-3.86909093217934,
-9.74596878888194)) ;
#36698 = CARTESIAN_POINT('Ctrl Pts',(-19.7965447233957,-4.66382796933867,
-9.72569073895414)) ;
#36699 = CARTESIAN_POINT('Ctrl Pts',(-19.7098949742089,-5.01742113284066,
-9.71674004681931)) ;
#36700 = CARTESIAN_POINT('Ctrl Pts',(-19.4626251649724,-5.92082112187331,
-9.69386137694853)) ;
#36701 = CARTESIAN_POINT('Ctrl Pts',(-19.2881857050826,-6.46651350902452,
-9.68002158856314)) ;
#36702 = CARTESIAN_POINT('Ctrl Pts',(-18.8557880747323,-7.64508921402875,
-9.64954447393179)) ;
#36703 = CARTESIAN_POINT('Ctrl Pts',(-18.5884971782981,-8.27380786498699,
-9.6328941190496)) ;
#36704 = CARTESIAN_POINT('Ctrl Pts',(-18.0367165696884,-9.40929921359298,
-9.60165612086801)) ;
#36705 = CARTESIAN_POINT('Ctrl Pts',(-17.7611625135032,-9.91963475623672,
-9.58715408442755)) ;
#36706 = CARTESIAN_POINT('Ctrl Pts',(-17.0949133576442,-11.0365536664555,
-9.55431360555433)) ;
#36707 = CARTESIAN_POINT('Ctrl Pts',(-16.6929876720756,-11.6355375762919,
-9.53591652660456)) ;
#36708 = CARTESIAN_POINT('Ctrl Pts',(-15.9944720974617,-12.5656084408824,
-9.50637440803287)) ;
#36709 = CARTESIAN_POINT('Ctrl Pts',(-15.7173605405647,-12.9105474296837,
-9.49518663648372)) ;
#36710 = CARTESIAN_POINT('Ctrl Pts',(-15.1903875197806,-13.5243685608157,
-9.47501654108906)) ;
#36711 = CARTESIAN_POINT('Ctrl Pts',(-14.9440750967618,-13.7960515355945,
-9.46600279388126)) ;
#36712 = CARTESIAN_POINT('Ctrl Pts',(-14.2877067459067,-14.48181100612,-9.44282006096143)) ;
#36713 = CARTESIAN_POINT('Ctrl Pts',(-13.866958795232,-14.8851896720789,-9.42874228551097)) ;
#36714 = CARTESIAN_POINT('Ctrl Pts',(-12.8964473607371,-15.7387261769407,
-9.39735968761845)) ;
#36715 = CARTESIAN_POINT('Ctrl Pts',(-12.3392466279428,-16.1792718713767,
-9.38003526662975)) ;
#36716 = CARTESIAN_POINT('Ctrl Pts',(-11.2686649084898,-16.9381855459576,
-9.34751320716504)) ;
#36717 = CARTESIAN_POINT('Ctrl Pts',(-10.7619369014238,-17.2645776899066,
-9.33241039137698)) ;
#36718 = CARTESIAN_POINT('Ctrl Pts',(-9.53826119513563,-17.977934220112,-9.29658075444099)) ;
#36719 = CARTESIAN_POINT('Ctrl Pts',(-8.81107458198392,-18.3452855796188,
-9.27575844311755)) ;
#36720 = CARTESIAN_POINT('Ctrl Pts',(-7.72593619808643,-18.814020699806,-9.24586181420824)) ;
#36721 = CARTESIAN_POINT('Ctrl Pts',(-7.38413331996738,-18.950779573039,-9.23661335380016)) ;
#36722 = CARTESIAN_POINT('Ctrl Pts',(-6.90643315141013,-19.1270247024386,
-9.22399311644376)) ;
#36723 = CARTESIAN_POINT('Ctrl Pts',(-6.77355780482382,-19.1744832450379,
-9.22051295894036)) ;
#36724 = CARTESIAN_POINT('Ctrl Pts',(-5.86184569907663,-19.4894559273203,
-9.19680703527173)) ;
#36725 = CARTESIAN_POINT('Ctrl Pts',(-5.06787299617498,-19.7108296906015,
-9.17698849863006)) ;
#36726 = CARTESIAN_POINT('Ctrl Pts',(-3.60983258549382,-20.0234081213887,
-9.14072306887849)) ;
#36727 = CARTESIAN_POINT('Ctrl Pts',(-2.95050835202995,-20.1311265055259,
-9.12437621116661)) ;
#36728 = CARTESIAN_POINT('Ctrl Pts',(-1.63982801643752,-20.2794787868767,
-9.09161677954966)) ;
#36729 = CARTESIAN_POINT('Ctrl Pts',(-0.989429106004565,-20.3215972276946,
-9.0752350353492)) ;
#36730 = CARTESIAN_POINT('Ctrl Pts',(0.461336783687866,-20.3457241267949,
-9.03844123722084)) ;
#36731 = CARTESIAN_POINT('Ctrl Pts',(1.26089775150676,-20.3118550747804,-9.01798257693822)) ;
#36732 = CARTESIAN_POINT('Ctrl Pts',(2.38350328160935,-20.1977476850636,-8.98954519437575)) ;
#36733 = CARTESIAN_POINT('Ctrl Pts',(2.70977206246689,-20.156568157791,-8.98132578441109)) ;
#36734 = CARTESIAN_POINT('Ctrl Pts',(3.66532035197343,-20.0123434835586,-8.95745472300499)) ;
#36735 = CARTESIAN_POINT('Ctrl Pts',(4.29091813027024,-19.8875965850159,-8.94201562076869)) ;
#36736 = CARTESIAN_POINT('Ctrl Pts',(5.72513655220656,-19.5307712539944,-8.90617302810925)) ;
#36737 = CARTESIAN_POINT('Ctrl Pts',(6.52728271107211,-19.2775201460758,-8.88576762481878)) ;
#36738 = CARTESIAN_POINT('Ctrl Pts',(7.85095262762428,-18.7674932266274,-8.85067246468831)) ;
#36739 = CARTESIAN_POINT('Ctrl Pts',(8.38133805824009,-18.5367047452253,-8.83621174535561)) ;
#36740 = CARTESIAN_POINT('Ctrl Pts',(9.54362907206953,-17.9708575065631,-8.80357360389728)) ;
#36741 = CARTESIAN_POINT('Ctrl Pts',(10.1691599024166,-17.6244362989125,-8.78533994997957)) ;
#36742 = CARTESIAN_POINT('Ctrl Pts',(11.1574434898248,-17.006958540734,-8.75573684021118)) ;
#36743 = CARTESIAN_POINT('Ctrl Pts',(11.5316890688778,-16.7554568878551,-8.74433158094691)) ;
#36744 = CARTESIAN_POINT('Ctrl Pts',(12.1919900283931,-16.2791102680347,-8.72402802510731)) ;
#36745 = CARTESIAN_POINT('Ctrl Pts',(12.4809596929103,-16.0586331143493,-8.71509108914202)) ;
#36746 = CARTESIAN_POINT('Ctrl Pts',(13.2079663950725,-15.4724609853883,-8.6922785529023)) ;
#36747 = CARTESIAN_POINT('Ctrl Pts',(13.6368036721768,-15.0958608406856,-8.67849048156248)) ;
#36748 = CARTESIAN_POINT('Ctrl Pts',(14.5457142325556,-14.2272893979939,-8.64797083023692)) ;
#36749 = CARTESIAN_POINT('Ctrl Pts',(15.0178340127291,-13.7280085420308,-8.6312250250989)) ;
#36750 = CARTESIAN_POINT('Ctrl Pts',(15.8404540417171,-12.7647335753372,-8.59988057389655)) ;
#36751 = CARTESIAN_POINT('Ctrl Pts',(16.1980747562379,-12.3077525526816,-8.58537048257343)) ;
#36752 = CARTESIAN_POINT('Ctrl Pts',(16.9559401947958,-11.2489749761785,-8.55249052851208)) ;
#36753 = CARTESIAN_POINT('Ctrl Pts',(17.3446396883675,-10.6398690101613,-8.53406155890164)) ;
#36754 = CARTESIAN_POINT('Ctrl Pts',(17.849916193536,-9.74654099798349,-8.5079960712815)) ;
#36755 = CARTESIAN_POINT('Ctrl Pts',(17.9937452640463,-9.4783796817226,-8.50029148886646)) ;
#36756 = CARTESIAN_POINT('Ctrl Pts',(18.131496444736,-9.20710717501038,-8.49264489791374)) ;
#36757 = CARTESIAN_POINT('Ctrl Pts',(18.1314964390739,-9.20710718616059,-7.85560087779543)) ;
#36758 = CARTESIAN_POINT('Ctrl Pts',(17.8882630500469,-9.68610512089045,-7.86874511426699)) ;
#36759 = CARTESIAN_POINT('Ctrl Pts',(17.6261380674114,-10.155287974147,-7.88199762182294)) ;
#36760 = CARTESIAN_POINT('Ctrl Pts',(16.8927925656504,-11.353795088599,-7.91703979929467)) ;
#36761 = CARTESIAN_POINT('Ctrl Pts',(16.3929324675541,-12.0642796468869,-7.93905694544084)) ;
#36762 = CARTESIAN_POINT('Ctrl Pts',(15.4616803202276,-13.2227469724641,-7.97688440688327)) ;
#36763 = CARTESIAN_POINT('Ctrl Pts',(15.0523404040361,-13.6869153000442,-7.9926288318601)) ;
#36764 = CARTESIAN_POINT('Ctrl Pts',(14.392468270309,-14.3697039890772,-8.01637363824206)) ;
#36765 = CARTESIAN_POINT('Ctrl Pts',(14.1566830725011,-14.6020498649752,-8.02454904267831)) ;
#36766 = CARTESIAN_POINT('Ctrl Pts',(13.3339607992616,-15.3741049928171,-8.05219587890495)) ;
#36767 = CARTESIAN_POINT('Ctrl Pts',(12.721009972887,-15.8850096636789,-8.07139047604844)) ;
#36768 = CARTESIAN_POINT('Ctrl Pts',(11.5575522247841,-16.7441389836427,-8.10658802442379)) ;
#36769 = CARTESIAN_POINT('Ctrl Pts',(11.0173028737393,-17.104450631235,-8.12249486882939)) ;
#36770 = CARTESIAN_POINT('Ctrl Pts',(9.88574650823828,-17.7832396516569,-8.15528524128576)) ;
#36771 = CARTESIAN_POINT('Ctrl Pts',(9.29403528847779,-18.0995163386267,-8.17216480123747)) ;
#36772 = CARTESIAN_POINT('Ctrl Pts',(8.10296931623272,-18.6623216988528,-8.20559292514709)) ;
#36773 = CARTESIAN_POINT('Ctrl Pts',(7.505299583517,-18.9106012583172,-8.2221112926014)) ;
#36774 = CARTESIAN_POINT('Ctrl Pts',(6.53628245870715,-19.2599552824999,-8.24818725338983)) ;
#36775 = CARTESIAN_POINT('Ctrl Pts',(6.17214191829832,-19.3797197136801,-8.25782913399017)) ;
#36776 = CARTESIAN_POINT('Ctrl Pts',(5.3010425589228,-19.6391764789149,-8.28037563349866)) ;
#36777 = CARTESIAN_POINT('Ctrl Pts',(4.7916210027444,-19.7696403915504,-8.29317666213022)) ;
#36778 = CARTESIAN_POINT('Ctrl Pts',(3.72434227071597,-19.9992914861906,-8.31968347802475)) ;
#36779 = CARTESIAN_POINT('Ctrl Pts',(3.166239957531,-20.0952061271093,-8.33337343160315)) ;
#36780 = CARTESIAN_POINT('Ctrl Pts',(1.99943603469413,-20.245910715939,-8.36205869249268)) ;
#36781 = CARTESIAN_POINT('Ctrl Pts',(1.39079739999137,-20.2968056351824,-8.37705966539734)) ;
#36782 = CARTESIAN_POINT('Ctrl Pts',(0.0731679175983439,-20.3474349678555,
-8.40987972686049)) ;
#36783 = CARTESIAN_POINT('Ctrl Pts',(-0.635392167642173,-20.3376430638463,
-8.42774866955298)) ;
#36784 = CARTESIAN_POINT('Ctrl Pts',(-1.9322415329278,-20.2518727712336,-8.4607730069592)) ;
#36785 = CARTESIAN_POINT('Ctrl Pts',(-2.52050965974613,-20.1870983445915,
-8.47587010111979)) ;
#36786 = CARTESIAN_POINT('Ctrl Pts',(-3.4698024662583,-20.0404248556819,-8.50016618382197)) ;
#36787 = CARTESIAN_POINT('Ctrl Pts',(-3.83289241839446,-19.9741607969628,
-8.50943903624526)) ;
#36788 = CARTESIAN_POINT('Ctrl Pts',(-4.62128767800484,-19.8079879854046,
-8.52941035018297)) ;
#36789 = CARTESIAN_POINT('Ctrl Pts',(-5.04558441927441,-19.7041815486263,
-8.54007279093563)) ;
#36790 = CARTESIAN_POINT('Ctrl Pts',(-6.16463724853136,-19.3918803534568,
-8.56832103602392)) ;
#36791 = CARTESIAN_POINT('Ctrl Pts',(-6.85213693819959,-19.1597493700807,
-8.58582255801348)) ;
#36792 = CARTESIAN_POINT('Ctrl Pts',(-8.06530669699869,-18.6764588466243,
-8.61773158692266)) ;
#36793 = CARTESIAN_POINT('Ctrl Pts',(-8.59538714632041,-18.4385085873238,
-8.63204236425467)) ;
#36794 = CARTESIAN_POINT('Ctrl Pts',(-9.90371777134193,-17.7825113919991,
-8.66854091206945)) ;
#36795 = CARTESIAN_POINT('Ctrl Pts',(-10.666273023241,-17.3358567790004,-8.69094452336418)) ;
#36796 = CARTESIAN_POINT('Ctrl Pts',(-11.9295889440631,-16.4808941328367,
-8.72976584349847)) ;
#36797 = CARTESIAN_POINT('Ctrl Pts',(-12.4444299033452,-16.0956868694347,
-8.74611852443698)) ;
#36798 = CARTESIAN_POINT('Ctrl Pts',(-13.2156213361805,-15.4595228040943,
-8.77105907575097)) ;
#36799 = CARTESIAN_POINT('Ctrl Pts',(-13.4850431837754,-15.2250813845003,
-8.77984625120089)) ;
#36800 = CARTESIAN_POINT('Ctrl Pts',(-14.3577672892834,-14.4243199046883,
-8.80879282232597)) ;
#36801 = CARTESIAN_POINT('Ctrl Pts',(-14.9326795648082,-13.8282889946704,
-8.82870442177622)) ;
#36802 = CARTESIAN_POINT('Ctrl Pts',(-15.8628051567735,-12.7381410546666,
-8.86365451420733)) ;
#36803 = CARTESIAN_POINT('Ctrl Pts',(-16.2351418589337,-12.2600564898606,
-8.87854358941128)) ;
#36804 = CARTESIAN_POINT('Ctrl Pts',(-16.9961301333448,-11.1873590729252,
-8.91128766448158)) ;
#36805 = CARTESIAN_POINT('Ctrl Pts',(-17.3761038082093,-10.5875608263402,
-8.92919673598262)) ;
#36806 = CARTESIAN_POINT('Ctrl Pts',(-18.0112429628168,-9.4583585864117,-8.96212037160191)) ;
#36807 = CARTESIAN_POINT('Ctrl Pts',(-18.2763251760578,-8.93539919819827,
-8.97707569962068)) ;
#36808 = CARTESIAN_POINT('Ctrl Pts',(-18.6703109372152,-8.06700520554083,
-9.00119329305808)) ;
#36809 = CARTESIAN_POINT('Ctrl Pts',(-18.813069633418,-7.72822752835531,-9.01042828487)) ;
#36810 = CARTESIAN_POINT('Ctrl Pts',(-19.1064229585065,-6.97569337953957,
-9.03044678180629)) ;
#36811 = CARTESIAN_POINT('Ctrl Pts',(-19.2529225977215,-6.56053905774759,
-9.04119116502603)) ;
#36812 = CARTESIAN_POINT('Ctrl Pts',(-19.6040212792152,-5.45218706636591,
-9.06945649809231)) ;
#36813 = CARTESIAN_POINT('Ctrl Pts',(-19.785343815118,-4.75227993549421,-9.08689643411367)) ;
#36814 = CARTESIAN_POINT('Ctrl Pts',(-20.0444073099992,-3.47566867337971,
-9.11872771758462)) ;
#36815 = CARTESIAN_POINT('Ctrl Pts',(-20.1353988861546,-2.90245427197672,
-9.13302361087297)) ;
#36816 = CARTESIAN_POINT('Ctrl Pts',(-20.2809206309282,-1.63864521514933,
-9.16475027109484)) ;
#36817 = CARTESIAN_POINT('Ctrl Pts',(-20.3249356444628,-0.947564026151293,
-9.18223878548889)) ;
#36818 = CARTESIAN_POINT('Ctrl Pts',(-20.3407620441901,0.311505017826325,
-9.21424923645223)) ;
#36819 = CARTESIAN_POINT('Ctrl Pts',(-20.3241631270323,0.87865239574256,-9.22871833912442)) ;
#36820 = CARTESIAN_POINT('Ctrl Pts',(-20.2581321205381,1.80595751199905,-9.25222262260541)) ;
#36821 = CARTESIAN_POINT('Ctrl Pts',(-20.2227191460455,2.1668032112663,-9.26132649509985)) ;
#36822 = CARTESIAN_POINT('Ctrl Pts',(-20.1213641475515,2.97626209251346,-9.28153918339051)) ;
#36823 = CARTESIAN_POINT('Ctrl Pts',(-20.0500280028594,3.42400547827348,-9.29259717550828)) ;
#36824 = CARTESIAN_POINT('Ctrl Pts',(-19.8281845624787,4.56870547157898,-9.32093419742774)) ;
#36825 = CARTESIAN_POINT('Ctrl Pts',(-19.65588745088,5.26080422166608,-9.33814385087967)) ;
#36826 = CARTESIAN_POINT('Ctrl Pts',(-19.2787896693064,6.49492165951928,-9.36968450652277)) ;
#36827 = CARTESIAN_POINT('Ctrl Pts',(-19.0865023884051,7.039968542636,-9.38392479558484)) ;
#36828 = CARTESIAN_POINT('Ctrl Pts',(-18.5165439765595,8.45967814926106,-9.42208579428037)) ;
#36829 = CARTESIAN_POINT('Ctrl Pts',(-18.1001983586443,9.31726041477277,-9.44629458698304)) ;
#36830 = CARTESIAN_POINT('Ctrl Pts',(-17.4213223148545,10.4969895559092,-9.48092347259129)) ;
#36831 = CARTESIAN_POINT('Ctrl Pts',(-17.2066824248624,10.8452451730826,-9.49131344937297)) ;
#36832 = CARTESIAN_POINT('Ctrl Pts',(-16.9009117351543,11.3094088237495,-9.50530414680677)) ;
#36833 = CARTESIAN_POINT('Ctrl Pts',(-16.8188109755505,11.4311479306215,-9.50898713664741)) ;
#36834 = CARTESIAN_POINT('Ctrl Pts',(-16.5378009552827,11.8382479874688,-9.52133641073563)) ;
#36835 = CARTESIAN_POINT('Ctrl Pts',(-16.3328911758984,12.1193911449966,-9.52990549974328)) ;
#36836 = CARTESIAN_POINT('Ctrl Pts',(-15.6440036891357,13.0153444164916,-9.55754793652415)) ;
#36837 = CARTESIAN_POINT('Ctrl Pts',(-15.1317416105862,13.6075143443474,-9.57638876339137)) ;
#36838 = CARTESIAN_POINT('Ctrl Pts',(-14.1444780986719,14.6238995865002,-9.61089334243074)) ;
#36839 = CARTESIAN_POINT('Ctrl Pts',(-13.6812563590108,15.0581511105426,-9.62646076785511)) ;
#36840 = CARTESIAN_POINT('Ctrl Pts',(-12.2414192402371,16.286570208368,-9.67351781771797)) ;
#36841 = CARTESIAN_POINT('Ctrl Pts',(-11.2106400565273,17.0125300812806,-9.70567673375053)) ;
#36842 = CARTESIAN_POINT('Ctrl Pts',(-9.76202827405727,17.8436144297636,-9.74801140413763)) ;
#36843 = CARTESIAN_POINT('Ctrl Pts',(-9.39846678293497,18.0377548382297,-9.75839798939039)) ;
#36844 = CARTESIAN_POINT('Ctrl Pts',(-8.62269824640536,18.4221860797962,-9.77990093242946)) ;
#36845 = CARTESIAN_POINT('Ctrl Pts',(-8.20950819024049,18.6099931744824,-9.79098646168336)) ;
#36846 = CARTESIAN_POINT('Ctrl Pts',(-7.11479442787982,19.0640134639661,-9.819808705586)) ;
#36847 = CARTESIAN_POINT('Ctrl Pts',(-6.42458537360321,19.3075532564698,-9.83745805170337)) ;
#36848 = CARTESIAN_POINT('Ctrl Pts',(-5.16396854351254,19.6772589158637,-9.8695537141949)) ;
#36849 = CARTESIAN_POINT('Ctrl Pts',(-4.59840029468319,19.8170582127219,-9.88390022624317)) ;
#36850 = CARTESIAN_POINT('Ctrl Pts',(-3.13790738370902,20.1121711054945,-9.92105328838455)) ;
#36851 = CARTESIAN_POINT('Ctrl Pts',(-2.23716577128077,20.2321760983763,-9.94409937575324)) ;
#36852 = CARTESIAN_POINT('Ctrl Pts',(-0.893628586157868,20.3203325810586,
-9.97836380789294)) ;
#36853 = CARTESIAN_POINT('Ctrl Pts',(-0.455002842144645,20.3348829031922,
-9.98952252649341)) ;
#36854 = CARTESIAN_POINT('Ctrl Pts',(0.312038583452749,20.3354958401899,-10.0088518552467)) ;
#36855 = CARTESIAN_POINT('Ctrl Pts',(0.640287622543884,20.3278084393698,-10.0170574121269)) ;
#36856 = CARTESIAN_POINT('Ctrl Pts',(1.61005161874381,20.2815831365506,-10.0410377290103)) ;
#36857 = CARTESIAN_POINT('Ctrl Pts',(2.25008566363119,20.2205837399273,-10.0565954211858)) ;
#36858 = CARTESIAN_POINT('Ctrl Pts',(3.710976709445,20.0111206217978,-10.092387039232)) ;
#36859 = CARTESIAN_POINT('Ctrl Pts',(4.52774025422039,19.8422743960425,-10.112622977512)) ;
#36860 = CARTESIAN_POINT('Ctrl Pts',(5.88938842104761,19.4723112323457,-10.1475309433996)) ;
#36861 = CARTESIAN_POINT('Ctrl Pts',(6.44022823999945,19.2971306732805,-10.161981094038)) ;
#36862 = CARTESIAN_POINT('Ctrl Pts',(7.65245535823624,18.8539176608413,-10.194567462467)) ;
#36863 = CARTESIAN_POINT('Ctrl Pts',(8.30871451488158,18.5740555581093,-10.2127592979663)) ;
#36864 = CARTESIAN_POINT('Ctrl Pts',(9.35565962503226,18.0609743923566,-10.2423787910021)) ;
#36865 = CARTESIAN_POINT('Ctrl Pts',(9.75563420448104,17.8481026608384,-10.2538405372012)) ;
#36866 = CARTESIAN_POINT('Ctrl Pts',(10.4624052872712,17.4410881150172,-10.2741800335069)) ;
#36867 = CARTESIAN_POINT('Ctrl Pts',(10.7717467628711,17.251752115875,-10.2830982771922)) ;
#36868 = CARTESIAN_POINT('Ctrl Pts',(11.5518246233472,16.7451314666697,-10.3058210329773)) ;
#36869 = CARTESIAN_POINT('Ctrl Pts',(12.0146412124843,16.4162261242857,-10.3195389147573)) ;
#36870 = CARTESIAN_POINT('Ctrl Pts',(13.0094560927125,15.6446199438071,-10.3501003655355)) ;
#36871 = CARTESIAN_POINT('Ctrl Pts',(13.5338446630016,15.1932590429419,-10.3669595559333)) ;
#36872 = CARTESIAN_POINT('Ctrl Pts',(14.4540468431467,14.3156931744071,-10.3984241293179)) ;
#36873 = CARTESIAN_POINT('Ctrl Pts',(14.8565455233173,13.8975389017678,-10.4129372843635)) ;
#36874 = CARTESIAN_POINT('Ctrl Pts',(15.7189478185064,12.9212497599537,-10.4458322055585)) ;
#36875 = CARTESIAN_POINT('Ctrl Pts',(16.1680825384402,12.3546394313075,-10.4642732566595)) ;
#36876 = CARTESIAN_POINT('Ctrl Pts',(16.8407381506725,11.406367521265,-10.4937997989432)) ;
#36877 = CARTESIAN_POINT('Ctrl Pts',(17.0836521290077,11.0392262191932,-10.5049299472697)) ;
#36878 = CARTESIAN_POINT('Ctrl Pts',(17.5072273679419,10.351525566645,-10.525066114738)) ;
#36879 = CARTESIAN_POINT('Ctrl Pts',(17.6914714713784,10.0333907221002,-10.5341016220387)) ;
#36880 = CARTESIAN_POINT('Ctrl Pts',(18.1468451329918,9.19551315903772,-10.5573896433154)) ;
#36881 = CARTESIAN_POINT('Ctrl Pts',(18.4043082986069,8.6687306066441,-10.5715499068541)) ;
#36882 = CARTESIAN_POINT('Ctrl Pts',(18.9223882860589,7.48122025175797,-10.6030113120323)) ;
#36883 = CARTESIAN_POINT('Ctrl Pts',(19.1718821335937,6.81647707442332,-10.6203316499522)) ;
#36884 = CARTESIAN_POINT('Ctrl Pts',(19.5690055468501,5.56263222914312,-10.6529326694459)) ;
#36885 = CARTESIAN_POINT('Ctrl Pts',(19.7259997231188,4.97732663842603,-10.6681206536517)) ;
#36886 = CARTESIAN_POINT('Ctrl Pts',(20.0347610418548,3.57944455740328,-10.7043410416274)) ;
#36887 = CARTESIAN_POINT('Ctrl Pts',(20.1635925341505,2.7628974755857,-10.7254734698459)) ;
#36888 = CARTESIAN_POINT('Ctrl Pts',(20.2765593789294,1.58465221010846,-10.7553893357962)) ;
#36889 = CARTESIAN_POINT('Ctrl Pts',(20.3013005026288,1.22767544682827,-10.7643697752945)) ;
#36890 = CARTESIAN_POINT('Ctrl Pts',(20.3418306564613,0.281445753206663,-10.7878287519677)) ;
#36891 = CARTESIAN_POINT('Ctrl Pts',(20.3414437677678,-0.308158963865643,
-10.8021384712817)) ;
#36892 = CARTESIAN_POINT('Ctrl Pts',(20.2737845864534,-1.84066206873555,-10.8393508987583)) ;
#36893 = CARTESIAN_POINT('Ctrl Pts',(20.166408049051,-2.78035121329638,-10.8622289185661)) ;
#36894 = CARTESIAN_POINT('Ctrl Pts',(19.8874994093046,-4.2837976432321,-10.9000789076202)) ;
#36895 = CARTESIAN_POINT('Ctrl Pts',(19.7561750138368,-4.85356516943185,-10.9147063704701)) ;
#36896 = CARTESIAN_POINT('Ctrl Pts',(19.403387817664,-6.13009396921374,-10.948162918131)) ;
#36897 = CARTESIAN_POINT('Ctrl Pts',(19.1674998270474,-6.83201681768048,-10.9670580286776)) ;
#36898 = CARTESIAN_POINT('Ctrl Pts',(18.7415600003681,-7.90225327399103,-10.9962932662791)) ;
#36899 = CARTESIAN_POINT('Ctrl Pts',(18.5776393121558,-8.28027772460641,-11.0067007695699)) ;
#36900 = CARTESIAN_POINT('Ctrl Pts',(18.3148670791874,-8.83911176884274,-11.0220934427904)) ;
#36901 = CARTESIAN_POINT('Ctrl Pts',(18.2245720180128,-9.02381405227549,-11.0271783889829)) ;
#36902 = CARTESIAN_POINT('Ctrl Pts',(18.1314964436398,-9.20710717716895,-11.0322347276753)) ;
#36903 = CARTESIAN_POINT('Origin',(0.,0.,5.8748638224677)) ;
#36904 = CARTESIAN_POINT('',(18.1314964553944,-9.20710715402079,-14.8444016786038)) ;
#36905 = CARTESIAN_POINT('',(18.1314964185968,-9.20710722648607,-14.2060611031549)) ;
#36906 = CARTESIAN_POINT('',(18.1314964405232,-9.20710718330643,5.8748638224677)) ;
#36907 = CARTESIAN_POINT('Ctrl Pts',(18.1314964554037,-9.20710715400241,-14.8444016794283)) ;
#36908 = CARTESIAN_POINT('Ctrl Pts',(18.3793175840612,-8.71907461124281,-14.8306536571053)) ;
#36909 = CARTESIAN_POINT('Ctrl Pts',(18.6073666963369,-8.22117033262147,-14.816774955725)) ;
#36910 = CARTESIAN_POINT('Ctrl Pts',(19.0167898114644,-7.22263228758697,-14.7893236747267)) ;
#36911 = CARTESIAN_POINT('Ctrl Pts',(19.1991357427948,-6.722938352433,-14.775766890081)) ;
#36912 = CARTESIAN_POINT('Ctrl Pts',(19.4695729787702,-5.88066771931294,-14.7534170506565)) ;
#36913 = CARTESIAN_POINT('Ctrl Pts',(19.5686943715667,-5.54190685110016,-14.7445634423528)) ;
#36914 = CARTESIAN_POINT('Ctrl Pts',(19.7781124555335,-4.7502994045236,-14.7242883946986)) ;
#36915 = CARTESIAN_POINT('Ctrl Pts',(19.881758767847,-4.2958992688073,-14.712930618706)) ;
#36916 = CARTESIAN_POINT('Ctrl Pts',(20.1019323774357,-3.15040311145857,-14.6845939920956)) ;
#36917 = CARTESIAN_POINT('Ctrl Pts',(20.1985226533667,-2.45609586418258,-14.6676719691478)) ;
#36918 = CARTESIAN_POINT('Ctrl Pts',(20.3087787733636,-1.18564937864585,-14.6364940506944)) ;
#36919 = CARTESIAN_POINT('Ctrl Pts',(20.3341734607863,-0.6112622026835,-14.6223230058526)) ;
#36920 = CARTESIAN_POINT('Ctrl Pts',(20.3365274559342,0.697512022562245,-14.5896675549361)) ;
#36921 = CARTESIAN_POINT('Ctrl Pts',(20.2980967610298,1.43112695980136,-14.5710915794615)) ;
#36922 = CARTESIAN_POINT('Ctrl Pts',(20.1635790872482,2.68975644455828,-14.5388943302587)) ;
#36923 = CARTESIAN_POINT('Ctrl Pts',(20.0863576339816,3.21604567820772,-14.5253375590982)) ;
#36924 = CARTESIAN_POINT('Ctrl Pts',(19.9237170107269,4.08558749479809,-14.5029877367147)) ;
#36925 = CARTESIAN_POINT('Ctrl Pts',(19.8498154701953,4.43072868203372,-14.4941341320922)) ;
#36926 = CARTESIAN_POINT('Ctrl Pts',(19.6575897469739,5.22668557556732,-14.4738590873597)) ;
#36927 = CARTESIAN_POINT('Ctrl Pts',(19.5326764966984,5.67570534257694,-14.4625013106784)) ;
#36928 = CARTESIAN_POINT('Ctrl Pts',(19.1816206861132,6.78808903594647,-14.434164686282)) ;
#36929 = CARTESIAN_POINT('Ctrl Pts',(18.9364126651438,7.44479680596961,-14.4172426661441)) ;
#36930 = CARTESIAN_POINT('Ctrl Pts',(18.4292436451885,8.61482665690823,-14.386064751637)) ;
#36931 = CARTESIAN_POINT('Ctrl Pts',(18.1784335648506,9.13218511036002,-14.3718937078825)) ;
#36932 = CARTESIAN_POINT('Ctrl Pts',(17.5581176850556,10.2846183525344,-14.3392382697389)) ;
#36933 = CARTESIAN_POINT('Ctrl Pts',(17.1754406882582,10.9116952381982,-14.3206623062712)) ;
#36934 = CARTESIAN_POINT('Ctrl Pts',(16.4585665486567,11.9549278042565,-14.288465061813)) ;
#36935 = CARTESIAN_POINT('Ctrl Pts',(16.1403589644349,12.3811762610222,-14.2749082832902)) ;
#36936 = CARTESIAN_POINT('Ctrl Pts',(15.5837754330599,13.0687592373938,-14.2525584516795)) ;
#36937 = CARTESIAN_POINT('Ctrl Pts',(15.3546333075434,13.3372323552268,-14.2437048451206)) ;
#36938 = CARTESIAN_POINT('Ctrl Pts',(14.8070175421818,13.9460140633165,-14.2234297988823)) ;
#36939 = CARTESIAN_POINT('Ctrl Pts',(14.4836016339789,14.2816093613836,-14.2120720225994)) ;
#36940 = CARTESIAN_POINT('Ctrl Pts',(13.6457881896671,15.0932166783478,-14.183735396665)) ;
#36941 = CARTESIAN_POINT('Ctrl Pts',(13.1177843029926,15.5543067732995,-14.1668133746529)) ;
#36942 = CARTESIAN_POINT('Ctrl Pts',(12.115226137486,16.3423852400491,-14.1356354575289)) ;
#36943 = CARTESIAN_POINT('Ctrl Pts',(11.6485617076652,16.6782271821253,-14.1214644130649)) ;
#36944 = CARTESIAN_POINT('Ctrl Pts',(10.5548374496442,17.3970192273679,-14.0888089693573)) ;
#36945 = CARTESIAN_POINT('Ctrl Pts',(9.91999445320359,17.7666700915468,-14.0702330009091)) ;
#36946 = CARTESIAN_POINT('Ctrl Pts',(8.79325938757738,18.3434811542774,-14.0380357545278)) ;
#36947 = CARTESIAN_POINT('Ctrl Pts',(8.31063355588396,18.5671237104765,-14.024478979104)) ;
#36948 = CARTESIAN_POINT('Ctrl Pts',(7.49403356605316,18.9072997977826,-14.0021291513409)) ;
#36949 = CARTESIAN_POINT('Ctrl Pts',(7.16478753904079,19.0345042069972,-13.9932755455622)) ;
#36950 = CARTESIAN_POINT('Ctrl Pts',(6.39355018054793,19.3096243579578,-13.9730004999153)) ;
#36951 = CARTESIAN_POINT('Ctrl Pts',(5.94945259307183,19.4510435733835,-13.9616427234541)) ;
#36952 = CARTESIAN_POINT('Ctrl Pts',(4.82647793343027,19.7665838150784,-13.9333060983236)) ;
#36953 = CARTESIAN_POINT('Ctrl Pts',(4.14272761925487,19.921107700979,-13.916384077262)) ;
#36954 = CARTESIAN_POINT('Ctrl Pts',(2.88601800327718,20.1376056114963,-13.8852061614592)) ;
#36955 = CARTESIAN_POINT('Ctrl Pts',(2.31578900329025,20.211120035043,-13.8710351173489)) ;
#36956 = CARTESIAN_POINT('Ctrl Pts',(1.01183071483298,20.3233134629898,-13.8383796752688)) ;
#36957 = CARTESIAN_POINT('Ctrl Pts',(0.277579105510846,20.346591996161,-13.8198037081226)) ;
#36958 = CARTESIAN_POINT('Ctrl Pts',(-0.987899490826792,20.3181880625369,
-13.7876064622164)) ;
#36959 = CARTESIAN_POINT('Ctrl Pts',(-1.51881324726421,20.2854114903864,-13.7740496859548)) ;
#36960 = CARTESIAN_POINT('Ctrl Pts',(-2.39893785524069,20.1963269409041,-13.7516998571747)) ;
#36961 = CARTESIAN_POINT('Ctrl Pts',(-2.74906395265028,20.1516544798401,-13.7428462512073)) ;
#36962 = CARTESIAN_POINT('Ctrl Pts',(-3.55834620266862,20.0269131185032,-13.7225712054274)) ;
#36963 = CARTESIAN_POINT('Ctrl Pts',(-4.0162657858277,19.9401276672434,-13.7112134290212)) ;
#36964 = CARTESIAN_POINT('Ctrl Pts',(-5.15418922315739,19.6836749219689,-13.6828768035733)) ;
#36965 = CARTESIAN_POINT('Ctrl Pts',(-5.82916060428898,19.4944507702114,-13.6659547821514)) ;
#36966 = CARTESIAN_POINT('Ctrl Pts',(-7.03762968589347,19.0872739826849,-13.6347768658501)) ;
#36967 = CARTESIAN_POINT('Ctrl Pts',(-7.57421360100202,18.8807717032836,-13.6206058216082)) ;
#36968 = CARTESIAN_POINT('Ctrl Pts',(-8.77464479071782,18.3593703648678,-13.5879503813168)) ;
#36969 = CARTESIAN_POINT('Ctrl Pts',(-9.43162786276003,18.0306752997138,-13.5693744161529)) ;
#36970 = CARTESIAN_POINT('Ctrl Pts',(-10.531347936492,17.4038910086251,-13.5371771710166)) ;
#36971 = CARTESIAN_POINT('Ctrl Pts',(-10.982800075023,17.1225820359373,-13.523620393526)) ;
#36972 = CARTESIAN_POINT('Ctrl Pts',(-11.7146719300653,16.6256725072387,-13.5012705631693)) ;
#36973 = CARTESIAN_POINT('Ctrl Pts',(-12.0014300436204,16.4198723444649,-13.4924169568436)) ;
#36974 = CARTESIAN_POINT('Ctrl Pts',(-12.654026035905,15.9252849843984,-13.4721419107723)) ;
#36975 = CARTESIAN_POINT('Ctrl Pts',(-13.0155820663386,15.6311773619367,-13.4607841344249)) ;
#36976 = CARTESIAN_POINT('Ctrl Pts',(-13.8946448012753,14.8644398090299,-13.4324475088949)) ;
#36977 = CARTESIAN_POINT('Ctrl Pts',(-14.3984242406956,14.3769991158017,-13.4155254873372)) ;
#36978 = CARTESIAN_POINT('Ctrl Pts',(-15.2678684628203,13.4441233365775,-13.3843475708726)) ;
#36979 = CARTESIAN_POINT('Ctrl Pts',(-15.6416933658884,13.0072933554173,-13.370176526606)) ;
#36980 = CARTESIAN_POINT('Ctrl Pts',(-16.44974914612,11.9777555821607,-13.3375210122179)) ;
#36981 = CARTESIAN_POINT('Ctrl Pts',(-16.8713807195268,11.3761756702548,-13.3189449707417)) ;
#36982 = CARTESIAN_POINT('Ctrl Pts',(-17.5407255078541,10.3018279088841,-13.2867476969551)) ;
#36983 = CARTESIAN_POINT('Ctrl Pts',(-17.8040855733151,9.83967722895478,-13.2731909677616)) ;
#36984 = CARTESIAN_POINT('Ctrl Pts',(-18.2115988808362,9.05451216737767,-13.2508411986072)) ;
#36985 = CARTESIAN_POINT('Ctrl Pts',(-18.3659884079632,8.73710480294482,-13.2419876056377)) ;
#36986 = CARTESIAN_POINT('Ctrl Pts',(-18.7048689174683,7.99168040154145,-13.2217125701352)) ;
#36987 = CARTESIAN_POINT('Ctrl Pts',(-18.8830630479746,7.56101926201225,-13.2103547912493)) ;
#36988 = CARTESIAN_POINT('Ctrl Pts',(-19.2917429981322,6.46849105799463,-13.1820181721876)) ;
#36989 = CARTESIAN_POINT('Ctrl Pts',(-19.503109886224,5.80012314008325,-13.1650961593188)) ;
#36990 = CARTESIAN_POINT('Ctrl Pts',(-19.8243216146061,4.56601928410968,-13.1339182538095)) ;
#36991 = CARTESIAN_POINT('Ctrl Pts',(-19.9454369469548,4.00397261185963,-13.1197472116332)) ;
#36992 = CARTESIAN_POINT('Ctrl Pts',(-20.1666572808306,2.71415284203437,-13.0870948303192)) ;
#36993 = CARTESIAN_POINT('Ctrl Pts',(-20.2514731144785,1.98456865362528,-13.0685220144798)) ;
#36994 = CARTESIAN_POINT('Ctrl Pts',(-20.329403307692,0.721217768220855,-13.0363259505766)) ;
#36995 = CARTESIAN_POINT('Ctrl Pts',(-20.3413112248757,0.189348972981878,
-13.0227671787657)) ;
#36996 = CARTESIAN_POINT('Ctrl Pts',(-20.3264156435255,-0.695245817713759,
-13.0004148214405)) ;
#36997 = CARTESIAN_POINT('Ctrl Pts',(-20.3112883989533,-1.04790714701697,
-12.9915606638422)) ;
#36998 = CARTESIAN_POINT('Ctrl Pts',(-20.2549134348881,-1.8648201028368,-12.9712851816854)) ;
#36999 = CARTESIAN_POINT('Ctrl Pts',(-20.2068705024629,-2.32840337181275,
-12.9599275102734)) ;
#37000 = CARTESIAN_POINT('Ctrl Pts',(-20.0468340372782,-3.48384722064875,
-12.9315906168136)) ;
#37001 = CARTESIAN_POINT('Ctrl Pts',(-19.9149283673365,-4.17233432271597,
-12.9146682355612)) ;
#37002 = CARTESIAN_POINT('Ctrl Pts',(-19.6106151643196,-5.4107334898701,-12.8834898657631)) ;
#37003 = CARTESIAN_POINT('Ctrl Pts',(-19.4498778512491,-5.96276007333131,
-12.8693187351503)) ;
#37004 = CARTESIAN_POINT('Ctrl Pts',(-19.0324601571692,-7.19860943130656,
-12.836771516659)) ;
#37005 = CARTESIAN_POINT('Ctrl Pts',(-18.7618976180403,-7.87690928700065,
-12.8183071257014)) ;
#37006 = CARTESIAN_POINT('Ctrl Pts',(-18.2310278865844,-9.02426027681257,
-12.786151369651)) ;
#37007 = CARTESIAN_POINT('Ctrl Pts',(-17.9875531216752,-9.50029396764206,
-12.7725235508096)) ;
#37008 = CARTESIAN_POINT('Ctrl Pts',(-17.5522851400165,-10.2744509724509,
-12.7500837103629)) ;
#37009 = CARTESIAN_POINT('Ctrl Pts',(-17.3709475889917,-10.5781492922524,
-12.7412104741872)) ;
#37010 = CARTESIAN_POINT('Ctrl Pts',(-16.9326544202609,-11.2704982178444,
-12.720919941201)) ;
#37011 = CARTESIAN_POINT('Ctrl Pts',(-16.6700805757201,-11.6553564893335,
-12.7095659404388)) ;
#37012 = CARTESIAN_POINT('Ctrl Pts',(-15.9797519222731,-12.5960713068128,
-12.6812198625451)) ;
#37013 = CARTESIAN_POINT('Ctrl Pts',(-15.5360304497324,-13.1394536018569,
-12.6642850815589)) ;
#37014 = CARTESIAN_POINT('Ctrl Pts',(-14.6790323109405,-14.0846875676049,
-12.6330910835965)) ;
#37015 = CARTESIAN_POINT('Ctrl Pts',(-14.2750497206702,-14.4939767155589,
-12.6189169760098)) ;
#37016 = CARTESIAN_POINT('Ctrl Pts',(-13.3035522912369,-15.3981655343969,
-12.5858031408785)) ;
#37017 = CARTESIAN_POINT('Ctrl Pts',(-12.724813319516,-15.8797706140345,-12.566757921796)) ;
#37018 = CARTESIAN_POINT('Ctrl Pts',(-11.5653282938198,-16.7404783152019,
-12.53002185721)) ;
#37019 = CARTESIAN_POINT('Ctrl Pts',(-10.9892530655328,-17.1241570683089,
-12.5123742754328)) ;
#37020 = CARTESIAN_POINT('Ctrl Pts',(-10.1196035711132,-17.6413744453928,
-12.4870257394034)) ;
#37021 = CARTESIAN_POINT('Ctrl Pts',(-9.84063600884161,-17.7984929912793,
-12.4790957632584)) ;
#37022 = CARTESIAN_POINT('Ctrl Pts',(-8.76973875852369,-18.368760611688,-12.4493068271358)) ;
#37023 = CARTESIAN_POINT('Ctrl Pts',(-7.95460237524104,-18.736168344006,-12.4278452409879)) ;
#37024 = CARTESIAN_POINT('Ctrl Pts',(-6.53507870208474,-19.2666010060396,
-12.3909211991686)) ;
#37025 = CARTESIAN_POINT('Ctrl Pts',(-5.94251788476641,-19.4575342757416,
-12.3756441334639)) ;
#37026 = CARTESIAN_POINT('Ctrl Pts',(-4.68058609153175,-19.8011160500778,
-12.3431097415594)) ;
#37027 = CARTESIAN_POINT('Ctrl Pts',(-4.01035082367705,-19.9476604071713,
-12.3258267224519)) ;
#37028 = CARTESIAN_POINT('Ctrl Pts',(-2.72525323735467,-20.1612448052724,
-12.2927443248325)) ;
#37029 = CARTESIAN_POINT('Ctrl Pts',(-2.11221498516215,-20.2346570257772,
-12.2769898775049)) ;
#37030 = CARTESIAN_POINT('Ctrl Pts',(-1.12212018118544,-20.3077318824365,
-12.2518683441286)) ;
#37031 = CARTESIAN_POINT('Ctrl Pts',(-0.746751946405798,-20.3249968190638,
-12.2424223496793)) ;
#37032 = CARTESIAN_POINT('Ctrl Pts',(0.0513961026171948,-20.3395654194972,
-12.2226279674806)) ;
#37033 = CARTESIAN_POINT('Ctrl Pts',(0.474050221572415,-20.3341054352808,
-12.2123026061609)) ;
#37034 = CARTESIAN_POINT('Ctrl Pts',(1.63162959178368,-20.2830381752318,-12.1841175910848)) ;
#37035 = CARTESIAN_POINT('Ctrl Pts',(2.36472561101066,-20.2106884269275,-12.1663566960149)) ;
#37036 = CARTESIAN_POINT('Ctrl Pts',(3.66898964405881,-20.01002163033,-12.1341201998595)) ;
#37037 = CARTESIAN_POINT('Ctrl Pts',(4.24160694275495,-19.8965125860197,-12.1197467362106)) ;
#37038 = CARTESIAN_POINT('Ctrl Pts',(5.7116274166498,-19.5387603669351,-12.0820257340898)) ;
#37039 = CARTESIAN_POINT('Ctrl Pts',(6.59857169675064,-19.2573275633482,-12.0584170482112)) ;
#37040 = CARTESIAN_POINT('Ctrl Pts',(8.0167078703821,-18.6978212513221,-12.0196230613945)) ;
#37041 = CARTESIAN_POINT('Ctrl Pts',(8.56042598330759,-18.455222523287,-12.0044969377431)) ;
#37042 = CARTESIAN_POINT('Ctrl Pts',(9.40661172232529,-18.0322153377766,-11.980885384834)) ;
#37043 = CARTESIAN_POINT('Ctrl Pts',(9.7163864692485,-17.8672037023283,-11.9722435455832)) ;
#37044 = CARTESIAN_POINT('Ctrl Pts',(10.7004117119079,-17.3098680515347,-11.9445910995291)) ;
#37045 = CARTESIAN_POINT('Ctrl Pts',(11.3564116163775,-16.8867482559813,-11.9258062681128)) ;
#37046 = CARTESIAN_POINT('Ctrl Pts',(12.4973696507733,-16.0542115421019,-11.8914086492038)) ;
#37047 = CARTESIAN_POINT('Ctrl Pts',(12.9905817363718,-15.6578010352562,-11.8758921440458)) ;
#37048 = CARTESIAN_POINT('Ctrl Pts',(14.404844553611,-14.4082246461022,-11.8289663288442)) ;
#37049 = CARTESIAN_POINT('Ctrl Pts',(15.2662510313588,-13.4921451386782,-11.7968916949704)) ;
#37050 = CARTESIAN_POINT('Ctrl Pts',(16.2914439660495,-12.1770753735735,-11.7546223485855)) ;
#37051 = CARTESIAN_POINT('Ctrl Pts',(16.5352189102869,-11.843937362808,-11.7442188775614)) ;
#37052 = CARTESIAN_POINT('Ctrl Pts',(17.0246289195859,-11.1305296550288,-11.722731659385)) ;
#37053 = CARTESIAN_POINT('Ctrl Pts',(17.2680485320547,-10.749008595165,-11.711677389608)) ;
#37054 = CARTESIAN_POINT('Ctrl Pts',(17.7219347600441,-9.98234945919308,-11.6900089439147)) ;
#37055 = CARTESIAN_POINT('Ctrl Pts',(17.9330259355545,-9.59795386329417,-11.6793991614211)) ;
#37056 = CARTESIAN_POINT('Ctrl Pts',(18.1314964616938,-9.20710714161543,-11.6687558745767)) ;
#37057 = CARTESIAN_POINT('Ctrl Pts',(18.1314964436398,-9.20710717716894,-11.0322347276753)) ;
#37058 = CARTESIAN_POINT('Ctrl Pts',(18.0566892618479,-9.35442447504745,-11.036298634348)) ;
#37059 = CARTESIAN_POINT('Ctrl Pts',(17.9800859455993,-9.50083148223316,-11.0403445448935)) ;
#37060 = CARTESIAN_POINT('Ctrl Pts',(17.6178387460248,-10.1730938980304,-11.0589891313672)) ;
#37061 = CARTESIAN_POINT('Ctrl Pts',(17.3108587948471,-10.6871068634057,-11.0734444332431)) ;
#37062 = CARTESIAN_POINT('Ctrl Pts',(16.6197502037577,-11.736212507307,-11.103958900449)) ;
#37063 = CARTESIAN_POINT('Ctrl Pts',(16.231397660812,-12.2677015846865,-11.1200202695315)) ;
#37064 = CARTESIAN_POINT('Ctrl Pts',(15.4495771182218,-13.2354142166768,-11.150819029114)) ;
#37065 = CARTESIAN_POINT('Ctrl Pts',(15.0616417406918,-13.675253622841,-11.1654932884422)) ;
#37066 = CARTESIAN_POINT('Ctrl Pts',(14.1372967015666,-14.6361545773828,-11.1991806525867)) ;
#37067 = CARTESIAN_POINT('Ctrl Pts',(13.5900626531215,-15.1456385955681,-11.2182625805862)) ;
#37068 = CARTESIAN_POINT('Ctrl Pts',(12.6791180873017,-15.9045356018542,-11.2483461517184)) ;
#37069 = CARTESIAN_POINT('Ctrl Pts',(12.3332013899885,-16.1742522617928,-11.2594161431569)) ;
#37070 = CARTESIAN_POINT('Ctrl Pts',(11.6232535875375,-16.6917820379748,-11.281254883196)) ;
#37071 = CARTESIAN_POINT('Ctrl Pts',(11.2593507949114,-16.9393812344377,-11.2920166697651)) ;
#37072 = CARTESIAN_POINT('Ctrl Pts',(9.84050989198713,-17.8388241530597,-11.3328969405192)) ;
#37073 = CARTESIAN_POINT('Ctrl Pts',(8.73480518989878,-18.405500877718,-11.3627229914717)) ;
#37074 = CARTESIAN_POINT('Ctrl Pts',(6.97323581450083,-19.1136033118688,-11.4098859154353)) ;
#37075 = CARTESIAN_POINT('Ctrl Pts',(6.35051016463328,-19.3294298320257,-11.4264574366206)) ;
#37076 = CARTESIAN_POINT('Ctrl Pts',(4.94453393834806,-19.741425701259,-11.4636197508681)) ;
#37077 = CARTESIAN_POINT('Ctrl Pts',(4.15784919182704,-19.9219625841466,-11.4842552003682)) ;
#37078 = CARTESIAN_POINT('Ctrl Pts',(3.04686803574372,-20.1082327192256,-11.5126185028616)) ;
#37079 = CARTESIAN_POINT('Ctrl Pts',(2.73000102682804,-20.1536975950115,-11.5206094675228)) ;
#37080 = CARTESIAN_POINT('Ctrl Pts',(1.72661538515555,-20.2735666118176,-11.5455533565328)) ;
#37081 = CARTESIAN_POINT('Ctrl Pts',(1.03731127826029,-20.320499567124,-11.5622429886949)) ;
#37082 = CARTESIAN_POINT('Ctrl Pts',(-0.421549536565036,-20.3453938772391,
-11.5976348281654)) ;
#37083 = CARTESIAN_POINT('Ctrl Pts',(-1.19017337345049,-20.3149263527762,
-11.6163302770035)) ;
#37084 = CARTESIAN_POINT('Ctrl Pts',(-2.52769396458766,-20.1857259512756,
-11.6495662217085)) ;
#37085 = CARTESIAN_POINT('Ctrl Pts',(-3.09755859930884,-20.1061654994494,
-11.6639462101679)) ;
#37086 = CARTESIAN_POINT('Ctrl Pts',(-4.35410842691338,-19.8760402791194,
-11.6961894305837)) ;
#37087 = CARTESIAN_POINT('Ctrl Pts',(-5.03791746861582,-19.7138179352369,
-11.7141042275286)) ;
#37088 = CARTESIAN_POINT('Ctrl Pts',(-6.15854630799884,-19.3858407094886,
-11.7437772690061)) ;
#37089 = CARTESIAN_POINT('Ctrl Pts',(-6.60052142164793,-19.2398449594205,
-11.7555593040985)) ;
#37090 = CARTESIAN_POINT('Ctrl Pts',(-7.37053878020162,-18.955828948767,-11.7760368056274)) ;
#37091 = CARTESIAN_POINT('Ctrl Pts',(-7.70069597317297,-18.8241221504686,
-11.7847841930272)) ;
#37092 = CARTESIAN_POINT('Ctrl Pts',(-8.52416630073965,-18.4703302904785,
-11.8066909854947)) ;
#37093 = CARTESIAN_POINT('Ctrl Pts',(-9.01238660192301,-18.2370886773914,
-11.8197720375566)) ;
#37094 = CARTESIAN_POINT('Ctrl Pts',(-10.1287370561163,-17.647976763951,-11.8504001826418)) ;
#37095 = CARTESIAN_POINT('Ctrl Pts',(-10.748373671431,-17.2775823501562,-11.8679693700332)) ;
#37096 = CARTESIAN_POINT('Ctrl Pts',(-11.8244770083481,-16.5539957724781,
-11.9000437433199)) ;
#37097 = CARTESIAN_POINT('Ctrl Pts',(-12.2880960828762,-16.212825744257,-11.9144298521117)) ;
#37098 = CARTESIAN_POINT('Ctrl Pts',(-13.2848401305551,-15.4119941257301,
-11.9467029966208)) ;
#37099 = CARTESIAN_POINT('Ctrl Pts',(-13.809840482815,-14.9433877917634,-11.9646419497777)) ;
#37100 = CARTESIAN_POINT('Ctrl Pts',(-14.6398529273788,-14.1213619056663,
-11.9943279910468)) ;
#37101 = CARTESIAN_POINT('Ctrl Pts',(-14.9588854111087,-13.7829571403322,
-12.006099598405)) ;
#37102 = CARTESIAN_POINT('Ctrl Pts',(-15.5016595812026,-13.1661591149811,
-12.026597334191)) ;
#37103 = CARTESIAN_POINT('Ctrl Pts',(-15.7301951048606,-12.8922518501087,
-12.0353746730684)) ;
#37104 = CARTESIAN_POINT('Ctrl Pts',(-16.2897519376653,-12.1845621239422,
-12.0574240567864)) ;
#37105 = CARTESIAN_POINT('Ctrl Pts',(-16.6107403448509,-11.7432057417062,
-12.0706162868542)) ;
#37106 = CARTESIAN_POINT('Ctrl Pts',(-17.3120051469498,-10.692589484698,-12.1012683055797)) ;
#37107 = CARTESIAN_POINT('Ctrl Pts',(-17.6785369989615,-10.0750340898224,
-12.1187497834374)) ;
#37108 = CARTESIAN_POINT('Ctrl Pts',(-18.2794016099887,-8.92850312041314,
-12.1507710190593)) ;
#37109 = CARTESIAN_POINT('Ctrl Pts',(-18.5252882686476,-8.40644854232918,
-12.165195550606)) ;
#37110 = CARTESIAN_POINT('Ctrl Pts',(-19.0232288734611,-7.22090883673879,
-12.1976565854428)) ;
#37111 = CARTESIAN_POINT('Ctrl Pts',(-19.2634274811846,-6.55325228302571,
-12.2157472232844)) ;
#37112 = CARTESIAN_POINT('Ctrl Pts',(-19.6006573210983,-5.43564802233724,
-12.2454075447318)) ;
#37113 = CARTESIAN_POINT('Ctrl Pts',(-19.7181837034024,-4.9925216744397,-12.2570072690369)) ;
#37114 = CARTESIAN_POINT('Ctrl Pts',(-19.9012846902632,-4.19416345328748,
-12.2774363918178)) ;
#37115 = CARTESIAN_POINT('Ctrl Pts',(-19.9725599621307,-3.84044115399536,
-12.2863107869349)) ;
#37116 = CARTESIAN_POINT('Ctrl Pts',(-20.1304720784916,-2.93264680309043,
-12.3088234309956)) ;
#37117 = CARTESIAN_POINT('Ctrl Pts',(-20.2036720143247,-2.37654458057251,
-12.3223771615009)) ;
#37118 = CARTESIAN_POINT('Ctrl Pts',(-20.3164784164307,-1.11989077530671,
-12.353001183084)) ;
#37119 = CARTESIAN_POINT('Ctrl Pts',(-20.3430080730884,-0.41888376827425,
-12.3700897316749)) ;
#37120 = CARTESIAN_POINT('Ctrl Pts',(-20.3252414322484,0.861762165061094,
-12.4017808313418)) ;
#37121 = CARTESIAN_POINT('Ctrl Pts',(-20.2924146577997,1.44082333602945,-12.4162832564512)) ;
#37122 = CARTESIAN_POINT('Ctrl Pts',(-20.163366808376,2.7350138593994,-12.4491255895736)) ;
#37123 = CARTESIAN_POINT('Ctrl Pts',(-20.0537463860115,3.44802991823574,-12.4675241558239)) ;
#37124 = CARTESIAN_POINT('Ctrl Pts',(-19.8161596500103,4.58665495070952,-12.4970657655909)) ;
#37125 = CARTESIAN_POINT('Ctrl Pts',(-19.7117206798026,5.01653853587843,-12.5082516052741)) ;
#37126 = CARTESIAN_POINT('Ctrl Pts',(-19.4952060723064,5.79597976929068,-12.5284205887677)) ;
#37127 = CARTESIAN_POINT('Ctrl Pts',(-19.3875264678072,6.14656483326287,-12.5374350903917)) ;
#37128 = CARTESIAN_POINT('Ctrl Pts',(-19.08433431817,7.04625688323722,-12.5606214490273)) ;
#37129 = CARTESIAN_POINT('Ctrl Pts',(-18.8745914461672,7.59021435148052,-12.5747020599811)) ;
#37130 = CARTESIAN_POINT('Ctrl Pts',(-18.3581811583187,8.77513761122839,-12.6060876021864)) ;
#37131 = CARTESIAN_POINT('Ctrl Pts',(-18.0407087789179,9.41056171121832,-12.6234121218039)) ;
#37132 = CARTESIAN_POINT('Ctrl Pts',(-17.3935133449375,10.5522875409961,-12.6559372739215)) ;
#37133 = CARTESIAN_POINT('Ctrl Pts',(-17.0732115187385,11.0630247912466,-12.6710431513239)) ;
#37134 = CARTESIAN_POINT('Ctrl Pts',(-16.267768063359,12.2288604308801,-12.7068878086331)) ;
#37135 = CARTESIAN_POINT('Ctrl Pts',(-15.7649931234071,12.8705201861648,-12.7277222660458)) ;
#37136 = CARTESIAN_POINT('Ctrl Pts',(-14.9813695185047,13.7555710024903,-12.7576196422071)) ;
#37137 = CARTESIAN_POINT('Ctrl Pts',(-14.7302170631559,14.0241890250451,-12.7668575576336)) ;
#37138 = CARTESIAN_POINT('Ctrl Pts',(-14.0270899450958,14.7364739457685,-12.7916641107128)) ;
#37139 = CARTESIAN_POINT('Ctrl Pts',(-13.5614545576104,15.1660766100367,-12.8070212246478)) ;
#37140 = CARTESIAN_POINT('Ctrl Pts',(-12.3831480523363,16.1554756381271,-12.8443386486679)) ;
#37141 = CARTESIAN_POINT('Ctrl Pts',(-11.6516583014095,16.6907338212634,-12.8662883651654)) ;
#37142 = CARTESIAN_POINT('Ctrl Pts',(-10.3952162257203,17.4871498557438,-12.9031044217192)) ;
#37143 = CARTESIAN_POINT('Ctrl Pts',(-9.89033530316382,17.7775754580964,-12.9176721986956)) ;
#37144 = CARTESIAN_POINT('Ctrl Pts',(-8.7251378485802,18.3828200002772,-12.9508351460039)) ;
#37145 = CARTESIAN_POINT('Ctrl Pts',(-8.0588928922872,18.6844946290157,-12.9694928070031)) ;
#37146 = CARTESIAN_POINT('Ctrl Pts',(-6.95430589570256,19.1145549278497,-12.9995878687193)) ;
#37147 = CARTESIAN_POINT('Ctrl Pts',(-6.52533673009241,19.2652164768086,-13.011074113294)) ;
#37148 = CARTESIAN_POINT('Ctrl Pts',(-5.69891768599815,19.52469696654,-13.0326252262983)) ;
#37149 = CARTESIAN_POINT('Ctrl Pts',(-5.30250099061949,19.636062252115,-13.0427102296833)) ;
#37150 = CARTESIAN_POINT('Ctrl Pts',(-3.68015293350261,20.0391129708792,-13.0834348842783)) ;
#37151 = CARTESIAN_POINT('Ctrl Pts',(-2.43174476311662,20.2285986005478,-13.1136983174551)) ;
#37152 = CARTESIAN_POINT('Ctrl Pts',(-0.5390004985823,20.3380392674615,-13.1607582867672)) ;
#37153 = CARTESIAN_POINT('Ctrl Pts',(0.0972128450064538,20.3449478059646,
-13.1767365319779)) ;
#37154 = CARTESIAN_POINT('Ctrl Pts',(1.51594820637505,20.2937962450181,-13.2127130412846)) ;
#37155 = CARTESIAN_POINT('Ctrl Pts',(2.29690909705949,20.2202984671873,-13.2327613045522)) ;
#37156 = CARTESIAN_POINT('Ctrl Pts',(3.41373945141306,20.0496411437315,-13.2612887840401)) ;
#37157 = CARTESIAN_POINT('Ctrl Pts',(3.75441923683923,19.9886485090049,-13.2699629951663)) ;
#37158 = CARTESIAN_POINT('Ctrl Pts',(4.71173751112913,19.7919182468557,-13.2941489981447)) ;
#37159 = CARTESIAN_POINT('Ctrl Pts',(5.32384633183264,19.636119027211,-13.3094505388668)) ;
#37160 = CARTESIAN_POINT('Ctrl Pts',(6.77058710057535,19.1952477725674,-13.3461305114116)) ;
#37161 = CARTESIAN_POINT('Ctrl Pts',(7.59586505908332,18.8838875411011,-13.3675047001487)) ;
#37162 = CARTESIAN_POINT('Ctrl Pts',(8.9271745921226,18.2801727861172,-13.4036779926435)) ;
#37163 = CARTESIAN_POINT('Ctrl Pts',(9.4454915734253,18.0178201624902,-13.4182053964112)) ;
#37164 = CARTESIAN_POINT('Ctrl Pts',(10.5838377577577,17.3789968142754,-13.4511701813564)) ;
#37165 = CARTESIAN_POINT('Ctrl Pts',(11.1963977951298,16.990815781739,-13.469667681205)) ;
#37166 = CARTESIAN_POINT('Ctrl Pts',(12.1432377407707,16.3173208458749,-13.499174706412)) ;
#37167 = CARTESIAN_POINT('Ctrl Pts',(12.4912868324381,16.0524434194065,-13.5102313986805)) ;
#37168 = CARTESIAN_POINT('Ctrl Pts',(13.1166301935421,15.5438731394018,-13.5303252021079)) ;
#37169 = CARTESIAN_POINT('Ctrl Pts',(13.3963512900077,15.3034555739844,-13.5393893199704)) ;
#37170 = CARTESIAN_POINT('Ctrl Pts',(14.1066521035878,14.6585530485366,-13.5628161249132)) ;
#37171 = CARTESIAN_POINT('Ctrl Pts',(14.5264213884448,14.2426786965329,-13.5770851948431)) ;
#37172 = CARTESIAN_POINT('Ctrl Pts',(15.4085840839167,13.2890716189011,-13.6086336472594)) ;
#37173 = CARTESIAN_POINT('Ctrl Pts',(15.862165002764,12.7442378610308,-13.6259314045786)) ;
#37174 = CARTESIAN_POINT('Ctrl Pts',(16.651465025194,11.688558941956,-13.6586111460248)) ;
#37175 = CARTESIAN_POINT('Ctrl Pts',(16.9943985513127,11.1841005657229,-13.6739036739568)) ;
#37176 = CARTESIAN_POINT('Ctrl Pts',(17.5382164045228,10.3012370006598,-13.7001450491441)) ;
#37177 = CARTESIAN_POINT('Ctrl Pts',(17.7507653702497,9.93050077307125,-13.7110148847182)) ;
#37178 = CARTESIAN_POINT('Ctrl Pts',(18.2429496488048,9.00564838391378,-13.7376773902474)) ;
#37179 = CARTESIAN_POINT('Ctrl Pts',(18.5092046976381,8.44489566614177,-13.7534651184153)) ;
#37180 = CARTESIAN_POINT('Ctrl Pts',(18.8804332177875,7.56080461403457,-13.7774231923831)) ;
#37181 = CARTESIAN_POINT('Ctrl Pts',(19.0036491510871,7.24553958597785,-13.7857718418013)) ;
#37182 = CARTESIAN_POINT('Ctrl Pts',(19.2819199811741,6.47753359224639,-13.805770076588)) ;
#37183 = CARTESIAN_POINT('Ctrl Pts',(19.4289757211978,6.02210803125775,-13.8173617184285)) ;
#37184 = CARTESIAN_POINT('Ctrl Pts',(19.786245072644,4.76568414680968,-13.8490404295854)) ;
#37185 = CARTESIAN_POINT('Ctrl Pts',(19.9638259441646,3.95637227027586,-13.8691465634733)) ;
#37186 = CARTESIAN_POINT('Ctrl Pts',(20.1807119036668,2.56794258003691,-13.9039114855573)) ;
#37187 = CARTESIAN_POINT('Ctrl Pts',(20.2454932410903,1.99385475191587,-13.91835382311)) ;
#37188 = CARTESIAN_POINT('Ctrl Pts',(20.3353798108998,0.707759959603777,-13.9509019621734)) ;
#37189 = CARTESIAN_POINT('Ctrl Pts',(20.3476919958434,-0.00438795168989717,
-13.969062928623)) ;
#37190 = CARTESIAN_POINT('Ctrl Pts',(20.3066418432188,-1.17001440531332,-13.9986946904666)) ;
#37191 = CARTESIAN_POINT('Ctrl Pts',(20.2754129431107,-1.62365974657679,-14.0101983246054)) ;
#37192 = CARTESIAN_POINT('Ctrl Pts',(20.192048098113,-2.43603301316927,-14.0305647493857)) ;
#37193 = CARTESIAN_POINT('Ctrl Pts',(20.1454777829067,-2.7951365758985,-14.0394694047063)) ;
#37194 = CARTESIAN_POINT('Ctrl Pts',(20.0016850960595,-3.71136854291113,-14.0621269840593)) ;
#37195 = CARTESIAN_POINT('Ctrl Pts',(19.8907671598969,-4.26603429286399,-14.0757939315026)) ;
#37196 = CARTESIAN_POINT('Ctrl Pts',(19.5924066585068,-5.49017466750817,-14.1063783939317)) ;
#37197 = CARTESIAN_POINT('Ctrl Pts',(19.3934684693106,-6.15611792462093,-14.1233124246089)) ;
#37198 = CARTESIAN_POINT('Ctrl Pts',(18.9665715038959,-7.35714903919237,-14.1548528757879)) ;
#37199 = CARTESIAN_POINT('Ctrl Pts',(18.7489979705012,-7.89515946049258,-14.1693645498328)) ;
#37200 = CARTESIAN_POINT('Ctrl Pts',(18.388566797702,-8.6871599391645,-14.1913380652936)) ;
#37201 = CARTESIAN_POINT('Ctrl Pts',(18.2627932302902,-8.94854526859602,-14.1986920259333)) ;
#37202 = CARTESIAN_POINT('Ctrl Pts',(18.1314964185826,-9.20710722651393,-14.2060611019251)) ;
#37203 = CARTESIAN_POINT('Origin',(0.,0.,5.8748638224677)) ;
#37204 = CARTESIAN_POINT('',(18.13149644046,-9.20710718343108,-18.0177676543358)) ;
#37205 = CARTESIAN_POINT('',(18.1314964193088,-9.20710722508389,-17.3804829809499)) ;
#37206 = CARTESIAN_POINT('',(18.1314964405232,-9.20710718330643,5.8748638224677)) ;
#37207 = CARTESIAN_POINT('Ctrl Pts',(18.1314964403967,-9.20710718355568,-18.0177676543358)) ;
#37208 = CARTESIAN_POINT('Ctrl Pts',(18.2848468652002,-8.90511518693541,-18.0092111172447)) ;
#37209 = CARTESIAN_POINT('Ctrl Pts',(18.4306320472352,-8.59933220051178,-18.0007113518994)) ;
#37210 = CARTESIAN_POINT('Ctrl Pts',(18.7638970465689,-7.85285814102169,-17.9804530256096)) ;
#37211 = CARTESIAN_POINT('Ctrl Pts',(18.9435802765869,-7.40891258858516,-17.9687815480159)) ;
#37212 = CARTESIAN_POINT('Ctrl Pts',(19.3470444774742,-6.30112102115447,-17.9401413350593)) ;
#37213 = CARTESIAN_POINT('Ctrl Pts',(19.552520645194,-5.63126910593042,-17.9232272954833)) ;
#37214 = CARTESIAN_POINT('Ctrl Pts',(19.8629563074807,-4.39489182516919,-17.8920606974358)) ;
#37215 = CARTESIAN_POINT('Ctrl Pts',(19.9791952998858,-3.83195181331826,-17.8778928539826)) ;
#37216 = CARTESIAN_POINT('Ctrl Pts',(20.188971113737,-2.5423051834774,-17.845291702278)) ;
#37217 = CARTESIAN_POINT('Ctrl Pts',(20.2673987781289,-1.81394643648051,-17.8267682718461)) ;
#37218 = CARTESIAN_POINT('Ctrl Pts',(20.3347660057942,-0.550749519922652,
-17.7945919644321)) ;
#37219 = CARTESIAN_POINT('Ctrl Pts',(20.3422153178882,-0.0176339134709528,
-17.7810031462317)) ;
#37220 = CARTESIAN_POINT('Ctrl Pts',(20.3197651828203,0.868274262940604,-17.7586129470385)) ;
#37221 = CARTESIAN_POINT('Ctrl Pts',(20.3016175165226,1.2211018192908,-17.7497507102282)) ;
#37222 = CARTESIAN_POINT('Ctrl Pts',(20.2382467390559,2.03773712335482,-17.7294688738315)) ;
#37223 = CARTESIAN_POINT('Ctrl Pts',(20.1862554309954,2.50082003081712,-17.718112778665)) ;
#37224 = CARTESIAN_POINT('Ctrl Pts',(20.0163339745423,3.6550682917691,-17.6897704054366)) ;
#37225 = CARTESIAN_POINT('Ctrl Pts',(19.878486812409,4.34268479864119,-17.6728411930499)) ;
#37226 = CARTESIAN_POINT('Ctrl Pts',(19.563466074364,5.57881594977015,-17.6416532069444)) ;
#37227 = CARTESIAN_POINT('Ctrl Pts',(19.3979640233866,6.12954941964333,-17.6274794100156)) ;
#37228 = CARTESIAN_POINT('Ctrl Pts',(18.9681516648124,7.36692435238321,-17.5947961003701)) ;
#37229 = CARTESIAN_POINT('Ctrl Pts',(18.6894740988052,8.04772603605271,-17.5761943392817)) ;
#37230 = CARTESIAN_POINT('Ctrl Pts',(18.1470175588704,9.19183408402059,-17.543986951799)) ;
#37231 = CARTESIAN_POINT('Ctrl Pts',(17.9007695949262,9.66263470761095,-17.5304460421146)) ;
#37232 = CARTESIAN_POINT('Ctrl Pts',(17.4607713559866,10.4291839844668,-17.5081160409011)) ;
#37233 = CARTESIAN_POINT('Ctrl Pts',(17.2772359495011,10.7304957492154,-17.4992665526856)) ;
#37234 = CARTESIAN_POINT('Ctrl Pts',(16.833278221658,11.4184000387083,-17.4789946898218)) ;
#37235 = CARTESIAN_POINT('Ctrl Pts',(16.5672188229569,11.8011177901146,-17.4676360429288)) ;
#37236 = CARTESIAN_POINT('Ctrl Pts',(15.8689611111785,12.7353266029941,-17.4393029863442)) ;
#37237 = CARTESIAN_POINT('Ctrl Pts',(15.4209771907138,13.274258250832,-17.4223852617783)) ;
#37238 = CARTESIAN_POINT('Ctrl Pts',(14.5564391609998,14.2113426630041,-17.3912133366882)) ;
#37239 = CARTESIAN_POINT('Ctrl Pts',(14.1490707226599,14.6169754436214,-17.3770439105198)) ;
#37240 = CARTESIAN_POINT('Ctrl Pts',(13.1836889780527,15.5000214367709,-17.3443994401186)) ;
#37241 = CARTESIAN_POINT('Ctrl Pts',(12.6159023526168,15.9655664468605,-17.3258330622126)) ;
#37242 = CARTESIAN_POINT('Ctrl Pts',(11.5952137037948,16.7139455775033,-17.2936394725038)) ;
#37243 = CARTESIAN_POINT('Ctrl Pts',(11.1540431690795,17.0115337359609,-17.2800766824873)) ;
#37244 = CARTESIAN_POINT('Ctrl Pts',(10.4015872509112,17.4772293666899,-17.2577194222446)) ;
#37245 = CARTESIAN_POINT('Ctrl Pts',(10.0966729479995,17.6551342450156,-17.2488643357817)) ;
#37246 = CARTESIAN_POINT('Ctrl Pts',(9.37887939602634,18.0492571050063,-17.2285881849787)) ;
#37247 = CARTESIAN_POINT('Ctrl Pts',(8.96289090314646,18.2593990295814,-17.217230766666)) ;
#37248 = CARTESIAN_POINT('Ctrl Pts',(7.90421558549184,18.7492991810976,-17.1888924321946)) ;
#37249 = CARTESIAN_POINT('Ctrl Pts',(7.2536011695045,19.0104737732274,-17.1719684103905)) ;
#37250 = CARTESIAN_POINT('Ctrl Pts',(6.04710580231004,19.4238206106951,-17.1407877182251)) ;
#37251 = CARTESIAN_POINT('Ctrl Pts',(5.49575524182426,19.5869589809446,-17.1266159344591)) ;
#37252 = CARTESIAN_POINT('Ctrl Pts',(4.22605273264442,19.9048099806835,-17.0939578919097)) ;
#37253 = CARTESIAN_POINT('Ctrl Pts',(3.50473852120334,20.0443950885938,-17.0753800291579)) ;
#37254 = CARTESIAN_POINT('Ctrl Pts',(2.25077640559223,20.2172863225218,-17.0431821328598)) ;
#37255 = CARTESIAN_POINT('Ctrl Pts',(1.72144134674525,20.2692205531145,-17.0296266179625)) ;
#37256 = CARTESIAN_POINT('Ctrl Pts',(0.83839413705373,20.3210140914646,-17.007278290098)) ;
#37257 = CARTESIAN_POINT('Ctrl Pts',(0.485625654000585,20.3325033459276,-16.9984249392236)) ;
#37258 = CARTESIAN_POINT('Ctrl Pts',(-0.333192031165951,20.3378480682913,
-16.9781500585281)) ;
#37259 = CARTESIAN_POINT('Ctrl Pts',(-0.799086858003867,20.3248750713429,
-16.9667921908016)) ;
#37260 = CARTESIAN_POINT('Ctrl Pts',(-1.96327042406237,20.2523641561014,-16.9384561726787)) ;
#37261 = CARTESIAN_POINT('Ctrl Pts',(-2.65969615688901,20.1727216860304,-16.9215348272028)) ;
#37262 = CARTESIAN_POINT('Ctrl Pts',(-3.91744974358327,19.9626109331623,-16.8903578417404)) ;
#37263 = CARTESIAN_POINT('Ctrl Pts',(-4.48000617322129,19.8439357121956,-16.8761870400015)) ;
#37264 = CARTESIAN_POINT('Ctrl Pts',(-5.74801992083268,19.5197638994597,-16.8435310805167)) ;
#37265 = CARTESIAN_POINT('Ctrl Pts',(-6.44888974641509,19.299552358675,-16.8249543236513)) ;
#37266 = CARTESIAN_POINT('Ctrl Pts',(-7.63419518228278,18.8553376330106,-16.7927567110361)) ;
#37267 = CARTESIAN_POINT('Ctrl Pts',(-8.12457243802752,18.6492899999245,-16.7792003641962)) ;
#37268 = CARTESIAN_POINT('Ctrl Pts',(-8.92604162034029,18.2749090635845,-16.7568511177691)) ;
#37269 = CARTESIAN_POINT('Ctrl Pts',(-9.24183490843041,18.1172573522834,-16.7479976670987)) ;
#37270 = CARTESIAN_POINT('Ctrl Pts',(-9.96468169632983,17.7325744260933,-16.7277227606743)) ;
#37271 = CARTESIAN_POINT('Ctrl Pts',(-10.3683523476635,17.4996100578037,-16.7163649739773)) ;
#37272 = CARTESIAN_POINT('Ctrl Pts',(-11.3580162748056,16.8821857765042,-16.6880282482898)) ;
#37273 = CARTESIAN_POINT('Ctrl Pts',(-11.9328080695378,16.4809229434472,-16.6711061399647)) ;
#37274 = CARTESIAN_POINT('Ctrl Pts',(-12.9393567353492,15.6979396197025,-16.6399281095113)) ;
#37275 = CARTESIAN_POINT('Ctrl Pts',(-13.377803957127,15.3260110404622,-16.6257570397981)) ;
#37276 = CARTESIAN_POINT('Ctrl Pts',(-14.3390525641398,14.4378798572536,-16.5931027361268)) ;
#37277 = CARTESIAN_POINT('Ctrl Pts',(-14.8508270856633,13.9109209828762,-16.574527968869)) ;
#37278 = CARTESIAN_POINT('Ctrl Pts',(-15.6822693853246,12.956510641737,-16.5423312204117)) ;
#37279 = CARTESIAN_POINT('Ctrl Pts',(-16.0156937568029,12.5420212101978,-16.5287737317652)) ;
#37280 = CARTESIAN_POINT('Ctrl Pts',(-16.5427380143628,11.8314981870084,-16.5064229912819)) ;
#37281 = CARTESIAN_POINT('Ctrl Pts',(-16.7455754381747,11.5426270735492,-16.4975691798431)) ;
#37282 = CARTESIAN_POINT('Ctrl Pts',(-17.1985274356489,10.8604663528818,-16.4772939663375)) ;
#37283 = CARTESIAN_POINT('Ctrl Pts',(-17.442845371727,10.4635666093895,-16.4659362229455)) ;
#37284 = CARTESIAN_POINT('Ctrl Pts',(-18.0198263305446,9.44979310335126,-16.4375995299252)) ;
#37285 = CARTESIAN_POINT('Ctrl Pts',(-18.3346447889792,8.82346475836924,-16.420677411076)) ;
#37286 = CARTESIAN_POINT('Ctrl Pts',(-18.8477487508107,7.65601910921282,-16.3894993556758)) ;
#37287 = CARTESIAN_POINT('Ctrl Pts',(-19.0565762035925,7.12033405608312,-16.3753282713825)) ;
#37288 = CARTESIAN_POINT('Ctrl Pts',(-19.4798530288185,5.88185746235006,-16.3426719435368)) ;
#37289 = CARTESIAN_POINT('Ctrl Pts',(-19.6794787986084,5.17484492062462,-16.3240951064432)) ;
#37290 = CARTESIAN_POINT('Ctrl Pts',(-19.9570136934487,3.93983429351838,-16.2918975100239)) ;
#37291 = CARTESIAN_POINT('Ctrl Pts',(-20.0532006406604,3.41669948229693,-16.2783412604372)) ;
#37292 = CARTESIAN_POINT('Ctrl Pts',(-20.1789347354474,2.54108516131153,-16.2559920971618)) ;
#37293 = CARTESIAN_POINT('Ctrl Pts',(-20.219993529437,2.19052246674787,-16.2471386349231)) ;
#37294 = CARTESIAN_POINT('Ctrl Pts',(-20.2940468022163,1.37504265726054,-16.226863703197)) ;
#37295 = CARTESIAN_POINT('Ctrl Pts',(-20.3202243573513,0.909706260809126,
-16.2155058998852)) ;
#37296 = CARTESIAN_POINT('Ctrl Pts',(-20.3456859909393,-0.25647622032154,
-16.1871693611005)) ;
#37297 = CARTESIAN_POINT('Ctrl Pts',(-20.3247773694971,-0.957153370477013,
-16.1702474496231)) ;
#37298 = CARTESIAN_POINT('Ctrl Pts',(-20.2209709212091,-2.22813658621772,
-16.1390696877212)) ;
#37299 = CARTESIAN_POINT('Ctrl Pts',(-20.1499294262565,-2.79867716241515,
-16.1248986860191)) ;
#37300 = CARTESIAN_POINT('Ctrl Pts',(-19.9333331497246,-4.0893855548962,-16.0922437421317)) ;
#37301 = CARTESIAN_POINT('Ctrl Pts',(-19.7727361782618,-4.80621818148921,
-16.0736682433026)) ;
#37302 = CARTESIAN_POINT('Ctrl Pts',(-19.4295863565967,-6.02460765284369,
-16.04147118245)) ;
#37303 = CARTESIAN_POINT('Ctrl Pts',(-19.2654172270123,-6.53057607672751,
-16.0279141190136)) ;
#37304 = CARTESIAN_POINT('Ctrl Pts',(-18.9596145754748,-7.36067537038867,
-16.0055639303227)) ;
#37305 = CARTESIAN_POINT('Ctrl Pts',(-18.8290211989872,-7.68859503422874,
-15.9967102488269)) ;
#37306 = CARTESIAN_POINT('Ctrl Pts',(-18.5063625802065,-8.44118594288248,
-15.9764351443152)) ;
#37307 = CARTESIAN_POINT('Ctrl Pts',(-18.308101698657,-8.86298447241692,-15.9650773834482)) ;
#37308 = CARTESIAN_POINT('Ctrl Pts',(-17.7759216759422,-9.90097661245427,
-15.9367406980118)) ;
#37309 = CARTESIAN_POINT('Ctrl Pts',(-17.4243187346176,-10.5074185766589,
-15.9198186034857)) ;
#37310 = CARTESIAN_POINT('Ctrl Pts',(-16.7285807071223,-11.5761327112718,
-15.8886405851111)) ;
#37311 = CARTESIAN_POINT('Ctrl Pts',(-16.3947644575661,-12.0442497277268,
-15.8744695131932)) ;
#37312 = CARTESIAN_POINT('Ctrl Pts',(-15.590413801362,-13.0766922488291,-15.841813854104)) ;
#37313 = CARTESIAN_POINT('Ctrl Pts',(-15.1082310161832,-13.6309289022104,
-15.8232376928488)) ;
#37314 = CARTESIAN_POINT('Ctrl Pts',(-14.226951014899,-14.5395519675784,-15.7910403720142)) ;
#37315 = CARTESIAN_POINT('Ctrl Pts',(-13.8419307099823,-14.9065644024412,
-15.77748371656)) ;
#37316 = CARTESIAN_POINT('Ctrl Pts',(-13.1781802256053,-15.4913553272338,
-15.7551340377466)) ;
#37317 = CARTESIAN_POINT('Ctrl Pts',(-12.9073594749646,-15.717716165862,-15.7462804621722)) ;
#37318 = CARTESIAN_POINT('Ctrl Pts',(-12.2656279341798,-16.2263196210202,
-15.7260054394226)) ;
#37319 = CARTESIAN_POINT('Ctrl Pts',(-11.8906328554521,-16.5030885853016,
-15.7146476560595)) ;
#37320 = CARTESIAN_POINT('Ctrl Pts',(-10.928865679103,-17.1631179494164,-15.6863110620378)) ;
#37321 = CARTESIAN_POINT('Ctrl Pts',(-10.3311750509017,-17.5293908635168,
-15.6693890777624)) ;
#37322 = CARTESIAN_POINT('Ctrl Pts',(-9.21092100351927,-18.1386656973709,
-15.6382112130951)) ;
#37323 = CARTESIAN_POINT('Ctrl Pts',(-8.69465526530311,-18.3917160953206,
-15.6240401826759)) ;
#37324 = CARTESIAN_POINT('Ctrl Pts',(-7.49610980689216,-18.9174312803453,
-15.5913848054304)) ;
#37325 = CARTESIAN_POINT('Ctrl Pts',(-6.80838122351373,-19.1756824678193,
-15.5728088905757)) ;
#37326 = CARTESIAN_POINT('Ctrl Pts',(-5.60103778724539,-19.5558965179745,
-15.5406116637739)) ;
#37327 = CARTESIAN_POINT('Ctrl Pts',(-5.08780149689677,-19.6956591742904,
-15.5270548538831)) ;
#37328 = CARTESIAN_POINT('Ctrl Pts',(-4.22580343339836,-19.8944492327781,
-15.5047049842164)) ;
#37329 = CARTESIAN_POINT('Ctrl Pts',(-3.8799182677934,-19.9647881361655,-15.4958513706128)) ;
#37330 = CARTESIAN_POINT('Ctrl Pts',(-3.07352708276674,-20.1070263322599,
-15.4755763194249)) ;
#37331 = CARTESIAN_POINT('Ctrl Pts',(-2.61203116819607,-20.172168334746,-15.4642185452072)) ;
#37332 = CARTESIAN_POINT('Ctrl Pts',(-1.45209688915559,-20.2954216622683,
-15.4358819073146)) ;
#37333 = CARTESIAN_POINT('Ctrl Pts',(-0.752131972562254,-20.3333967285738,
-15.4189598717337)) ;
#37334 = CARTESIAN_POINT('Ctrl Pts',(0.523086470668565,-20.3366329681707,
-15.3877819358679)) ;
#37335 = CARTESIAN_POINT('Ctrl Pts',(1.09757853848662,-20.3137286924139,-15.3736108864778)) ;
#37336 = CARTESIAN_POINT('Ctrl Pts',(2.4019320821558,-20.2062266049689,-15.3409554422)) ;
#37337 = CARTESIAN_POINT('Ctrl Pts',(3.12973246549749,-20.1063579631095,-15.3223794783815)) ;
#37338 = CARTESIAN_POINT('Ctrl Pts',(4.37263038854816,-19.866675994929,-15.2901822347595)) ;
#37339 = CARTESIAN_POINT('Ctrl Pts',(4.8905815211749,-19.7455545744569,-15.2766254574297)) ;
#37340 = CARTESIAN_POINT('Ctrl Pts',(5.74340477639792,-19.5105055379013,-15.2542756265258)) ;
#37341 = CARTESIAN_POINT('Ctrl Pts',(6.08112553807109,-19.4078964113495,-15.2454220195245)) ;
#37342 = CARTESIAN_POINT('Ctrl Pts',(6.85814013758017,-19.1495428304986,-15.2251469726107)) ;
#37343 = CARTESIAN_POINT('Ctrl Pts',(7.29509134239601,-18.9873832995528,-15.2137891960326)) ;
#37344 = CARTESIAN_POINT('Ctrl Pts',(8.37408516501341,-18.5442018549637,-15.1854525737386)) ;
#37345 = CARTESIAN_POINT('Ctrl Pts',(9.00789491764561,-18.2447404240817,-15.1685305555329)) ;
#37346 = CARTESIAN_POINT('Ctrl Pts',(10.1312286204141,-17.6411583030212,-15.1373526435956)) ;
#37347 = CARTESIAN_POINT('Ctrl Pts',(10.625710614469,-17.3478103998223,-15.1231816004402)) ;
#37348 = CARTESIAN_POINT('Ctrl Pts',(11.7220139194575,-16.6329571072558,-15.0905261431185)) ;
#37349 = CARTESIAN_POINT('Ctrl Pts',(12.3147600163876,-16.1989982006957,-15.0719501592592)) ;
#37350 = CARTESIAN_POINT('Ctrl Pts',(13.2941431665818,-15.3970928621927,-15.0397529063177)) ;
#37351 = CARTESIAN_POINT('Ctrl Pts',(13.6921794945441,-15.0442325592076,-15.0261961398718)) ;
#37352 = CARTESIAN_POINT('Ctrl Pts',(14.3306208199668,-14.4319032553308,-15.0038463237411)) ;
#37353 = CARTESIAN_POINT('Ctrl Pts',(14.5789142184307,-14.1810363169254,-14.9949927206885)) ;
#37354 = CARTESIAN_POINT('Ctrl Pts',(15.1395853811299,-13.584256742991,-14.9747176773215)) ;
#37355 = CARTESIAN_POINT('Ctrl Pts',(15.4468516640989,-13.2338148669836,-14.9633599004859)) ;
#37356 = CARTESIAN_POINT('Ctrl Pts',(16.1852759965221,-12.3308380024637,-14.9350232755944)) ;
#37357 = CARTESIAN_POINT('Ctrl Pts',(16.600422774887,-11.7659971027763,-14.9181012551279)) ;
#37358 = CARTESIAN_POINT('Ctrl Pts',(17.3015739403144,-10.7008316898369,-14.8869233402179)) ;
#37359 = CARTESIAN_POINT('Ctrl Pts',(17.5970628635087,-10.2076260875571,-14.8727522963968)) ;
#37360 = CARTESIAN_POINT('Ctrl Pts',(17.9602893881657,-9.538595533303,-14.8537576929866)) ;
#37361 = CARTESIAN_POINT('Ctrl Pts',(18.0470410689725,-9.37342459922203,-14.8490868914772)) ;
#37362 = CARTESIAN_POINT('Ctrl Pts',(18.1314964554037,-9.20710715400241,-14.8444016794283)) ;
#37363 = CARTESIAN_POINT('Ctrl Pts',(18.1314964185826,-9.20710722651395,-14.2060611019251)) ;
#37364 = CARTESIAN_POINT('Ctrl Pts',(17.9358763267721,-9.59234060186247,-14.2170403428017)) ;
#37365 = CARTESIAN_POINT('Ctrl Pts',(17.7279956224823,-9.97130655589842,-14.2280546280103)) ;
#37366 = CARTESIAN_POINT('Ctrl Pts',(17.284148524616,-10.7226001072057,-14.2502160005134)) ;
#37367 = CARTESIAN_POINT('Ctrl Pts',(17.047877993267,-11.0944041437719,-14.2613538164525)) ;
#37368 = CARTESIAN_POINT('Ctrl Pts',(16.5926782493387,-11.7618038366014,-14.2814944671437)) ;
#37369 = CARTESIAN_POINT('Ctrl Pts',(16.3774457319728,-12.059696215226,-14.290527048049)) ;
#37370 = CARTESIAN_POINT('Ctrl Pts',(15.7985717768379,-12.8167872494878,-14.3138008947374)) ;
#37371 = CARTESIAN_POINT('Ctrl Pts',(15.4229541086325,-13.2664010149578,-14.3279500499567)) ;
#37372 = CARTESIAN_POINT('Ctrl Pts',(14.5504153941473,-14.2236052365707,-14.359401565525)) ;
#37373 = CARTESIAN_POINT('Ctrl Pts',(14.0452548052217,-14.7226472103789,-14.3767231881684)) ;
#37374 = CARTESIAN_POINT('Ctrl Pts',(13.0627935843752,-15.5965305615437,-14.409314660392)) ;
#37375 = CARTESIAN_POINT('Ctrl Pts',(12.5928090209797,-15.9784070825999,-14.4244915076494)) ;
#37376 = CARTESIAN_POINT('Ctrl Pts',(11.4225885965584,-16.8455034298845,-14.461340489271)) ;
#37377 = CARTESIAN_POINT('Ctrl Pts',(10.7075407047529,-17.3088151129628,-14.4831295564706)) ;
#37378 = CARTESIAN_POINT('Ctrl Pts',(9.66356012251429,-17.895743379507,-14.5133717407458)) ;
#37379 = CARTESIAN_POINT('Ctrl Pts',(9.35725611455952,-18.0577902677465,-14.5220572295973)) ;
#37380 = CARTESIAN_POINT('Ctrl Pts',(8.48808657723682,-18.489558794215,-14.5460753687141)) ;
#37381 = CARTESIAN_POINT('Ctrl Pts',(7.91672812828408,-18.7413133345442,-14.5612049193879)) ;
#37382 = CARTESIAN_POINT('Ctrl Pts',(6.50440272820335,-19.2874886385148,-14.5979300476961)) ;
#37383 = CARTESIAN_POINT('Ctrl Pts',(5.65392662827631,-19.5537099908529,-14.6195197088102)) ;
#37384 = CARTESIAN_POINT('Ctrl Pts',(4.22385052510927,-19.900224159471,-14.6559337505174)) ;
#37385 = CARTESIAN_POINT('Ctrl Pts',(3.65334484369751,-20.0128183289596,-14.6704765150215)) ;
#37386 = CARTESIAN_POINT('Ctrl Pts',(2.36016473251122,-20.2108923170943,-14.7035166569855)) ;
#37387 = CARTESIAN_POINT('Ctrl Pts',(1.63613970786653,-20.2823466401737,-14.7220750538599)) ;
#37388 = CARTESIAN_POINT('Ctrl Pts',(0.450302395088354,-20.3354572780443,
-14.7522166891377)) ;
#37389 = CARTESIAN_POINT('Ctrl Pts',(-0.00981580338987972,-20.3404401002588,
-14.7638441743822)) ;
#37390 = CARTESIAN_POINT('Ctrl Pts',(-0.878733626513398,-20.3203642717784,
-14.7854707490982)) ;
#37391 = CARTESIAN_POINT('Ctrl Pts',(-1.28738263790034,-20.2985720133255,
-14.7954953941133)) ;
#37392 = CARTESIAN_POINT('Ctrl Pts',(-2.96347683346068,-20.1583688742635,
-14.8364751683913)) ;
#37393 = CARTESIAN_POINT('Ctrl Pts',(-4.21909058816922,-19.9334220812544,
-14.8670412017991)) ;
#37394 = CARTESIAN_POINT('Ctrl Pts',(-6.06689801808748,-19.4198559139412,
-14.9146618712423)) ;
#37395 = CARTESIAN_POINT('Ctrl Pts',(-6.67980000883116,-19.217656347121,-14.9308780736159)) ;
#37396 = CARTESIAN_POINT('Ctrl Pts',(-8.02273855991015,-18.7025927007995,
-14.9673419798132)) ;
#37397 = CARTESIAN_POINT('Ctrl Pts',(-8.74616799484573,-18.3754142924498,
-14.9876378056753)) ;
#37398 = CARTESIAN_POINT('Ctrl Pts',(-9.74526611379734,-17.851162276582,-15.0160952926151)) ;
#37399 = CARTESIAN_POINT('Ctrl Pts',(-10.0380131877422,-17.6882023680529,
-15.0244790979386)) ;
#37400 = CARTESIAN_POINT('Ctrl Pts',(-10.8346760546563,-17.2185834688636,
-15.0473402724233)) ;
#37401 = CARTESIAN_POINT('Ctrl Pts',(-11.3294809836519,-16.8971208228581,
-15.0616477938207)) ;
#37402 = CARTESIAN_POINT('Ctrl Pts',(-12.5504129673034,-16.0261404239907,
-15.0980235895946)) ;
#37403 = CARTESIAN_POINT('Ctrl Pts',(-13.2548979994215,-15.4485503999224,
-15.120081495915)) ;
#37404 = CARTESIAN_POINT('Ctrl Pts',(-14.3429776035582,-14.4270662107565,
-15.1570181236818)) ;
#37405 = CARTESIAN_POINT('Ctrl Pts',(-14.7503019787096,-14.0103471988409,
-15.1715930934248)) ;
#37406 = CARTESIAN_POINT('Ctrl Pts',(-15.627842607075,-13.0318165116084,-15.2047913792323)) ;
#37407 = CARTESIAN_POINT('Ctrl Pts',(-16.0867349806377,-12.4609251806071,
-15.2234776101177)) ;
#37408 = CARTESIAN_POINT('Ctrl Pts',(-16.7781755725741,-11.4986952782749,
-15.2535598154692)) ;
#37409 = CARTESIAN_POINT('Ctrl Pts',(-17.0301419704014,-11.1221148098039,
-15.2650059803411)) ;
#37410 = CARTESIAN_POINT('Ctrl Pts',(-17.4870978845055,-10.3871794541201,
-15.2865369525305)) ;
#37411 = CARTESIAN_POINT('Ctrl Pts',(-17.6941678523924,-10.0303796837544,
-15.2966403326889)) ;
#37412 = CARTESIAN_POINT('Ctrl Pts',(-18.4874191611665,-8.56242856749256,
-15.337288239056)) ;
#37413 = CARTESIAN_POINT('Ctrl Pts',(-18.9809131254149,-7.40437684840318,
-15.3674603915569)) ;
#37414 = CARTESIAN_POINT('Ctrl Pts',(-19.5577514721686,-5.6051262129008,-15.4143555214567)) ;
#37415 = CARTESIAN_POINT('Ctrl Pts',(-19.7228195259651,-4.9933417024841,-15.4302663369936)) ;
#37416 = CARTESIAN_POINT('Ctrl Pts',(-20.0270799951898,-3.612193070057,-15.4661019720934)) ;
#37417 = CARTESIAN_POINT('Ctrl Pts',(-20.1510176811904,-2.84048492571852,
-15.4860772580447)) ;
#37418 = CARTESIAN_POINT('Ctrl Pts',(-20.2657464435653,-1.71573646667443,
-15.514633659491)) ;
#37419 = CARTESIAN_POINT('Ctrl Pts',(-20.2922503472445,-1.3670451592217,-15.5234019992902)) ;
#37420 = CARTESIAN_POINT('Ctrl Pts',(-20.341497512413,-0.384377930322299,
-15.5477579544355)) ;
#37421 = CARTESIAN_POINT('Ctrl Pts',(-20.3435902926221,0.250227276189321,
-15.5631321567441)) ;
#37422 = CARTESIAN_POINT('Ctrl Pts',(-20.2776451958704,1.76595391228162,-15.5999271289221)) ;
#37423 = CARTESIAN_POINT('Ctrl Pts',(-20.181866006293,2.64457186147614,-15.6213430419292)) ;
#37424 = CARTESIAN_POINT('Ctrl Pts',(-19.9289262116076,4.08621997057266,-15.6575629482805)) ;
#37425 = CARTESIAN_POINT('Ctrl Pts',(-19.8041002585643,4.65369721003538,-15.6720933342683)) ;
#37426 = CARTESIAN_POINT('Ctrl Pts',(-19.4691943455686,5.91593452280017,-15.705072745162)) ;
#37427 = CARTESIAN_POINT('Ctrl Pts',(-19.2458740792131,6.60637065508469,-15.7235820634347)) ;
#37428 = CARTESIAN_POINT('Ctrl Pts',(-18.8297569377225,7.69109339204809,-15.7530850757679)) ;
#37429 = CARTESIAN_POINT('Ctrl Pts',(-18.6602652571632,8.0936498854933,-15.7641264675232)) ;
#37430 = CARTESIAN_POINT('Ctrl Pts',(-18.3238657942352,8.82576408561461,-15.7842115842327)) ;
#37431 = CARTESIAN_POINT('Ctrl Pts',(-18.1606874541884,9.15683357519549,-15.7932817966719)) ;
#37432 = CARTESIAN_POINT('Ctrl Pts',(-17.7127060980746,10.0065979909938,-15.8167382137131)) ;
#37433 = CARTESIAN_POINT('Ctrl Pts',(-17.414115835438,10.517629680803,-15.8310305102049)) ;
#37434 = CARTESIAN_POINT('Ctrl Pts',(-16.7100989795109,11.6101693347247,-15.862595529692)) ;
#37435 = CARTESIAN_POINT('Ctrl Pts',(-16.2956986105653,12.1849758283577,-15.8798864139723)) ;
#37436 = CARTESIAN_POINT('Ctrl Pts',(-15.4697779922949,13.2128975311609,-15.9125799145422)) ;
#37437 = CARTESIAN_POINT('Ctrl Pts',(-15.0661586634025,13.6713402910528,-15.9278938183899)) ;
#37438 = CARTESIAN_POINT('Ctrl Pts',(-14.2176386588299,14.5518268088224,-15.9588410428491)) ;
#37439 = CARTESIAN_POINT('Ctrl Pts',(-13.7730493294221,14.9733102931769,-15.9744590929112)) ;
#37440 = CARTESIAN_POINT('Ctrl Pts',(-12.9622391298698,15.6752695819456,-16.0017088370085)) ;
#37441 = CARTESIAN_POINT('Ctrl Pts',(-12.6042300423405,15.9645579075918,-16.0133558358841)) ;
#37442 = CARTESIAN_POINT('Ctrl Pts',(-11.9490623645648,16.4581775406919,-16.0338162517828)) ;
#37443 = CARTESIAN_POINT('Ctrl Pts',(-11.6557030213528,16.6672219255522,-16.0426762000691)) ;
#37444 = CARTESIAN_POINT('Ctrl Pts',(-10.8937479261421,17.1802226536296,-16.0651197441503)) ;
#37445 = CARTESIAN_POINT('Ctrl Pts',(-10.4178990008301,17.4728697796118,-16.0786195188759)) ;
#37446 = CARTESIAN_POINT('Ctrl Pts',(-9.31625051688439,18.0893642552714,-16.109259619691)) ;
#37447 = CARTESIAN_POINT('Ctrl Pts',(-8.68445642331316,18.4010279577892,-16.1264189439552)) ;
#37448 = CARTESIAN_POINT('Ctrl Pts',(-7.50545867371461,18.9083554803841,-16.158177454499)) ;
#37449 = CARTESIAN_POINT('Ctrl Pts',(-6.96359604916064,19.114553046566,-16.1726739943814)) ;
#37450 = CARTESIAN_POINT('Ctrl Pts',(-5.73042922750216,19.5244091944784,-16.2054874926823)) ;
#37451 = CARTESIAN_POINT('Ctrl Pts',(-5.03560946930113,19.7150451019282,-16.2238627660137)) ;
#37452 = CARTESIAN_POINT('Ctrl Pts',(-3.89887327313653,19.962901286656,-16.2534127738905)) ;
#37453 = CARTESIAN_POINT('Ctrl Pts',(-3.46261862467731,20.0431763198624,-16.2646292945534)) ;
#37454 = CARTESIAN_POINT('Ctrl Pts',(-2.66195517821135,20.1635831616703,-16.2848166102783)) ;
#37455 = CARTESIAN_POINT('Ctrl Pts',(-2.29841784722897,20.208249977966,-16.2938197889457)) ;
#37456 = CARTESIAN_POINT('Ctrl Pts',(-1.35557703796695,20.2983219725844,-16.3169514223199)) ;
#37457 = CARTESIAN_POINT('Ctrl Pts',(-0.775178092395972,20.3287620541768,
-16.330989172813)) ;
#37458 = CARTESIAN_POINT('Ctrl Pts',(0.525800891148537,20.3411915233625,-16.3625793739936)) ;
#37459 = CARTESIAN_POINT('Ctrl Pts',(1.24572608182642,20.3098176921019,-16.3801545596301)) ;
#37460 = CARTESIAN_POINT('Ctrl Pts',(2.56729544218104,20.1816808104442,-16.4130698324889)) ;
#37461 = CARTESIAN_POINT('Ctrl Pts',(3.16918972236981,20.0959566274744,-16.4283095354248)) ;
#37462 = CARTESIAN_POINT('Ctrl Pts',(4.18186173607639,19.9050951551573,-16.4543855016734)) ;
#37463 = CARTESIAN_POINT('Ctrl Pts',(4.59484272414636,19.813838585845,-16.465142037111)) ;
#37464 = CARTESIAN_POINT('Ctrl Pts',(5.61952630538609,19.5536524456278,-16.4920474314851)) ;
#37465 = CARTESIAN_POINT('Ctrl Pts',(6.22673658324856,19.3688450435273,-16.5081937605405)) ;
#37466 = CARTESIAN_POINT('Ctrl Pts',(7.14603656153679,19.0413441848069,-16.532570000997)) ;
#37467 = CARTESIAN_POINT('Ctrl Pts',(7.46481913699451,18.9186443007041,-16.5409909522811)) ;
#37468 = CARTESIAN_POINT('Ctrl Pts',(8.23303242687312,18.6005165280536,-16.5613401997083)) ;
#37469 = CARTESIAN_POINT('Ctrl Pts',(8.67878310928617,18.396759633008,-16.5732066521846)) ;
#37470 = CARTESIAN_POINT('Ctrl Pts',(9.83717795615027,17.8157657972116,-16.6046367772584)) ;
#37471 = CARTESIAN_POINT('Ctrl Pts',(10.5354919712934,17.411920592555,-16.6242230332246)) ;
#37472 = CARTESIAN_POINT('Ctrl Pts',(11.6889518512255,16.6500043968405,-16.6584186308077)) ;
#37473 = CARTESIAN_POINT('Ctrl Pts',(12.1561838820426,16.3120025311964,-16.6728327672675)) ;
#37474 = CARTESIAN_POINT('Ctrl Pts',(13.1635063121564,15.5159476804399,-16.7052429806693)) ;
#37475 = CARTESIAN_POINT('Ctrl Pts',(13.6953179463166,15.0486142157575,-16.723292591908)) ;
#37476 = CARTESIAN_POINT('Ctrl Pts',(14.5312812685789,14.2329165126168,-16.7529699546142)) ;
#37477 = CARTESIAN_POINT('Ctrl Pts',(14.8498581943657,13.9002073291417,-16.76462614677)) ;
#37478 = CARTESIAN_POINT('Ctrl Pts',(15.3968959495581,13.2886120721922,-16.7850927101015)) ;
#37479 = CARTESIAN_POINT('Ctrl Pts',(15.6297567451281,13.0139279257207,-16.7939499098735)) ;
#37480 = CARTESIAN_POINT('Ctrl Pts',(16.2045818323457,12.2981641541507,-16.8163803002743)) ;
#37481 = CARTESIAN_POINT('Ctrl Pts',(16.5359090602219,11.8489252294761,-16.8298698029265)) ;
#37482 = CARTESIAN_POINT('Ctrl Pts',(17.2428671739373,10.8028674754818,-16.8605128805814)) ;
#37483 = CARTESIAN_POINT('Ctrl Pts',(17.606783170301,10.1989995034871,-16.8776855894045)) ;
#37484 = CARTESIAN_POINT('Ctrl Pts',(18.2115370599317,9.06629390603653,-16.9094568234527)) ;
#37485 = CARTESIAN_POINT('Ctrl Pts',(18.4624773590473,8.54369289445659,-16.9239522237103)) ;
#37486 = CARTESIAN_POINT('Ctrl Pts',(18.9743287038201,7.3494878938411,-16.9567600995734)) ;
#37487 = CARTESIAN_POINT('Ctrl Pts',(19.2225720434545,6.67329294055859,-16.9751308228226)) ;
#37488 = CARTESIAN_POINT('Ctrl Pts',(19.56503125503,5.56133073220388,-17.0046824935636)) ;
#37489 = CARTESIAN_POINT('Ctrl Pts',(19.6817127130537,5.13313124283561,-17.0159050304079)) ;
#37490 = CARTESIAN_POINT('Ctrl Pts',(19.8689376607649,4.34526619725645,-17.0360959193856)) ;
#37491 = CARTESIAN_POINT('Ctrl Pts',(19.943946782144,3.98685456518818,-17.045096856844)) ;
#37492 = CARTESIAN_POINT('Ctrl Pts',(20.1127798097398,3.05534630776733,-17.0682176846032)) ;
#37493 = CARTESIAN_POINT('Ctrl Pts',(20.1918083544377,2.47990560977458,-17.0822469775228)) ;
#37494 = CARTESIAN_POINT('Ctrl Pts',(20.3136472950072,1.18288690624342,-17.1138780036046)) ;
#37495 = CARTESIAN_POINT('Ctrl Pts',(20.3428395797298,0.460819480629736,-17.1315030976438)) ;
#37496 = CARTESIAN_POINT('Ctrl Pts',(20.3257407620204,-0.869940269848479,
-17.1644971582826)) ;
#37497 = CARTESIAN_POINT('Ctrl Pts',(20.2905933221345,-1.47795339420346,-17.1797646295784)) ;
#37498 = CARTESIAN_POINT('Ctrl Pts',(20.1846674587742,-2.50637917286517,-17.2059274371778)) ;
#37499 = CARTESIAN_POINT('Ctrl Pts',(20.1278565607367,-2.92781927268253,-17.2167434211728)) ;
#37500 = CARTESIAN_POINT('Ctrl Pts',(19.9546686600175,-3.96564670157676,-17.2435209473983)) ;
#37501 = CARTESIAN_POINT('Ctrl Pts',(19.8229083481296,-4.57902462313986,-17.2594786405501)) ;
#37502 = CARTESIAN_POINT('Ctrl Pts',(19.576353644806,-5.51397105890394,-17.2836342401105)) ;
#37503 = CARTESIAN_POINT('Ctrl Pts',(19.4814636605641,-5.84038291029885,-17.292016445134)) ;
#37504 = CARTESIAN_POINT('Ctrl Pts',(19.2317827409194,-6.62529842866866,-17.3121781252484)) ;
#37505 = CARTESIAN_POINT('Ctrl Pts',(19.0687213537764,-7.08095443782718,-17.323897830387)) ;
#37506 = CARTESIAN_POINT('Ctrl Pts',(18.6622661199277,-8.10052863368516,-17.3505173436298)) ;
#37507 = CARTESIAN_POINT('Ctrl Pts',(18.4093092976805,-8.66001212927637,-17.3654140700582)) ;
#37508 = CARTESIAN_POINT('Ctrl Pts',(18.131496419296,-9.20710722510901,-17.3804829797999)) ;
#37509 = CARTESIAN_POINT('Origin',(0.,0.,-315.477129595899)) ;
#37510 = CARTESIAN_POINT('',(18.5446545942647,-0.888979967106324,-319.159121327694)) ;
#37511 = CARTESIAN_POINT('',(18.5446545937445,-0.888979977957671,-318.864005972278)) ;
#37512 = CARTESIAN_POINT('',(18.544654593745,-0.888979977948782,-315.477129595899)) ;
#37513 = CARTESIAN_POINT('',(-15.1336583262364,-10.7548540235205,-318.25)) ;
#37514 = CARTESIAN_POINT('Ctrl Pts',(18.5446545942648,-0.888979967104711,
-319.159121327827)) ;
#37515 = CARTESIAN_POINT('Ctrl Pts',(18.5602689642712,-0.563254856088902,
-319.155126550097)) ;
#37516 = CARTESIAN_POINT('Ctrl Pts',(18.5673008594752,-0.237133928660758,
-319.151136261858)) ;
#37517 = CARTESIAN_POINT('Ctrl Pts',(18.5639848688748,0.454254634712284,-319.142610920134)) ;
#37518 = CARTESIAN_POINT('Ctrl Pts',(18.5514574374049,0.819333613877284,-319.13806986498)) ;
#37519 = CARTESIAN_POINT('Ctrl Pts',(18.5180763409334,1.34179379210061,-319.131464220557)) ;
#37520 = CARTESIAN_POINT('Ctrl Pts',(18.5059617259299,1.49964744098828,-319.129454667652)) ;
#37521 = CARTESIAN_POINT('Ctrl Pts',(18.4807422496105,1.78103690751676,-319.125845180896)) ;
#37522 = CARTESIAN_POINT('Ctrl Pts',(18.4684136000839,1.90463267002766,-319.124250374317)) ;
#37523 = CARTESIAN_POINT('Ctrl Pts',(18.4390218585907,2.17208561171922,-319.120778140491)) ;
#37524 = CARTESIAN_POINT('Ctrl Pts',(18.421513417929,2.31588564456462,-319.118897916994)) ;
#37525 = CARTESIAN_POINT('Ctrl Pts',(18.3641442814051,2.74513552295158,-319.113245342165)) ;
#37526 = CARTESIAN_POINT('Ctrl Pts',(18.3193179528783,3.02987679463541,-319.10944209017)) ;
#37527 = CARTESIAN_POINT('Ctrl Pts',(18.1897974753758,3.74395388119465,-319.099785218467)) ;
#37528 = CARTESIAN_POINT('Ctrl Pts',(18.0965206139479,4.17155406676792,-319.093890983782)) ;
#37529 = CARTESIAN_POINT('Ctrl Pts',(17.8777899404563,5.02774224115309,-319.081988015267)) ;
#37530 = CARTESIAN_POINT('Ctrl Pts',(17.751807178305,5.45590580439147,-319.075983307905)) ;
#37531 = CARTESIAN_POINT('Ctrl Pts',(17.5739425268451,5.98868833864924,-319.068588741989)) ;
#37532 = CARTESIAN_POINT('Ctrl Pts',(17.5363403569636,6.09791857126738,-319.067077126615)) ;
#37533 = CARTESIAN_POINT('Ctrl Pts',(17.4768575727714,6.26560799361809,-319.064767119793)) ;
#37534 = CARTESIAN_POINT('Ctrl Pts',(17.4556975126237,6.32431960832953,-319.0639603586)) ;
#37535 = CARTESIAN_POINT('Ctrl Pts',(17.4098631644016,6.44951100624338,-319.062245298802)) ;
#37536 = CARTESIAN_POINT('Ctrl Pts',(17.3851032159711,6.51595839515908,-319.061338165955)) ;
#37537 = CARTESIAN_POINT('Ctrl Pts',(17.3158320455551,6.69865317473294,-319.058850804712)) ;
#37538 = CARTESIAN_POINT('Ctrl Pts',(17.270531439088,6.81459739623427,-319.057279814005)) ;
#37539 = CARTESIAN_POINT('Ctrl Pts',(17.1623822603318,7.08339220602497,-319.053646912958)) ;
#37540 = CARTESIAN_POINT('Ctrl Pts',(17.0986519257871,7.23587675668323,-319.051592927197)) ;
#37541 = CARTESIAN_POINT('Ctrl Pts',(16.8434926916753,7.82418213797548,-319.043664708043)) ;
#37542 = CARTESIAN_POINT('Ctrl Pts',(16.637367043777,8.25342905545798,-319.037867645929)) ;
#37543 = CARTESIAN_POINT('Ctrl Pts',(16.2040220929921,9.07347940620958,-319.026477257805)) ;
#37544 = CARTESIAN_POINT('Ctrl Pts',(15.9785784620398,9.46485021332613,-319.020892772631)) ;
#37545 = CARTESIAN_POINT('Ctrl Pts',(15.6593832850657,9.97500867674571,-319.013312424007)) ;
#37546 = CARTESIAN_POINT('Ctrl Pts',(15.5781300400181,10.1014329350564,-319.011408780047)) ;
#37547 = CARTESIAN_POINT('Ctrl Pts',(15.4256443411548,10.3324735668653,-319.007880621998)) ;
#37548 = CARTESIAN_POINT('Ctrl Pts',(15.3548597489361,10.437374927953,-319.00625960607)) ;
#37549 = CARTESIAN_POINT('Ctrl Pts',(15.2063368188461,10.6527017438039,-319.002891498421)) ;
#37550 = CARTESIAN_POINT('Ctrl Pts',(15.1284549811114,10.7630192654991,-319.001143340073)) ;
#37551 = CARTESIAN_POINT('Ctrl Pts',(14.9155173915696,11.0577614781655,-318.996411003453)) ;
#37552 = CARTESIAN_POINT('Ctrl Pts',(14.7782479870054,11.2405575529418,-318.993409718934)) ;
#37553 = CARTESIAN_POINT('Ctrl Pts',(14.5397237453007,11.5462664518458,-318.988280019695)) ;
#37554 = CARTESIAN_POINT('Ctrl Pts',(14.44019912732,11.6704963325322,-318.986163564225)) ;
#37555 = CARTESIAN_POINT('Ctrl Pts',(13.971284365632,12.2406281926226,-318.976309148053)) ;
#37556 = CARTESIAN_POINT('Ctrl Pts',(13.5827613493189,12.6703732122854,-318.968462947069)) ;
#37557 = CARTESIAN_POINT('Ctrl Pts',(12.9737467394363,13.2837425015678,-318.956878270431)) ;
#37558 = CARTESIAN_POINT('Ctrl Pts',(12.7680580198789,13.4815657209763,-318.953078519596)) ;
#37559 = CARTESIAN_POINT('Ctrl Pts',(12.4950209821368,13.7323062986608,-318.948221047424)) ;
#37560 = CARTESIAN_POINT('Ctrl Pts',(12.431752879163,13.789608623984,-318.947108093075)) ;
#37561 = CARTESIAN_POINT('Ctrl Pts',(12.3181165561857,13.8911120546022,-318.945133301297)) ;
#37562 = CARTESIAN_POINT('Ctrl Pts',(12.2678999504967,13.9354806321743,-318.944268981605)) ;
#37563 = CARTESIAN_POINT('Ctrl Pts',(12.1586034327819,14.0310002704813,-318.942406544563)) ;
#37564 = CARTESIAN_POINT('Ctrl Pts',(12.0994386529375,14.082052063953,-318.941409867692)) ;
#37565 = CARTESIAN_POINT('Ctrl Pts',(11.9152540704735,14.2389625794178,-318.938339632435)) ;
#37566 = CARTESIAN_POINT('Ctrl Pts',(11.789154102652,14.3435414247497,-318.936283455166)) ;
#37567 = CARTESIAN_POINT('Ctrl Pts',(11.2685627490624,14.7637815723509,-318.927946438416)) ;
#37568 = CARTESIAN_POINT('Ctrl Pts',(10.8626484278794,15.0649468671552,-318.921789813333)) ;
#37569 = CARTESIAN_POINT('Ctrl Pts',(10.0116776814233,15.6440235255924,-318.909170967969)) ;
#37570 = CARTESIAN_POINT('Ctrl Pts',(9.56610922093536,15.9203867673038,-318.902710439529)) ;
#37571 = CARTESIAN_POINT('Ctrl Pts',(8.97854663842178,16.2512389727499,-318.894216439311)) ;
#37572 = CARTESIAN_POINT('Ctrl Pts',(8.84675497468873,16.3233573207557,-318.892313406443)) ;
#37573 = CARTESIAN_POINT('Ctrl Pts',(8.60236262678938,16.4532632100368,-318.888785868166)) ;
#37574 = CARTESIAN_POINT('Ctrl Pts',(8.49001831243035,16.5115142256101,-318.887164852958)) ;
#37575 = CARTESIAN_POINT('Ctrl Pts',(8.25654015526587,16.629560740872,-318.883796164784)) ;
#37576 = CARTESIAN_POINT('Ctrl Pts',(8.13533149768715,16.6891919255227,-318.88204741897)) ;
#37577 = CARTESIAN_POINT('Ctrl Pts',(7.80710937199113,16.8462424234499,-318.877311822209)) ;
#37578 = CARTESIAN_POINT('Ctrl Pts',(7.59892846058663,16.9411666211697,-318.87430782646)) ;
#37579 = CARTESIAN_POINT('Ctrl Pts',(7.24283356526584,17.0956504179605,-318.869172612588)) ;
#37580 = CARTESIAN_POINT('Ctrl Pts',(7.09580967690666,17.1571963389631,-318.867053361369)) ;
#37581 = CARTESIAN_POINT('Ctrl Pts',(6.40958256758438,17.4341294800548,-318.857174597596)) ;
#37582 = CARTESIAN_POINT('Ctrl Pts',(5.86125825431229,17.6260395130887,-318.849306299)) ;
#37583 = CARTESIAN_POINT('Ctrl Pts',(5.03359195347694,17.872816540472,-318.83773199408)) ;
#37584 = CARTESIAN_POINT('Ctrl Pts',(4.76052363866778,17.9474798871337,-318.833963135922)) ;
#37585 = CARTESIAN_POINT('Ctrl Pts',(4.4029616932434,18.0365108885831,-318.829134705794)) ;
#37586 = CARTESIAN_POINT('Ctrl Pts',(4.31992687419947,18.0565785389903,-318.828020888114)) ;
#37587 = CARTESIAN_POINT('Ctrl Pts',(4.17150517814051,18.0913663271595,-318.826045092615)) ;
#37588 = CARTESIAN_POINT('Ctrl Pts',(4.10617149994144,18.1063068207655,-318.825180623535)) ;
#37589 = CARTESIAN_POINT('Ctrl Pts',(3.96454428321469,18.1378881186817,-318.823318787552)) ;
#37590 = CARTESIAN_POINT('Ctrl Pts',(3.88822389397825,18.1544019937816,-318.822322851705)) ;
#37591 = CARTESIAN_POINT('Ctrl Pts',(3.65176627396126,18.2040061762582,-318.819257085943)) ;
#37592 = CARTESIAN_POINT('Ctrl Pts',(3.4912942062205,18.2354627774394,-318.817204572854)) ;
#37593 = CARTESIAN_POINT('Ctrl Pts',(2.83382432440572,18.3553467206454,-318.808876413922)) ;
#37594 = CARTESIAN_POINT('Ctrl Pts',(2.33373384078386,18.4256072390721,-318.802725003206)) ;
#37595 = CARTESIAN_POINT('Ctrl Pts',(1.352420382488,18.5228814337528,-318.790636017191)) ;
#37596 = CARTESIAN_POINT('Ctrl Pts',(0.871773872791576,18.5517165397807,-318.784706468524)) ;
#37597 = CARTESIAN_POINT('Ctrl Pts',(0.205140700510149,18.5657428971848,-318.77633451)) ;
#37598 = CARTESIAN_POINT('Ctrl Pts',(0.0196814447135078,18.5668657698757,
-318.773990293903)) ;
#37599 = CARTESIAN_POINT('Ctrl Pts',(-0.292086859466395,18.5640820833563,
-318.770019298556)) ;
#37600 = CARTESIAN_POINT('Ctrl Pts',(-0.41839555666227,18.5616648885815,-318.768402192849)) ;
#37601 = CARTESIAN_POINT('Ctrl Pts',(-0.677301023370646,18.5540661033441,
-318.765069429211)) ;
#37602 = CARTESIAN_POINT('Ctrl Pts',(-0.809886748483699,18.5487516840306,
-318.763353001344)) ;
#37603 = CARTESIAN_POINT('Ctrl Pts',(-1.15739072023135,18.5310896824256,-318.758828362998)) ;
#37604 = CARTESIAN_POINT('Ctrl Pts',(-1.37217082284677,18.5164247379902,-318.756005663441)) ;
#37605 = CARTESIAN_POINT('Ctrl Pts',(-1.85894929379247,18.4746718782548,-318.749552448906)) ;
#37606 = CARTESIAN_POINT('Ctrl Pts',(-2.13070226663562,18.4453056610072,-318.745909885078)) ;
#37607 = CARTESIAN_POINT('Ctrl Pts',(-2.74944388752091,18.3645864748853,-318.737547411276)) ;
#37608 = CARTESIAN_POINT('Ctrl Pts',(-3.09582519599233,18.3093785834638,-318.732815558718)) ;
#37609 = CARTESIAN_POINT('Ctrl Pts',(-3.53341348580599,18.2268604295015,-318.726821792608)) ;
#37610 = CARTESIAN_POINT('Ctrl Pts',(-3.62625741274178,18.208616343989,-318.725549271372)) ;
#37611 = CARTESIAN_POINT('Ctrl Pts',(-4.03422819987566,18.1252048962627,-318.71995834476)) ;
#37612 = CARTESIAN_POINT('Ctrl Pts',(-4.34777011644217,18.0525606343029,-318.715662488817)) ;
#37613 = CARTESIAN_POINT('Ctrl Pts',(-4.75402736579329,17.947236738845,-318.710158445573)) ;
#37614 = CARTESIAN_POINT('Ctrl Pts',(-4.84859346628896,17.9219202150331,-318.708881769034)) ;
#37615 = CARTESIAN_POINT('Ctrl Pts',(-5.00695331122746,17.8781801700861,-318.706754024377)) ;
#37616 = CARTESIAN_POINT('Ctrl Pts',(-5.07085636005197,17.860160230684,-318.705898284603)) ;
#37617 = CARTESIAN_POINT('Ctrl Pts',(-5.21206349339977,17.8195224623743,-318.704014250737)) ;
#37618 = CARTESIAN_POINT('Ctrl Pts',(-5.28931968261299,17.7967436337499,-318.702987828093)) ;
#37619 = CARTESIAN_POINT('Ctrl Pts',(-5.53741294583378,17.721835667284,-318.699702391115)) ;
#37620 = CARTESIAN_POINT('Ctrl Pts',(-5.70764701574402,17.667743695579,-318.697464369429)) ;
#37621 = CARTESIAN_POINT('Ctrl Pts',(-6.14563602350867,17.5215814032531,-318.691721530713)) ;
#37622 = CARTESIAN_POINT('Ctrl Pts',(-6.41211301018302,17.4258275027864,-318.688242077665)) ;
#37623 = CARTESIAN_POINT('Ctrl Pts',(-7.33936226880055,17.0684859878422,-318.67605949018)) ;
#37624 = CARTESIAN_POINT('Ctrl Pts',(-7.98721189798678,16.7750975591633,-318.667388752436)) ;
#37625 = CARTESIAN_POINT('Ctrl Pts',(-8.75432584874016,16.3731621316589,-318.656491183854)) ;
#37626 = CARTESIAN_POINT('Ctrl Pts',(-8.89109464336208,16.2992973838001,-318.654524004584)) ;
#37627 = CARTESIAN_POINT('Ctrl Pts',(-9.13737203238803,16.1622680436406,-318.650934540585)) ;
#37628 = CARTESIAN_POINT('Ctrl Pts',(-9.2471938514487,16.0996857669079,-318.649316582503)) ;
#37629 = CARTESIAN_POINT('Ctrl Pts',(-9.47093178478554,15.9691434791818,-318.645983644309)) ;
#37630 = CARTESIAN_POINT('Ctrl Pts',(-9.58477591511213,15.9010742695455,-318.644267910623)) ;
#37631 = CARTESIAN_POINT('Ctrl Pts',(-9.8811208305962,15.719545999035,-318.639748975747)) ;
#37632 = CARTESIAN_POINT('Ctrl Pts',(-10.0623980895875,15.6041282909349,-318.63693136277)) ;
#37633 = CARTESIAN_POINT('Ctrl Pts',(-10.4689874569629,15.3352242246589,-318.630492998658)) ;
#37634 = CARTESIAN_POINT('Ctrl Pts',(-10.6930048253221,15.1798698213774,-318.626860292161)) ;
#37635 = CARTESIAN_POINT('Ctrl Pts',(-11.1979542227078,14.8129651950213,-318.618495819203)) ;
#37636 = CARTESIAN_POINT('Ctrl Pts',(-11.4764600815456,14.5982526456681,-318.61375177208)) ;
#37637 = CARTESIAN_POINT('Ctrl Pts',(-11.7911611138096,14.3410608418183,-318.608281240642)) ;
#37638 = CARTESIAN_POINT('Ctrl Pts',(-11.8334677611648,14.3061716481852,-318.607543484001)) ;
#37639 = CARTESIAN_POINT('Ctrl Pts',(-12.1306642129733,14.058861139532,-318.602345714431)) ;
#37640 = CARTESIAN_POINT('Ctrl Pts',(-12.3799744482791,13.8398274609973,-318.59790527827)) ;
#37641 = CARTESIAN_POINT('Ctrl Pts',(-12.7060976809789,13.5374420106455,-318.592053327911)) ;
#37642 = CARTESIAN_POINT('Ctrl Pts',(-12.7882119762277,13.4598992930987,-318.590576144318)) ;
#37643 = CARTESIAN_POINT('Ctrl Pts',(-12.914289658331,13.3386455118696,-318.588305850461)) ;
#37644 = CARTESIAN_POINT('Ctrl Pts',(-12.9587502015143,13.2954554153335,-318.587504809431)) ;
#37645 = CARTESIAN_POINT('Ctrl Pts',(-13.054107212376,13.2018904784254,-318.585786697686)) ;
#37646 = CARTESIAN_POINT('Ctrl Pts',(-13.104930218344,13.1514421759214,-318.58487091452)) ;
#37647 = CARTESIAN_POINT('Ctrl Pts',(-13.2457409007182,13.0100429250027,-318.582331393171)) ;
#37648 = CARTESIAN_POINT('Ctrl Pts',(-13.3350822610358,12.9184538584369,-318.580717519741)) ;
#37649 = CARTESIAN_POINT('Ctrl Pts',(-13.5421371321574,12.7017529407807,-318.576961776424)) ;
#37650 = CARTESIAN_POINT('Ctrl Pts',(-13.6590752301625,12.5759162634834,-318.574828574908)) ;
#37651 = CARTESIAN_POINT('Ctrl Pts',(-14.1229851451993,12.0625994631588,-318.5662809536)) ;
#37652 = CARTESIAN_POINT('Ctrl Pts',(-14.4553511707041,11.6622398838606,-318.55995431712)) ;
#37653 = CARTESIAN_POINT('Ctrl Pts',(-14.9505217350408,11.0120260128224,-318.549897637633)) ;
#37654 = CARTESIAN_POINT('Ctrl Pts',(-15.1248714250512,10.7713082318509,-318.546219969152)) ;
#37655 = CARTESIAN_POINT('Ctrl Pts',(-15.4134301199703,10.3520777089572,-318.539853914446)) ;
#37656 = CARTESIAN_POINT('Ctrl Pts',(-15.5304994132162,10.1756045868752,-318.537185705044)) ;
#37657 = CARTESIAN_POINT('Ctrl Pts',(-15.7156502983618,9.8858627766046,-318.532815694429)) ;
#37658 = CARTESIAN_POINT('Ctrl Pts',(-15.785586519244,9.77380198905806,-318.531128152536)) ;
#37659 = CARTESIAN_POINT('Ctrl Pts',(-15.921054578928,9.55149031568692,-318.527784175687)) ;
#37660 = CARTESIAN_POINT('Ctrl Pts',(-15.9866517133622,9.44128768204757,-318.526128356935)) ;
#37661 = CARTESIAN_POINT('Ctrl Pts',(-16.1462579007195,9.16671733074994,-318.522006849643)) ;
#37662 = CARTESIAN_POINT('Ctrl Pts',(-16.2389041643838,9.00157442803382,-318.519531329207)) ;
#37663 = CARTESIAN_POINT('Ctrl Pts',(-16.4370412482625,8.63537566324837,-318.514050979254)) ;
#37664 = CARTESIAN_POINT('Ctrl Pts',(-16.541402933734,8.43374333079441,-318.511039217987)) ;
#37665 = CARTESIAN_POINT('Ctrl Pts',(-16.8886048482437,7.7316808686993,-318.500587796269)) ;
#37666 = CARTESIAN_POINT('Ctrl Pts',(-17.1126401192644,7.22228557587834,-318.493056941253)) ;
#37667 = CARTESIAN_POINT('Ctrl Pts',(-17.4261477460373,6.41258627639805,-318.481404513876)) ;
#37668 = CARTESIAN_POINT('Ctrl Pts',(-17.5314721620727,6.11877214399491,-318.477241434961)) ;
#37669 = CARTESIAN_POINT('Ctrl Pts',(-17.6596064516527,5.73080387792469,-318.471884885673)) ;
#37670 = CARTESIAN_POINT('Ctrl Pts',(-17.6891571151897,5.63893019176652,-318.470626676888)) ;
#37671 = CARTESIAN_POINT('Ctrl Pts',(-17.7377678891916,5.48365498363562,-318.468519914761)) ;
#37672 = CARTESIAN_POINT('Ctrl Pts',(-17.7572076253362,5.42037443860558,-318.46766690355)) ;
#37673 = CARTESIAN_POINT('Ctrl Pts',(-17.7997355321152,5.27925245645252,-318.465777481868)) ;
#37674 = CARTESIAN_POINT('Ctrl Pts',(-17.8226523196749,5.20136095928083,-318.464743068812)) ;
#37675 = CARTESIAN_POINT('Ctrl Pts',(-17.8956273485174,4.94718140774883,-318.461391520513)) ;
#37676 = CARTESIAN_POINT('Ctrl Pts',(-17.9435866691828,4.77030184957938,-318.459096621088)) ;
#37677 = CARTESIAN_POINT('Ctrl Pts',(-18.0619446800004,4.30671535820382,-318.453149528427)) ;
#37678 = CARTESIAN_POINT('Ctrl Pts',(-18.1281377124707,4.01898822142204,-318.449524953752)) ;
#37679 = CARTESIAN_POINT('Ctrl Pts',(-18.3251680355522,3.05822018577023,-318.437506739991)) ;
#37680 = CARTESIAN_POINT('Ctrl Pts',(-18.4255900720567,2.37952180469889,-318.429134787705)) ;
#37681 = CARTESIAN_POINT('Ctrl Pts',(-18.5043188370393,1.52171228094436,-318.418302299987)) ;
#37682 = CARTESIAN_POINT('Ctrl Pts',(-18.5179020693778,1.34637539465069,-318.416076495061)) ;
#37683 = CARTESIAN_POINT('Ctrl Pts',(-18.5369432144629,1.04505026301386,-318.412227400989)) ;
#37684 = CARTESIAN_POINT('Ctrl Pts',(-18.5436122629388,0.919150682497201,
-318.410612040555)) ;
#37685 = CARTESIAN_POINT('Ctrl Pts',(-18.5540282093306,0.67557142995478,-318.407472122584)) ;
#37686 = CARTESIAN_POINT('Ctrl Pts',(-18.557939051304,0.557904717806982,-318.405948705179)) ;
#37687 = CARTESIAN_POINT('Ctrl Pts',(-18.5651912253845,0.25212794626181,-318.401972420641)) ;
#37688 = CARTESIAN_POINT('Ctrl Pts',(-18.5667929056849,0.0639903423706501,
-318.399508691408)) ;
#37689 = CARTESIAN_POINT('Ctrl Pts',(-18.5638984000726,-0.368896367162233,
-318.393802427836)) ;
#37690 = CARTESIAN_POINT('Ctrl Pts',(-18.5574218695251,-0.613597248698912,
-318.390549095427)) ;
#37691 = CARTESIAN_POINT('Ctrl Pts',(-18.5143817902944,-1.54382427506486,
-318.378099834224)) ;
#37692 = CARTESIAN_POINT('Ctrl Pts',(-18.4446477669696,-2.22726109135783,
-318.368764315729)) ;
#37693 = CARTESIAN_POINT('Ctrl Pts',(-18.3089863403239,-3.0835194181925,-318.357243022656)) ;
#37694 = CARTESIAN_POINT('Ctrl Pts',(-18.27814623129,-3.26135606137891,-318.354861264853)) ;
#37695 = CARTESIAN_POINT('Ctrl Pts',(-18.2297458640308,-3.51815288053859,
-318.351451092482)) ;
#37696 = CARTESIAN_POINT('Ctrl Pts',(-18.2142549483766,-3.59749227350268,
-318.350401550622)) ;
#37697 = CARTESIAN_POINT('Ctrl Pts',(-18.1858442295867,-3.73811329733303,
-318.348550114836)) ;
#37698 = CARTESIAN_POINT('Ctrl Pts',(-18.1731316170183,-3.79943529920401,
-318.347745848588)) ;
#37699 = CARTESIAN_POINT('Ctrl Pts',(-18.158429225038,-3.8685931205935,-318.346842019715)) ;
#37700 = CARTESIAN_POINT('Ctrl Pts',(-18.1567443315294,-3.87649325201482,
-318.346738818546)) ;
#37701 = CARTESIAN_POINT('Ctrl Pts',(-18.1539314428153,-3.88964026281774,
-318.346567151481)) ;
#37702 = CARTESIAN_POINT('Ctrl Pts',(-18.1528063275652,-3.89488775685342,
-318.3464986523)) ;
#37703 = CARTESIAN_POINT('Ctrl Pts',(-18.1508174306041,-3.9041443136841,-318.346377854715)) ;
#37704 = CARTESIAN_POINT('Ctrl Pts',(-18.149954595568,-3.9081535793794,-318.346325545485)) ;
#37705 = CARTESIAN_POINT('Ctrl Pts',(-18.1483734457119,-3.91548876325583,
-318.346229863474)) ;
#37706 = CARTESIAN_POINT('Ctrl Pts',(-18.1476555448736,-3.91881477041541,
-318.346186485996)) ;
#37707 = CARTESIAN_POINT('Ctrl Pts',(-18.1463049319,-3.9250637784958,-318.346105001539)) ;
#37708 = CARTESIAN_POINT('Ctrl Pts',(-18.1456724277551,-3.92798682423524,
-318.346066892216)) ;
#37709 = CARTESIAN_POINT('Ctrl Pts',(-18.1444572512732,-3.93359606649929,
-318.345993772863)) ;
#37710 = CARTESIAN_POINT('Ctrl Pts',(-18.1438746886403,-3.93628228669855,
-318.345958761606)) ;
#37711 = CARTESIAN_POINT('Ctrl Pts',(-18.1427353884965,-3.94153001977682,
-318.345890374176)) ;
#37712 = CARTESIAN_POINT('Ctrl Pts',(-18.1421787049898,-3.94409154432547,
-318.345856997402)) ;
#37713 = CARTESIAN_POINT('Ctrl Pts',(-18.1410727097517,-3.9491754843671,-318.345790762332)) ;
#37714 = CARTESIAN_POINT('Ctrl Pts',(-18.1405234143736,-3.95169790335584,
-318.345757903857)) ;
#37715 = CARTESIAN_POINT('Ctrl Pts',(-18.1394161344572,-3.95677754672119,
-318.345691742188)) ;
#37716 = CARTESIAN_POINT('Ctrl Pts',(-18.1388581352217,-3.95933476780442,
-318.345658439159)) ;
#37717 = CARTESIAN_POINT('Ctrl Pts',(-18.1377176875766,-3.96455595549308,
-318.345590451913)) ;
#37718 = CARTESIAN_POINT('Ctrl Pts',(-18.1371351929829,-3.96721991196936,
-318.345555768203)) ;
#37719 = CARTESIAN_POINT('Ctrl Pts',(-18.1359285503817,-3.97273250071204,
-318.345484006164)) ;
#37720 = CARTESIAN_POINT('Ctrl Pts',(-18.1353043180758,-3.97558111444687,
-318.345446928757)) ;
#37721 = CARTESIAN_POINT('Ctrl Pts',(-18.133993709784,-3.98155519560775,-318.345369181675)) ;
#37722 = CARTESIAN_POINT('Ctrl Pts',(-18.1333071968592,-3.98468063293579,
-318.345328513487)) ;
#37723 = CARTESIAN_POINT('Ctrl Pts',(-18.1318459158649,-3.99132510197802,
-318.345242069256)) ;
#37724 = CARTESIAN_POINT('Ctrl Pts',(-18.1310709312786,-3.99484408598062,
-318.345196295546)) ;
#37725 = CARTESIAN_POINT('Ctrl Pts',(-18.1293976485544,-4.00243146873174,
-318.345097618819)) ;
#37726 = CARTESIAN_POINT('Ctrl Pts',(-18.1284990052823,-4.00649979118784,
-318.345044719496)) ;
#37727 = CARTESIAN_POINT('Ctrl Pts',(-18.1265293287268,-4.01540264694927,
-318.344928981165)) ;
#37728 = CARTESIAN_POINT('Ctrl Pts',(-18.1254577305941,-4.02023705504703,
-318.344866148149)) ;
#37729 = CARTESIAN_POINT('Ctrl Pts',(-18.1230709949504,-4.03098422284104,
-318.344726499441)) ;
#37730 = CARTESIAN_POINT('Ctrl Pts',(-18.1217548976287,-4.03689676894075,
-318.344649693826)) ;
#37731 = CARTESIAN_POINT('Ctrl Pts',(-18.1187728395093,-4.05026277199221,
-318.34447611454)) ;
#37732 = CARTESIAN_POINT('Ctrl Pts',(-18.117105172565,-4.05771584739041,-318.344379358558)) ;
#37733 = CARTESIAN_POINT('Ctrl Pts',(-18.1132570179065,-4.074864213554,-318.344156815123)) ;
#37734 = CARTESIAN_POINT('Ctrl Pts',(-18.1110733439094,-4.08455878733749,
-318.344031060171)) ;
#37735 = CARTESIAN_POINT('Ctrl Pts',(-18.1059391720616,-4.1072672382508,-318.343736621695)) ;
#37736 = CARTESIAN_POINT('Ctrl Pts',(-18.1029824250556,-4.12027969766941,
-318.34356800057)) ;
#37737 = CARTESIAN_POINT('Ctrl Pts',(-18.0750185728465,-4.24273570201157,
-318.341982050093)) ;
#37738 = CARTESIAN_POINT('Ctrl Pts',(-18.0490332825581,-4.35195361406421,
-318.340574212525)) ;
#37739 = CARTESIAN_POINT('Ctrl Pts',(-17.9668517425299,-4.68396528585044,
-318.336306934106)) ;
#37740 = CARTESIAN_POINT('Ctrl Pts',(-17.9075088299259,-4.90595761318199,
-318.333470611908)) ;
#37741 = CARTESIAN_POINT('Ctrl Pts',(-17.6252202696703,-5.88847745537046,
-318.320903469693)) ;
#37742 = CARTESIAN_POINT('Ctrl Pts',(-17.3578351629958,-6.63536862936886,
-318.311275402797)) ;
#37743 = CARTESIAN_POINT('Ctrl Pts',(-16.9817878734702,-7.50583971962521,
-318.299342870323)) ;
#37744 = CARTESIAN_POINT('Ctrl Pts',(-16.918234904781,-7.64801130293698,-318.297371936375)) ;
#37745 = CARTESIAN_POINT('Ctrl Pts',(-16.7997576900633,-7.90434598660228,
-318.293775222344)) ;
#37746 = CARTESIAN_POINT('Ctrl Pts',(-16.7454391792276,-8.01877862034104,
-318.292153768767)) ;
#37747 = CARTESIAN_POINT('Ctrl Pts',(-16.6389050002422,-8.23740985922531,
-318.289024407353)) ;
#37748 = CARTESIAN_POINT('Ctrl Pts',(-16.5868708111661,-8.34169032315824,
-318.287517859778)) ;
#37749 = CARTESIAN_POINT('Ctrl Pts',(-16.4739218003158,-8.56281266263802,
-318.2842931734)) ;
#37750 = CARTESIAN_POINT('Ctrl Pts',(-16.4127379426994,-8.67950997138908,
-318.282573183366)) ;
#37751 = CARTESIAN_POINT('Ctrl Pts',(-15.9857591937404,-9.47323419920945,
-318.270750914775)) ;
#37752 = CARTESIAN_POINT('Ctrl Pts',(-15.5794215653148,-10.1275997121318,
-318.260347666216)) ;
#37753 = CARTESIAN_POINT('Ctrl Pts',(-15.1336583262364,-10.7548540235205,
-318.25)) ;
#37754 = CARTESIAN_POINT('',(-15.1169169700218,10.7783728235744,-318.25)) ;
#37755 = CARTESIAN_POINT('Origin',(0.,0.,-318.25)) ;
#37756 = CARTESIAN_POINT('Ctrl Pts',(-15.1169169700218,10.7783728235744,-318.25)) ;
#37757 = CARTESIAN_POINT('Ctrl Pts',(-15.0804944480825,10.8294562523078,-318.250806729991)) ;
#37758 = CARTESIAN_POINT('Ctrl Pts',(-15.0438190603979,10.8803466676463,-318.251609740784)) ;
#37759 = CARTESIAN_POINT('Ctrl Pts',(-14.9579853298804,10.998184895247,-318.253468673654)) ;
#37760 = CARTESIAN_POINT('Ctrl Pts',(-14.9086402498598,11.0649826949969,-318.254522080836)) ;
#37761 = CARTESIAN_POINT('Ctrl Pts',(-14.5784009174709,11.5058037452061,-318.261478585359)) ;
#37762 = CARTESIAN_POINT('Ctrl Pts',(-14.2839052146774,11.8694291017734,-318.267243743558)) ;
#37763 = CARTESIAN_POINT('Ctrl Pts',(-13.6209747107106,12.6275256931051,-318.279666832644)) ;
#37764 = CARTESIAN_POINT('Ctrl Pts',(-13.248436743511,13.0178446772958,-318.286323244042)) ;
#37765 = CARTESIAN_POINT('Ctrl Pts',(-12.7598241901181,13.4870478312939,-318.294856579549)) ;
#37766 = CARTESIAN_POINT('Ctrl Pts',(-12.6591461570025,13.5815901528953,-318.296604476164)) ;
#37767 = CARTESIAN_POINT('Ctrl Pts',(-12.4700111119216,13.7552683005789,-318.299871675423)) ;
#37768 = CARTESIAN_POINT('Ctrl Pts',(-12.3818319254856,13.8346962843052,-318.301388458098)) ;
#37769 = CARTESIAN_POINT('Ctrl Pts',(-12.1966947945626,13.9982718639443,-318.304561025838)) ;
#37770 = CARTESIAN_POINT('Ctrl Pts',(-12.0996133420859,14.0822702716743,-318.306217959224)) ;
#37771 = CARTESIAN_POINT('Ctrl Pts',(-11.8645152255382,14.2814597456724,-318.3102157174)) ;
#37772 = CARTESIAN_POINT('Ctrl Pts',(-11.7256815267206,14.3956662431381,-318.31256463121)) ;
#37773 = CARTESIAN_POINT('Ctrl Pts',(-10.8544872507128,15.09135705424,-318.327232159744)) ;
#37774 = CARTESIAN_POINT('Ctrl Pts',(-10.0807227641066,15.6188334184307,-318.340025544145)) ;
#37775 = CARTESIAN_POINT('Ctrl Pts',(-9.08320412226288,16.1937225475383,-318.355554114097)) ;
#37776 = CARTESIAN_POINT('Ctrl Pts',(-8.89400347550464,16.2984032805629,-318.358455446921)) ;
#37777 = CARTESIAN_POINT('Ctrl Pts',(-8.60845672260143,16.4499371486907,-318.362748276585)) ;
#37778 = CARTESIAN_POINT('Ctrl Pts',(-8.5134635221799,16.4992999319676,-318.364162380739)) ;
#37779 = CARTESIAN_POINT('Ctrl Pts',(-8.39152923399645,16.5613291071284,-318.365957300581)) ;
#37780 = CARTESIAN_POINT('Ctrl Pts',(-8.36497743171584,16.5747560237762,-318.366346934525)) ;
#37781 = CARTESIAN_POINT('Ctrl Pts',(-8.32742032269198,16.5936349546005,-318.366896285397)) ;
#37782 = CARTESIAN_POINT('Ctrl Pts',(-8.31644171426074,16.5991399611761,-318.367056655943)) ;
#37783 = CARTESIAN_POINT('Ctrl Pts',(-8.29492316239464,16.6099033071463,-318.367370563337)) ;
#37784 = CARTESIAN_POINT('Ctrl Pts',(-8.28438366125306,16.6151625178938,-318.367524111155)) ;
#37785 = CARTESIAN_POINT('Ctrl Pts',(-8.26717845326089,16.6237274756253,-318.367774439919)) ;
#37786 = CARTESIAN_POINT('Ctrl Pts',(-8.26051575240305,16.6270392513593,-318.367871298751)) ;
#37787 = CARTESIAN_POINT('Ctrl Pts',(-8.24983555684862,16.6323399671715,-318.36802643134)) ;
#37788 = CARTESIAN_POINT('Ctrl Pts',(-8.24581932980345,16.634331458729,-318.368084738526)) ;
#37789 = CARTESIAN_POINT('Ctrl Pts',(-8.18861115537183,16.6626729685035,-318.368914858298)) ;
#37790 = CARTESIAN_POINT('Ctrl Pts',(-8.1352937953847,16.6887692176808,-318.369683285192)) ;
#37791 = CARTESIAN_POINT('Ctrl Pts',(-8.01968606929195,16.744667893812,-318.371337613913)) ;
#37792 = CARTESIAN_POINT('Ctrl Pts',(-7.95735283482998,16.7743793745763,-318.372222345166)) ;
#37793 = CARTESIAN_POINT('Ctrl Pts',(-7.79236082525833,16.8518971083591,-318.374546844281)) ;
#37794 = CARTESIAN_POINT('Ctrl Pts',(-7.68942784001788,16.8991130812709,-318.375979424839)) ;
#37795 = CARTESIAN_POINT('Ctrl Pts',(-7.12736806461566,17.1507346594597,-318.383721888176)) ;
#37796 = CARTESIAN_POINT('Ctrl Pts',(-6.66051661901487,17.337375700734,-318.389869841283)) ;
#37797 = CARTESIAN_POINT('Ctrl Pts',(-5.81707614590315,17.635469527898,-318.400840395687)) ;
#37798 = CARTESIAN_POINT('Ctrl Pts',(-5.44343991918518,17.7543550083848,-318.405652938792)) ;
#37799 = CARTESIAN_POINT('Ctrl Pts',(-4.8810697088908,17.9138699693625,-318.412920224449)) ;
#37800 = CARTESIAN_POINT('Ctrl Pts',(-4.69501173579473,17.9635309289428,-318.415327935294)) ;
#37801 = CARTESIAN_POINT('Ctrl Pts',(-4.38050282546227,18.0422566993248,-318.419411484194)) ;
#37802 = CARTESIAN_POINT('Ctrl Pts',(-4.25245416643611,18.0728654428255,-318.421077777132)) ;
#37803 = CARTESIAN_POINT('Ctrl Pts',(-4.01051882246542,18.1279840655623,-318.42423499826)) ;
#37804 = CARTESIAN_POINT('Ctrl Pts',(-3.89670584611696,18.1527890698395,-318.425723933116)) ;
#37805 = CARTESIAN_POINT('Ctrl Pts',(-3.65877194330506,18.2023048557559,-318.428845269554)) ;
#37806 = CARTESIAN_POINT('Ctrl Pts',(-3.53461654536178,18.2268208971872,-318.430478870912)) ;
#37807 = CARTESIAN_POINT('Ctrl Pts',(-3.22719365502355,18.2842661584178,-318.434536451853)) ;
#37808 = CARTESIAN_POINT('Ctrl Pts',(-3.04366311077679,18.3157113577331,-318.436969901929)) ;
#37809 = CARTESIAN_POINT('Ctrl Pts',(-2.27776241053797,18.4351069440466,-318.447168610217)) ;
#37810 = CARTESIAN_POINT('Ctrl Pts',(-1.69184858502896,18.4980814588032,-318.455086823874)) ;
#37811 = CARTESIAN_POINT('Ctrl Pts',(-0.596788143931648,18.5633094174577,
-318.469870661373)) ;
#37812 = CARTESIAN_POINT('Ctrl Pts',(-0.0886155740524386,18.5726884753098,
-318.476722158459)) ;
#37813 = CARTESIAN_POINT('Ctrl Pts',(0.520446927102541,18.5589296618443,-318.484719967855)) ;
#37814 = CARTESIAN_POINT('Ctrl Pts',(0.621572978063025,18.5558180168559,-318.486040563542)) ;
#37815 = CARTESIAN_POINT('Ctrl Pts',(0.789256073556296,18.5492861013175,-318.488215355147)) ;
#37816 = CARTESIAN_POINT('Ctrl Pts',(0.855829086489303,18.5463337786349,-318.489074790814)) ;
#37817 = CARTESIAN_POINT('Ctrl Pts',(1.00110580434746,18.5391072834794,-318.490940999427)) ;
#37818 = CARTESIAN_POINT('Ctrl Pts',(1.07980094253777,18.5346902225778,-318.491946199504)) ;
#37819 = CARTESIAN_POINT('Ctrl Pts',(1.32423476406868,18.5194084275355,-318.495053688154)) ;
#37820 = CARTESIAN_POINT('Ctrl Pts',(1.48985763389259,18.5068206510279,-318.49713821824)) ;
#37821 = CARTESIAN_POINT('Ctrl Pts',(2.29840258448145,18.4344447563835,-318.507253006644)) ;
#37822 = CARTESIAN_POINT('Ctrl Pts',(2.93807602782849,18.3433672413775,-318.51508049397)) ;
#37823 = CARTESIAN_POINT('Ctrl Pts',(3.84160384304844,18.1662386140285,-318.526419542586)) ;
#37824 = CARTESIAN_POINT('Ctrl Pts',(4.11029517597141,18.107336046666,-318.529825362182)) ;
#37825 = CARTESIAN_POINT('Ctrl Pts',(4.58807701960243,17.9914136966011,-318.535972908446)) ;
#37826 = CARTESIAN_POINT('Ctrl Pts',(4.79766558568324,17.936661401507,-318.538701387193)) ;
#37827 = CARTESIAN_POINT('Ctrl Pts',(5.13506523197348,17.8421831495394,-318.543153613366)) ;
#37828 = CARTESIAN_POINT('Ctrl Pts',(5.26348894196061,17.8047206822806,-318.544862382922)) ;
#37829 = CARTESIAN_POINT('Ctrl Pts',(5.5136780625553,17.7287945678808,-318.548220312384)) ;
#37830 = CARTESIAN_POINT('Ctrl Pts',(5.63547381165989,17.6904561125664,-318.549868553271)) ;
#37831 = CARTESIAN_POINT('Ctrl Pts',(5.93598431759697,17.5924440175862,-318.553969487297)) ;
#37832 = CARTESIAN_POINT('Ctrl Pts',(6.1142044638569,17.5313005773715,-318.55643181362)) ;
#37833 = CARTESIAN_POINT('Ctrl Pts',(6.64595668316723,17.3397730033988,-318.563867606771)) ;
#37834 = CARTESIAN_POINT('Ctrl Pts',(6.99648067898841,17.2013291650822,-318.568890111049)) ;
#37835 = CARTESIAN_POINT('Ctrl Pts',(7.79254290494892,16.8585531381439,-318.580518963213)) ;
#37836 = CARTESIAN_POINT('Ctrl Pts',(8.23469113401574,16.6470538043224,-318.587145676751)) ;
#37837 = CARTESIAN_POINT('Ctrl Pts',(8.81609980789244,16.3401024373588,-318.595926855089)) ;
#37838 = CARTESIAN_POINT('Ctrl Pts',(8.96317956412928,16.2598885515971,-318.598153619319)) ;
#37839 = CARTESIAN_POINT('Ctrl Pts',(9.21884671867051,16.1159303803091,-318.602022216398)) ;
#37840 = CARTESIAN_POINT('Ctrl Pts',(9.32790887175798,16.0530515168696,-318.60367175563)) ;
#37841 = CARTESIAN_POINT('Ctrl Pts',(9.49805628517949,15.952635035051,-318.606239122047)) ;
#37842 = CARTESIAN_POINT('Ctrl Pts',(9.55957791798111,15.9158445520717,-318.607166159245)) ;
#37843 = CARTESIAN_POINT('Ctrl Pts',(9.67432929580857,15.8463168262155,-318.608891749969)) ;
#37844 = CARTESIAN_POINT('Ctrl Pts',(9.7276097919673,15.8136653568912,-318.609691485485)) ;
#37845 = CARTESIAN_POINT('Ctrl Pts',(9.87932726954172,15.7196326104818,-318.61196590319)) ;
#37846 = CARTESIAN_POINT('Ctrl Pts',(9.97735528193598,15.6575968254532,-318.613432024187)) ;
#37847 = CARTESIAN_POINT('Ctrl Pts',(10.4124171795256,15.3765285940358,-318.61993684575)) ;
#37848 = CARTESIAN_POINT('Ctrl Pts',(10.7428673430728,15.1475036200241,-318.624874309655)) ;
#37849 = CARTESIAN_POINT('Ctrl Pts',(11.4392363981211,14.630613894219,-318.635501819375)) ;
#37850 = CARTESIAN_POINT('Ctrl Pts',(11.8022924624233,14.3393474287269,-318.641185621807)) ;
#37851 = CARTESIAN_POINT('Ctrl Pts',(12.2614842130961,13.941689740524,-318.648714630063)) ;
#37852 = CARTESIAN_POINT('Ctrl Pts',(12.3678737358538,13.8473971246321,-318.650483707777)) ;
#37853 = CARTESIAN_POINT('Ctrl Pts',(12.6298718970273,13.609760912265,-318.654907636104)) ;
#37854 = CARTESIAN_POINT('Ctrl Pts',(12.7841329818794,13.4649619346898,-318.657573073036)) ;
#37855 = CARTESIAN_POINT('Ctrl Pts',(13.0302631450031,13.2258857100484,-318.661933668541)) ;
#37856 = CARTESIAN_POINT('Ctrl Pts',(13.1236635202806,13.1332123332325,-318.663614482381)) ;
#37857 = CARTESIAN_POINT('Ctrl Pts',(13.3045094654124,12.9499182721772,-318.666921759855)) ;
#37858 = CARTESIAN_POINT('Ctrl Pts',(13.392033802588,12.8593851310248,-318.668547368957)) ;
#37859 = CARTESIAN_POINT('Ctrl Pts',(13.5855118747432,12.6551381231626,-318.672197759126)) ;
#37860 = CARTESIAN_POINT('Ctrl Pts',(13.6909723504897,12.5409700507982,-318.674226722456)) ;
#37861 = CARTESIAN_POINT('Ctrl Pts',(14.2732844650016,11.8944774778714,-318.685650738065)) ;
#37862 = CARTESIAN_POINT('Ctrl Pts',(14.7205210233672,11.3362911184259,-318.69529739059)) ;
#37863 = CARTESIAN_POINT('Ctrl Pts',(15.2993019893397,10.5217322075699,-318.708755512442)) ;
#37864 = CARTESIAN_POINT('Ctrl Pts',(15.4587849136962,10.285983634175,-318.712579501153)) ;
#37865 = CARTESIAN_POINT('Ctrl Pts',(15.7097043879317,9.89604796700484,-318.718742919378)) ;
#37866 = CARTESIAN_POINT('Ctrl Pts',(15.8044387785662,9.74403881422784,-318.721106763069)) ;
#37867 = CARTESIAN_POINT('Ctrl Pts',(15.9384277147384,9.52194652831368,-318.724491941304)) ;
#37868 = CARTESIAN_POINT('Ctrl Pts',(15.9794502044216,9.45294212901537,-318.725534286593)) ;
#37869 = CARTESIAN_POINT('Ctrl Pts',(16.053453600627,9.32660182750237,-318.727424000042)) ;
#37870 = CARTESIAN_POINT('Ctrl Pts',(16.0865780189105,9.26935174596814,-318.728273207419)) ;
#37871 = CARTESIAN_POINT('Ctrl Pts',(16.1675446721413,9.12767306130208,-318.730358195759)) ;
#37872 = CARTESIAN_POINT('Ctrl Pts',(16.2150322632963,9.04304401068473,-318.731589353394)) ;
#37873 = CARTESIAN_POINT('Ctrl Pts',(16.4150211196561,8.67999726425118,-318.73681774899)) ;
#37874 = CARTESIAN_POINT('Ctrl Pts',(16.5610319771791,8.39806475392093,-318.740746362187)) ;
#37875 = CARTESIAN_POINT('Ctrl Pts',(16.8915132772734,7.71776470182411,-318.750048222256)) ;
#37876 = CARTESIAN_POINT('Ctrl Pts',(17.0692260987333,7.31632650772171,-318.755398222172)) ;
#37877 = CARTESIAN_POINT('Ctrl Pts',(17.336815034305,6.64889858287995,-318.764247519535)) ;
#37878 = CARTESIAN_POINT('Ctrl Pts',(17.435182949256,6.38650163104886,-318.767714539907)) ;
#37879 = CARTESIAN_POINT('Ctrl Pts',(17.5998078872297,5.91517109759757,-318.77395375779)) ;
#37880 = CARTESIAN_POINT('Ctrl Pts',(17.6683753383254,5.70710079120582,-318.776711868424)) ;
#37881 = CARTESIAN_POINT('Ctrl Pts',(17.772801633614,5.37027610886836,-318.781191453457)) ;
#37882 = CARTESIAN_POINT('Ctrl Pts',(17.8109803999193,5.24226292022075,-318.782897288386)) ;
#37883 = CARTESIAN_POINT('Ctrl Pts',(17.8825714032875,4.9924041401712,-318.786234527583)) ;
#37884 = CARTESIAN_POINT('Ctrl Pts',(17.9161280021315,4.87060740051896,-318.787864856509)) ;
#37885 = CARTESIAN_POINT('Ctrl Pts',(17.9878719651966,4.59942741508577,-318.791503119001)) ;
#37886 = CARTESIAN_POINT('Ctrl Pts',(18.025446825523,4.44989179961282,-318.793514950972)) ;
#37887 = CARTESIAN_POINT('Ctrl Pts',(18.25433226632,3.48849039844217,-318.806483433725)) ;
#37888 = CARTESIAN_POINT('Ctrl Pts',(18.392609251568,2.6649807815381,-318.817796297087)) ;
#37889 = CARTESIAN_POINT('Ctrl Pts',(18.4902689215981,1.68171798566272,-318.831046357692)) ;
#37890 = CARTESIAN_POINT('Ctrl Pts',(18.5035834900991,1.52827297112301,-318.833105091512)) ;
#37891 = CARTESIAN_POINT('Ctrl Pts',(18.5284746013748,1.19302505287816,-318.837572730536)) ;
#37892 = CARTESIAN_POINT('Ctrl Pts',(18.5392878163098,1.01118113964923,-318.839976677257)) ;
#37893 = CARTESIAN_POINT('Ctrl Pts',(18.5510529277244,0.748023208970792,-318.843414310031)) ;
#37894 = CARTESIAN_POINT('Ctrl Pts',(18.5541493988392,0.666815985553406,-318.844469427861)) ;
#37895 = CARTESIAN_POINT('Ctrl Pts',(18.5588082255007,0.519183065203262,-318.846375644876)) ;
#37896 = CARTESIAN_POINT('Ctrl Pts',(18.5605473543417,0.452764519066003,-318.847228669419)) ;
#37897 = CARTESIAN_POINT('Ctrl Pts',(18.5639567475703,0.288957371814897,-318.849321956189)) ;
#37898 = CARTESIAN_POINT('Ctrl Pts',(18.5652172202946,0.191562238656035,-318.850557587054)) ;
#37899 = CARTESIAN_POINT('Ctrl Pts',(18.5673482578771,-0.228611399058598,
-318.855857258373)) ;
#37900 = CARTESIAN_POINT('Ctrl Pts',(18.5605676962895,-0.551373037934079,
-318.859850299482)) ;
#37901 = CARTESIAN_POINT('Ctrl Pts',(18.5451378280777,-0.87885608722279,-318.863881370167)) ;
#37902 = CARTESIAN_POINT('Ctrl Pts',(18.5448972467379,-0.883918091233771,
-318.863943674443)) ;
#37903 = CARTESIAN_POINT('Ctrl Pts',(18.5446545937441,-0.888979977966575,
-318.864005972278)) ;
#37904 = CARTESIAN_POINT('Origin',(0.,0.,-315.477129595899)) ;
#37905 = CARTESIAN_POINT('',(18.5446554538441,-0.88896203566046,-320.660059650531)) ;
#37906 = CARTESIAN_POINT('Ctrl Pts',(18.5446550920983,-0.888969581938671,
-320.660059750084)) ;
#37907 = CARTESIAN_POINT('Ctrl Pts',(18.589273190788,0.0418015803997639,-320.647780645843)) ;
#37908 = CARTESIAN_POINT('Ctrl Pts',(18.5637543137461,0.974592717322047,-320.635048004708)) ;
#37909 = CARTESIAN_POINT('Ctrl Pts',(18.4549963209679,2.03089251855565,-320.620930538161)) ;
#37910 = CARTESIAN_POINT('Ctrl Pts',(18.4403171247722,2.16011991256673,-320.61921007732)) ;
#37911 = CARTESIAN_POINT('Ctrl Pts',(18.4144686995445,2.36815865994873,-320.616456413024)) ;
#37912 = CARTESIAN_POINT('Ctrl Pts',(18.4041483514296,2.44707098477785,-320.615415644062)) ;
#37913 = CARTESIAN_POINT('Ctrl Pts',(18.3849139688139,2.58713279723982,-320.613576463609)) ;
#37914 = CARTESIAN_POINT('Ctrl Pts',(18.3762014213575,2.64830872146057,-320.612775896959)) ;
#37915 = CARTESIAN_POINT('Ctrl Pts',(18.3574013160327,2.77575386891301,-320.611114668359)) ;
#37916 = CARTESIAN_POINT('Ctrl Pts',(18.3472599694369,2.84201411374271,-320.610254836975)) ;
#37917 = CARTESIAN_POINT('Ctrl Pts',(18.3233706743031,2.99263977822422,-320.608308017056)) ;
#37918 = CARTESIAN_POINT('Ctrl Pts',(18.3093984815837,3.07696814729683,-320.60722356865)) ;
#37919 = CARTESIAN_POINT('Ctrl Pts',(18.24532625923,3.44777430354018,-320.602473901092)) ;
#37920 = CARTESIAN_POINT('Ctrl Pts',(18.1890812345201,3.73314914096403,-320.598867527116)) ;
#37921 = CARTESIAN_POINT('Ctrl Pts',(18.0018010468585,4.57820712232696,-320.58820688783)) ;
#37922 = CARTESIAN_POINT('Ctrl Pts',(17.851457819502,5.13325201940272,-320.58122097992)) ;
#37923 = CARTESIAN_POINT('Ctrl Pts',(17.6052489297788,5.89937261776771,-320.571270868736)) ;
#37924 = CARTESIAN_POINT('Ctrl Pts',(17.5308245118115,6.11699099811218,-320.56841032899)) ;
#37925 = CARTESIAN_POINT('Ctrl Pts',(17.3901414750641,6.50467256229697,-320.563236576897)) ;
#37926 = CARTESIAN_POINT('Ctrl Pts',(17.325381681515,6.67524794360466,-320.560932778364)) ;
#37927 = CARTESIAN_POINT('Ctrl Pts',(17.2148320344999,6.95398033901283,-320.557118248154)) ;
#37928 = CARTESIAN_POINT('Ctrl Pts',(17.1705113447932,7.06270660917089,-320.555617666966)) ;
#37929 = CARTESIAN_POINT('Ctrl Pts',(17.0769180642834,7.28621783382526,-320.552505817593)) ;
#37930 = CARTESIAN_POINT('Ctrl Pts',(17.0275123717725,7.40094070191585,-320.550893675624)) ;
#37931 = CARTESIAN_POINT('Ctrl Pts',(16.9024095239062,7.68355161479172,-320.546884729432)) ;
#37932 = CARTESIAN_POINT('Ctrl Pts',(16.825364968578,7.85082840492873,-320.544478631442)) ;
#37933 = CARTESIAN_POINT('Ctrl Pts',(16.5007865651158,8.52881097617581,-320.534592602845)) ;
#37934 = CARTESIAN_POINT('Ctrl Pts',(16.2323875959267,9.02918396261254,-320.526972447014)) ;
#37935 = CARTESIAN_POINT('Ctrl Pts',(15.7564942678808,9.8263752974343,-320.514466441475)) ;
#37936 = CARTESIAN_POINT('Ctrl Pts',(15.562497289475,10.1308164298362,-320.509600472102)) ;
#37937 = CARTESIAN_POINT('Ctrl Pts',(15.2785972371669,10.5489258171139,-320.502866547339)) ;
#37938 = CARTESIAN_POINT('Ctrl Pts',(15.1960520378454,10.667491363163,-320.500951231677)) ;
#37939 = CARTESIAN_POINT('Ctrl Pts',(15.0515141518069,10.8700188566082,-320.497677234812)) ;
#37940 = CARTESIAN_POINT('Ctrl Pts',(14.9901818155747,10.9544437278829,-320.496311739768)) ;
#37941 = CARTESIAN_POINT('Ctrl Pts',(14.9271528348508,11.0396834379257,-320.494934189799)) ;
#37942 = CARTESIAN_POINT('Ctrl Pts',(14.9261645412174,11.0410196201761,-320.494912596184)) ;
#37943 = CARTESIAN_POINT('Ctrl Pts',(14.9241562792725,11.0437340467001,-320.494868729797)) ;
#37944 = CARTESIAN_POINT('Ctrl Pts',(14.9231362994197,11.0451122824231,-320.494846457182)) ;
#37945 = CARTESIAN_POINT('Ctrl Pts',(14.9210653351239,11.047909837906,-320.494801248676)) ;
#37946 = CARTESIAN_POINT('Ctrl Pts',(14.9200143390571,11.0493291490419,-320.494778312942)) ;
#37947 = CARTESIAN_POINT('Ctrl Pts',(14.9185678653785,11.0512819477927,-320.494746756654)) ;
#37948 = CARTESIAN_POINT('Ctrl Pts',(14.9181725617037,11.0518155640936,-320.494738133721)) ;
#37949 = CARTESIAN_POINT('Ctrl Pts',(14.9173082735625,11.0529821267643,-320.494719282846)) ;
#37950 = CARTESIAN_POINT('Ctrl Pts',(14.9168392774149,11.0536150645315,-320.494709055064)) ;
#37951 = CARTESIAN_POINT('Ctrl Pts',(14.8909803290288,11.0885085868346,-320.494145206794)) ;
#37952 = CARTESIAN_POINT('Ctrl Pts',(14.8654724419213,11.1226816425733,-320.493593208123)) ;
#37953 = CARTESIAN_POINT('Ctrl Pts',(14.799905728718,11.2098932904887,-320.492185341768)) ;
#37954 = CARTESIAN_POINT('Ctrl Pts',(14.7596795019669,11.2628050749281,-320.491332168469)) ;
#37955 = CARTESIAN_POINT('Ctrl Pts',(14.65914671431,11.3935778395313,-320.489225123336)) ;
#37956 = CARTESIAN_POINT('Ctrl Pts',(14.5985031018322,11.4711771673058,-320.487976077157)) ;
#37957 = CARTESIAN_POINT('Ctrl Pts',(14.3220776007096,11.8191477389605,-320.482372436743)) ;
#37958 = CARTESIAN_POINT('Ctrl Pts',(14.0993818595498,12.0839394396551,-320.478099739798)) ;
#37959 = CARTESIAN_POINT('Ctrl Pts',(13.4114930507716,12.8569375986979,-320.465389141573)) ;
#37960 = CARTESIAN_POINT('Ctrl Pts',(12.9252851988334,13.34563575612,-320.457012916148)) ;
#37961 = CARTESIAN_POINT('Ctrl Pts',(12.2511605211432,13.9517367518548,-320.445682427678)) ;
#37962 = CARTESIAN_POINT('Ctrl Pts',(12.0867254424444,14.0944301178278,-320.442941156745)) ;
#37963 = CARTESIAN_POINT('Ctrl Pts',(11.8177536497681,14.3196690143079,-320.438484336524)) ;
#37964 = CARTESIAN_POINT('Ctrl Pts',(11.7147717603235,14.4040391747493,-320.436784210811)) ;
#37965 = CARTESIAN_POINT('Ctrl Pts',(11.5125001822917,14.5661504206842,-320.433455716434)) ;
#37966 = CARTESIAN_POINT('Ctrl Pts',(11.4133081972689,14.6440019962394,-320.43182839283)) ;
#37967 = CARTESIAN_POINT('Ctrl Pts',(11.1911749538968,14.8147169423849,-320.428194514757)) ;
#37968 = CARTESIAN_POINT('Ctrl Pts',(11.0678552826335,14.9070726260846,-320.426184037137)) ;
#37969 = CARTESIAN_POINT('Ctrl Pts',(10.3566271446436,15.426029508022,-320.414629628021)) ;
#37970 = CARTESIAN_POINT('Ctrl Pts',(9.74523493849762,15.8193710177711,-320.404825468476)) ;
#37971 = CARTESIAN_POINT('Ctrl Pts',(8.87248368166176,16.3110191454446,-320.391344698482)) ;
#37972 = CARTESIAN_POINT('Ctrl Pts',(8.62961130768387,16.4408065868858,-320.387648695088)) ;
#37973 = CARTESIAN_POINT('Ctrl Pts',(8.22732415650954,16.6444119517029,-320.38166000695)) ;
#37974 = CARTESIAN_POINT('Ctrl Pts',(8.06958941796149,16.7214544464697,-320.379344713582)) ;
#37975 = CARTESIAN_POINT('Ctrl Pts',(7.83835967058113,16.8303602521073,-320.376010160024)) ;
#37976 = CARTESIAN_POINT('Ctrl Pts',(7.76571364613351,16.8640030873791,-320.374970995909)) ;
#37977 = CARTESIAN_POINT('Ctrl Pts',(7.63232953628261,16.9247294659801,-320.373080012037)) ;
#37978 = CARTESIAN_POINT('Ctrl Pts',(7.57165935167884,16.9519584798445,-320.372226446842)) ;
#37979 = CARTESIAN_POINT('Ctrl Pts',(7.42052451758098,17.0188151541721,-320.370115506499)) ;
#37980 = CARTESIAN_POINT('Ctrl Pts',(7.32988745247924,17.0580480519605,-320.368863002112)) ;
#37981 = CARTESIAN_POINT('Ctrl Pts',(6.98951781796482,17.2021657276769,-320.364202622321)) ;
#37982 = CARTESIAN_POINT('Ctrl Pts',(6.73781223802198,17.3023048136194,-320.360842253274)) ;
#37983 = CARTESIAN_POINT('Ctrl Pts',(5.93778281974094,17.6004840858427,-320.350320760546)) ;
#37984 = CARTESIAN_POINT('Ctrl Pts',(5.38227495244984,17.7782288933439,-320.343237744653)) ;
#37985 = CARTESIAN_POINT('Ctrl Pts',(4.66513129355442,17.9709917254191,-320.334056974556)) ;
#37986 = CARTESIAN_POINT('Ctrl Pts',(4.51040734500845,18.0104474983281,-320.332074898616)) ;
#37987 = CARTESIAN_POINT('Ctrl Pts',(4.13253098029535,18.1016339849885,-320.327223142056)) ;
#37988 = CARTESIAN_POINT('Ctrl Pts',(3.9088931648892,18.1512401554142,-320.324342303235)) ;
#37989 = CARTESIAN_POINT('Ctrl Pts',(3.55196154187433,18.223510262761,-320.319719289467)) ;
#37990 = CARTESIAN_POINT('Ctrl Pts',(3.41923926590918,18.2488783181322,-320.317994848141)) ;
#37991 = CARTESIAN_POINT('Ctrl Pts',(3.16173591308726,18.2951887432147,-320.314637295797)) ;
#37992 = CARTESIAN_POINT('Ctrl Pts',(3.03699427155919,18.31630887691,-320.313005456138)) ;
#37993 = CARTESIAN_POINT('Ctrl Pts',(2.7637991500359,18.3596962199525,-320.309419383519)) ;
#37994 = CARTESIAN_POINT('Ctrl Pts',(2.61527175868124,18.3814413083073,-320.307461892687)) ;
#37995 = CARTESIAN_POINT('Ctrl Pts',(2.00412125681012,18.4633591186382,-320.29937603076)) ;
#37996 = CARTESIAN_POINT('Ctrl Pts',(1.53957503955576,18.5078858438168,-320.293151697139)) ;
#37997 = CARTESIAN_POINT('Ctrl Pts',(0.609758023463925,18.5617562867355,-320.280633701536)) ;
#37998 = CARTESIAN_POINT('Ctrl Pts',(0.144822765875304,18.5712042559841,-320.274345079612)) ;
#37999 = CARTESIAN_POINT('Ctrl Pts',(-0.483448678337892,18.5603746770248,
-320.265951934022)) ;
#38000 = CARTESIAN_POINT('Ctrl Pts',(-0.64687756191638,18.5553976059387,-320.263778772134)) ;
#38001 = CARTESIAN_POINT('Ctrl Pts',(-0.933632067622933,18.5428716840832,
-320.259994451255)) ;
#38002 = CARTESIAN_POINT('Ctrl Pts',(-1.0569879404011,18.5362492349128,-320.258375881455)) ;
#38003 = CARTESIAN_POINT('Ctrl Pts',(-1.25085233263537,18.5238999705078,-320.255851612869)) ;
#38004 = CARTESIAN_POINT('Ctrl Pts',(-1.32140983208596,18.5190004523242,-320.254936960759)) ;
#38005 = CARTESIAN_POINT('Ctrl Pts',(-1.46329132091133,18.5083332051818,-320.253107099174)) ;
#38006 = CARTESIAN_POINT('Ctrl Pts',(-1.53461341402841,18.5025560723666,-320.252192002265)) ;
#38007 = CARTESIAN_POINT('Ctrl Pts',(-1.7331711968201,18.4853167938127,-320.249655611776)) ;
#38008 = CARTESIAN_POINT('Ctrl Pts',(-1.86032474652054,18.4729535073326,-320.248044153148)) ;
#38009 = CARTESIAN_POINT('Ctrl Pts',(-2.18891480000634,18.4375772401306,-320.243902744987)) ;
#38010 = CARTESIAN_POINT('Ctrl Pts',(-2.39012021708224,18.4125752693644,-320.241389082151)) ;
#38011 = CARTESIAN_POINT('Ctrl Pts',(-3.17771190458831,18.3015808766074,-320.231580719873)) ;
#38012 = CARTESIAN_POINT('Ctrl Pts',(-3.76025159372194,18.1908280487864,-320.22438269932)) ;
#38013 = CARTESIAN_POINT('Ctrl Pts',(-4.49291909800089,18.0148288294783,-320.215068573923)) ;
#38014 = CARTESIAN_POINT('Ctrl Pts',(-4.64884789006029,17.9752216397224,-320.21307187091)) ;
#38015 = CARTESIAN_POINT('Ctrl Pts',(-5.02660179785301,17.8740248956172,-320.208191434611)) ;
#38016 = CARTESIAN_POINT('Ctrl Pts',(-5.24783404764432,17.8103264746178,-320.205296515049)) ;
#38017 = CARTESIAN_POINT('Ctrl Pts',(-5.59714391020538,17.7026775184402,-320.200656734144)) ;
#38018 = CARTESIAN_POINT('Ctrl Pts',(-5.726023917642,17.6614116452616,-320.198929846528)) ;
#38019 = CARTESIAN_POINT('Ctrl Pts',(-5.97441671540665,17.5788744734997,-320.19557104091)) ;
#38020 = CARTESIAN_POINT('Ctrl Pts',(-6.09398184177534,17.5377840134527,-320.19394043432)) ;
#38021 = CARTESIAN_POINT('Ctrl Pts',(-6.38062886402289,17.4359878823611,-320.18999722914)) ;
#38022 = CARTESIAN_POINT('Ctrl Pts',(-6.54727667816326,17.3740975618289,-320.187676705245)) ;
#38023 = CARTESIAN_POINT('Ctrl Pts',(-7.47566094617769,17.0140561907429,-320.174593799675)) ;
#38024 = CARTESIAN_POINT('Ctrl Pts',(-8.21793022773138,16.668209995275,-320.163497308287)) ;
#38025 = CARTESIAN_POINT('Ctrl Pts',(-9.11946161975605,16.1732563144482,-320.149700286211)) ;
#38026 = CARTESIAN_POINT('Ctrl Pts',(-9.30222620421671,16.0688328105123,-320.146888760632)) ;
#38027 = CARTESIAN_POINT('Ctrl Pts',(-9.60980196023276,15.8860913964448,-320.142153922907)) ;
#38028 = CARTESIAN_POINT('Ctrl Pts',(-9.73552850381538,15.809354143702,-320.14021756961)) ;
#38029 = CARTESIAN_POINT('Ctrl Pts',(-9.92408759345924,15.691164621376,-320.137319661557)) ;
#38030 = CARTESIAN_POINT('Ctrl Pts',(-9.98760295331322,15.6508130461312,-320.136344591362)) ;
#38031 = CARTESIAN_POINT('Ctrl Pts',(-10.1074959309155,15.5736174671756,-320.134507434476)) ;
#38032 = CARTESIAN_POINT('Ctrl Pts',(-10.1639217189721,15.5368507197949,-320.133644376945)) ;
#38033 = CARTESIAN_POINT('Ctrl Pts',(-10.3110873954476,15.4398135395337,-320.131396121166)) ;
#38034 = CARTESIAN_POINT('Ctrl Pts',(-10.4014991978202,15.3790500325348,-320.130017546942)) ;
#38035 = CARTESIAN_POINT('Ctrl Pts',(-11.0314674816962,14.947567513022,-320.120413206063)) ;
#38036 = CARTESIAN_POINT('Ctrl Pts',(-11.5516223402338,14.5493325418654,-320.112472518047)) ;
#38037 = CARTESIAN_POINT('Ctrl Pts',(-12.4098739769892,13.8171531071765,-320.098624350499)) ;
#38038 = CARTESIAN_POINT('Ctrl Pts',(-12.7582035519693,13.4961821565171,-320.092771396495)) ;
#38039 = CARTESIAN_POINT('Ctrl Pts',(-13.210279238432,13.0464546345825,-320.084735021276)) ;
#38040 = CARTESIAN_POINT('Ctrl Pts',(-13.3251361475084,12.9291222683097,-320.082653044646)) ;
#38041 = CARTESIAN_POINT('Ctrl Pts',(-13.524467222832,12.7200171912822,-320.078965034228)) ;
#38042 = CARTESIAN_POINT('Ctrl Pts',(-13.609601197605,12.6288877656985,-320.077365046512)) ;
#38043 = CARTESIAN_POINT('Ctrl Pts',(-13.7891506476407,12.432769534724,-320.073936245527)) ;
#38044 = CARTESIAN_POINT('Ctrl Pts',(-13.8832996604095,12.3275473777791,-320.072105242701)) ;
#38045 = CARTESIAN_POINT('Ctrl Pts',(-14.1453171039769,12.0279041359731,-320.066914913687)) ;
#38046 = CARTESIAN_POINT('Ctrl Pts',(-14.3103639000479,11.8310590611469,-320.063532611767)) ;
#38047 = CARTESIAN_POINT('Ctrl Pts',(-14.5884607006544,11.4850470709389,-320.057640630475)) ;
#38048 = CARTESIAN_POINT('Ctrl Pts',(-14.7034378217574,11.3374780237061,-320.055144017861)) ;
#38049 = CARTESIAN_POINT('Ctrl Pts',(-15.1423860606155,10.7561931504176,-320.045385567056)) ;
#38050 = CARTESIAN_POINT('Ctrl Pts',(-15.4495560737919,10.3101291325037,-320.038050697572)) ;
#38051 = CARTESIAN_POINT('Ctrl Pts',(-15.8036135586821,9.7445449137338,-320.029126962571)) ;
#38052 = CARTESIAN_POINT('Ctrl Pts',(-15.869344240706,9.6371297856845,-320.027448693463)) ;
#38053 = CARTESIAN_POINT('Ctrl Pts',(-16.0159828418118,9.39192852465593,-320.023661159842)) ;
#38054 = CARTESIAN_POINT('Ctrl Pts',(-16.09621519664,9.25374974218617,-320.021557437177)) ;
#38055 = CARTESIAN_POINT('Ctrl Pts',(-16.2126786293103,9.0470741267786,-320.018465439613)) ;
#38056 = CARTESIAN_POINT('Ctrl Pts',(-16.2502806143696,8.97935847200445,-320.017460954369)) ;
#38057 = CARTESIAN_POINT('Ctrl Pts',(-16.3193593926118,8.85310260965741,-320.015605429166)) ;
#38058 = CARTESIAN_POINT('Ctrl Pts',(-16.3509476261824,8.79462497883068,-320.014753007017)) ;
#38059 = CARTESIAN_POINT('Ctrl Pts',(-16.4308440345105,8.6447985383438,-320.012585677615)) ;
#38060 = CARTESIAN_POINT('Ctrl Pts',(-16.4787048552872,8.55321365298748,-320.011276468719)) ;
#38061 = CARTESIAN_POINT('Ctrl Pts',(-16.6441670106533,8.23004633564286,-320.006703927432)) ;
#38062 = CARTESIAN_POINT('Ctrl Pts',(-16.7576713070831,7.99639987874069,-320.003482091307)) ;
#38063 = CARTESIAN_POINT('Ctrl Pts',(-17.1103923121456,7.22981073568241,-319.993082327014)) ;
#38064 = CARTESIAN_POINT('Ctrl Pts',(-17.3293701326168,6.68794591498471,-319.985985262188)) ;
#38065 = CARTESIAN_POINT('Ctrl Pts',(-17.575264584893,5.98582625184031,-319.976788184808)) ;
#38066 = CARTESIAN_POINT('Ctrl Pts',(-17.6261398215666,5.83431538943539,-319.974804301298)) ;
#38067 = CARTESIAN_POINT('Ctrl Pts',(-17.7451986765086,5.46396872089428,-319.969948997443)) ;
#38068 = CARTESIAN_POINT('Ctrl Pts',(-17.8112982585629,5.24449085423753,-319.967066415359)) ;
#38069 = CARTESIAN_POINT('Ctrl Pts',(-17.909887055619,4.89374186637616,-319.962441325652)) ;
#38070 = CARTESIAN_POINT('Ctrl Pts',(-17.9450350776897,4.76324257159204,-319.960716581303)) ;
#38071 = CARTESIAN_POINT('Ctrl Pts',(-18.0103186816377,4.50986954630541,-319.95735887546)) ;
#38072 = CARTESIAN_POINT('Ctrl Pts',(-18.0406293564702,4.38704851890468,-319.9557271903)) ;
#38073 = CARTESIAN_POINT('Ctrl Pts',(-18.1041437654839,4.11788699634963,-319.952141989477)) ;
#38074 = CARTESIAN_POINT('Ctrl Pts',(-18.1368333566289,3.97143431291526,-319.950185222726)) ;
#38075 = CARTESIAN_POINT('Ctrl Pts',(-18.2637127848125,3.36872762743181,-319.942108617553)) ;
#38076 = CARTESIAN_POINT('Ctrl Pts',(-18.3424887783077,2.90940435395312,-319.935893105163)) ;
#38077 = CARTESIAN_POINT('Ctrl Pts',(-18.4652698419783,1.98619602934424,-319.923375897237)) ;
#38078 = CARTESIAN_POINT('Ctrl Pts',(-18.5092606437092,1.52264088932407,-319.917078982594)) ;
#38079 = CARTESIAN_POINT('Ctrl Pts',(-18.5451061496133,0.894595137415581,
-319.908676350537)) ;
#38080 = CARTESIAN_POINT('Ctrl Pts',(-18.5522689205552,0.73115017494928,-319.906501870915)) ;
#38081 = CARTESIAN_POINT('Ctrl Pts',(-18.5610490294874,0.44410695793475,-319.902715543493)) ;
#38082 = CARTESIAN_POINT('Ctrl Pts',(-18.5635939829878,0.320547305205466,
-319.901096274562)) ;
#38083 = CARTESIAN_POINT('Ctrl Pts',(-18.5656555770196,0.126238340883433,
-319.898571178995)) ;
#38084 = CARTESIAN_POINT('Ctrl Pts',(-18.5660017969246,0.0555015476074166,
-319.897656389765)) ;
#38085 = CARTESIAN_POINT('Ctrl Pts',(-18.565892430471,-0.0777715679331076,
-319.895942380189)) ;
#38086 = CARTESIAN_POINT('Ctrl Pts',(-18.5655251508092,-0.140306960566763,
-319.8951420525)) ;
#38087 = CARTESIAN_POINT('Ctrl Pts',(-18.5635716173354,-0.319103830453604,
-319.892863653786)) ;
#38088 = CARTESIAN_POINT('Ctrl Pts',(-18.5612091587844,-0.435353963888956,
-319.891394174298)) ;
#38089 = CARTESIAN_POINT('Ctrl Pts',(-18.5441401948836,-1.00964037652752,
-319.884178693673)) ;
#38090 = CARTESIAN_POINT('Ctrl Pts',(-18.5135703148142,-1.46704658749342,
-319.878565864524)) ;
#38091 = CARTESIAN_POINT('Ctrl Pts',(-18.4216939222867,-2.34938104204668,
-319.867700069148)) ;
#38092 = CARTESIAN_POINT('Ctrl Pts',(-18.3625155757877,-2.77424216081369,
-319.862450586824)) ;
#38093 = CARTESIAN_POINT('Ctrl Pts',(-18.2396021542069,-3.47744987903692,
-319.853591866354)) ;
#38094 = CARTESIAN_POINT('Ctrl Pts',(-18.1840656208683,-3.75706020909621,
-319.850024908786)) ;
#38095 = CARTESIAN_POINT('Ctrl Pts',(-18.0907345996278,-4.17620217944348,
-319.844589062615)) ;
#38096 = CARTESIAN_POINT('Ctrl Pts',(-18.0577126689862,-4.31675295616627,
-319.842751183851)) ;
#38097 = CARTESIAN_POINT('Ctrl Pts',(-17.9932269219158,-4.57752368870319,
-319.839311280314)) ;
#38098 = CARTESIAN_POINT('Ctrl Pts',(-17.9621889324688,-4.69784066218678,
-319.837712177261)) ;
#38099 = CARTESIAN_POINT('Ctrl Pts',(-17.8886843298084,-4.97139361828649,
-319.834048425729)) ;
#38100 = CARTESIAN_POINT('Ctrl Pts',(-17.8454522205785,-5.12441377104221,
-319.831978780777)) ;
#38101 = CARTESIAN_POINT('Ctrl Pts',(-17.6940060998695,-5.63528208216325,
-319.825001598787)) ;
#38102 = CARTESIAN_POINT('Ctrl Pts',(-17.5769511157485,-5.99041269765255,
-319.820037838604)) ;
#38103 = CARTESIAN_POINT('Ctrl Pts',(-17.2603757059369,-6.861464245383,-319.807628695331)) ;
#38104 = CARTESIAN_POINT('Ctrl Pts',(-17.0483734140392,-7.37246388527609,
-319.800134949259)) ;
#38105 = CARTESIAN_POINT('Ctrl Pts',(-16.7599433945097,-7.98842756413033,
-319.791037471443)) ;
#38106 = CARTESIAN_POINT('Ctrl Pts',(-16.704822356033,-8.10306038711319,-319.789342052749)) ;
#38107 = CARTESIAN_POINT('Ctrl Pts',(-16.5773406620451,-8.36134833742875,
-319.785523086718)) ;
#38108 = CARTESIAN_POINT('Ctrl Pts',(-16.5042822578401,-8.50464794964898,
-319.783405070073)) ;
#38109 = CARTESIAN_POINT('Ctrl Pts',(-16.3932121144931,-8.71568261505193,
-319.780296587227)) ;
#38110 = CARTESIAN_POINT('Ctrl Pts',(-16.3566226176274,-8.78415752611084,
-319.779289671204)) ;
#38111 = CARTESIAN_POINT('Ctrl Pts',(-16.2879425561549,-8.91077079807433,
-319.777432454845)) ;
#38112 = CARTESIAN_POINT('Ctrl Pts',(-16.2559675707652,-8.96897024506396,
-319.776580739249)) ;
#38113 = CARTESIAN_POINT('Ctrl Pts',(-16.1820483866412,-9.10182076837794,
-319.774640078183)) ;
#38114 = CARTESIAN_POINT('Ctrl Pts',(-16.139898573098,-9.17635577798928,-319.773553776277)) ;
#38115 = CARTESIAN_POINT('Ctrl Pts',(-15.9512794075741,-9.50457752352469,
-319.768775824324)) ;
#38116 = CARTESIAN_POINT('Ctrl Pts',(-15.7993333548143,-9.75506919028073,
-319.765143881003)) ;
#38117 = CARTESIAN_POINT('Ctrl Pts',(-15.3328906526168,-10.484520915646,-319.754481175163)) ;
#38118 = CARTESIAN_POINT('Ctrl Pts',(-15.002082097532,-10.9526365997029,-319.747517034356)) ;
#38119 = CARTESIAN_POINT('Ctrl Pts',(-14.5528637001184,-11.5296897142065,
-319.738474438905)) ;
#38120 = CARTESIAN_POINT('Ctrl Pts',(-14.4539724684033,-11.6534229559753,
-319.736507892625)) ;
#38121 = CARTESIAN_POINT('Ctrl Pts',(-14.2090024684019,-11.9520147148731,
-319.731686649185)) ;
#38122 = CARTESIAN_POINT('Ctrl Pts',(-14.0612649826143,-12.1254787001854,
-319.728820825041)) ;
#38123 = CARTESIAN_POINT('Ctrl Pts',(-13.8210240906026,-12.3972574560836,
-319.72421569102)) ;
#38124 = CARTESIAN_POINT('Ctrl Pts',(-13.7305764707638,-12.4973584833696,
-319.722493860154)) ;
#38125 = CARTESIAN_POINT('Ctrl Pts',(-13.5531442360367,-12.6894763878504,
-319.719137606224)) ;
#38126 = CARTESIAN_POINT('Ctrl Pts',(-13.4662933705959,-12.7816068036632,
-319.717504411412)) ;
#38127 = CARTESIAN_POINT('Ctrl Pts',(-13.2741031281485,-12.9813465810857,
-319.713910725803)) ;
#38128 = CARTESIAN_POINT('Ctrl Pts',(-13.1683831970627,-13.0885773406175,
-319.711946917912)) ;
#38129 = CARTESIAN_POINT('Ctrl Pts',(-12.7379436134082,-13.5146735673453,
-319.704003837386)) ;
#38130 = CARTESIAN_POINT('Ctrl Pts',(-12.4028549722467,-13.8228360181523,
-319.697934104992)) ;
#38131 = CARTESIAN_POINT('Ctrl Pts',(-11.6974120629538,-14.4252689156461,
-319.685469289314)) ;
#38132 = CARTESIAN_POINT('Ctrl Pts',(-11.3264540185173,-14.7183311354844,
-319.679075101517)) ;
#38133 = CARTESIAN_POINT('Ctrl Pts',(-10.8116620103455,-15.0940252359024,
-319.670561337337)) ;
#38134 = CARTESIAN_POINT('Ctrl Pts',(-10.6773175397551,-15.1893555993554,
-319.668371545987)) ;
#38135 = CARTESIAN_POINT('Ctrl Pts',(-10.4394931789651,-15.3534004271312,
-319.6645619171)) ;
#38136 = CARTESIAN_POINT('Ctrl Pts',(-10.3365590904613,-15.4228878215087,
-319.662934538102)) ;
#38137 = CARTESIAN_POINT('Ctrl Pts',(-10.173813684113,-15.5303906930307,-319.660399847607)) ;
#38138 = CARTESIAN_POINT('Ctrl Pts',(-10.1144687461817,-15.5691053680162,
-319.659483465818)) ;
#38139 = CARTESIAN_POINT('Ctrl Pts',(-10.002405234924,-15.6413007412492,-319.657768944831)) ;
#38140 = CARTESIAN_POINT('Ctrl Pts',(-9.94973653430783,-15.6748570096053,
-319.656969675867)) ;
#38141 = CARTESIAN_POINT('Ctrl Pts',(-9.79895508253931,-15.7698566859488,
-319.654698711009)) ;
#38142 = CARTESIAN_POINT('Ctrl Pts',(-9.70043552433415,-15.8306491119577,
-319.653235518469)) ;
#38143 = CARTESIAN_POINT('Ctrl Pts',(-9.40632503290428,-16.0083562950231,
-319.64891953732)) ;
#38144 = CARTESIAN_POINT('Ctrl Pts',(-9.20914307031659,-16.1225961346538,
-319.646093371657)) ;
#38145 = CARTESIAN_POINT('Ctrl Pts',(-8.64613809009402,-16.4350810524499,
-319.638154393099)) ;
#38146 = CARTESIAN_POINT('Ctrl Pts',(-8.27568391531246,-16.6246999785226,
-319.633080757162)) ;
#38147 = CARTESIAN_POINT('Ctrl Pts',(-7.5688576005142,-16.9570079515821,-319.623492563115)) ;
#38148 = CARTESIAN_POINT('Ctrl Pts',(-7.23403506658379,-17.1025278850562,
-319.618988307289)) ;
#38149 = CARTESIAN_POINT('Ctrl Pts',(-6.6972691184655,-17.3172314106357,-319.611758369888)) ;
#38150 = CARTESIAN_POINT('Ctrl Pts',(-6.49804868953566,-17.3929664053021,
-319.609073489313)) ;
#38151 = CARTESIAN_POINT('Ctrl Pts',(-6.17309444926559,-17.5101374257881,
-319.604683771035)) ;
#38152 = CARTESIAN_POINT('Ctrl Pts',(-6.04814383133484,-17.5536880422411,
-319.602993458984)) ;
#38153 = CARTESIAN_POINT('Ctrl Pts',(-5.80277073989572,-17.6362800502884,
-319.599668181251)) ;
#38154 = CARTESIAN_POINT('Ctrl Pts',(-5.68239329096042,-17.6754329142077,
-319.59803408364)) ;
#38155 = CARTESIAN_POINT('Ctrl Pts',(-5.41250614154726,-17.7601718807105,
-319.594363822718)) ;
#38156 = CARTESIAN_POINT('Ctrl Pts',(-5.26280218775656,-17.8051071605327,
-319.592323450258)) ;
#38157 = CARTESIAN_POINT('Ctrl Pts',(-4.43492343116874,-18.0422505832194,
-319.581016970826)) ;
#38158 = CARTESIAN_POINT('Ctrl Pts',(-3.74679571311203,-18.1976060495182,
-319.571509207816)) ;
#38159 = CARTESIAN_POINT('Ctrl Pts',(-2.77012693716534,-18.3603450587266,
-319.558180557617)) ;
#38160 = CARTESIAN_POINT('Ctrl Pts',(-2.48770068963297,-18.4007396459706,
-319.554349056747)) ;
#38161 = CARTESIAN_POINT('Ctrl Pts',(-2.02628186463724,-18.4559172401889,
-319.54817395547)) ;
#38162 = CARTESIAN_POINT('Ctrl Pts',(-1.84780794830388,-18.4746395189185,
-319.545806134378)) ;
#38163 = CARTESIAN_POINT('Ctrl Pts',(-1.58874576667963,-18.4980240611802,
-319.542411836864)) ;
#38164 = CARTESIAN_POINT('Ctrl Pts',(-1.50835451975316,-18.5047527393947,
-319.541364490148)) ;
#38165 = CARTESIAN_POINT('Ctrl Pts',(-1.36174630030572,-18.5160619918388,
-319.539466910562)) ;
#38166 = CARTESIAN_POINT('Ctrl Pts',(-1.29554393291029,-18.520811823039,-319.538614824716)) ;
#38167 = CARTESIAN_POINT('Ctrl Pts',(-1.13185198966875,-18.531674285358,-319.536518965107)) ;
#38168 = CARTESIAN_POINT('Ctrl Pts',(-1.03433692062121,-18.5373727350905,
-319.535279887093)) ;
#38169 = CARTESIAN_POINT('Ctrl Pts',(-0.609092997731742,-18.5588566148113,
-319.52990989548)) ;
#38170 = CARTESIAN_POINT('Ctrl Pts',(-0.281022531967197,-18.5667223936328,
-319.525852426534)) ;
#38171 = CARTESIAN_POINT('Ctrl Pts',(0.184118473903266,-18.5655427690672,
-319.520134623313)) ;
#38172 = CARTESIAN_POINT('Ctrl Pts',(0.32114476542577,-18.5636780833577,-319.518454656876)) ;
#38173 = CARTESIAN_POINT('Ctrl Pts',(0.906303355729485,-18.5492341708577,
-319.511283498925)) ;
#38174 = CARTESIAN_POINT('Ctrl Pts',(1.35392106694975,-18.5219429732882,-319.505801602371)) ;
#38175 = CARTESIAN_POINT('Ctrl Pts',(1.93881339966618,-18.4649647457342,-319.498513547611)) ;
#38176 = CARTESIAN_POINT('Ctrl Pts',(2.07735962557479,-18.4498915279457,-319.496778316142)) ;
#38177 = CARTESIAN_POINT('Ctrl Pts',(2.4232214954552,-18.4083180858861,-319.492419424493)) ;
#38178 = CARTESIAN_POINT('Ctrl Pts',(2.63028384640021,-18.3798744239215,-319.489785269557)) ;
#38179 = CARTESIAN_POINT('Ctrl Pts',(2.96687142071308,-18.3278337687785,-319.485455853957)) ;
#38180 = CARTESIAN_POINT('Ctrl Pts',(3.09670373300719,-18.3063443268507,-319.483774328255)) ;
#38181 = CARTESIAN_POINT('Ctrl Pts',(3.35144072665906,-18.261393517356,-319.480451165037)) ;
#38182 = CARTESIAN_POINT('Ctrl Pts',(3.47635483074433,-18.2380263508963,-319.478810229669)) ;
#38183 = CARTESIAN_POINT('Ctrl Pts',(3.78749123606108,-18.1765106842142,-319.474694034491)) ;
#38184 = CARTESIAN_POINT('Ctrl Pts',(3.97338594814523,-18.1367812592745,-319.472208647292)) ;
#38185 = CARTESIAN_POINT('Ctrl Pts',(4.51494083217563,-18.0123143075917,-319.464893868234)) ;
#38186 = CARTESIAN_POINT('Ctrl Pts',(4.86874678467191,-17.9199180008609,-319.460019296871)) ;
#38187 = CARTESIAN_POINT('Ctrl Pts',(5.61655142170223,-17.7008459997476,-319.449560612637)) ;
#38188 = CARTESIAN_POINT('Ctrl Pts',(6.00951244052909,-17.5713220583901,-319.443969806547)) ;
#38189 = CARTESIAN_POINT('Ctrl Pts',(6.69232682536536,-17.3206721569203,-319.434207699202)) ;
#38190 = CARTESIAN_POINT('Ctrl Pts',(6.9840484788382,-17.2051152236083,-319.430022090306)) ;
#38191 = CARTESIAN_POINT('Ctrl Pts',(7.36171656553722,-17.0443242295472,-319.42464046336)) ;
#38192 = CARTESIAN_POINT('Ctrl Pts',(7.45043366801918,-17.0057313112646,-319.423379084769)) ;
#38193 = CARTESIAN_POINT('Ctrl Pts',(7.59940488049363,-16.939537669084,-319.42126824932)) ;
#38194 = CARTESIAN_POINT('Ctrl Pts',(7.65982011193505,-16.9123045994988,-319.420414305255)) ;
#38195 = CARTESIAN_POINT('Ctrl Pts',(7.79396136092571,-16.8509721901524,-319.418523451429)) ;
#38196 = CARTESIAN_POINT('Ctrl Pts',(7.86761186664843,-16.8167113607032,-319.417488532541)) ;
#38197 = CARTESIAN_POINT('Ctrl Pts',(8.10650110863314,-16.7036717068692,-319.414138908742)) ;
#38198 = CARTESIAN_POINT('Ctrl Pts',(8.27080026357403,-16.6229321097865,-319.411846339661)) ;
#38199 = CARTESIAN_POINT('Ctrl Pts',(8.69638681670377,-16.4059191721764,-319.405907796482)) ;
#38200 = CARTESIAN_POINT('Ctrl Pts',(8.95567135540168,-16.2658316285078,-319.402289274278)) ;
#38201 = CARTESIAN_POINT('Ctrl Pts',(9.80633387742465,-15.7797232771298,-319.39028165961)) ;
#38202 = CARTESIAN_POINT('Ctrl Pts',(10.381886077836,-15.4071506637186,-319.381914294169)) ;
#38203 = CARTESIAN_POINT('Ctrl Pts',(11.0774515813883,-14.900181513698,-319.371089710774)) ;
#38204 = CARTESIAN_POINT('Ctrl Pts',(11.2179016110272,-14.7947296694031,-319.368866679468)) ;
#38205 = CARTESIAN_POINT('Ctrl Pts',(11.4566050793388,-14.6101541862775,-319.365019752049)) ;
#38206 = CARTESIAN_POINT('Ctrl Pts',(11.5555871827429,-14.5319926403659,-319.363403729201)) ;
#38207 = CARTESIAN_POINT('Ctrl Pts',(11.7596883324532,-14.3674195379613,-319.360026884995)) ;
#38208 = CARTESIAN_POINT('Ctrl Pts',(11.864669301118,-14.2808485799772,-319.358264795079)) ;
#38209 = CARTESIAN_POINT('Ctrl Pts',(12.1479463653666,-14.0419685916833,-319.353440471498)) ;
#38210 = CARTESIAN_POINT('Ctrl Pts',(12.3243235517851,-13.8874235009306,-319.350359918428)) ;
#38211 = CARTESIAN_POINT('Ctrl Pts',(12.7275846140105,-13.5203440707657,-319.343141018793)) ;
#38212 = CARTESIAN_POINT('Ctrl Pts',(12.9521523391632,-13.3053697101697,-319.338985534863)) ;
#38213 = CARTESIAN_POINT('Ctrl Pts',(13.6407228177951,-12.6122548185456,-319.325860348181)) ;
#38214 = CARTESIAN_POINT('Ctrl Pts',(14.0844514653631,-12.1147231422276,-319.316812260794)) ;
#38215 = CARTESIAN_POINT('Ctrl Pts',(14.5705253646179,-11.5068184638548,-319.306572258987)) ;
#38216 = CARTESIAN_POINT('Ctrl Pts',(14.6397775653115,-11.4185810614698,-319.305105374053)) ;
#38217 = CARTESIAN_POINT('Ctrl Pts',(14.745969058318,-11.2807234377254,-319.302847068333)) ;
#38218 = CARTESIAN_POINT('Ctrl Pts',(14.7834671033498,-11.231537079516,-319.302047844628)) ;
#38219 = CARTESIAN_POINT('Ctrl Pts',(14.8639491190266,-11.124867092156,-319.300329470611)) ;
#38220 = CARTESIAN_POINT('Ctrl Pts',(14.9068469414477,-11.0673197077355,-319.299411641926)) ;
#38221 = CARTESIAN_POINT('Ctrl Pts',(15.0258371940304,-10.9057474257479,-319.296858298652)) ;
#38222 = CARTESIAN_POINT('Ctrl Pts',(15.1011817947939,-10.8011767312512,-319.295232829479)) ;
#38223 = CARTESIAN_POINT('Ctrl Pts',(15.275425437824,-10.5539567868967,-319.291443501416)) ;
#38224 = CARTESIAN_POINT('Ctrl Pts',(15.3734250283514,-10.4106882194146,-319.289288527965)) ;
#38225 = CARTESIAN_POINT('Ctrl Pts',(15.7641603301079,-9.8219095264266,-319.280560743145)) ;
#38226 = CARTESIAN_POINT('Ctrl Pts',(16.0396538267447,-9.36526370183947,-319.274078941908)) ;
#38227 = CARTESIAN_POINT('Ctrl Pts',(16.4035580828228,-8.69879218013309,-319.26472978127)) ;
#38228 = CARTESIAN_POINT('Ctrl Pts',(16.5083598094517,-8.49822095449446,-319.261931090967)) ;
#38229 = CARTESIAN_POINT('Ctrl Pts',(16.7178267743022,-8.07883505314419,-319.256089054779)) ;
#38230 = CARTESIAN_POINT('Ctrl Pts',(16.8219233848406,-7.85978378745533,-319.253043061591)) ;
#38231 = CARTESIAN_POINT('Ctrl Pts',(16.9782519439022,-7.51347810882402,-319.248223499294)) ;
#38232 = CARTESIAN_POINT('Ctrl Pts',(17.0334118875921,-7.38757549961326,-319.246470563163)) ;
#38233 = CARTESIAN_POINT('Ctrl Pts',(17.1363014433096,-7.14544993472415,-319.243096539011)) ;
#38234 = CARTESIAN_POINT('Ctrl Pts',(17.1842594079578,-7.02933214983275,-319.241477171997)) ;
#38235 = CARTESIAN_POINT('Ctrl Pts',(17.2950886627656,-6.7530735753301,-319.237620909285)) ;
#38236 = CARTESIAN_POINT('Ctrl Pts',(17.3569198759194,-6.59252810801264,-319.235376999484)) ;
#38237 = CARTESIAN_POINT('Ctrl Pts',(17.6149749324984,-5.89367627372671,-319.225598438985)) ;
#38238 = CARTESIAN_POINT('Ctrl Pts',(17.788452638621,-5.34730871639522,-319.217915196714)) ;
#38239 = CARTESIAN_POINT('Ctrl Pts',(18.0737427564873,-4.27987248603568,-319.203034167735)) ;
#38240 = CARTESIAN_POINT('Ctrl Pts',(18.1889466423228,-3.76028014806394,-319.195849853529)) ;
#38241 = CARTESIAN_POINT('Ctrl Pts',(18.3010007757784,-3.12732376796146,-319.187395377202)) ;
#38242 = CARTESIAN_POINT('Ctrl Pts',(18.31934380851,-3.01801686980458,-319.185946268824)) ;
#38243 = CARTESIAN_POINT('Ctrl Pts',(18.3463625236249,-2.847679797751,-319.183708439823)) ;
#38244 = CARTESIAN_POINT('Ctrl Pts',(18.3557148824173,-2.78675963328895,-319.182912139066)) ;
#38245 = CARTESIAN_POINT('Ctrl Pts',(18.3753571557655,-2.65442178406473,-319.181191952716)) ;
#38246 = CARTESIAN_POINT('Ctrl Pts',(18.3855344372085,-2.58298840221,-319.180269455555)) ;
#38247 = CARTESIAN_POINT('Ctrl Pts',(18.4129916835092,-2.38187963893132,-319.177687144177)) ;
#38248 = CARTESIAN_POINT('Ctrl Pts',(18.4293178689586,-2.25207822311147,-319.17603773838)) ;
#38249 = CARTESIAN_POINT('Ctrl Pts',(18.4645347151988,-1.94599252276742,-319.172178934301)) ;
#38250 = CARTESIAN_POINT('Ctrl Pts',(18.4822748975798,-1.76958862527774,-319.169978865435)) ;
#38251 = CARTESIAN_POINT('Ctrl Pts',(18.5176691574958,-1.35858909876342,-319.164885897476)) ;
#38252 = CARTESIAN_POINT('Ctrl Pts',(18.5333937718384,-1.1238874679167,-319.162002294695)) ;
#38253 = CARTESIAN_POINT('Ctrl Pts',(18.5446545942648,-0.888979967104711,
-319.159121327827)) ;
#38254 = CARTESIAN_POINT('',(18.5446545933324,-0.888979986554686,-320.363441000746)) ;
#38255 = CARTESIAN_POINT('Ctrl Pts',(18.5446545937441,-0.888979977966572,
-318.864005972278)) ;
#38256 = CARTESIAN_POINT('Ctrl Pts',(18.5239048097641,-1.3218328951763,-318.869333195369)) ;
#38257 = CARTESIAN_POINT('Ctrl Pts',(18.4880064180289,-1.75382819271705,-318.874616863806)) ;
#38258 = CARTESIAN_POINT('Ctrl Pts',(18.4044894733845,-2.45881100342708,-318.88335565816)) ;
#38259 = CARTESIAN_POINT('Ctrl Pts',(18.3658215259591,-2.73268799347742,-318.886778748155)) ;
#38260 = CARTESIAN_POINT('Ctrl Pts',(18.2859291398535,-3.21968332545473,-318.892947460273)) ;
#38261 = CARTESIAN_POINT('Ctrl Pts',(18.247058481313,-3.43313585008995,-318.895679448152)) ;
#38262 = CARTESIAN_POINT('Ctrl Pts',(18.1783537986686,-3.77619129929169,-318.900124312305)) ;
#38263 = CARTESIAN_POINT('Ctrl Pts',(18.1508526438783,-3.90624062201917,-318.901821897016)) ;
#38264 = CARTESIAN_POINT('Ctrl Pts',(18.0945574417779,-4.15901155331034,-318.905147258973)) ;
#38265 = CARTESIAN_POINT('Ctrl Pts',(18.0659054235743,-4.28175749982331,-318.90677401269)) ;
#38266 = CARTESIAN_POINT('Ctrl Pts',(17.9923492921944,-4.58298319144293,-318.910796174569)) ;
#38267 = CARTESIAN_POINT('Ctrl Pts',(17.9460370604387,-4.76110508698323,-318.913200715102)) ;
#38268 = CARTESIAN_POINT('Ctrl Pts',(17.7265757794533,-5.5564296008708,-318.924052056488)) ;
#38269 = CARTESIAN_POINT('Ctrl Pts',(17.5241802006144,-6.16510352217633,-318.932685717344)) ;
#38270 = CARTESIAN_POINT('Ctrl Pts',(17.1769661461046,-7.05293303398665,-318.945526639362)) ;
#38271 = CARTESIAN_POINT('Ctrl Pts',(17.0558999419879,-7.34086560802061,-318.949728053781)) ;
#38272 = CARTESIAN_POINT('Ctrl Pts',(16.8497562788778,-7.79847157723484,-318.956405112556)) ;
#38273 = CARTESIAN_POINT('Ctrl Pts',(16.7692403530135,-7.97013323646255,-318.958909612272)) ;
#38274 = CARTESIAN_POINT('Ctrl Pts',(16.6500923380935,-8.21435767579969,-318.96245758868)) ;
#38275 = CARTESIAN_POINT('Ctrl Pts',(16.6135858120306,-8.28794385748215,-318.963524590733)) ;
#38276 = CARTESIAN_POINT('Ctrl Pts',(16.546846235046,-8.42025781307905,-318.965437823793)) ;
#38277 = CARTESIAN_POINT('Ctrl Pts',(16.5167859451356,-8.47907093999281,-318.966286174342)) ;
#38278 = CARTESIAN_POINT('Ctrl Pts',(16.4427167561653,-8.6220991529967,-318.968344868961)) ;
#38279 = CARTESIAN_POINT('Ctrl Pts',(16.3983739621138,-8.70613918814556,-318.969550937377)) ;
#38280 = CARTESIAN_POINT('Ctrl Pts',(16.2205951974769,-9.03689454864697,-318.974290075635)) ;
#38281 = CARTESIAN_POINT('Ctrl Pts',(16.0822205171451,-9.28091350691477,-318.977770166413)) ;
#38282 = CARTESIAN_POINT('Ctrl Pts',(15.6399177203402,-10.0212837031289,-318.988397161506)) ;
#38283 = CARTESIAN_POINT('Ctrl Pts',(15.3181414640535,-10.5065549443357,-318.995468369947)) ;
#38284 = CARTESIAN_POINT('Ctrl Pts',(14.8797779206677,-11.1046011832239,-319.004635630996)) ;
#38285 = CARTESIAN_POINT('Ctrl Pts',(14.783794185736,-11.2320696137224,-319.006616357578)) ;
#38286 = CARTESIAN_POINT('Ctrl Pts',(14.5461054389716,-11.5393994283668,-319.011465613476)) ;
#38287 = CARTESIAN_POINT('Ctrl Pts',(14.4026933545458,-11.7179070856838,-319.014345302267)) ;
#38288 = CARTESIAN_POINT('Ctrl Pts',(14.1694589055316,-11.997465981152,-319.018967081999)) ;
#38289 = CARTESIAN_POINT('Ctrl Pts',(14.0817712212364,-12.1002675529442,-319.020691460425)) ;
#38290 = CARTESIAN_POINT('Ctrl Pts',(13.9098038311551,-12.297474089388,-319.024049279851)) ;
#38291 = CARTESIAN_POINT('Ctrl Pts',(13.8256655979386,-12.3919926694717,-319.02568145373)) ;
#38292 = CARTESIAN_POINT('Ctrl Pts',(13.639572904166,-12.5967894220402,-319.029268804922)) ;
#38293 = CARTESIAN_POINT('Ctrl Pts',(13.5372333057059,-12.7067055954676,-319.031227247094)) ;
#38294 = CARTESIAN_POINT('Ctrl Pts',(13.0724397191812,-13.1939204721091,-319.040057222058)) ;
#38295 = CARTESIAN_POINT('Ctrl Pts',(12.6954692369816,-13.5570378521579,-319.047053511322)) ;
#38296 = CARTESIAN_POINT('Ctrl Pts',(11.9251716007837,-14.2386876796208,-319.060895070699)) ;
#38297 = CARTESIAN_POINT('Ctrl Pts',(11.5331545114255,-14.5580318682217,-319.067730678607)) ;
#38298 = CARTESIAN_POINT('Ctrl Pts',(10.9973180109475,-14.9592912561138,-319.076609754852)) ;
#38299 = CARTESIAN_POINT('Ctrl Pts',(10.8647411462511,-15.055855947113,-319.07877023523)) ;
#38300 = CARTESIAN_POINT('Ctrl Pts',(10.6670956887502,-15.1958442549146,-319.081927826572)) ;
#38301 = CARTESIAN_POINT('Ctrl Pts',(10.603004345948,-15.2406335798324,-319.082942097779)) ;
#38302 = CARTESIAN_POINT('Ctrl Pts',(10.4834563925153,-15.3230588660487,-319.08481465851)) ;
#38303 = CARTESIAN_POINT('Ctrl Pts',(10.4280753705299,-15.3608018997376,-319.085674355254)) ;
#38304 = CARTESIAN_POINT('Ctrl Pts',(10.3016989706831,-15.4459309617981,-319.087619519784)) ;
#38305 = CARTESIAN_POINT('Ctrl Pts',(10.2305786917239,-15.4931289486109,-319.088702465644)) ;
#38306 = CARTESIAN_POINT('Ctrl Pts',(9.91942702799352,-15.6965437156434,-319.093394791924)) ;
#38307 = CARTESIAN_POINT('Ctrl Pts',(9.67612421714811,-15.8476855722377,-319.096947218304)) ;
#38308 = CARTESIAN_POINT('Ctrl Pts',(8.93132554843639,-16.2868127060859,-319.107598774921)) ;
#38309 = CARTESIAN_POINT('Ctrl Pts',(8.41978122199558,-16.5570567921206,-319.114626111497)) ;
#38310 = CARTESIAN_POINT('Ctrl Pts',(7.75249401370287,-16.8706443234602,-319.123742170205)) ;
#38311 = CARTESIAN_POINT('Ctrl Pts',(7.60766347017833,-16.9364476727888,-319.125717009088)) ;
#38312 = CARTESIAN_POINT('Ctrl Pts',(7.25278532580786,-17.0922149173546,-319.13055458758)) ;
#38313 = CARTESIAN_POINT('Ctrl Pts',(7.04188822126367,-17.1801779900213,-319.133428469975)) ;
#38314 = CARTESIAN_POINT('Ctrl Pts',(6.70385988599226,-17.3138960061632,-319.138043293821)) ;
#38315 = CARTESIAN_POINT('Ctrl Pts',(6.57776006256005,-17.3621946993573,-319.139766622674)) ;
#38316 = CARTESIAN_POINT('Ctrl Pts',(6.33246014012001,-17.4530933715797,-319.143123834731)) ;
#38317 = CARTESIAN_POINT('Ctrl Pts',(6.21332904144026,-17.4958584194064,-319.144756467252)) ;
#38318 = CARTESIAN_POINT('Ctrl Pts',(5.92497661617308,-17.5960530429265,-319.148714024358)) ;
#38319 = CARTESIAN_POINT('Ctrl Pts',(5.7553454206456,-17.6522641474869,-319.151047022867)) ;
#38320 = CARTESIAN_POINT('Ctrl Pts',(5.19428110401107,-17.8292381395432,-319.158777857256)) ;
#38321 = CARTESIAN_POINT('Ctrl Pts',(4.79966281914314,-17.9394962072996,-319.164240477413)) ;
#38322 = CARTESIAN_POINT('Ctrl Pts',(4.34704079716518,-18.0499557855242,-319.170497486158)) ;
#38323 = CARTESIAN_POINT('Ctrl Pts',(4.2922988829226,-18.0630517313536,-319.171254036483)) ;
#38324 = CARTESIAN_POINT('Ctrl Pts',(4.00531255431341,-18.1303293866809,-319.175218521963)) ;
#38325 = CARTESIAN_POINT('Ctrl Pts',(3.77209965359929,-18.1802815296054,-319.178434477915)) ;
#38326 = CARTESIAN_POINT('Ctrl Pts',(3.26537600469475,-18.2786470384953,-319.185381663846)) ;
#38327 = CARTESIAN_POINT('Ctrl Pts',(2.99160923062968,-18.3254438562568,-319.189109913104)) ;
#38328 = CARTESIAN_POINT('Ctrl Pts',(2.54231816375434,-18.3919075158911,-319.195143130723)) ;
#38329 = CARTESIAN_POINT('Ctrl Pts',(2.36738082938012,-18.4152423800399,-319.197471087954)) ;
#38330 = CARTESIAN_POINT('Ctrl Pts',(2.1124902818856,-18.4455500741961,-319.200820085025)) ;
#38331 = CARTESIAN_POINT('Ctrl Pts',(2.03278269999845,-18.4545042536832,-319.201861259473)) ;
#38332 = CARTESIAN_POINT('Ctrl Pts',(1.88692394427232,-18.4699332684472,-319.203753809782)) ;
#38333 = CARTESIAN_POINT('Ctrl Pts',(1.82079142166774,-18.4765699063621,-319.204606957925)) ;
#38334 = CARTESIAN_POINT('Ctrl Pts',(1.65658055377771,-18.4921588663495,-319.206713994954)) ;
#38335 = CARTESIAN_POINT('Ctrl Pts',(1.55846388479071,-18.5006861772765,-319.207963057453)) ;
#38336 = CARTESIAN_POINT('Ctrl Pts',(1.11695386597697,-18.5355205690204,-319.213547498424)) ;
#38337 = CARTESIAN_POINT('Ctrl Pts',(0.772935634072581,-18.5530504317124,
-319.217801750189)) ;
#38338 = CARTESIAN_POINT('Ctrl Pts',(0.0158926184002063,-18.5705328095592,
-319.227103965614)) ;
#38339 = CARTESIAN_POINT('Ctrl Pts',(-0.397046604407999,-18.5662946116803,
-319.232140091817)) ;
#38340 = CARTESIAN_POINT('Ctrl Pts',(-1.08685987030517,-18.5361891927507,
-319.240638798175)) ;
#38341 = CARTESIAN_POINT('Ctrl Pts',(-1.36391251313407,-18.5178647928887,
-319.244074712797)) ;
#38342 = CARTESIAN_POINT('Ctrl Pts',(-1.85715757030585,-18.4741115369794,
-319.250263933246)) ;
#38343 = CARTESIAN_POINT('Ctrl Pts',(-2.07351069451286,-18.4510808485935,
-319.253003468106)) ;
#38344 = CARTESIAN_POINT('Ctrl Pts',(-2.4214855428232,-18.4078412859056,-319.257458108734)) ;
#38345 = CARTESIAN_POINT('Ctrl Pts',(-2.5533819388906,-18.3900096153762,-319.25915781626)) ;
#38346 = CARTESIAN_POINT('Ctrl Pts',(-2.80983972785376,-18.3525256808239,
-319.262485879989)) ;
#38347 = CARTESIAN_POINT('Ctrl Pts',(-2.93441526355954,-18.3330195322253,
-319.264113195574)) ;
#38348 = CARTESIAN_POINT('Ctrl Pts',(-3.21077512143554,-18.2868578189954,
-319.267747536089)) ;
#38349 = CARTESIAN_POINT('Ctrl Pts',(-3.36244578582736,-18.2595784183176,
-319.269758490247)) ;
#38350 = CARTESIAN_POINT('Ctrl Pts',(-4.2263845233712,-18.0930614878937,-319.281305235459)) ;
#38351 = CARTESIAN_POINT('Ctrl Pts',(-4.93034124645549,-17.9140427199375,
-319.291100745919)) ;
#38352 = CARTESIAN_POINT('Ctrl Pts',(-5.88477134465508,-17.6107916630486,
-319.304578295527)) ;
#38353 = CARTESIAN_POINT('Ctrl Pts',(-6.14564708095058,-17.5214593867005,
-319.308279388589)) ;
#38354 = CARTESIAN_POINT('Ctrl Pts',(-6.56933416195158,-17.3657482399414,
-319.314275072093)) ;
#38355 = CARTESIAN_POINT('Ctrl Pts',(-6.73336358095217,-17.3028083945092,
-319.316592334836)) ;
#38356 = CARTESIAN_POINT('Ctrl Pts',(-6.97082076714864,-17.2078054742524,
-319.319929060994)) ;
#38357 = CARTESIAN_POINT('Ctrl Pts',(-7.04497323235441,-17.1775802599382,
-319.320968467206)) ;
#38358 = CARTESIAN_POINT('Ctrl Pts',(-7.18033805084221,-17.1213803802278,
-319.322859600248)) ;
#38359 = CARTESIAN_POINT('Ctrl Pts',(-7.24161067181002,-17.0955548468008,
-319.323713076339)) ;
#38360 = CARTESIAN_POINT('Ctrl Pts',(-7.39349896150327,-17.0305729993541,
-319.325823305844)) ;
#38361 = CARTESIAN_POINT('Ctrl Pts',(-7.48394361229586,-16.9910220890064,
-319.32707519626)) ;
#38362 = CARTESIAN_POINT('Ctrl Pts',(-7.87917907735069,-16.8144198603484,
-319.332533426962)) ;
#38363 = CARTESIAN_POINT('Ctrl Pts',(-8.18055378770408,-16.6698745922381,
-319.336663882051)) ;
#38364 = CARTESIAN_POINT('Ctrl Pts',(-9.10152525283095,-16.1971652312636,
-319.349385160626)) ;
#38365 = CARTESIAN_POINT('Ctrl Pts',(-9.70655597666266,-15.8419915340611,
-319.357904709276)) ;
#38366 = CARTESIAN_POINT('Ctrl Pts',(-10.4708478389784,-15.3330696735458,
-319.369382105004)) ;
#38367 = CARTESIAN_POINT('Ctrl Pts',(-10.6495176719626,-15.2095185063944,
-319.372117373067)) ;
#38368 = CARTESIAN_POINT('Ctrl Pts',(-10.934063956693,-15.0052806052894,-319.376567121194)) ;
#38369 = CARTESIAN_POINT('Ctrl Pts',(-11.0413125707712,-14.9265407012279,
-319.378266275821)) ;
#38370 = CARTESIAN_POINT('Ctrl Pts',(-11.2485849340564,-14.7709089261429,
-319.381594595799)) ;
#38371 = CARTESIAN_POINT('Ctrl Pts',(-11.3486896676676,-14.6941367999769,
-319.383222735165)) ;
#38372 = CARTESIAN_POINT('Ctrl Pts',(-11.5694883267313,-14.5212000633758,
-319.386860714791)) ;
#38373 = CARTESIAN_POINT('Ctrl Pts',(-11.6897814259169,-14.424538867556,-319.388874508813)) ;
#38374 = CARTESIAN_POINT('Ctrl Pts',(-12.3655126594377,-13.867551884254,-319.400367303846)) ;
#38375 = CARTESIAN_POINT('Ctrl Pts',(-12.8949527241165,-13.3766619248727,
-319.410102302259)) ;
#38376 = CARTESIAN_POINT('Ctrl Pts',(-13.5870107167304,-12.6556288969575,
-319.423553243901)) ;
#38377 = CARTESIAN_POINT('Ctrl Pts',(-13.7750096200314,-12.4507394667984,
-319.427286016803)) ;
#38378 = CARTESIAN_POINT('Ctrl Pts',(-14.0747847599679,-12.108927434066,-319.433325447807)) ;
#38379 = CARTESIAN_POINT('Ctrl Pts',(-14.1893330199395,-11.9744944895627,
-319.435655145479)) ;
#38380 = CARTESIAN_POINT('Ctrl Pts',(-14.3531046481112,-11.7766431281461,
-319.439006155434)) ;
#38381 = CARTESIAN_POINT('Ctrl Pts',(-14.4038622375929,-11.7145076324911,
-319.440047632248)) ;
#38382 = CARTESIAN_POINT('Ctrl Pts',(-14.495929680981,-11.6002991253359,-319.441940505001)) ;
#38383 = CARTESIAN_POINT('Ctrl Pts',(-14.5373655918537,-11.5483296954832,
-319.442793676275)) ;
#38384 = CARTESIAN_POINT('Ctrl Pts',(-14.6394921063487,-11.4188206820169,
-319.444900496962)) ;
#38385 = CARTESIAN_POINT('Ctrl Pts',(-14.6998466333324,-11.3410186446011,
-319.446149323912)) ;
#38386 = CARTESIAN_POINT('Ctrl Pts',(-14.9690212521228,-10.988271077602,-319.451744345257)) ;
#38387 = CARTESIAN_POINT('Ctrl Pts',(-15.1707668441045,-10.7080125608712,
-319.456008972419)) ;
#38388 = CARTESIAN_POINT('Ctrl Pts',(-15.5963413522244,-10.0806290561425,
-319.465321525315)) ;
#38389 = CARTESIAN_POINT('Ctrl Pts',(-15.8166412597065,-9.73133111185656,
-319.470357778874)) ;
#38390 = CARTESIAN_POINT('Ctrl Pts',(-16.1650907288684,-9.13570935190439,
-319.478851738198)) ;
#38391 = CARTESIAN_POINT('Ctrl Pts',(-16.2996918586295,-8.89333394255288,
-319.482282655383)) ;
#38392 = CARTESIAN_POINT('Ctrl Pts',(-16.5300533034447,-8.45571254644613,
-319.488464155222)) ;
#38393 = CARTESIAN_POINT('Ctrl Pts',(-16.6279062283607,-8.26162642003638,
-319.491201025431)) ;
#38394 = CARTESIAN_POINT('Ctrl Pts',(-16.7801361857393,-7.94602001413403,
-319.495652571288)) ;
#38395 = CARTESIAN_POINT('Ctrl Pts',(-16.8366533689915,-7.82555478849491,
-319.497351893413)) ;
#38396 = CARTESIAN_POINT('Ctrl Pts',(-16.944209056286,-7.58974214479628,-319.500680006021)) ;
#38397 = CARTESIAN_POINT('Ctrl Pts',(-16.995376769289,-7.47446150461247,-319.502307764712)) ;
#38398 = CARTESIAN_POINT('Ctrl Pts',(-17.1064915475144,-7.21707906813494,
-319.505944161889)) ;
#38399 = CARTESIAN_POINT('Ctrl Pts',(-17.1658506236061,-7.07473360724396,
-319.507956744087)) ;
#38400 = CARTESIAN_POINT('Ctrl Pts',(-17.4935257941067,-6.26054395960238,
-319.519475047018)) ;
#38401 = CARTESIAN_POINT('Ctrl Pts',(-17.724164668576,-5.5742114699139,-319.529238513901)) ;
#38402 = CARTESIAN_POINT('Ctrl Pts',(-17.9869089557257,-4.60893865526558,
-319.542702316971)) ;
#38403 = CARTESIAN_POINT('Ctrl Pts',(-18.0536624005308,-4.34010178958931,
-319.546420511394)) ;
#38404 = CARTESIAN_POINT('Ctrl Pts',(-18.1529976434216,-3.89797587374466,
-319.552439817454)) ;
#38405 = CARTESIAN_POINT('Ctrl Pts',(-18.1891699891861,-3.72553816866229,
-319.554763801168)) ;
#38406 = CARTESIAN_POINT('Ctrl Pts',(-18.238220777323,-3.47393544510405,-319.558108222011)) ;
#38407 = CARTESIAN_POINT('Ctrl Pts',(-18.253049290147,-3.3951607081905,-319.559148722954)) ;
#38408 = CARTESIAN_POINT('Ctrl Pts',(-18.2792412556928,-3.25088565586482,
-319.56104074298)) ;
#38409 = CARTESIAN_POINT('Ctrl Pts',(-18.290763916458,-3.1854157934459,-319.561894025508)) ;
#38410 = CARTESIAN_POINT('Ctrl Pts',(-18.3184991170657,-3.02271499854085,
-319.564002295232)) ;
#38411 = CARTESIAN_POINT('Ctrl Pts',(-18.3342894069702,-2.92541413251193,
-319.565252442192)) ;
#38412 = CARTESIAN_POINT('Ctrl Pts',(-18.402242510466,-2.48450335993266,-319.570877554075)) ;
#38413 = CARTESIAN_POINT('Ctrl Pts',(-18.4455257640374,-2.13959500572097,
-319.575169840832)) ;
#38414 = CARTESIAN_POINT('Ctrl Pts',(-18.4865416086821,-1.71703460431869,
-319.580384504812)) ;
#38415 = CARTESIAN_POINT('Ctrl Pts',(-18.4935038467758,-1.64034872967172,
-319.581329032511)) ;
#38416 = CARTESIAN_POINT('Ctrl Pts',(-18.5399093606199,-1.09130195206812,
-319.58808329453)) ;
#38417 = CARTESIAN_POINT('Ctrl Pts',(-18.5617271927112,-0.617626492395772,
-319.593871694817)) ;
#38418 = CARTESIAN_POINT('Ctrl Pts',(-18.5677214768945,0.157147599598682,
-319.603473466903)) ;
#38419 = CARTESIAN_POINT('Ctrl Pts',(-18.5627385678948,0.457943790936195,
-319.607232968799)) ;
#38420 = CARTESIAN_POINT('Ctrl Pts',(-18.5444560085571,0.905084518578797,
-319.61289457403)) ;
#38421 = CARTESIAN_POINT('Ctrl Pts',(-18.5367243238609,1.05160729322288,-319.614761341118)) ;
#38422 = CARTESIAN_POINT('Ctrl Pts',(-18.519251253741,1.32182588836328,-319.61822732856)) ;
#38423 = CARTESIAN_POINT('Ctrl Pts',(-18.5100051050406,1.44554544680253,-319.619823245149)) ;
#38424 = CARTESIAN_POINT('Ctrl Pts',(-18.4863505684078,1.72441869773139,-319.623441612675)) ;
#38425 = CARTESIAN_POINT('Ctrl Pts',(-18.4712275705704,1.87950235957931,-319.625468570995)) ;
#38426 = CARTESIAN_POINT('Ctrl Pts',(-18.4151109568633,2.38854497977584,-319.632170063606)) ;
#38427 = CARTESIAN_POINT('Ctrl Pts',(-18.3658801911698,2.74151462355908,-319.636895183147)) ;
#38428 = CARTESIAN_POINT('Ctrl Pts',(-18.2108539057103,3.65911306735283,-319.649341253961)) ;
#38429 = CARTESIAN_POINT('Ctrl Pts',(-18.0889624278294,4.22063324367381,-319.6571266098)) ;
#38430 = CARTESIAN_POINT('Ctrl Pts',(-17.8952280267619,4.94846580360892,-319.667203581026)) ;
#38431 = CARTESIAN_POINT('Ctrl Pts',(-17.8467180259244,5.12065970226074,-319.669585584653)) ;
#38432 = CARTESIAN_POINT('Ctrl Pts',(-17.7582010069487,5.41831413967188,-319.673685541971)) ;
#38433 = CARTESIAN_POINT('Ctrl Pts',(-17.7193336957532,5.54409997983431,-319.675412611917)) ;
#38434 = CARTESIAN_POINT('Ctrl Pts',(-17.6570491662795,5.73832236347726,-319.678065147737)) ;
#38435 = CARTESIAN_POINT('Ctrl Pts',(-17.6345643852379,5.80705327758613,-319.679001042792)) ;
#38436 = CARTESIAN_POINT('Ctrl Pts',(-17.5922010763289,5.9340330736187,-319.680723768735)) ;
#38437 = CARTESIAN_POINT('Ctrl Pts',(-17.5724333650502,5.9923178205215,-319.681511989539)) ;
#38438 = CARTESIAN_POINT('Ctrl Pts',(-17.5164358181222,6.15476546772547,-319.683703098889)) ;
#38439 = CARTESIAN_POINT('Ctrl Pts',(-17.4795671159689,6.25870555518904,-319.685098420167)) ;
#38440 = CARTESIAN_POINT('Ctrl Pts',(-17.2196924098855,6.97113158525681,-319.694634221157)) ;
#38441 = CARTESIAN_POINT('Ctrl Pts',(-16.9658847798747,7.56790871993275,-319.702497239951)) ;
#38442 = CARTESIAN_POINT('Ctrl Pts',(-16.5397577983865,8.44008347033473,-319.714411703903)) ;
#38443 = CARTESIAN_POINT('Ctrl Pts',(-16.3905902247648,8.72623336110013,-319.718389290374)) ;
#38444 = CARTESIAN_POINT('Ctrl Pts',(-16.1789612946889,9.10761207210454,-319.723826136733)) ;
#38445 = CARTESIAN_POINT('Ctrl Pts',(-16.122971185852,9.20636661987439,-319.725246423577)) ;
#38446 = CARTESIAN_POINT('Ctrl Pts',(-15.9751615553829,9.4615867085999,-319.728951959854)) ;
#38447 = CARTESIAN_POINT('Ctrl Pts',(-15.8819482667882,9.61723083167077,-319.731246377199)) ;
#38448 = CARTESIAN_POINT('Ctrl Pts',(-15.71964220456,9.87944685914268,-319.73517565264)) ;
#38449 = CARTESIAN_POINT('Ctrl Pts',(-15.6517096131371,9.98672155484111,-319.736801683126)) ;
#38450 = CARTESIAN_POINT('Ctrl Pts',(-15.5097453416722,10.2058952744082,-319.740163190908)) ;
#38451 = CARTESIAN_POINT('Ctrl Pts',(-15.4355903156368,10.317705678064,-319.741899556146)) ;
#38452 = CARTESIAN_POINT('Ctrl Pts',(-15.2346380366665,10.6136843249216,-319.746554134101)) ;
#38453 = CARTESIAN_POINT('Ctrl Pts',(-15.105714948132,10.7963821107631,-319.74948845167)) ;
#38454 = CARTESIAN_POINT('Ctrl Pts',(-14.8138365795276,11.1945386718311,-319.756015757554)) ;
#38455 = CARTESIAN_POINT('Ctrl Pts',(-14.6494151507777,11.4088599620917,-319.759618197178)) ;
#38456 = CARTESIAN_POINT('Ctrl Pts',(-14.4114476179268,11.7054178519844,-319.764716238847)) ;
#38457 = CARTESIAN_POINT('Ctrl Pts',(-14.3417553689894,11.7907032214126,-319.766195892485)) ;
#38458 = CARTESIAN_POINT('Ctrl Pts',(-14.1220604864761,12.054723220087,-319.770815905728)) ;
#38459 = CARTESIAN_POINT('Ctrl Pts',(-13.9694445735006,12.2312535160645,-319.773962342769)) ;
#38460 = CARTESIAN_POINT('Ctrl Pts',(-13.6278621793669,12.6116256205328,-319.780842973065)) ;
#38461 = CARTESIAN_POINT('Ctrl Pts',(-13.4375631121709,12.8141962793856,-319.784573933402)) ;
#38462 = CARTESIAN_POINT('Ctrl Pts',(-13.119046828619,13.1383515247736,-319.790610848116)) ;
#38463 = CARTESIAN_POINT('Ctrl Pts',(-12.9935146797489,13.2625128439319,-319.792939823999)) ;
#38464 = CARTESIAN_POINT('Ctrl Pts',(-12.8083985314719,13.4404561453371,-319.796289954076)) ;
#38465 = CARTESIAN_POINT('Ctrl Pts',(-12.7502067083679,13.4956720193375,-319.797331262211)) ;
#38466 = CARTESIAN_POINT('Ctrl Pts',(-12.6431490888848,13.5959441769179,-319.79922395058)) ;
#38467 = CARTESIAN_POINT('Ctrl Pts',(-12.5943958297316,13.6411183787552,-319.800077104591)) ;
#38468 = CARTESIAN_POINT('Ctrl Pts',(-12.4728119687584,13.7525691284561,-319.802183981378)) ;
#38469 = CARTESIAN_POINT('Ctrl Pts',(-12.3996946459614,13.8185299062045,-319.803432880374)) ;
#38470 = CARTESIAN_POINT('Ctrl Pts',(-12.0681935569585,14.1128347651821,-319.809022528047)) ;
#38471 = CARTESIAN_POINT('Ctrl Pts',(-11.8040027467239,14.3345359572437,-319.813281932622)) ;
#38472 = CARTESIAN_POINT('Ctrl Pts',(-11.2102648370461,14.8052326426246,-319.822589408397)) ;
#38473 = CARTESIAN_POINT('Ctrl Pts',(-10.8782734615348,15.0508510729773,-319.827625722343)) ;
#38474 = CARTESIAN_POINT('Ctrl Pts',(-10.3099708235192,15.4426670033821,-319.836122265988)) ;
#38475 = CARTESIAN_POINT('Ctrl Pts',(-10.0780707317283,15.5949976771392,-319.839555768992)) ;
#38476 = CARTESIAN_POINT('Ctrl Pts',(-9.65846284602696,15.8573605127594,-319.845741302014)) ;
#38477 = CARTESIAN_POINT('Ctrl Pts',(-9.47206997903367,15.9693981430799,-319.848479590589)) ;
#38478 = CARTESIAN_POINT('Ctrl Pts',(-9.16850189045506,16.144682830759,-319.852932860013)) ;
#38479 = CARTESIAN_POINT('Ctrl Pts',(-9.05253932730333,16.2099889662829,-319.85463246526)) ;
#38480 = CARTESIAN_POINT('Ctrl Pts',(-8.82533735082764,16.3347428905617,-319.857960766976)) ;
#38481 = CARTESIAN_POINT('Ctrl Pts',(-8.7141744196257,16.3943151362728,-319.859588427558)) ;
#38482 = CARTESIAN_POINT('Ctrl Pts',(-8.46578558572374,16.5241866402308,-319.863224138451)) ;
#38483 = CARTESIAN_POINT('Ctrl Pts',(-8.3282735280697,16.5939184537859,-319.865236126318)) ;
#38484 = CARTESIAN_POINT('Ctrl Pts',(-7.53988370801585,16.9814390582658,-319.876765187352)) ;
#38485 = CARTESIAN_POINT('Ctrl Pts',(-6.87171979668173,17.2626352898733,-319.886540733513)) ;
#38486 = CARTESIAN_POINT('Ctrl Pts',(-5.92820194030155,17.5962310982935,-319.900009171244)) ;
#38487 = CARTESIAN_POINT('Ctrl Pts',(-5.66553199569972,17.6825528310066,-319.903720390948)) ;
#38488 = CARTESIAN_POINT('Ctrl Pts',(-5.23266435444511,17.8141710959272,-319.909730082764)) ;
#38489 = CARTESIAN_POINT('Ctrl Pts',(-5.06357656710662,17.8629689754263,-319.912051342808)) ;
#38490 = CARTESIAN_POINT('Ctrl Pts',(-4.81652668189091,17.930476584419,-319.915392692316)) ;
#38491 = CARTESIAN_POINT('Ctrl Pts',(-4.73909691644011,17.9510969097205,-319.916432794473)) ;
#38492 = CARTESIAN_POINT('Ctrl Pts',(-4.59718118539811,17.9879082928282,-319.918324525295)) ;
#38493 = CARTESIAN_POINT('Ctrl Pts',(-4.53273727125493,18.0042553977027,-319.919177911769)) ;
#38494 = CARTESIAN_POINT('Ctrl Pts',(-4.3724706414082,18.0439942590534,-319.921287079592)) ;
#38495 = CARTESIAN_POINT('Ctrl Pts',(-4.27654666169823,18.066969226243,-319.922538010712)) ;
#38496 = CARTESIAN_POINT('Ctrl Pts',(-3.84094213516165,18.1676382720442,-319.928175252157)) ;
#38497 = CARTESIAN_POINT('Ctrl Pts',(-3.49929775127554,18.2365247036286,-319.932478455298)) ;
#38498 = CARTESIAN_POINT('Ctrl Pts',(-2.7490992488878,18.3659298118304,-319.941828824024)) ;
#38499 = CARTESIAN_POINT('Ctrl Pts',(-2.34005409434378,18.422515342876,-319.946864964147)) ;
#38500 = CARTESIAN_POINT('Ctrl Pts',(-1.65551987148274,18.4940427655919,-319.955337967357)) ;
#38501 = CARTESIAN_POINT('Ctrl Pts',(-1.38097356447629,18.5165675961726,-319.958747518266)) ;
#38502 = CARTESIAN_POINT('Ctrl Pts',(-0.890008694264454,18.5458678578923,
-319.964895875783)) ;
#38503 = CARTESIAN_POINT('Ctrl Pts',(-0.673780509989867,18.5549818018221,
-319.967621213158)) ;
#38504 = CARTESIAN_POINT('Ctrl Pts',(-0.324584938680104,18.5635881755225,
-319.972059069452)) ;
#38505 = CARTESIAN_POINT('Ctrl Pts',(-0.191695890545446,18.5654360023381,
-319.973756420582)) ;
#38506 = CARTESIAN_POINT('Ctrl Pts',(0.0674249714563399,18.5662566454235,
-319.97708392605)) ;
#38507 = CARTESIAN_POINT('Ctrl Pts',(0.193649211159391,18.5653691554949,-319.978713084605)) ;
#38508 = CARTESIAN_POINT('Ctrl Pts',(0.504550860100535,18.5600121422162,-319.982746700352)) ;
#38509 = CARTESIAN_POINT('Ctrl Pts',(0.6891892195366,18.5540734165393,-319.985160385014)) ;
#38510 = CARTESIAN_POINT('Ctrl Pts',(1.51233830771507,18.5152933067266,-319.995999431483)) ;
#38511 = CARTESIAN_POINT('Ctrl Pts',(2.14898649596295,18.4522384785831,-320.004609907316)) ;
#38512 = CARTESIAN_POINT('Ctrl Pts',(3.0887807274062,18.3098544208974,-320.017411465897)) ;
#38513 = CARTESIAN_POINT('Ctrl Pts',(3.39523397472678,18.2555120960985,-320.021597204388)) ;
#38514 = CARTESIAN_POINT('Ctrl Pts',(3.88557008711895,18.1557879752052,-320.02825325447)) ;
#38515 = CARTESIAN_POINT('Ctrl Pts',(4.0703769357173,18.1152511361994,-320.030752150826)) ;
#38516 = CARTESIAN_POINT('Ctrl Pts',(4.33449654003708,18.0530714243576,-320.034294725367)) ;
#38517 = CARTESIAN_POINT('Ctrl Pts',(4.41433521615896,18.0337154445048,-320.035361770274)) ;
#38518 = CARTESIAN_POINT('Ctrl Pts',(4.55819934105968,17.9978246019581,-320.037275961302)) ;
#38519 = CARTESIAN_POINT('Ctrl Pts',(4.62226971507521,17.9814764219975,-320.038125215467)) ;
#38520 = CARTESIAN_POINT('Ctrl Pts',(4.77845717552494,17.9407337317494,-320.040188223477)) ;
#38521 = CARTESIAN_POINT('Ctrl Pts',(4.87047639526634,17.9159716323842,-320.041397667061)) ;
#38522 = CARTESIAN_POINT('Ctrl Pts',(5.24497135151118,17.8120977070797,-320.046302164943)) ;
#38523 = CARTESIAN_POINT('Ctrl Pts',(5.52574451263457,17.7270047529477,-320.04993879566)) ;
#38524 = CARTESIAN_POINT('Ctrl Pts',(6.34754608396632,17.4565215134081,-320.06059257353)) ;
#38525 = CARTESIAN_POINT('Ctrl Pts',(6.88215907115174,17.2527497020884,-320.067543972492)) ;
#38526 = CARTESIAN_POINT('Ctrl Pts',(7.55162703804269,16.9614996919909,-320.07657173726)) ;
#38527 = CARTESIAN_POINT('Ctrl Pts',(7.69592687685017,16.896515976897,-320.078536593918)) ;
#38528 = CARTESIAN_POINT('Ctrl Pts',(8.04578298633694,16.7335507974973,-320.08335451286)) ;
#38529 = CARTESIAN_POINT('Ctrl Pts',(8.25040130628812,16.6336172905842,-320.086218698649)) ;
#38530 = CARTESIAN_POINT('Ctrl Pts',(8.57322127727884,16.4685327198421,-320.090821880119)) ;
#38531 = CARTESIAN_POINT('Ctrl Pts',(8.69264023068258,16.4058129566795,-320.092543424442)) ;
#38532 = CARTESIAN_POINT('Ctrl Pts',(8.92281739151623,16.2817032939308,-320.095899534717)) ;
#38533 = CARTESIAN_POINT('Ctrl Pts',(9.03365198864775,16.2204705248554,-320.097532877132)) ;
#38534 = CARTESIAN_POINT('Ctrl Pts',(9.27494514780877,16.0839230599919,-320.101127396337)) ;
#38535 = CARTESIAN_POINT('Ctrl Pts',(9.40513105028525,16.0081447498608,-320.103091896737)) ;
#38536 = CARTESIAN_POINT('Ctrl Pts',(9.93666896574076,15.6900259134925,-320.111215926243)) ;
#38537 = CARTESIAN_POINT('Ctrl Pts',(10.3296923532581,15.4341101756063,-320.117472350451)) ;
#38538 = CARTESIAN_POINT('Ctrl Pts',(11.0899376495795,14.8970206119009,-320.129984184648)) ;
#38539 = CARTESIAN_POINT('Ctrl Pts',(11.4571878805374,14.6164559976904,-320.136233512233)) ;
#38540 = CARTESIAN_POINT('Ctrl Pts',(11.9393609646369,14.2187460603731,-320.144581680247)) ;
#38541 = CARTESIAN_POINT('Ctrl Pts',(12.0637605490455,14.1133540062695,-320.14674857129)) ;
#38542 = CARTESIAN_POINT('Ctrl Pts',(12.2797603217164,13.9254150399708,-320.150523340422)) ;
#38543 = CARTESIAN_POINT('Ctrl Pts',(12.3719565054994,13.8435685390282,-320.152138580305)) ;
#38544 = CARTESIAN_POINT('Ctrl Pts',(12.5157162349746,13.7133636247249,-320.154658909564)) ;
#38545 = CARTESIAN_POINT('Ctrl Pts',(12.5678304142424,13.6656186643628,-320.155572908172)) ;
#38546 = CARTESIAN_POINT('Ctrl Pts',(12.6655711162328,13.5750404759047,-320.157286674107)) ;
#38547 = CARTESIAN_POINT('Ctrl Pts',(12.7112561675805,13.5322718815756,-320.158087537528)) ;
#38548 = CARTESIAN_POINT('Ctrl Pts',(12.8413884142572,13.4092066014094,-320.160369687735)) ;
#38549 = CARTESIAN_POINT('Ctrl Pts',(12.9252971235976,13.3283446990111,-320.161842338388)) ;
#38550 = CARTESIAN_POINT('Ctrl Pts',(13.3366125049587,12.9244273584927,-320.169081810957)) ;
#38551 = CARTESIAN_POINT('Ctrl Pts',(13.6526976119873,12.5900717163233,-320.174714636213)) ;
#38552 = CARTESIAN_POINT('Ctrl Pts',(14.2379479098119,11.9230053296396,-320.185584059432)) ;
#38553 = CARTESIAN_POINT('Ctrl Pts',(14.5086749540123,11.5920475947371,-320.19081706137)) ;
#38554 = CARTESIAN_POINT('Ctrl Pts',(14.9401752058827,11.025725300284,-320.199652727215)) ;
#38555 = CARTESIAN_POINT('Ctrl Pts',(15.1073879545976,10.7954750838082,-320.203213441597)) ;
#38556 = CARTESIAN_POINT('Ctrl Pts',(15.3513268032109,10.4428006697178,-320.208641948314)) ;
#38557 = CARTESIAN_POINT('Ctrl Pts',(15.4320244489777,10.3231749852063,-320.210478866598)) ;
#38558 = CARTESIAN_POINT('Ctrl Pts',(15.5796050754802,10.0988041840275,-320.213917929155)) ;
#38559 = CARTESIAN_POINT('Ctrl Pts',(15.6468467997275,9.99430464964471,-320.21551716458)) ;
#38560 = CARTESIAN_POINT('Ctrl Pts',(15.7977885547452,9.75447050384159,-320.219182564621)) ;
#38561 = CARTESIAN_POINT('Ctrl Pts',(15.8808079355028,9.61871910602072,-320.221253743268)) ;
#38562 = CARTESIAN_POINT('Ctrl Pts',(16.1524546149686,9.16142301085318,-320.228218656002)) ;
#38563 = CARTESIAN_POINT('Ctrl Pts',(16.3331410593165,8.83526816939149,-320.233168185275)) ;
#38564 = CARTESIAN_POINT('Ctrl Pts',(16.6949491006004,8.13309138027728,-320.243744190874)) ;
#38565 = CARTESIAN_POINT('Ctrl Pts',(16.8734613046573,7.7559528023655,-320.249378676435)) ;
#38566 = CARTESIAN_POINT('Ctrl Pts',(17.1751764750888,7.05869596066065,-320.259595551739)) ;
#38567 = CARTESIAN_POINT('Ctrl Pts',(17.3025054370407,6.74056243641117,-320.264183310802)) ;
#38568 = CARTESIAN_POINT('Ctrl Pts',(17.4602303554772,6.31250797324157,-320.27018670905)) ;
#38569 = CARTESIAN_POINT('Ctrl Pts',(17.4985230086725,6.20556955915865,-320.27167252722)) ;
#38570 = CARTESIAN_POINT('Ctrl Pts',(17.5562243478787,6.03964737653708,-320.273952692707)) ;
#38571 = CARTESIAN_POINT('Ctrl Pts',(17.5763224982979,5.98090638916209,-320.274755081634)) ;
#38572 = CARTESIAN_POINT('Ctrl Pts',(17.6188997919324,5.85439725314229,-320.276471882379)) ;
#38573 = CARTESIAN_POINT('Ctrl Pts',(17.6412834232062,5.78659798806358,-320.277385040377)) ;
#38574 = CARTESIAN_POINT('Ctrl Pts',(17.7023779429912,5.59789517860218,-320.279909439235)) ;
#38575 = CARTESIAN_POINT('Ctrl Pts',(17.7402407436729,5.47672107230045,-320.281510992794)) ;
#38576 = CARTESIAN_POINT('Ctrl Pts',(17.8258630370353,5.19249183469465,-320.285231355031)) ;
#38577 = CARTESIAN_POINT('Ctrl Pts',(17.8726330161994,5.02915039226601,-320.287341708953)) ;
#38578 = CARTESIAN_POINT('Ctrl Pts',(18.0499734966762,4.37605424666018,-320.295703943975)) ;
#38579 = CARTESIAN_POINT('Ctrl Pts',(18.1627068807465,3.88168443521965,-320.301871192323)) ;
#38580 = CARTESIAN_POINT('Ctrl Pts',(18.3226297249567,3.01880393951633,-320.312662409177)) ;
#38581 = CARTESIAN_POINT('Ctrl Pts',(18.3792547700535,2.65234435559654,-320.317252058086)) ;
#38582 = CARTESIAN_POINT('Ctrl Pts',(18.4475384453953,2.10160987598044,-320.324221304029)) ;
#38583 = CARTESIAN_POINT('Ctrl Pts',(18.4674839589907,1.91845636824946,-320.326550414766)) ;
#38584 = CARTESIAN_POINT('Ctrl Pts',(18.4964891004421,1.60944193958221,-320.330503948382)) ;
#38585 = CARTESIAN_POINT('Ctrl Pts',(18.506997491946,1.48373049431182,-320.332118908144)) ;
#38586 = CARTESIAN_POINT('Ctrl Pts',(18.5259538031235,1.22524779539483,-320.335454077873)) ;
#38587 = CARTESIAN_POINT('Ctrl Pts',(18.5342574400419,1.09247313882107,-320.337175128993)) ;
#38588 = CARTESIAN_POINT('Ctrl Pts',(18.5523575088749,0.742756068931193,-320.341729375101)) ;
#38589 = CARTESIAN_POINT('Ctrl Pts',(18.5597759406601,0.525711411823962,-320.344577418692)) ;
#38590 = CARTESIAN_POINT('Ctrl Pts',(18.5679868762546,0.031773627231106,-320.351103987191)) ;
#38591 = CARTESIAN_POINT('Ctrl Pts',(18.5663962055185,-0.245107563597892,
-320.354795004192)) ;
#38592 = CARTESIAN_POINT('Ctrl Pts',(18.5551718341297,-0.644282005015534,
-320.360148157064)) ;
#38593 = CARTESIAN_POINT('Ctrl Pts',(18.5505180401484,-0.766664977760487,
-320.361793608738)) ;
#38594 = CARTESIAN_POINT('Ctrl Pts',(18.5446545929199,-0.888979995160607,
-320.363441000746)) ;
#38595 = CARTESIAN_POINT('',(18.544654593745,-0.888979977948782,-315.477129595899)) ;
#38596 = CARTESIAN_POINT('Origin',(0.,0.,-315.477129595899)) ;
#38597 = CARTESIAN_POINT('',(18.544654593745,-0.888979977947869,-322.15838043089)) ;
#38598 = CARTESIAN_POINT('',(18.5446545934554,-0.888979983988388,-321.863010318849)) ;
#38599 = CARTESIAN_POINT('',(18.544654593745,-0.888979977948782,-315.477129595899)) ;
#38600 = CARTESIAN_POINT('Ctrl Pts',(18.5446545937451,-0.888979977946956,
-322.15838043089)) ;
#38601 = CARTESIAN_POINT('Ctrl Pts',(18.5487996595587,-0.802511423324546,
-322.157272162262)) ;
#38602 = CARTESIAN_POINT('Ctrl Pts',(18.5523399110549,-0.716014844920947,
-322.156171030603)) ;
#38603 = CARTESIAN_POINT('Ctrl Pts',(18.5628298984463,-0.406808063188213,
-322.152256951415)) ;
#38604 = CARTESIAN_POINT('Ctrl Pts',(18.5663752672,-0.184001171814233,-322.149477575187)) ;
#38605 = CARTESIAN_POINT('Ctrl Pts',(18.5650377213936,0.455758810308087,-322.141557399885)) ;
#38606 = CARTESIAN_POINT('Ctrl Pts',(18.5501210484485,0.872554674511302,-322.136469030416)) ;
#38607 = CARTESIAN_POINT('Ctrl Pts',(18.486526737587,1.78667737075809,-322.125236540751)) ;
#38608 = CARTESIAN_POINT('Ctrl Pts',(18.4317827840163,2.28325839234699,-322.119084876013)) ;
#38609 = CARTESIAN_POINT('Ctrl Pts',(18.3302147114612,2.95465787815983,-322.110550934314)) ;
#38610 = CARTESIAN_POINT('Ctrl Pts',(18.300766083257,3.13189003138177,-322.108278207396)) ;
#38611 = CARTESIAN_POINT('Ctrl Pts',(18.2461695268471,3.43334404513227,-322.10437405166)) ;
#38612 = CARTESIAN_POINT('Ctrl Pts',(18.222313407616,3.55778691822792,-322.102751157992)) ;
#38613 = CARTESIAN_POINT('Ctrl Pts',(18.170471084917,3.81400380454635,-322.099385583639)) ;
#38614 = CARTESIAN_POINT('Ctrl Pts',(18.142320773578,3.94573711141024,-322.097641903981)) ;
#38615 = CARTESIAN_POINT('Ctrl Pts',(18.0629616468464,4.29828984594866,-322.092939271591)) ;
#38616 = CARTESIAN_POINT('Ctrl Pts',(18.0091383609485,4.51849690259196,-322.089963598779)) ;
#38617 = CARTESIAN_POINT('Ctrl Pts',(17.9111874601896,4.88963890781372,-322.084886636578)) ;
#38618 = CARTESIAN_POINT('Ctrl Pts',(17.8691499990125,5.04109939555204,-322.082797235378)) ;
#38619 = CARTESIAN_POINT('Ctrl Pts',(17.6675659559886,5.7331774868269,-322.073177068932)) ;
#38620 = CARTESIAN_POINT('Ctrl Pts',(17.4853745621891,6.26688800631222,-322.06554326626)) ;
#38621 = CARTESIAN_POINT('Ctrl Pts',(17.1680672917803,7.07419541659538,-322.053907116497)) ;
#38622 = CARTESIAN_POINT('Ctrl Pts',(17.0500254521064,7.35414223921198,-322.049857225287)) ;
#38623 = CARTESIAN_POINT('Ctrl Pts',(16.8858803849559,7.71820442275282,-322.044622873257)) ;
#38624 = CARTESIAN_POINT('Ctrl Pts',(16.8459202056976,7.80503737003947,-322.043376959761)) ;
#38625 = CARTESIAN_POINT('Ctrl Pts',(16.7771734814474,7.95143542370017,-322.041283108319)) ;
#38626 = CARTESIAN_POINT('Ctrl Pts',(16.74873594041,8.01116219744681,-322.040430869139)) ;
#38627 = CARTESIAN_POINT('Ctrl Pts',(16.6843517497622,8.14454561722796,-322.038532532803)) ;
#38628 = CARTESIAN_POINT('Ctrl Pts',(16.6482354216506,8.21811864062088,-322.037488552967)) ;
#38629 = CARTESIAN_POINT('Ctrl Pts',(16.5277194054222,8.45956830293604,-322.034069196931)) ;
#38630 = CARTESIAN_POINT('Ctrl Pts',(16.4412582536297,8.62640318326902,-322.031717231844)) ;
#38631 = CARTESIAN_POINT('Ctrl Pts',(16.2065944922168,9.06286045647185,-322.025560620256)) ;
#38632 = CARTESIAN_POINT('Ctrl Pts',(16.0541968237118,9.33016128040263,-322.021785838148)) ;
#38633 = CARTESIAN_POINT('Ctrl Pts',(15.5540396636236,10.1588545606611,-322.009926437806)) ;
#38634 = CARTESIAN_POINT('Ctrl Pts',(15.1829375846837,10.7055537539624,-322.001853855825)) ;
#38635 = CARTESIAN_POINT('Ctrl Pts',(14.6759626629927,11.3728721957208,-321.991318106432)) ;
#38636 = CARTESIAN_POINT('Ctrl Pts',(14.5663939243873,11.5128740967222,-321.98906857793)) ;
#38637 = CARTESIAN_POINT('Ctrl Pts',(14.3754907319645,11.7497127398196,-321.985191198123)) ;
#38638 = CARTESIAN_POINT('Ctrl Pts',(14.2951465345319,11.8473317146042,-321.983571571629)) ;
#38639 = CARTESIAN_POINT('Ctrl Pts',(14.1267570630213,12.0477194999068,-321.980201097481)) ;
#38640 = CARTESIAN_POINT('Ctrl Pts',(14.0385726028535,12.1503617013837,-321.978449127807)) ;
#38641 = CARTESIAN_POINT('Ctrl Pts',(13.7973744066635,12.4249724861135,-321.973691839733)) ;
#38642 = CARTESIAN_POINT('Ctrl Pts',(13.6422720040161,12.5950742777077,-321.970669090305)) ;
#38643 = CARTESIAN_POINT('Ctrl Pts',(13.3734778831224,12.8790706909869,-321.965495095661)) ;
#38644 = CARTESIAN_POINT('Ctrl Pts',(13.2613951364485,12.994451566119,-321.963355867377)) ;
#38645 = CARTESIAN_POINT('Ctrl Pts',(12.7295298781362,13.5279181403464,-321.95329754996)) ;
#38646 = CARTESIAN_POINT('Ctrl Pts',(12.291390773185,13.9272111606732,-321.945265532659)) ;
#38647 = CARTESIAN_POINT('Ctrl Pts',(11.6774504042566,14.435145217785,-321.934595144184)) ;
#38648 = CARTESIAN_POINT('Ctrl Pts',(11.5178470092958,14.5628110569883,-321.931872181912)) ;
#38649 = CARTESIAN_POINT('Ctrl Pts',(11.255735027087,14.7654679945165,-321.927501288321)) ;
#38650 = CARTESIAN_POINT('Ctrl Pts',(11.1545077010781,14.8420879300768,-321.925837013899)) ;
#38651 = CARTESIAN_POINT('Ctrl Pts',(10.99513389696,14.96016803904,-321.923258658101)) ;
#38652 = CARTESIAN_POINT('Ctrl Pts',(10.937520623894,15.0023411435658,-321.922335011599)) ;
#38653 = CARTESIAN_POINT('Ctrl Pts',(10.8222354750771,15.085713170374,-321.92050471892)) ;
#38654 = CARTESIAN_POINT('Ctrl Pts',(10.7645680905551,15.1269162876888,-321.919598026613)) ;
#38655 = CARTESIAN_POINT('Ctrl Pts',(10.6051312803491,15.2394598356136,-321.917113536746)) ;
#38656 = CARTESIAN_POINT('Ctrl Pts',(10.5028791639552,15.3101102183431,-321.9155449411)) ;
#38657 = CARTESIAN_POINT('Ctrl Pts',(10.2633278797534,15.4720971762055,-321.91191888245)) ;
#38658 = CARTESIAN_POINT('Ctrl Pts',(10.1255057892276,15.5626418975683,-321.909869302491)) ;
#38659 = CARTESIAN_POINT('Ctrl Pts',(9.5871780159321,15.9061274048885,-321.901973837252)) ;
#38660 = CARTESIAN_POINT('Ctrl Pts',(9.17825545263083,16.145541158633,-321.896204557637)) ;
#38661 = CARTESIAN_POINT('Ctrl Pts',(8.36041795762826,16.5832431621111,-321.884813995728)) ;
#38662 = CARTESIAN_POINT('Ctrl Pts',(7.95249087693705,16.7826824359189,-321.879200507621)) ;
#38663 = CARTESIAN_POINT('Ctrl Pts',(7.40014379729122,17.0280655458937,-321.87158754533)) ;
#38664 = CARTESIAN_POINT('Ctrl Pts',(7.26188372340456,17.0874863323628,-321.869681380037)) ;
#38665 = CARTESIAN_POINT('Ctrl Pts',(7.00601269810024,17.1937869827731,-321.866150142373)) ;
#38666 = CARTESIAN_POINT('Ctrl Pts',(6.88861512619969,17.2411573371497,-321.864528593878)) ;
#38667 = CARTESIAN_POINT('Ctrl Pts',(6.64508671565606,17.3365375243023,-321.861161092913)) ;
#38668 = CARTESIAN_POINT('Ctrl Pts',(6.51889832372935,17.3843802124067,-321.85941409182)) ;
#38669 = CARTESIAN_POINT('Ctrl Pts',(6.17806942596655,17.5093682230922,-321.854689585883)) ;
#38670 = CARTESIAN_POINT('Ctrl Pts',(5.9625107369892,17.5839410490731,-321.851695077855)) ;
#38671 = CARTESIAN_POINT('Ctrl Pts',(5.59477809289496,17.7036189846872,-321.846579369567)) ;
#38672 = CARTESIAN_POINT('Ctrl Pts',(5.44329996735557,17.7507789250897,-321.844470110137)) ;
#38673 = CARTESIAN_POINT('Ctrl Pts',(4.74021165383412,17.9598263561176,-321.834678947671)) ;
#38674 = CARTESIAN_POINT('Ctrl Pts',(4.18187522988316,18.0979801827844,-321.826890213764)) ;
#38675 = CARTESIAN_POINT('Ctrl Pts',(3.33293282120812,18.2666512822746,-321.815286893583)) ;
#38676 = CARTESIAN_POINT('Ctrl Pts',(3.04654090590706,18.3165930067094,-321.811414947406)) ;
#38677 = CARTESIAN_POINT('Ctrl Pts',(2.67457516022838,18.3724917187028,-321.806486035236)) ;
#38678 = CARTESIAN_POINT('Ctrl Pts',(2.58996908361435,18.3846094441639,-321.805371628944)) ;
#38679 = CARTESIAN_POINT('Ctrl Pts',(2.43886581087167,18.4051874730474,-321.803395114084)) ;
#38680 = CARTESIAN_POINT('Ctrl Pts',(2.37240076842532,18.4138726778305,-321.80253050881)) ;
#38681 = CARTESIAN_POINT('Ctrl Pts',(2.22842778455192,18.431893646759,-321.800668773673)) ;
#38682 = CARTESIAN_POINT('Ctrl Pts',(2.15090518075313,18.4411008543941,-321.799673070621)) ;
#38683 = CARTESIAN_POINT('Ctrl Pts',(1.91097405005321,18.4680634840008,-321.79660933925)) ;
#38684 = CARTESIAN_POINT('Ctrl Pts',(1.74838733653556,18.4841643724296,-321.794558591313)) ;
#38685 = CARTESIAN_POINT('Ctrl Pts',(1.08290493219999,18.5412077444992,-321.786235060189)) ;
#38686 = CARTESIAN_POINT('Ctrl Pts',(0.578652091199881,18.5637881830208,-321.780086470651)) ;
#38687 = CARTESIAN_POINT('Ctrl Pts',(-0.407649254588204,18.5677250509697,
-321.767995191749)) ;
#38688 = CARTESIAN_POINT('Ctrl Pts',(-0.889296348461817,18.5508959957287,
-321.762060415628)) ;
#38689 = CARTESIAN_POINT('Ctrl Pts',(-1.55467839403078,18.5016719062076,-321.75368313893)) ;
#38690 = CARTESIAN_POINT('Ctrl Pts',(-1.73939966838831,18.4852204983317,-321.751339040825)) ;
#38691 = CARTESIAN_POINT('Ctrl Pts',(-2.04949957614768,18.452913368602,-321.747368062005)) ;
#38692 = CARTESIAN_POINT('Ctrl Pts',(-2.17501891170769,18.4385398820578,-321.745750850888)) ;
#38693 = CARTESIAN_POINT('Ctrl Pts',(-2.43206945327457,18.4064431554954,-321.742417694058)) ;
#38694 = CARTESIAN_POINT('Ctrl Pts',(-2.56357703946243,18.388588422237,-321.740700976515)) ;
#38695 = CARTESIAN_POINT('Ctrl Pts',(-2.90793927422231,18.3380685751711,-321.736175075831)) ;
#38696 = CARTESIAN_POINT('Ctrl Pts',(-3.12043652426833,18.3031075376664,-321.733351392112)) ;
#38697 = CARTESIAN_POINT('Ctrl Pts',(-3.60126935198572,18.2153815158039,-321.726895439337)) ;
#38698 = CARTESIAN_POINT('Ctrl Pts',(-3.86914412389228,18.1603686099956,-321.723251107187)) ;
#38699 = CARTESIAN_POINT('Ctrl Pts',(-4.47741226710087,18.0213800440598,-321.714889101795)) ;
#38700 = CARTESIAN_POINT('Ctrl Pts',(-4.81683915442632,17.9336393276997,-321.71015954964)) ;
#38701 = CARTESIAN_POINT('Ctrl Pts',(-5.24416761433995,17.8101683607781,-321.704172438769)) ;
#38702 = CARTESIAN_POINT('Ctrl Pts',(-5.33455658544967,17.7833038845697,-321.702904262159)) ;
#38703 = CARTESIAN_POINT('Ctrl Pts',(-5.73291839956111,17.6615963912092,-321.697311579922)) ;
#38704 = CARTESIAN_POINT('Ctrl Pts',(-6.03859688022656,17.55943304675,-321.69300967336)) ;
#38705 = CARTESIAN_POINT('Ctrl Pts',(-6.4333764213085,17.4159619712753,-321.687501142742)) ;
#38706 = CARTESIAN_POINT('Ctrl Pts',(-6.52502605383703,17.3818324293006,-321.686225775439)) ;
#38707 = CARTESIAN_POINT('Ctrl Pts',(-6.67842860185837,17.3233223670344,-321.684099459676)) ;
#38708 = CARTESIAN_POINT('Ctrl Pts',(-6.74032805700307,17.2993318986975,-321.683243855703)) ;
#38709 = CARTESIAN_POINT('Ctrl Pts',(-6.87709669785578,17.2454787507199,-321.681359202854)) ;
#38710 = CARTESIAN_POINT('Ctrl Pts',(-6.95190262372793,17.2154595136883,-321.680332035678)) ;
#38711 = CARTESIAN_POINT('Ctrl Pts',(-7.1922032880742,17.1172064025887,-321.677040892551)) ;
#38712 = CARTESIAN_POINT('Ctrl Pts',(-7.35690764339327,17.0470658264597,-321.674798010701)) ;
#38713 = CARTESIAN_POINT('Ctrl Pts',(-7.78035955291097,16.859455563299,-321.669037818533)) ;
#38714 = CARTESIAN_POINT('Ctrl Pts',(-8.03747085924693,16.7384079070025,-321.665546055258)) ;
#38715 = CARTESIAN_POINT('Ctrl Pts',(-8.92505589653861,16.2953661495479,-321.653384775717)) ;
#38716 = CARTESIAN_POINT('Ctrl Pts',(-9.53981093312355,15.943261511577,-321.644746594839)) ;
#38717 = CARTESIAN_POINT('Ctrl Pts',(-10.263522168483,15.4718742367918,-321.633879358036)) ;
#38718 = CARTESIAN_POINT('Ctrl Pts',(-10.3930132002504,15.3851895090078,-321.631907415922)) ;
#38719 = CARTESIAN_POINT('Ctrl Pts',(-10.6256039078403,15.2252105798601,-321.628312224208)) ;
#38720 = CARTESIAN_POINT('Ctrl Pts',(-10.7290750709102,15.1524731868025,-321.626693353294)) ;
#38721 = CARTESIAN_POINT('Ctrl Pts',(-10.9393947051829,15.0013897709901,-321.623361547521)) ;
#38722 = CARTESIAN_POINT('Ctrl Pts',(-11.0461640351006,14.9229458092083,-321.621647890495)) ;
#38723 = CARTESIAN_POINT('Ctrl Pts',(-11.3232203741165,14.7147884591784,-321.617142003634)) ;
#38724 = CARTESIAN_POINT('Ctrl Pts',(-11.4921195280334,14.5832612108531,-321.614335517162)) ;
#38725 = CARTESIAN_POINT('Ctrl Pts',(-11.7710476516844,14.3581953660808,-321.609602225746)) ;
#38726 = CARTESIAN_POINT('Ctrl Pts',(-11.8823278815949,14.2662406063667,-321.607686773499)) ;
#38727 = CARTESIAN_POINT('Ctrl Pts',(-12.3569680743402,13.864622385992,-321.599404245368)) ;
#38728 = CARTESIAN_POINT('Ctrl Pts',(-12.70938147799,13.542305376322,-321.592960822087)) ;
#38729 = CARTESIAN_POINT('Ctrl Pts',(-13.1888076029562,13.0686071696249,-321.583888466479)) ;
#38730 = CARTESIAN_POINT('Ctrl Pts',(-13.326433789351,12.9282366117419,-321.581246674254)) ;
#38731 = CARTESIAN_POINT('Ctrl Pts',(-13.6277804579957,12.6109549736229,-321.575398008909)) ;
#38732 = CARTESIAN_POINT('Ctrl Pts',(-13.7903377390698,12.4329872113515,-321.572198863869)) ;
#38733 = CARTESIAN_POINT('Ctrl Pts',(-14.0033019680442,12.1905171745171,-321.567974764716)) ;
#38734 = CARTESIAN_POINT('Ctrl Pts',(-14.0568138828617,12.1287739890283,-321.566910509794)) ;
#38735 = CARTESIAN_POINT('Ctrl Pts',(-14.1530416783587,12.0162520514127,-321.564993115923)) ;
#38736 = CARTESIAN_POINT('Ctrl Pts',(-14.1958961934523,11.9655937341931,-321.564137973355)) ;
#38737 = CARTESIAN_POINT('Ctrl Pts',(-14.290312509757,11.8527630346874,-321.562251688621)) ;
#38738 = CARTESIAN_POINT('Ctrl Pts',(-14.3417419203426,11.7904818348291,-321.561222457326)) ;
#38739 = CARTESIAN_POINT('Ctrl Pts',(-14.5065158545704,11.5882666969086,-321.55791584383)) ;
#38740 = CARTESIAN_POINT('Ctrl Pts',(-14.6182315254804,11.4470185877134,-321.555659828862)) ;
#38741 = CARTESIAN_POINT('Ctrl Pts',(-14.9025557995998,11.0765806667062,-321.549852844566)) ;
#38742 = CARTESIAN_POINT('Ctrl Pts',(-15.0719382923908,10.8449751108958,-321.546327916026)) ;
#38743 = CARTESIAN_POINT('Ctrl Pts',(-15.6361128171834,10.0347891237646,-321.534225822185)) ;
#38744 = CARTESIAN_POINT('Ctrl Pts',(-16.0034974686149,9.43785383690433,-321.525677257406)) ;
#38745 = CARTESIAN_POINT('Ctrl Pts',(-16.4190670036199,8.66828111787151,-321.5146752888)) ;
#38746 = CARTESIAN_POINT('Ctrl Pts',(-16.499694292565,8.51380919030238,-321.512469312529)) ;
#38747 = CARTESIAN_POINT('Ctrl Pts',(-16.6348258776578,8.24578223896283,-321.508641902744)) ;
#38748 = CARTESIAN_POINT('Ctrl Pts',(-16.6903710473401,8.13276527151816,-321.507028117773)) ;
#38749 = CARTESIAN_POINT('Ctrl Pts',(-16.8037554534973,7.89600888900553,-321.503646694235)) ;
#38750 = CARTESIAN_POINT('Ctrl Pts',(-16.8613876501391,7.77217859805641,-321.501877689096)) ;
#38751 = CARTESIAN_POINT('Ctrl Pts',(-17.0154569842627,7.43135943921193,-321.497007335688)) ;
#38752 = CARTESIAN_POINT('Ctrl Pts',(-17.1091058977917,7.21313902140694,-321.49388704746)) ;
#38753 = CARTESIAN_POINT('Ctrl Pts',(-17.4434474832382,6.39088278290552,-321.482132718024)) ;
#38754 = CARTESIAN_POINT('Ctrl Pts',(-17.6565429536326,5.77613442327295,-321.473334193799)) ;
#38755 = CARTESIAN_POINT('Ctrl Pts',(-17.9337361569647,4.81635581475174,-321.459908429103)) ;
#38756 = CARTESIAN_POINT('Ctrl Pts',(-18.0210597868333,4.47856906930221,-321.45524464081)) ;
#38757 = CARTESIAN_POINT('Ctrl Pts',(-18.1208090108261,4.04234028817951,-321.449374925292)) ;
#38758 = CARTESIAN_POINT('Ctrl Pts',(-18.1420353476001,3.94598374300328,-321.448087988367)) ;
#38759 = CARTESIAN_POINT('Ctrl Pts',(-18.1762782288956,3.78441934811357,-321.445948790714)) ;
#38760 = CARTESIAN_POINT('Ctrl Pts',(-18.1897143551459,3.71930259201257,-321.44509173517)) ;
#38761 = CARTESIAN_POINT('Ctrl Pts',(-18.2185677140576,3.57557094725609,-321.44321182946)) ;
#38762 = CARTESIAN_POINT('Ctrl Pts',(-18.2338264609811,3.49692575915674,-321.442190774184)) ;
#38763 = CARTESIAN_POINT('Ctrl Pts',(-18.2809559628799,3.24531665021227,-321.438945017754)) ;
#38764 = CARTESIAN_POINT('Ctrl Pts',(-18.3108782737827,3.07199741370157,-321.43674061953)) ;
#38765 = CARTESIAN_POINT('Ctrl Pts',(-18.3814490209434,2.62547384533979,-321.431116143139)) ;
#38766 = CARTESIAN_POINT('Ctrl Pts',(-18.4184716994345,2.3517401358521,-321.427720204435)) ;
#38767 = CARTESIAN_POINT('Ctrl Pts',(-18.5302756169096,1.35875415618312,-321.415466975611)) ;
#38768 = CARTESIAN_POINT('Ctrl Pts',(-18.5691326711767,0.636112376331237,
-321.406649262026)) ;
#38769 = CARTESIAN_POINT('Ctrl Pts',(-18.5650214629265,-0.241742058535704,
-321.395601475048)) ;
#38770 = CARTESIAN_POINT('Ctrl Pts',(-18.5623606325034,-0.39652086832534,
-321.393642168482)) ;
#38771 = CARTESIAN_POINT('Ctrl Pts',(-18.554015991005,-0.67744317070272,-321.390062424453)) ;
#38772 = CARTESIAN_POINT('Ctrl Pts',(-18.5489803257875,-0.803596580637598,
-321.388446231327)) ;
#38773 = CARTESIAN_POINT('Ctrl Pts',(-18.5360057298744,-1.06237513830523,
-321.385112190483)) ;
#38774 = CARTESIAN_POINT('Ctrl Pts',(-18.5279291130494,-1.19498622238906,
-321.383393539874)) ;
#38775 = CARTESIAN_POINT('Ctrl Pts',(-18.5029748879721,-1.5430942410394,-321.378854997202)) ;
#38776 = CARTESIAN_POINT('Ctrl Pts',(-18.4837560873108,-1.75840273852584,
-321.376020449715)) ;
#38777 = CARTESIAN_POINT('Ctrl Pts',(-18.4315581388728,-2.24672290020516,
-321.369533046572)) ;
#38778 = CARTESIAN_POINT('Ctrl Pts',(-18.3962642893974,-2.51943624577202,
-321.365867937757)) ;
#38779 = CARTESIAN_POINT('Ctrl Pts',(-18.2928622568172,-3.19939213119415,
-321.356649462532)) ;
#38780 = CARTESIAN_POINT('Ctrl Pts',(-18.2172026127313,-3.60533605136708,
-321.351071687942)) ;
#38781 = CARTESIAN_POINT('Ctrl Pts',(-18.0526673496658,-4.34944676330505,
-321.340829769545)) ;
#38782 = CARTESIAN_POINT('Ctrl Pts',(-17.9676520818475,-4.68827954790101,
-321.336159915841)) ;
#38783 = CARTESIAN_POINT('Ctrl Pts',(-17.8464172843778,-5.11953437651732,
-321.330283798345)) ;
#38784 = CARTESIAN_POINT('Ctrl Pts',(-17.8189472675903,-5.21434180282661,
-321.328996327711)) ;
#38785 = CARTESIAN_POINT('Ctrl Pts',(-17.7717088874472,-5.37264217338237,
-321.326856534197)) ;
#38786 = CARTESIAN_POINT('Ctrl Pts',(-17.7523531157764,-5.43625602711678,
-321.325999410075)) ;
#38787 = CARTESIAN_POINT('Ctrl Pts',(-17.7089314123988,-5.57625876556316,
-321.324119715452)) ;
#38788 = CARTESIAN_POINT('Ctrl Pts',(-17.6847121379826,-5.65259853606334,
-321.323098935911)) ;
#38789 = CARTESIAN_POINT('Ctrl Pts',(-17.6057745591643,-5.89593791946631,
-321.319855212502)) ;
#38790 = CARTESIAN_POINT('Ctrl Pts',(-17.5491787803681,-6.06231854184286,
-321.31765253648)) ;
#38791 = CARTESIAN_POINT('Ctrl Pts',(-17.3977002568815,-6.48772783950895,
-321.312034085747)) ;
#38792 = CARTESIAN_POINT('Ctrl Pts',(-17.2993913045127,-6.7454909107858,-321.308642388856)) ;
#38793 = CARTESIAN_POINT('Ctrl Pts',(-16.9218236738815,-7.67285086517161,
-321.296364294087)) ;
#38794 = CARTESIAN_POINT('Ctrl Pts',(-16.6091271095143,-8.32812423915863,
-321.28751796952)) ;
#38795 = CARTESIAN_POINT('Ctrl Pts',(-16.1844895669003,-9.09838166631953,
-321.276447431909)) ;
#38796 = CARTESIAN_POINT('Ctrl Pts',(-16.10840611673,-9.23241592298982,-321.274496487235)) ;
#38797 = CARTESIAN_POINT('Ctrl Pts',(-15.967050667723,-9.47437039733924,-321.270926941445)) ;
#38798 = CARTESIAN_POINT('Ctrl Pts',(-15.9023309449355,-9.58260256487726,
-321.269312496044)) ;
#38799 = CARTESIAN_POINT('Ctrl Pts',(-15.7670413936007,-9.80370451854424,
-321.265976833247)) ;
#38800 = CARTESIAN_POINT('Ctrl Pts',(-15.6963502084062,-9.91649165111407,
-321.264254758497)) ;
#38801 = CARTESIAN_POINT('Ctrl Pts',(-15.5069229827646,-10.2116199437786,
-321.259693817793)) ;
#38802 = CARTESIAN_POINT('Ctrl Pts',(-15.3861839077494,-10.3926506131017,
-321.256840020618)) ;
#38803 = CARTESIAN_POINT('Ctrl Pts',(-15.1041888982384,-10.7997719307196,
-321.250296723522)) ;
#38804 = CARTESIAN_POINT('Ctrl Pts',(-14.94098638489,-11.0244510725298,-321.2465946287)) ;
#38805 = CARTESIAN_POINT('Ctrl Pts',(-14.5227354164783,-11.5738978646879,
-321.237337398802)) ;
#38806 = CARTESIAN_POINT('Ctrl Pts',(-14.2617757511996,-11.8939777922701,
-321.231758688496)) ;
#38807 = CARTESIAN_POINT('Ctrl Pts',(-13.7640319265021,-12.4645279967601,
-321.22158476529)) ;
#38808 = CARTESIAN_POINT('Ctrl Pts',(-13.5305274002108,-12.7176201458588,
-321.21698279818)) ;
#38809 = CARTESIAN_POINT('Ctrl Pts',(-13.2213439333629,-13.0345796016436,
-321.211175022859)) ;
#38810 = CARTESIAN_POINT('Ctrl Pts',(-13.1520071673275,-13.1045376991168,
-321.209890343524)) ;
#38811 = CARTESIAN_POINT('Ctrl Pts',(-13.0349531942135,-13.2207757927619,
-321.207753664809)) ;
#38812 = CARTESIAN_POINT('Ctrl Pts',(-12.9875382713322,-13.2673571981927,
-321.206896897808)) ;
#38813 = CARTESIAN_POINT('Ctrl Pts',(-12.8823586180403,-13.3695837159411,
-321.205016091625)) ;
#38814 = CARTESIAN_POINT('Ctrl Pts',(-12.8244814940322,-13.4251110510982,
-321.203993864037)) ;
#38815 = CARTESIAN_POINT('Ctrl Pts',(-12.6381150642949,-13.601606123072,-321.200739450131)) ;
#38816 = CARTESIAN_POINT('Ctrl Pts',(-12.5082600044262,-13.7211177882528,
-321.198527716494)) ;
#38817 = CARTESIAN_POINT('Ctrl Pts',(-12.1697321553273,-14.023880797109,-321.192877529467)) ;
#38818 = CARTESIAN_POINT('Ctrl Pts',(-11.9586159832558,-14.2043344617312,
-321.18946347939)) ;
#38819 = CARTESIAN_POINT('Ctrl Pts',(-11.5584460208683,-14.5311365177886,
-321.183128385953)) ;
#38820 = CARTESIAN_POINT('Ctrl Pts',(-11.3704594376938,-14.6787007294498,
-321.180205678497)) ;
#38821 = CARTESIAN_POINT('Ctrl Pts',(-11.1364970237608,-14.8551626918416,
-321.176610858299)) ;
#38822 = CARTESIAN_POINT('Ctrl Pts',(-11.0931750088994,-14.8875415291433,
-321.175946991067)) ;
#38823 = CARTESIAN_POINT('Ctrl Pts',(-10.7170795188159,-15.1660818736563,
-321.170197464649)) ;
#38824 = CARTESIAN_POINT('Ctrl Pts',(-10.3763020132811,-15.4012398305283,
-321.165077653316)) ;
#38825 = CARTESIAN_POINT('Ctrl Pts',(-9.87855046465923,-15.720695100656,-321.157641884768)) ;
#38826 = CARTESIAN_POINT('Ctrl Pts',(-9.72778275923691,-15.8144318956399,
-321.155395421945)) ;
#38827 = CARTESIAN_POINT('Ctrl Pts',(-9.46741128734566,-15.9711802195836,
-321.151521572812)) ;
#38828 = CARTESIAN_POINT('Ctrl Pts',(-9.35846566829252,-16.0352609698795,
-321.149902370479)) ;
#38829 = CARTESIAN_POINT('Ctrl Pts',(-9.1314697835787,-16.1656763734935,-321.146531202773)) ;
#38830 = CARTESIAN_POINT('Ctrl Pts',(-9.01333098238725,-16.2318420875986,
-321.144778098761)) ;
#38831 = CARTESIAN_POINT('Ctrl Pts',(-8.69201142966656,-16.4072130754982,
-321.140013315394)) ;
#38832 = CARTESIAN_POINT('Ctrl Pts',(-8.48750237065317,-16.5139337166767,
-321.136984106584)) ;
#38833 = CARTESIAN_POINT('Ctrl Pts',(-8.13663973559233,-16.6887875492076,
-321.131796748152)) ;
#38834 = CARTESIAN_POINT('Ctrl Pts',(-7.99128912571933,-16.7588732936713,
-321.129650632382)) ;
#38835 = CARTESIAN_POINT('Ctrl Pts',(-7.30430432112103,-17.0791566467067,
-321.11952925617)) ;
#38836 = CARTESIAN_POINT('Ctrl Pts',(-6.75172893726466,-17.3050457214866,
-321.111439588634)) ;
#38837 = CARTESIAN_POINT('Ctrl Pts',(-6.02972049173782,-17.5603416286927,
-321.101187198994)) ;
#38838 = CARTESIAN_POINT('Ctrl Pts',(-5.86943732355182,-17.6145630926653,
-321.098931735677)) ;
#38839 = CARTESIAN_POINT('Ctrl Pts',(-5.57070866755272,-17.7110884316116,
-321.094778502953)) ;
#38840 = CARTESIAN_POINT('Ctrl Pts',(-5.43246610636719,-17.7539787261206,
-321.092876318307)) ;
#38841 = CARTESIAN_POINT('Ctrl Pts',(-5.22205801705098,-17.8165709907623,
-321.090018272863)) ;
#38842 = CARTESIAN_POINT('Ctrl Pts',(-5.15025175736081,-17.8374605439789,
-321.089049422022)) ;
#38843 = CARTESIAN_POINT('Ctrl Pts',(-5.01251899244279,-17.8766281170937,
-321.087204857893)) ;
#38844 = CARTESIAN_POINT('Ctrl Pts',(-4.94661392167707,-17.8949766747085,
-321.086328379568)) ;
#38845 = CARTESIAN_POINT('Ctrl Pts',(-4.77332140743007,-17.9421923760844,
-321.084038318427)) ;
#38846 = CARTESIAN_POINT('Ctrl Pts',(-4.66577327704844,-17.9704597688143,
-321.082631655385)) ;
#38847 = CARTESIAN_POINT('Ctrl Pts',(-4.42100569489804,-18.0324477717365,
-321.07945728508)) ;
#38848 = CARTESIAN_POINT('Ctrl Pts',(-4.2836421025616,-18.0655715220009,-321.077694995562)) ;
#38849 = CARTESIAN_POINT('Ctrl Pts',(-3.80869134639994,-18.1743791335283,
-321.071650161654)) ;
#38850 = CARTESIAN_POINT('Ctrl Pts',(-3.4693750718466,-18.2421935053115,-321.067414504976)) ;
#38851 = CARTESIAN_POINT('Ctrl Pts',(-2.55090668467733,-18.3992003563335,
-321.056001949037)) ;
#38852 = CARTESIAN_POINT('Ctrl Pts',(-1.96910279591997,-18.4705260229598,
-321.048819995786)) ;
#38853 = CARTESIAN_POINT('Ctrl Pts',(-1.19977361247041,-18.528073501455,-321.039133731395)) ;
#38854 = CARTESIAN_POINT('Ctrl Pts',(-1.01444628055894,-18.5391440736732,
-321.036787103497)) ;
#38855 = CARTESIAN_POINT('Ctrl Pts',(-0.70274171273618,-18.5530758239662,
-321.032813177132)) ;
#38856 = CARTESIAN_POINT('Ctrl Pts',(-0.576444870820422,-18.5574292320431,
-321.03119558323)) ;
#38857 = CARTESIAN_POINT('Ctrl Pts',(-0.317494920592336,-18.5637090696417,
-321.02786274773)) ;
#38858 = CARTESIAN_POINT('Ctrl Pts',(-0.184845762462451,-18.5655037483158,
-321.026146745863)) ;
#38859 = CARTESIAN_POINT('Ctrl Pts',(0.162848336460811,-18.5664811205678,
-321.021625525326)) ;
#38860 = CARTESIAN_POINT('Ctrl Pts',(0.377879500041982,-18.5633495795523,
-321.018805863255)) ;
#38861 = CARTESIAN_POINT('Ctrl Pts',(0.865538594469597,-18.5477707712694,
-321.012361536018)) ;
#38862 = CARTESIAN_POINT('Ctrl Pts',(1.13804417427402,-18.5330465032616,-321.00872487761)) ;
#38863 = CARTESIAN_POINT('Ctrl Pts',(1.76035905674306,-18.4856433641254,-321.000360923647)) ;
#38864 = CARTESIAN_POINT('Ctrl Pts',(2.10976473556348,-18.4490316012564,-320.995621477894)) ;
#38865 = CARTESIAN_POINT('Ctrl Pts',(2.67472303940375,-18.3735733562417,-320.987949575845)) ;
#38866 = CARTESIAN_POINT('Ctrl Pts',(2.89099700256591,-18.3407872698519,-320.985010980969)) ;
#38867 = CARTESIAN_POINT('Ctrl Pts',(3.32395468581166,-18.2673044038235,-320.979150678499)) ;
#38868 = CARTESIAN_POINT('Ctrl Pts',(3.54059455844515,-18.2265541293349,-320.976229747398)) ;
#38869 = CARTESIAN_POINT('Ctrl Pts',(3.84180506439198,-18.1643229535366,-320.972206660472)) ;
#38870 = CARTESIAN_POINT('Ctrl Pts',(3.9270273744167,-18.1460891252998,-320.971072710082)) ;
#38871 = CARTESIAN_POINT('Ctrl Pts',(4.07631377204857,-18.1130474626584,-320.969095827574)) ;
#38872 = CARTESIAN_POINT('Ctrl Pts',(4.14043325883232,-18.0984981365315,-320.968249958418)) ;
#38873 = CARTESIAN_POINT('Ctrl Pts',(4.28957087228558,-18.063823349431,-320.96628997208)) ;
#38874 = CARTESIAN_POINT('Ctrl Pts',(4.37452674907062,-18.0434378104393,-320.965178879921)) ;
#38875 = CARTESIAN_POINT('Ctrl Pts',(4.68093816193899,-17.9676217544116,-320.961186340006)) ;
#38876 = CARTESIAN_POINT('Ctrl Pts',(4.90151098323219,-17.9087074923046,-320.958340182304)) ;
#38877 = CARTESIAN_POINT('Ctrl Pts',(5.54119533449275,-17.7251462613375,-320.950105384838)) ;
#38878 = CARTESIAN_POINT('Ctrl Pts',(5.95705865844338,-17.5897444218911,-320.944773699598)) ;
#38879 = CARTESIAN_POINT('Ctrl Pts',(6.52898730769165,-17.3809173002409,-320.937306280708)) ;
#38880 = CARTESIAN_POINT('Ctrl Pts',(6.68939668491061,-17.3198133189774,-320.935197241083)) ;
#38881 = CARTESIAN_POINT('Ctrl Pts',(7.18265247710496,-17.1240448640527,-320.928650009788)) ;
#38882 = CARTESIAN_POINT('Ctrl Pts',(7.51245640728795,-16.9819435579419,-320.924182775271)) ;
#38883 = CARTESIAN_POINT('Ctrl Pts',(7.97955432853323,-16.7644152610639,-320.917678466205)) ;
#38884 = CARTESIAN_POINT('Ctrl Pts',(8.12033879191652,-16.6966764397983,-320.91569461067)) ;
#38885 = CARTESIAN_POINT('Ctrl Pts',(8.37137484181892,-16.571963634615,-320.912112281403)) ;
#38886 = CARTESIAN_POINT('Ctrl Pts',(8.48194197793596,-16.5156457845681,-320.910518610243)) ;
#38887 = CARTESIAN_POINT('Ctrl Pts',(8.72171101956119,-16.3904755162238,-320.907027147084)) ;
#38888 = CARTESIAN_POINT('Ctrl Pts',(8.85067990100838,-16.3211946855445,-320.905126311799)) ;
#38889 = CARTESIAN_POINT('Ctrl Pts',(9.2401331729044,-16.1060104399365,-320.89931640354)) ;
#38890 = CARTESIAN_POINT('Ctrl Pts',(9.49792926356835,-15.9553430677548,-320.895373679594)) ;
#38891 = CARTESIAN_POINT('Ctrl Pts',(10.1495847319862,-15.5530947181484,-320.885174929886)) ;
#38892 = CARTESIAN_POINT('Ctrl Pts',(10.5377826787426,-15.2927420819336,-320.878871342854)) ;
#38893 = CARTESIAN_POINT('Ctrl Pts',(11.0519558102177,-14.9190189967723,-320.87031301975)) ;
#38894 = CARTESIAN_POINT('Ctrl Pts',(11.1868146477109,-14.8181656470127,-320.868048380536)) ;
#38895 = CARTESIAN_POINT('Ctrl Pts',(11.5250936291658,-14.5579355553234,-320.862330984766)) ;
#38896 = CARTESIAN_POINT('Ctrl Pts',(11.7265931647289,-14.3961204488615,-320.858890585307)) ;
#38897 = CARTESIAN_POINT('Ctrl Pts',(12.0030453667017,-14.1644577368843,-320.854155430891)) ;
#38898 = CARTESIAN_POINT('Ctrl Pts',(12.080896989979,-14.0981165060473,-320.852820306291)) ;
#38899 = CARTESIAN_POINT('Ctrl Pts',(12.2088074101956,-13.9872801416566,-320.850626801878)) ;
#38900 = CARTESIAN_POINT('Ctrl Pts',(12.2591807240461,-13.9431514427424,-320.84976304513)) ;
#38901 = CARTESIAN_POINT('Ctrl Pts',(12.347012908264,-13.8653635923331,-320.848257719402)) ;
#38902 = CARTESIAN_POINT('Ctrl Pts',(12.3845755026972,-13.8318229069246,-320.847614098582)) ;
#38903 = CARTESIAN_POINT('Ctrl Pts',(12.422830908549,-13.797382826699,-320.846958501836)) ;
#38904 = CARTESIAN_POINT('Ctrl Pts',(12.4236605585145,-13.7966357847014,-320.846944283774)) ;
#38905 = CARTESIAN_POINT('Ctrl Pts',(12.4253334184184,-13.7951292176448,-320.846915615159)) ;
#38906 = CARTESIAN_POINT('Ctrl Pts',(12.4261766261117,-13.7943696900967,-320.846901164644)) ;
#38907 = CARTESIAN_POINT('Ctrl Pts',(12.4278775871989,-13.792837250299,-320.846872014218)) ;
#38908 = CARTESIAN_POINT('Ctrl Pts',(12.4287353381248,-13.7920643353518,-320.846857314349)) ;
#38909 = CARTESIAN_POINT('Ctrl Pts',(12.4304664070157,-13.7905041854523,-320.8468276477)) ;
#38910 = CARTESIAN_POINT('Ctrl Pts',(12.4313397223338,-13.7897169475247,-320.846812680963)) ;
#38911 = CARTESIAN_POINT('Ctrl Pts',(12.4331029805614,-13.7881271793275,-320.846782462391)) ;
#38912 = CARTESIAN_POINT('Ctrl Pts',(12.4339929205518,-13.7873246458557,-320.846767210603)) ;
#38913 = CARTESIAN_POINT('Ctrl Pts',(12.4357905311635,-13.7857032741128,-320.846736403009)) ;
#38914 = CARTESIAN_POINT('Ctrl Pts',(12.4366981986449,-13.7848844323297,-320.846720847254)) ;
#38915 = CARTESIAN_POINT('Ctrl Pts',(12.4385324136172,-13.7832293877603,-320.846689412012)) ;
#38916 = CARTESIAN_POINT('Ctrl Pts',(12.4394589576725,-13.7823931811789,-320.84667353258)) ;
#38917 = CARTESIAN_POINT('Ctrl Pts',(12.4413321252574,-13.7807023035147,-320.846641429409)) ;
#38918 = CARTESIAN_POINT('Ctrl Pts',(12.442278745047,-13.7798476283161,-320.846625205729)) ;
#38919 = CARTESIAN_POINT('Ctrl Pts',(12.4441933176402,-13.7781186588381,-320.846592392559)) ;
#38920 = CARTESIAN_POINT('Ctrl Pts',(12.4451612663977,-13.7772443600736,-320.846575803134)) ;
#38921 = CARTESIAN_POINT('Ctrl Pts',(12.4471198088701,-13.7754749336878,-320.846542235964)) ;
#38922 = CARTESIAN_POINT('Ctrl Pts',(12.4481103981702,-13.7745798012134,-320.84652525829)) ;
#38923 = CARTESIAN_POINT('Ctrl Pts',(12.4501155964154,-13.7727674382869,-320.846490891038)) ;
#38924 = CARTESIAN_POINT('Ctrl Pts',(12.4511302005791,-13.7718502025498,-320.846473501536)) ;
#38925 = CARTESIAN_POINT('Ctrl Pts',(12.4531848707809,-13.769992300043,-320.846438285883)) ;
#38926 = CARTESIAN_POINT('Ctrl Pts',(12.454224931607,-13.7690516275461,-320.846420459814)) ;
#38927 = CARTESIAN_POINT('Ctrl Pts',(12.4563320297982,-13.767145449827,-320.846384345035)) ;
#38928 = CARTESIAN_POINT('Ctrl Pts',(12.4573990615042,-13.7661799383745,-320.846366056414)) ;
#38929 = CARTESIAN_POINT('Ctrl Pts',(12.45956169374,-13.7642226074135,-320.846328989207)) ;
#38930 = CARTESIAN_POINT('Ctrl Pts',(12.4606572881552,-13.7632307810954,-320.846310210716)) ;
#38931 = CARTESIAN_POINT('Ctrl Pts',(12.4628787214654,-13.7612192658872,-320.84627213501)) ;
#38932 = CARTESIAN_POINT('Ctrl Pts',(12.4640045536628,-13.7601995696302,-320.8462528379)) ;
#38933 = CARTESIAN_POINT('Ctrl Pts',(12.4662882272162,-13.7581306753456,-320.846213694666)) ;
#38934 = CARTESIAN_POINT('Ctrl Pts',(12.467446061298,-13.7570814692848,-320.846193848656)) ;
#38935 = CARTESIAN_POINT('Ctrl Pts',(12.4697955986901,-13.7549518253206,-320.846153575691)) ;
#38936 = CARTESIAN_POINT('Ctrl Pts',(12.4709872940606,-13.753871378684,-320.84613314886)) ;
#38937 = CARTESIAN_POINT('Ctrl Pts',(12.4734065159742,-13.7516774262804,-320.846091680573)) ;
#38938 = CARTESIAN_POINT('Ctrl Pts',(12.4746340338825,-13.7505639109789,-320.84607063925)) ;
#38939 = CARTESIAN_POINT('Ctrl Pts',(12.4771269717987,-13.7483018897778,-320.84602790642)) ;
#38940 = CARTESIAN_POINT('Ctrl Pts',(12.4783923823665,-13.7471533735007,-320.84600621506)) ;
#38941 = CARTESIAN_POINT('Ctrl Pts',(12.4809632928688,-13.7448193074489,-320.845962144594)) ;
#38942 = CARTESIAN_POINT('Ctrl Pts',(12.4822687824885,-13.7436337463595,-320.845939765649)) ;
#38943 = CARTESIAN_POINT('Ctrl Pts',(12.4849221626022,-13.7412234285417,-320.845894280315)) ;
#38944 = CARTESIAN_POINT('Ctrl Pts',(12.4862700418181,-13.7399986594663,-320.845871174101)) ;
#38945 = CARTESIAN_POINT('Ctrl Pts',(12.489010645151,-13.7375076360629,-320.845824192248)) ;
#38946 = CARTESIAN_POINT('Ctrl Pts',(12.4904033569655,-13.7362413682159,-320.845800316799)) ;
#38947 = CARTESIAN_POINT('Ctrl Pts',(12.4932362110586,-13.733664921199,-320.845751752057)) ;
#38948 = CARTESIAN_POINT('Ctrl Pts',(12.4946763398566,-13.7323547272602,-320.845727062971)) ;
#38949 = CARTESIAN_POINT('Ctrl Pts',(12.4976067642843,-13.7296878562249,-320.845676823939)) ;
#38950 = CARTESIAN_POINT('Ctrl Pts',(12.4990970451752,-13.7283311629399,-320.845651274217)) ;
#38951 = CARTESIAN_POINT('Ctrl Pts',(12.5021306711494,-13.7255685653632,-320.84559926412)) ;
#38952 = CARTESIAN_POINT('Ctrl Pts',(12.5036740000402,-13.724162643371,-320.845572803991)) ;
#38953 = CARTESIAN_POINT('Ctrl Pts',(12.5068167907788,-13.7212986939471,-320.845518920331)) ;
#38954 = CARTESIAN_POINT('Ctrl Pts',(12.5084162349025,-13.719840647072,-320.845491497067)) ;
#38955 = CARTESIAN_POINT('Ctrl Pts',(12.5116745077088,-13.7168693752333,-320.845435631234)) ;
#38956 = CARTESIAN_POINT('Ctrl Pts',(12.5133333169261,-13.715356128937,-320.845407188957)) ;
#38957 = CARTESIAN_POINT('Ctrl Pts',(12.5167137664157,-13.7122711950416,-320.845349225831)) ;
#38958 = CARTESIAN_POINT('Ctrl Pts',(12.5184353852484,-13.7106994840565,-320.845319705302)) ;
#38959 = CARTESIAN_POINT('Ctrl Pts',(12.5207010381076,-13.7086303276533,-320.845280855335)) ;
#38960 = CARTESIAN_POINT('Ctrl Pts',(12.5212453385744,-13.7081331740378,-320.845271521949)) ;
#38961 = CARTESIAN_POINT('Ctrl Pts',(12.52238946442,-13.707088026418,-320.845251902919)) ;
#38962 = CARTESIAN_POINT('Ctrl Pts',(12.5229892833514,-13.7065400255372,-320.845241617369)) ;
#38963 = CARTESIAN_POINT('Ctrl Pts',(12.5242505324788,-13.7053875831748,-320.845219989595)) ;
#38964 = CARTESIAN_POINT('Ctrl Pts',(12.5249119549761,-13.7047831331048,-320.845208647484)) ;
#38965 = CARTESIAN_POINT('Ctrl Pts',(12.5263032406586,-13.7035115026549,-320.845184789413)) ;
#38966 = CARTESIAN_POINT('Ctrl Pts',(12.5270330943375,-13.70284431181,-320.845172273595)) ;
#38967 = CARTESIAN_POINT('Ctrl Pts',(12.5285689174822,-13.7014401241312,-320.845145936418)) ;
#38968 = CARTESIAN_POINT('Ctrl Pts',(12.5293748751748,-13.7007031145336,-320.845132115234)) ;
#38969 = CARTESIAN_POINT('Ctrl Pts',(12.5310715453699,-13.6991513162155,-320.845103019084)) ;
#38970 = CARTESIAN_POINT('Ctrl Pts',(12.5319622434424,-13.6983365117332,-320.845087744329)) ;
#38971 = CARTESIAN_POINT('Ctrl Pts',(12.533838134394,-13.6966201234746,-320.845055573887)) ;
#38972 = CARTESIAN_POINT('Ctrl Pts',(12.5348233094746,-13.6957185202607,-320.845038678459)) ;
#38973 = CARTESIAN_POINT('Ctrl Pts',(12.5368991531778,-13.693818357647,-320.845003077894)) ;
#38974 = CARTESIAN_POINT('Ctrl Pts',(12.537989799808,-13.6928197742134,-320.844984373078)) ;
#38975 = CARTESIAN_POINT('Ctrl Pts',(12.5402890262243,-13.6907141240886,-320.844944940207)) ;
#38976 = CARTESIAN_POINT('Ctrl Pts',(12.5414975787445,-13.6896070276363,-320.844924212547)) ;
#38977 = CARTESIAN_POINT('Ctrl Pts',(12.5440467071742,-13.6872712736131,-320.844880492086)) ;
#38978 = CARTESIAN_POINT('Ctrl Pts',(12.5453872492322,-13.6860425790674,-320.844857499776)) ;
#38979 = CARTESIAN_POINT('Ctrl Pts',(12.5482163392036,-13.6834487679956,-320.844808975583)) ;
#38980 = CARTESIAN_POINT('Ctrl Pts',(12.5497048449031,-13.6820836054905,-320.844783444308)) ;
#38981 = CARTESIAN_POINT('Ctrl Pts',(12.5528480138123,-13.6791999469402,-320.84472953045)) ;
#38982 = CARTESIAN_POINT('Ctrl Pts',(12.5545026243144,-13.6776813935083,-320.844701148622)) ;
#38983 = CARTESIAN_POINT('Ctrl Pts',(12.5579986406389,-13.6744716824819,-320.844641179143)) ;
#38984 = CARTESIAN_POINT('Ctrl Pts',(12.5598399805121,-13.6727804530469,-320.844609592432)) ;
#38985 = CARTESIAN_POINT('Ctrl Pts',(12.5637329407349,-13.6692034062649,-320.844542809657)) ;
#38986 = CARTESIAN_POINT('Ctrl Pts',(12.5657844782362,-13.6673174988537,-320.844507614768)) ;
#38987 = CARTESIAN_POINT('Ctrl Pts',(12.570124574674,-13.6633259951856,-320.844433156025)) ;
#38988 = CARTESIAN_POINT('Ctrl Pts',(12.5724130293264,-13.6612202856685,-320.84439389364)) ;
#38989 = CARTESIAN_POINT('Ctrl Pts',(12.5772574159256,-13.656760500591,-320.844310776258)) ;
#38990 = CARTESIAN_POINT('Ctrl Pts',(12.5798132163043,-13.6544062822173,-320.844266923099)) ;
#38991 = CARTESIAN_POINT('Ctrl Pts',(12.5852269761786,-13.649416708182,-320.844174027606)) ;
#38992 = CARTESIAN_POINT('Ctrl Pts',(12.5880847692085,-13.6467811720843,-320.844124987578)) ;
#38993 = CARTESIAN_POINT('Ctrl Pts',(12.5941419839316,-13.6411915188584,-320.844021039087)) ;
#38994 = CARTESIAN_POINT('Ctrl Pts',(12.597341194515,-13.638237173278,-320.84396613352)) ;
#38995 = CARTESIAN_POINT('Ctrl Pts',(12.6041261097789,-13.6319671457317,-320.843849681353)) ;
#38996 = CARTESIAN_POINT('Ctrl Pts',(12.6077115462354,-13.6286511739221,-320.843788138393)) ;
#38997 = CARTESIAN_POINT('Ctrl Pts',(12.6153198202074,-13.6216091304664,-320.843657534154)) ;
#38998 = CARTESIAN_POINT('Ctrl Pts',(12.6193423163008,-13.6178826905415,-320.843588477452)) ;
#38999 = CARTESIAN_POINT('Ctrl Pts',(12.6278823246765,-13.6099641945841,-320.843441851935)) ;
#39000 = CARTESIAN_POINT('Ctrl Pts',(12.6323994017711,-13.6057716700626,-320.843364288875)) ;
#39001 = CARTESIAN_POINT('Ctrl Pts',(12.6419935569205,-13.5968579596751,-320.843199528471)) ;
#39002 = CARTESIAN_POINT('Ctrl Pts',(12.6470700797698,-13.5921361774447,-320.843112338354)) ;
#39003 = CARTESIAN_POINT('Ctrl Pts',(12.7559151491712,-13.490783283132,-320.84124265685)) ;
#39004 = CARTESIAN_POINT('Ctrl Pts',(12.8585760876792,-13.3929692737651,-320.839474299984)) ;
#39005 = CARTESIAN_POINT('Ctrl Pts',(13.2094835596114,-13.0508749413233,-320.83339507716)) ;
#39006 = CARTESIAN_POINT('Ctrl Pts',(13.4519708152967,-12.8007919462534,-320.829131610642)) ;
#39007 = CARTESIAN_POINT('Ctrl Pts',(14.0834582008665,-12.1117517965977,-320.817684179353)) ;
#39008 = CARTESIAN_POINT('Ctrl Pts',(14.458934082965,-11.6609412289553,-320.810494308593)) ;
#39009 = CARTESIAN_POINT('Ctrl Pts',(14.9232976235467,-11.0464245610801,-320.800820895901)) ;
#39010 = CARTESIAN_POINT('Ctrl Pts',(15.0319644135627,-10.8980894317352,-320.798496179525)) ;
#39011 = CARTESIAN_POINT('Ctrl Pts',(15.1951310177363,-10.668275045164,-320.794905878076)) ;
#39012 = CARTESIAN_POINT('Ctrl Pts',(15.2512189090527,-10.5879375162876,-320.793652903881)) ;
#39013 = CARTESIAN_POINT('Ctrl Pts',(15.3618082707327,-10.4268326418247,-320.79114394585)) ;
#39014 = CARTESIAN_POINT('Ctrl Pts',(15.4163151233284,-10.3460726984133,-320.789888056903)) ;
#39015 = CARTESIAN_POINT('Ctrl Pts',(15.5581665798855,-10.1322887586249,-320.786567982216)) ;
#39016 = CARTESIAN_POINT('Ctrl Pts',(15.644440906834,-9.99856446808686,-320.784495683405)) ;
#39017 = CARTESIAN_POINT('Ctrl Pts',(15.8252165767743,-9.7102949448736,-320.780038208964)) ;
#39018 = CARTESIAN_POINT('Ctrl Pts',(15.9191969056721,-9.55544228986516,-320.777649594224)) ;
#39019 = CARTESIAN_POINT('Ctrl Pts',(16.1863093086688,-9.10043643957008,-320.770652604501)) ;
#39020 = CARTESIAN_POINT('Ctrl Pts',(16.3533231653468,-8.79678197746626,-320.766008732895)) ;
#39021 = CARTESIAN_POINT('Ctrl Pts',(16.7839538411502,-7.95913678783804,-320.753336220576)) ;
#39022 = CARTESIAN_POINT('Ctrl Pts',(17.0305388138956,-7.41685331340842,-320.74527165753)) ;
#39023 = CARTESIAN_POINT('Ctrl Pts',(17.2933933793987,-6.75621327027029,-320.735911031052)) ;
#39024 = CARTESIAN_POINT('Ctrl Pts',(17.3351401608174,-6.64836731805396,-320.734397777836)) ;
#39025 = CARTESIAN_POINT('Ctrl Pts',(17.3978682413441,-6.48171099600536,-320.732085870426)) ;
#39026 = CARTESIAN_POINT('Ctrl Pts',(17.4195649763844,-6.42317311181392,-320.731278825554)) ;
#39027 = CARTESIAN_POINT('Ctrl Pts',(17.4616779413934,-6.30776927918751,-320.729698439182)) ;
#39028 = CARTESIAN_POINT('Ctrl Pts',(17.482112654417,-6.25091089004718,-320.728924868416)) ;
#39029 = CARTESIAN_POINT('Ctrl Pts',(17.526419773313,-6.1257121612018,-320.727231666812)) ;
#39030 = CARTESIAN_POINT('Ctrl Pts',(17.5501707797211,-6.05732987140556,-320.726313476044)) ;
#39031 = CARTESIAN_POINT('Ctrl Pts',(17.6617734445469,-5.72984383007534,-320.721944267278)) ;
#39032 = CARTESIAN_POINT('Ctrl Pts',(17.7442907779709,-5.46895757131407,-320.718546811316)) ;
#39033 = CARTESIAN_POINT('Ctrl Pts',(17.8244844903586,-5.19445909918696,-320.715020738442)) ;
#39034 = CARTESIAN_POINT('Ctrl Pts',(17.827944405358,-5.1825718479975,-320.714868136358)) ;
#39035 = CARTESIAN_POINT('Ctrl Pts',(17.9629053570108,-4.71715121498048,-320.708896945127)) ;
#39036 = CARTESIAN_POINT('Ctrl Pts',(18.0770676090544,-4.25876881699607,-320.703145854989)) ;
#39037 = CARTESIAN_POINT('Ctrl Pts',(18.2577648608132,-3.39378896399032,-320.692274171537)) ;
#39038 = CARTESIAN_POINT('Ctrl Pts',(18.3284883741086,-2.98835975916959,-320.687171453859)) ;
#39039 = CARTESIAN_POINT('Ctrl Pts',(18.4078610802873,-2.4229322985058,-320.679971512952)) ;
#39040 = CARTESIAN_POINT('Ctrl Pts',(18.428001193603,-2.2646682716537,-320.677947632587)) ;
#39041 = CARTESIAN_POINT('Ctrl Pts',(18.4596253998129,-1.98769881711682,-320.674387965691)) ;
#39042 = CARTESIAN_POINT('Ctrl Pts',(18.4720101908752,-1.8691056556958,-320.6728581244)) ;
#39043 = CARTESIAN_POINT('Ctrl Pts',(18.4942285503858,-1.63449232577273,-320.669819773694)) ;
#39044 = CARTESIAN_POINT('Ctrl Pts',(18.5041148287334,-1.51848253198411,-320.668311678593)) ;
#39045 = CARTESIAN_POINT('Ctrl Pts',(18.5258613915667,-1.23140628741382,-320.664565458404)) ;
#39046 = CARTESIAN_POINT('Ctrl Pts',(18.5364441843054,-1.06025403462769,-320.662319402394)) ;
#39047 = CARTESIAN_POINT('Ctrl Pts',(18.544654593745,-0.888979977948724,-320.660059887232)) ;
#39048 = CARTESIAN_POINT('Ctrl Pts',(18.5446545929199,-0.888979995160609,
-320.363441000746)) ;
#39049 = CARTESIAN_POINT('Ctrl Pts',(18.5193716592953,-1.41639711783526,-320.370544484615)) ;
#39050 = CARTESIAN_POINT('Ctrl Pts',(18.4715976939239,-1.94255064943188,-320.377691476469)) ;
#39051 = CARTESIAN_POINT('Ctrl Pts',(18.3801584619138,-2.62487471795141,-320.386818421463)) ;
#39052 = CARTESIAN_POINT('Ctrl Pts',(18.356811497647,-2.78346262004066,-320.388929041152)) ;
#39053 = CARTESIAN_POINT('Ctrl Pts',(18.3191274118357,-3.01829142334129,-320.392028994592)) ;
#39054 = CARTESIAN_POINT('Ctrl Pts',(18.3063614400486,-3.09477674403978,-320.393034654064)) ;
#39055 = CARTESIAN_POINT('Ctrl Pts',(18.2816380081548,-3.23739515041758,-320.394900897312)) ;
#39056 = CARTESIAN_POINT('Ctrl Pts',(18.2697999343643,-3.30354748251078,-320.395762773958)) ;
#39057 = CARTESIAN_POINT('Ctrl Pts',(18.2387500911096,-3.47178406006102,-320.397946263074)) ;
#39058 = CARTESIAN_POINT('Ctrl Pts',(18.2190402623446,-3.57377411313504,-320.399262172644)) ;
#39059 = CARTESIAN_POINT('Ctrl Pts',(18.1043956400099,-4.14139873480308,-320.40655445357)) ;
#39060 = CARTESIAN_POINT('Ctrl Pts',(17.9924661075652,-4.60342166354413,-320.412376491316)) ;
#39061 = CARTESIAN_POINT('Ctrl Pts',(17.693740389311,-5.65785678600442,-320.425800636004)) ;
#39062 = CARTESIAN_POINT('Ctrl Pts',(17.4947030179841,-6.24621145109414,-320.43340081197)) ;
#39063 = CARTESIAN_POINT('Ctrl Pts',(17.1997330863639,-6.99262145291462,-320.44348371235)) ;
#39064 = CARTESIAN_POINT('Ctrl Pts',(17.1304126483206,-7.16076360291563,-320.445783670312)) ;
#39065 = CARTESIAN_POINT('Ctrl Pts',(17.008987049837,-7.44343204386877,-320.449703363068)) ;
#39066 = CARTESIAN_POINT('Ctrl Pts',(16.9581676935921,-7.55849650900434,-320.45131403318)) ;
#39067 = CARTESIAN_POINT('Ctrl Pts',(16.850931186642,-7.79477327342072,-320.454653692936)) ;
#39068 = CARTESIAN_POINT('Ctrl Pts',(16.7943660971786,-7.9159105332999,-320.456383662993)) ;
#39069 = CARTESIAN_POINT('Ctrl Pts',(16.6408801684696,-8.2355572061199,-320.460996291646)) ;
#39070 = CARTESIAN_POINT('Ctrl Pts',(16.5417165587628,-8.4329655693732,-320.463894525112)) ;
#39071 = CARTESIAN_POINT('Ctrl Pts',(16.3687656032414,-8.76247027133729,-320.468813228458)) ;
#39072 = CARTESIAN_POINT('Ctrl Pts',(16.2968434236332,-8.89551948922025,-320.470822041759)) ;
#39073 = CARTESIAN_POINT('Ctrl Pts',(15.9698111304275,-9.48321723483742,-320.479790516225)) ;
#39074 = CARTESIAN_POINT('Ctrl Pts',(15.6972440931399,-9.92788007665474,-320.48683958191)) ;
#39075 = CARTESIAN_POINT('Ctrl Pts',(15.2098622808899,-10.6526306193253,-320.498579551596)) ;
#39076 = CARTESIAN_POINT('Ctrl Pts',(15.0051259613828,-10.9391336708383,-320.503288649293)) ;
#39077 = CARTESIAN_POINT('Ctrl Pts',(14.7316748338556,-11.2996611733321,-320.509226608935)) ;
#39078 = CARTESIAN_POINT('Ctrl Pts',(14.6703339610787,-11.3791865946703,-320.510537086004)) ;
#39079 = CARTESIAN_POINT('Ctrl Pts',(14.5671782146053,-11.5107023611944,-320.512702690796)) ;
#39080 = CARTESIAN_POINT('Ctrl Pts',(14.525722984345,-11.5629720143339,-320.513562897238)) ;
#39081 = CARTESIAN_POINT('Ctrl Pts',(14.4344574769705,-11.6767805753733,-320.515434113947)) ;
#39082 = CARTESIAN_POINT('Ctrl Pts',(14.3845335694874,-11.7382264959883,-320.516443497067)) ;
#39083 = CARTESIAN_POINT('Ctrl Pts',(14.2261619267553,-11.9306212829844,-320.519604250803)) ;
#39084 = CARTESIAN_POINT('Ctrl Pts',(14.1163074260117,-12.0604009963385,-320.521736759783)) ;
#39085 = CARTESIAN_POINT('Ctrl Pts',(13.8328279435697,-12.3861171246223,-320.527113064288)) ;
#39086 = CARTESIAN_POINT('Ctrl Pts',(13.6568128341549,-12.5799240816472,-320.530335198743)) ;
#39087 = CARTESIAN_POINT('Ctrl Pts',(12.9529339046992,-13.3227625818285,-320.542890836321)) ;
#39088 = CARTESIAN_POINT('Ctrl Pts',(12.3955920297996,-13.8428247923646,-320.552166281128)) ;
#39089 = CARTESIAN_POINT('Ctrl Pts',(11.6815548918013,-14.431305411428,-320.563824446303)) ;
#39090 = CARTESIAN_POINT('Ctrl Pts',(11.5538493224394,-14.5337492166543,-320.565899823802)) ;
#39091 = CARTESIAN_POINT('Ctrl Pts',(11.326300204395,-14.7113915108615,-320.569584002307)) ;
#39092 = CARTESIAN_POINT('Ctrl Pts',(11.2270208256463,-14.7872958932533,-320.571186877826)) ;
#39093 = CARTESIAN_POINT('Ctrl Pts',(11.0149913247747,-14.9460375236911,-320.574601467596)) ;
#39094 = CARTESIAN_POINT('Ctrl Pts',(10.9020558649811,-15.0286143535752,-320.576415149722)) ;
#39095 = CARTESIAN_POINT('Ctrl Pts',(10.5790265694362,-15.2592513823096,-320.581588839354)) ;
#39096 = CARTESIAN_POINT('Ctrl Pts',(10.3667769346681,-15.4042361535363,-320.584972100217)) ;
#39097 = CARTESIAN_POINT('Ctrl Pts',(9.43889840845377,-16.0101917524411,-320.599677034769)) ;
#39098 = CARTESIAN_POINT('Ctrl Pts',(8.69505118729786,-16.4260499290374,-320.611300674135)) ;
#39099 = CARTESIAN_POINT('Ctrl Pts',(7.7759922587815,-16.8598845264129,-320.624782828388)) ;
#39100 = CARTESIAN_POINT('Ctrl Pts',(7.62574443468624,-16.928372155302,-320.626958165112)) ;
#39101 = CARTESIAN_POINT('Ctrl Pts',(7.40287525068303,-17.0263935551351,-320.630132612123)) ;
#39102 = CARTESIAN_POINT('Ctrl Pts',(7.33094851569702,-17.0574861381796,-320.631149147234)) ;
#39103 = CARTESIAN_POINT('Ctrl Pts',(7.19721557953243,-17.1142942664819,-320.633022981492)) ;
#39104 = CARTESIAN_POINT('Ctrl Pts',(7.13546313077644,-17.1401326201928,-320.633881722819)) ;
#39105 = CARTESIAN_POINT('Ctrl Pts',(6.97918969310046,-17.2045293849733,-320.636039550578)) ;
#39106 = CARTESIAN_POINT('Ctrl Pts',(6.88448785613743,-17.2426432757354,-320.637333227203)) ;
#39107 = CARTESIAN_POINT('Ctrl Pts',(6.67247750495302,-17.3259442842373,-320.640202929229)) ;
#39108 = CARTESIAN_POINT('Ctrl Pts',(6.55501459945844,-17.3707249433977,-320.64177494667)) ;
#39109 = CARTESIAN_POINT('Ctrl Pts',(6.1748866788987,-17.5112371877173,-320.646816330522)) ;
#39110 = CARTESIAN_POINT('Ctrl Pts',(5.91051128012946,-17.6022302605808,-320.65025287239)) ;
#39111 = CARTESIAN_POINT('Ctrl Pts',(4.95955635045958,-17.9056902199376,-320.662491724235)) ;
#39112 = CARTESIAN_POINT('Ctrl Pts',(4.26282267319932,-18.0842274927248,-320.671257947083)) ;
#39113 = CARTESIAN_POINT('Ctrl Pts',(3.40589453628108,-18.2515271164235,-320.68224657714)) ;
#39114 = CARTESIAN_POINT('Ctrl Pts',(3.25392575824277,-18.2792321157788,-320.684201841342)) ;
#39115 = CARTESIAN_POINT('Ctrl Pts',(2.97722309426901,-18.3261169715746,-320.687776652543)) ;
#39116 = CARTESIAN_POINT('Ctrl Pts',(2.85260552008239,-18.3459276762617,-320.689391998074)) ;
#39117 = CARTESIAN_POINT('Ctrl Pts',(2.59626449120315,-18.3840037065592,-320.692726807802)) ;
#39118 = CARTESIAN_POINT('Ctrl Pts',(2.4645272111221,-18.4021272453484,-320.694447101111)) ;
#39119 = CARTESIAN_POINT('Ctrl Pts',(2.11748773488935,-18.4460771838712,-320.698996389186)) ;
#39120 = CARTESIAN_POINT('Ctrl Pts',(1.90190831532076,-18.4695495961033,-320.701840171462)) ;
#39121 = CARTESIAN_POINT('Ctrl Pts',(1.41085733004987,-18.5143267764086,-320.708354362466)) ;
#39122 = CARTESIAN_POINT('Ctrl Pts',(1.1352218550829,-18.5332696874902,-320.712037187506)) ;
#39123 = CARTESIAN_POINT('Ctrl Pts',(0.446871419186728,-18.5651620111208,
-320.721274192816)) ;
#39124 = CARTESIAN_POINT('Ctrl Pts',(0.0339533922777227,-18.5705083738189,
-320.72685238069)) ;
#39125 = CARTESIAN_POINT('Ctrl Pts',(-0.725741605102334,-18.5550052139741,
-320.737063511099)) ;
#39126 = CARTESIAN_POINT('Ctrl Pts',(-1.07241920081694,-18.5381994078459,
-320.741702639691)) ;
#39127 = CARTESIAN_POINT('Ctrl Pts',(-1.51667508841897,-18.5041591654962,
-320.747546865568)) ;
#39128 = CARTESIAN_POINT('Ctrl Pts',(-1.61486677574162,-18.4958485905259,
-320.748832149939)) ;
#39129 = CARTESIAN_POINT('Ctrl Pts',(-1.77917719082368,-18.4806235443016,
-320.750969503372)) ;
#39130 = CARTESIAN_POINT('Ctrl Pts',(-1.84533326089137,-18.4741349798789,
-320.751826347344)) ;
#39131 = CARTESIAN_POINT('Ctrl Pts',(-1.9912071493842,-18.4590363321358,-320.75370691056)) ;
#39132 = CARTESIAN_POINT('Ctrl Pts',(-2.07090676697799,-18.4502648601334,
-320.754728822699)) ;
#39133 = CARTESIAN_POINT('Ctrl Pts',(-2.32567074987145,-18.4205548322995,
-320.757980905396)) ;
#39134 = CARTESIAN_POINT('Ctrl Pts',(-2.50049487729528,-18.3976387160583,
-320.760190663647)) ;
#39135 = CARTESIAN_POINT('Ctrl Pts',(-2.94936177529857,-18.3322844608753,
-320.765833919831)) ;
#39136 = CARTESIAN_POINT('Ctrl Pts',(-3.22282822417419,-18.2861906110619,
-320.769243085707)) ;
#39137 = CARTESIAN_POINT('Ctrl Pts',(-4.20503639547139,-18.097917250415,-320.781506029079)) ;
#39138 = CARTESIAN_POINT('Ctrl Pts',(-4.90636203821725,-17.9205064443765,
-320.790321308779)) ;
#39139 = CARTESIAN_POINT('Ctrl Pts',(-5.7426287535191,-17.6561747490109,-320.801360029236)) ;
#39140 = CARTESIAN_POINT('Ctrl Pts',(-5.88911900450835,-17.6078553216548,
-320.803312583352)) ;
#39141 = CARTESIAN_POINT('Ctrl Pts',(-6.15427188587219,-17.5167161913796,
-320.806884090276)) ;
#39142 = CARTESIAN_POINT('Ctrl Pts',(-6.27313278925437,-17.4745018106372,
-320.808498870328)) ;
#39143 = CARTESIAN_POINT('Ctrl Pts',(-6.51647758245965,-17.3852731758689,
-320.811834211267)) ;
#39144 = CARTESIAN_POINT('Ctrl Pts',(-6.64090482468461,-17.3381252310895,
-320.813555618956)) ;
#39145 = CARTESIAN_POINT('Ctrl Pts',(-6.9671803853991,-17.2104653661899,-320.818112196618)) ;
#39146 = CARTESIAN_POINT('Ctrl Pts',(-7.16814035790034,-17.1277401951755,
-320.820962243944)) ;
#39147 = CARTESIAN_POINT('Ctrl Pts',(-7.87722464414272,-16.8211798319423,
-320.831168527099)) ;
#39148 = CARTESIAN_POINT('Ctrl Pts',(-8.37670686978186,-16.5781041689362,
-320.838643890504)) ;
#39149 = CARTESIAN_POINT('Ctrl Pts',(-9.25674234508558,-16.0998901560729,
-320.852134786645)) ;
#39150 = CARTESIAN_POINT('Ctrl Pts',(-9.64112979901616,-15.8726922455904,
-320.858142212965)) ;
#39151 = CARTESIAN_POINT('Ctrl Pts',(-10.1142193174863,-15.5695347426882,
-320.865539419656)) ;
#39152 = CARTESIAN_POINT('Ctrl Pts',(-10.21090013687,-15.5063007504566,-320.867051066866)) ;
#39153 = CARTESIAN_POINT('Ctrl Pts',(-10.3588927164377,-15.4075220565231,
-320.869361114072)) ;
#39154 = CARTESIAN_POINT('Ctrl Pts',(-10.4106258646635,-15.3726140701835,
-320.870167884188)) ;
#39155 = CARTESIAN_POINT('Ctrl Pts',(-10.5207642992943,-15.2974849800264,
-320.871883001329)) ;
#39156 = CARTESIAN_POINT('Ctrl Pts',(-10.5791171598126,-15.2571887413449,
-320.872790182385)) ;
#39157 = CARTESIAN_POINT('Ctrl Pts',(-10.7392647230928,-15.1452365128485,
-320.875277696229)) ;
#39158 = CARTESIAN_POINT('Ctrl Pts',(-10.8405719181734,-15.0728894504592,
-320.876848790576)) ;
#39159 = CARTESIAN_POINT('Ctrl Pts',(-11.0746688883295,-14.9021315115285,
-320.880481969504)) ;
#39160 = CARTESIAN_POINT('Ctrl Pts',(-11.2068875054635,-14.8029553514131,
-320.882536128561)) ;
#39161 = CARTESIAN_POINT('Ctrl Pts',(-11.7147673121994,-14.4112936035401,
-320.890465622905)) ;
#39162 = CARTESIAN_POINT('Ctrl Pts',(-12.0804481929238,-14.1061663503894,
-320.896263772568)) ;
#39163 = CARTESIAN_POINT('Ctrl Pts',(-12.7691943815611,-13.4850255795518,
-320.907653703306)) ;
#39164 = CARTESIAN_POINT('Ctrl Pts',(-13.0932561961628,-13.1706067028363,
-320.913236594749)) ;
#39165 = CARTESIAN_POINT('Ctrl Pts',(-13.5094977649877,-12.7361905631823,
-320.920815162566)) ;
#39166 = CARTESIAN_POINT('Ctrl Pts',(-13.6121382787943,-12.6264314562078,
-320.922718684115)) ;
#39167 = CARTESIAN_POINT('Ctrl Pts',(-13.7987412060125,-12.4219666194397,
-320.926246732688)) ;
#39168 = CARTESIAN_POINT('Ctrl Pts',(-13.8830895089743,-12.3276250428531,
-320.927867763352)) ;
#39169 = CARTESIAN_POINT('Ctrl Pts',(-14.0554439670209,-12.1308380541493,
-320.931236037986)) ;
#39170 = CARTESIAN_POINT('Ctrl Pts',(-14.1433101269116,-12.0282798269091,
-320.932984350049)) ;
#39171 = CARTESIAN_POINT('Ctrl Pts',(-14.3768963867407,-11.7495370575697,
-320.937717499267)) ;
#39172 = CARTESIAN_POINT('Ctrl Pts',(-14.52049366311,-11.5716046537157,-320.940719451999)) ;
#39173 = CARTESIAN_POINT('Ctrl Pts',(-14.7584589546418,-11.2653335884569,
-320.945850502904)) ;
#39174 = CARTESIAN_POINT('Ctrl Pts',(-14.8545284322047,-11.1383498126716,
-320.947967639855)) ;
#39175 = CARTESIAN_POINT('Ctrl Pts',(-15.2925576635272,-10.5436185440467,
-320.957827933863)) ;
#39176 = CARTESIAN_POINT('Ctrl Pts',(-15.6141344513214,-10.0612630948273,
-320.965679462726)) ;
#39177 = CARTESIAN_POINT('Ctrl Pts',(-16.0593527340625,-9.32055815677543,
-320.977261871365)) ;
#39178 = CARTESIAN_POINT('Ctrl Pts',(-16.2004414701441,-9.07310924334838,
-320.981054400805)) ;
#39179 = CARTESIAN_POINT('Ctrl Pts',(-16.3763494467086,-8.74739767941218,
-320.985905016079)) ;
#39180 = CARTESIAN_POINT('Ctrl Pts',(-16.4163984030275,-8.67200385508084,
-320.98701810583)) ;
#39181 = CARTESIAN_POINT('Ctrl Pts',(-16.4869525235056,-8.53694243767363,
-320.988993042143)) ;
#39182 = CARTESIAN_POINT('Ctrl Pts',(-16.5176573349996,-8.47738083961355,
-320.989857372597)) ;
#39183 = CARTESIAN_POINT('Ctrl Pts',(-16.5834625710932,-8.34801610146167,
-320.991719628829)) ;
#39184 = CARTESIAN_POINT('Ctrl Pts',(-16.6184461286385,-8.27815510659376,
-320.992716116189)) ;
#39185 = CARTESIAN_POINT('Ctrl Pts',(-16.725382220958,-8.06119737157336,-320.995785338825)) ;
#39186 = CARTESIAN_POINT('Ctrl Pts',(-16.7958305233936,-7.91336784735064,
-320.997840706024)) ;
#39187 = CARTESIAN_POINT('Ctrl Pts',(-17.0755732533782,-7.30578294797287,
-321.006175883769)) ;
#39188 = CARTESIAN_POINT('Ctrl Pts',(-17.2680186484266,-6.83850865352852,
-321.012331461682)) ;
#39189 = CARTESIAN_POINT('Ctrl Pts',(-17.6209186493473,-5.87134667026382,
-321.024952902675)) ;
#39190 = CARTESIAN_POINT('Ctrl Pts',(-17.7797156257219,-5.37133097263386,
-321.031417134798)) ;
#39191 = CARTESIAN_POINT('Ctrl Pts',(-17.9564959858786,-4.72030862886497,
-321.039914773461)) ;
#39192 = CARTESIAN_POINT('Ctrl Pts',(-17.9940976357184,-4.57487834093764,
-321.041817545377)) ;
#39193 = CARTESIAN_POINT('Ctrl Pts',(-18.060115854795,-4.30612653321886,-321.045344690236)) ;
#39194 = CARTESIAN_POINT('Ctrl Pts',(-18.089044322004,-4.18293985991804,-321.046965574619)) ;
#39195 = CARTESIAN_POINT('Ctrl Pts',(-18.1462453946832,-3.92766120838814,
-321.050334071567)) ;
#39196 = CARTESIAN_POINT('Ctrl Pts',(-18.1743402529945,-3.79553695735537,
-321.052082757768)) ;
#39197 = CARTESIAN_POINT('Ctrl Pts',(-18.2461312995022,-3.43882768235407,
-321.056818374293)) ;
#39198 = CARTESIAN_POINT('Ctrl Pts',(-18.2871219915042,-3.21372248255536,
-321.059822452332)) ;
#39199 = CARTESIAN_POINT('Ctrl Pts',(-18.3495933365787,-2.83060573415165,
-321.064957886123)) ;
#39200 = CARTESIAN_POINT('Ctrl Pts',(-18.3732178716206,-2.67297014561105,
-321.067077274874)) ;
#39201 = CARTESIAN_POINT('Ctrl Pts',(-18.4734767312523,-1.93968747265878,
-321.076957468502)) ;
#39202 = CARTESIAN_POINT('Ctrl Pts',(-18.5251055740794,-1.36095235873069,
-321.08482709712)) ;
#39203 = CARTESIAN_POINT('Ctrl Pts',(-18.5614233639371,-0.498095116336742,
-321.096400656331)) ;
#39204 = CARTESIAN_POINT('Ctrl Pts',(-18.5668582310402,-0.215202318513333,
-321.100167539376)) ;
#39205 = CARTESIAN_POINT('Ctrl Pts',(-18.5655150223184,0.153131570288138,
-321.104994104965)) ;
#39206 = CARTESIAN_POINT('Ctrl Pts',(-18.5646138793491,0.238555778466489,
-321.10610797171)) ;
#39207 = CARTESIAN_POINT('Ctrl Pts',(-18.561953678839,0.390981958181049,-321.108083839441)) ;
#39208 = CARTESIAN_POINT('Ctrl Pts',(-18.5604213256749,0.457986375672511,
-321.108948331881)) ;
#39209 = CARTESIAN_POINT('Ctrl Pts',(-18.5563179967306,0.603042485896432,
-321.110810279628)) ;
#39210 = CARTESIAN_POINT('Ctrl Pts',(-18.5536173160079,0.68108909025185,-321.111806303374)) ;
#39211 = CARTESIAN_POINT('Ctrl Pts',(-18.5437380350147,0.922507739674279,
-321.114872279359)) ;
#39212 = CARTESIAN_POINT('Ctrl Pts',(-18.5348933346528,1.08580388235186,-321.116924915394)) ;
#39213 = CARTESIAN_POINT('Ctrl Pts',(-18.4899344429207,1.75260852954898,-321.125253207177)) ;
#39214 = CARTESIAN_POINT('Ctrl Pts',(-18.4354499703916,2.25466161129387,-321.131404653285)) ;
#39215 = CARTESIAN_POINT('Ctrl Pts',(-18.289190299241,3.22980268418589,-321.143492840528)) ;
#39216 = CARTESIAN_POINT('Ctrl Pts',(-18.1993277829494,3.70277925181585,-321.149421544324)) ;
#39217 = CARTESIAN_POINT('Ctrl Pts',(-18.0495192505376,4.35244163217773,-321.157792661133)) ;
#39218 = CARTESIAN_POINT('Ctrl Pts',(-18.005142355098,4.53252048579793,-321.16013692883)) ;
#39219 = CARTESIAN_POINT('Ctrl Pts',(-17.9260112406139,4.83410610606355,-321.164108105024)) ;
#39220 = CARTESIAN_POINT('Ctrl Pts',(-17.8927009317089,4.9559776188439,-321.165725341579)) ;
#39221 = CARTESIAN_POINT('Ctrl Pts',(-17.8218560745214,5.20514712284266,-321.169058476106)) ;
#39222 = CARTESIAN_POINT('Ctrl Pts',(-17.784195275679,5.33240178958517,-321.170775145127)) ;
#39223 = CARTESIAN_POINT('Ctrl Pts',(-17.6818601151187,5.66504051473134,-321.17530072952)) ;
#39224 = CARTESIAN_POINT('Ctrl Pts',(-17.6149715707018,5.86972209518751,-321.178124141604)) ;
#39225 = CARTESIAN_POINT('Ctrl Pts',(-17.4551068272755,6.33154717228465,-321.184579309028)) ;
#39226 = CARTESIAN_POINT('Ctrl Pts',(-17.3599799383985,6.58789344749354,-321.188223122735)) ;
#39227 = CARTESIAN_POINT('Ctrl Pts',(-17.1300351161867,7.16793492925832,-321.19658526272)) ;
#39228 = CARTESIAN_POINT('Ctrl Pts',(-16.991638893254,7.49010024141506,-321.201315486226)) ;
#39229 = CARTESIAN_POINT('Ctrl Pts',(-16.8044953428927,7.8938172541963,-321.207304951171)) ;
#39230 = CARTESIAN_POINT('Ctrl Pts',(-16.7641327838068,7.97917706199322,-321.208574806681)) ;
#39231 = CARTESIAN_POINT('Ctrl Pts',(-16.5832880139387,8.35420241637968,-321.214164954287)) ;
#39232 = CARTESIAN_POINT('Ctrl Pts',(-16.4359362982263,8.64049408939169,-321.218462686487)) ;
#39233 = CARTESIAN_POINT('Ctrl Pts',(-16.2341665074723,9.00865809886574,-321.223968555225)) ;
#39234 = CARTESIAN_POINT('Ctrl Pts',(-16.1864395314654,9.09413317855522,-321.225245240994)) ;
#39235 = CARTESIAN_POINT('Ctrl Pts',(-16.1052113535417,9.23694079198204,-321.227373021199)) ;
#39236 = CARTESIAN_POINT('Ctrl Pts',(-16.0720746156947,9.2944782273945,-321.228228787018)) ;
#39237 = CARTESIAN_POINT('Ctrl Pts',(-15.9980579159046,9.42141868450193,-321.230112881591)) ;
#39238 = CARTESIAN_POINT('Ctrl Pts',(-15.9570335957347,9.49073579644474,-321.231139338693)) ;
#39239 = CARTESIAN_POINT('Ctrl Pts',(-15.8235754521061,9.71292293630367,-321.23442517731)) ;
#39240 = CARTESIAN_POINT('Ctrl Pts',(-15.7293858203537,9.86472675585621,-321.236663557968)) ;
#39241 = CARTESIAN_POINT('Ctrl Pts',(-15.4802493805616,10.2536131745221,-321.242407769472)) ;
#39242 = CARTESIAN_POINT('Ctrl Pts',(-15.322042226032,10.4885521617144,-321.245888220912)) ;
#39243 = CARTESIAN_POINT('Ctrl Pts',(-14.7484061869017,11.2997138451177,-321.258068049271)) ;
#39244 = CARTESIAN_POINT('Ctrl Pts',(-14.3053465158289,11.8556348917969,-321.26673513444)) ;
#39245 = CARTESIAN_POINT('Ctrl Pts',(-13.7278278157521,12.5006163989102,-321.277629083777)) ;
#39246 = CARTESIAN_POINT('Ctrl Pts',(-13.6226752597952,12.6151252694939,-321.279596560882)) ;
#39247 = CARTESIAN_POINT('Ctrl Pts',(-13.4294434693726,12.8203168242976,-321.283186288704)) ;
#39248 = CARTESIAN_POINT('Ctrl Pts',(-13.34185249404,12.9114463692653,-321.284804208268)) ;
#39249 = CARTESIAN_POINT('Ctrl Pts',(-13.1604694361469,13.0963403218624,-321.288136774294)) ;
#39250 = CARTESIAN_POINT('Ctrl Pts',(-13.0665894825651,13.1900085230339,-321.289852171234)) ;
#39251 = CARTESIAN_POINT('Ctrl Pts',(-12.818050527327,13.432729153268,-321.294369436931)) ;
#39252 = CARTESIAN_POINT('Ctrl Pts',(-12.6617945910645,13.5801174261797,-321.297185700842)) ;
#39253 = CARTESIAN_POINT('Ctrl Pts',(-12.3016498752988,13.9082029503217,-321.303620212185)) ;
#39254 = CARTESIAN_POINT('Ctrl Pts',(-12.0962704588932,14.0871906191903,-321.30725039405)) ;
#39255 = CARTESIAN_POINT('Ctrl Pts',(-11.6167417330582,14.486877439103,-321.315615916459)) ;
#39256 = CARTESIAN_POINT('Ctrl Pts',(-11.3401061268932,14.7044312751157,-321.320363636395)) ;
#39257 = CARTESIAN_POINT('Ctrl Pts',(-10.9892289722789,14.9645768324444,-321.326242966776)) ;
#39258 = CARTESIAN_POINT('Ctrl Pts',(-10.9206553617482,15.0146927925513,-321.327385356424)) ;
#39259 = CARTESIAN_POINT('Ctrl Pts',(-10.5822525014676,15.2584645616812,-321.332987034861)) ;
#39260 = CARTESIAN_POINT('Ctrl Pts',(-10.3076035153886,15.4453267801448,-321.337423271941)) ;
#39261 = CARTESIAN_POINT('Ctrl Pts',(-9.94570660781616,15.6775955487692,-321.343062809468)) ;
#39262 = CARTESIAN_POINT('Ctrl Pts',(-9.86290627571715,15.7298176072214,-321.34433943979)) ;
#39263 = CARTESIAN_POINT('Ctrl Pts',(-9.72325870829841,15.8163569751191,-321.346467158386)) ;
#39264 = CARTESIAN_POINT('Ctrl Pts',(-9.66663345701099,15.8510285317965,-321.347322917376)) ;
#39265 = CARTESIAN_POINT('Ctrl Pts',(-9.54090415520071,15.9270881016373,-321.349207035323)) ;
#39266 = CARTESIAN_POINT('Ctrl Pts',(-9.47171442221973,15.9683315792215,-321.350233522206)) ;
#39267 = CARTESIAN_POINT('Ctrl Pts',(-9.24820577598284,16.0995996058698,-321.353519583147)) ;
#39268 = CARTESIAN_POINT('Ctrl Pts',(-9.09285493241683,16.1878475073278,-321.355758152445)) ;
#39269 = CARTESIAN_POINT('Ctrl Pts',(-8.6879795962993,16.4101717484031,-321.361503033109)) ;
#39270 = CARTESIAN_POINT('Ctrl Pts',(-8.43661703185502,16.540804688525,-321.364983958062)) ;
#39271 = CARTESIAN_POINT('Ctrl Pts',(-7.54486101314455,16.9786321230456,-321.37716303195)) ;
#39272 = CARTESIAN_POINT('Ctrl Pts',(-6.88992291155278,17.2547917500965,-321.385828929384)) ;
#39273 = CARTESIAN_POINT('Ctrl Pts',(-6.07429430837448,17.5448459679738,-321.396721775595)) ;
#39274 = CARTESIAN_POINT('Ctrl Pts',(-5.92715956189682,17.5950973518105,-321.398689430733)) ;
#39275 = CARTESIAN_POINT('Ctrl Pts',(-5.65929210221363,17.6828416573478,-321.402279376305)) ;
#39276 = CARTESIAN_POINT('Ctrl Pts',(-5.5387744512947,17.720960857171,-321.403897333695)) ;
#39277 = CARTESIAN_POINT('Ctrl Pts',(-5.29104113258263,17.7965437085786,-321.407229868785)) ;
#39278 = CARTESIAN_POINT('Ctrl Pts',(-5.16379438083837,17.8338810068994,-321.408945195831)) ;
#39279 = CARTESIAN_POINT('Ctrl Pts',(-4.82945525785488,17.9281058998016,-321.413462004474)) ;
#39280 = CARTESIAN_POINT('Ctrl Pts',(-4.62175697511332,17.9827690152042,-321.41627787565)) ;
#39281 = CARTESIAN_POINT('Ctrl Pts',(-4.14862213822516,18.0985525240186,-321.422711252947)) ;
#39282 = CARTESIAN_POINT('Ctrl Pts',(-3.88269480506963,18.1574598927173,-321.426340686715)) ;
#39283 = CARTESIAN_POINT('Ctrl Pts',(-3.27037357511702,18.2790320529916,-321.434706385579)) ;
#39284 = CARTESIAN_POINT('Ctrl Pts',(-2.92329988653985,18.3377390523937,-321.43945505655)) ;
#39285 = CARTESIAN_POINT('Ctrl Pts',(-2.47944983952775,18.3998937950808,-321.445487636589)) ;
#39286 = CARTESIAN_POINT('Ctrl Pts',(-2.38402901419855,18.4125003420151,-321.446782085803)) ;
#39287 = CARTESIAN_POINT('Ctrl Pts',(-1.9694817469615,18.4639918020053,-321.452390556825)) ;
#39288 = CARTESIAN_POINT('Ctrl Pts',(-1.64947290386272,18.495326206806,-321.456682025195)) ;
#39289 = CARTESIAN_POINT('Ctrl Pts',(-1.23146410867236,18.5253210748946,-321.462177725154)) ;
#39290 = CARTESIAN_POINT('Ctrl Pts',(-1.13406269647112,18.5315387008074,-321.463450448728)) ;
#39291 = CARTESIAN_POINT('Ctrl Pts',(-0.97035751361738,18.5406933448562,-321.465573830478)) ;
#39292 = CARTESIAN_POINT('Ctrl Pts',(-0.904078920903511,18.5440433765597,
-321.466429112353)) ;
#39293 = CARTESIAN_POINT('Ctrl Pts',(-0.757146689066578,18.5506804151138,
-321.468314896735)) ;
#39294 = CARTESIAN_POINT('Ctrl Pts',(-0.67648685661603,18.5537969302624,-321.469343497276)) ;
#39295 = CARTESIAN_POINT('Ctrl Pts',(-0.416151820788321,18.5621557776636,
-321.472645376182)) ;
#39296 = CARTESIAN_POINT('Ctrl Pts',(-0.236419828834445,18.5653148456518,
-321.474897371089)) ;
#39297 = CARTESIAN_POINT('Ctrl Pts',(0.229379589953863,18.566736644263,-321.480690006208)) ;
#39298 = CARTESIAN_POINT('Ctrl Pts',(0.51541169693746,18.5609987827475,-321.484204757496)) ;
#39299 = CARTESIAN_POINT('Ctrl Pts',(1.50325343420382,18.5183296042975,-321.496325492573)) ;
#39300 = CARTESIAN_POINT('Ctrl Pts',(2.20302263230478,18.4481704515664,-321.504902048803)) ;
#39301 = CARTESIAN_POINT('Ctrl Pts',(3.06880127824176,18.3113944419386,-321.515928851407)) ;
#39302 = CARTESIAN_POINT('Ctrl Pts',(3.24008794888846,18.2818636262046,-321.518129473395)) ;
#39303 = CARTESIAN_POINT('Ctrl Pts',(3.53465837936602,18.2268080548199,-321.521950769586)) ;
#39304 = CARTESIAN_POINT('Ctrl Pts',(3.65814378877568,18.2024263683139,-321.523563865548)) ;
#39305 = CARTESIAN_POINT('Ctrl Pts',(3.91525216625968,18.1489393517034,-321.526946807155)) ;
#39306 = CARTESIAN_POINT('Ctrl Pts',(4.0488207947935,18.1196095217521,-321.528718050772)) ;
#39307 = CARTESIAN_POINT('Ctrl Pts',(4.41433246276992,18.0351048217017,-321.533603350425)) ;
#39308 = CARTESIAN_POINT('Ctrl Pts',(4.64555551121885,17.9769338507959,-321.536736549811)) ;
#39309 = CARTESIAN_POINT('Ctrl Pts',(5.18329146056139,17.8305827141844,-321.544117224469)) ;
#39310 = CARTESIAN_POINT('Ctrl Pts',(5.48878005674475,17.7389256492352,-321.548383041199)) ;
#39311 = CARTESIAN_POINT('Ctrl Pts',(6.18700467137919,17.5096697969373,-321.558259792365)) ;
#39312 = CARTESIAN_POINT('Ctrl Pts',(6.57778003876474,17.3666454107648,-321.563883117522)) ;
#39313 = CARTESIAN_POINT('Ctrl Pts',(7.1783313263465,17.1236621798088,-321.572560240795)) ;
#39314 = CARTESIAN_POINT('Ctrl Pts',(7.39159534272431,17.0326910873819,-321.57564802626)) ;
#39315 = CARTESIAN_POINT('Ctrl Pts',(7.70704648244808,16.8910898400069,-321.580198713579)) ;
#39316 = CARTESIAN_POINT('Ctrl Pts',(7.81056150998061,16.8434738229718,-321.581689251149)) ;
#39317 = CARTESIAN_POINT('Ctrl Pts',(7.96984644043119,16.7684199857695,-321.583974871216)) ;
#39318 = CARTESIAN_POINT('Ctrl Pts',(8.02592783070173,16.7416499656676,-321.584778055086)) ;
#39319 = CARTESIAN_POINT('Ctrl Pts',(8.1460699349838,16.6835586328574,-321.586494506742)) ;
#39320 = CARTESIAN_POINT('Ctrl Pts',(8.21008676528212,16.6521487912436,-321.587406537155)) ;
#39321 = CARTESIAN_POINT('Ctrl Pts',(8.38714961336141,16.5640037044952,-321.589923971845)) ;
#39322 = CARTESIAN_POINT('Ctrl Pts',(8.49979930678429,16.5064808237003,-321.591519774152)) ;
#39323 = CARTESIAN_POINT('Ctrl Pts',(8.76158902219487,16.3694112537705,-321.595223619239)) ;
#39324 = CARTESIAN_POINT('Ctrl Pts',(8.91024814132779,16.2889700465853,-321.597323308824)) ;
#39325 = CARTESIAN_POINT('Ctrl Pts',(9.49496724126799,15.9621716341102,-321.605601170565)) ;
#39326 = CARTESIAN_POINT('Ctrl Pts',(9.9220808266281,15.7002432949059,-321.611696171592)) ;
#39327 = CARTESIAN_POINT('Ctrl Pts',(10.6425686314715,15.2172471239336,-321.622359435912)) ;
#39328 = CARTESIAN_POINT('Ctrl Pts',(10.940943343888,15.0041539286127,-321.626895188228)) ;
#39329 = CARTESIAN_POINT('Ctrl Pts',(11.3838681358433,14.6675846174657,-321.633875264549)) ;
#39330 = CARTESIAN_POINT('Ctrl Pts',(11.5331545986901,14.5504926748882,-321.63627205675)) ;
#39331 = CARTESIAN_POINT('Ctrl Pts',(11.7793503444038,14.3512208042749,-321.640304590439)) ;
#39332 = CARTESIAN_POINT('Ctrl Pts',(11.8772578456402,14.2702970930319,-321.641929927098)) ;
#39333 = CARTESIAN_POINT('Ctrl Pts',(12.0749565108811,14.1034486366182,-321.645257421477)) ;
#39334 = CARTESIAN_POINT('Ctrl Pts',(12.1746794456967,14.0174540669482,-321.64696011822)) ;
#39335 = CARTESIAN_POINT('Ctrl Pts',(12.4306400744634,13.7919382128315,-321.65139430076)) ;
#39336 = CARTESIAN_POINT('Ctrl Pts',(12.5854463507763,13.6508209366875,-321.65413918112)) ;
#39337 = CARTESIAN_POINT('Ctrl Pts',(12.8395504368079,13.4111890772959,-321.658749183073)) ;
#39338 = CARTESIAN_POINT('Ctrl Pts',(12.940182484306,13.3141175111215,-321.660603172423)) ;
#39339 = CARTESIAN_POINT('Ctrl Pts',(13.360660962612,12.8992453488769,-321.668466314579)) ;
#39340 = CARTESIAN_POINT('Ctrl Pts',(13.6699708490437,12.5709859454001,-321.674544424176)) ;
#39341 = CARTESIAN_POINT('Ctrl Pts',(14.247254545063,11.9118075164964,-321.686345206954)) ;
#39342 = CARTESIAN_POINT('Ctrl Pts',(14.516407656839,11.5822851858498,-321.69206437684)) ;
#39343 = CARTESIAN_POINT('Ctrl Pts',(14.8440660071315,11.1517526354932,-321.699187274537)) ;
#39344 = CARTESIAN_POINT('Ctrl Pts',(14.9132647878151,11.0590422686061,-321.700701112628)) ;
#39345 = CARTESIAN_POINT('Ctrl Pts',(15.0184697109015,10.9153087564481,-321.703013697433)) ;
#39346 = CARTESIAN_POINT('Ctrl Pts',(15.0550924459194,10.8647406394531,-321.703820842318)) ;
#39347 = CARTESIAN_POINT('Ctrl Pts',(15.1327412416412,10.7563778806971,-321.705535843599)) ;
#39348 = CARTESIAN_POINT('Ctrl Pts',(15.1736928621663,10.6985310925191,-321.706442541296)) ;
#39349 = CARTESIAN_POINT('Ctrl Pts',(15.2855419383057,10.538603027454,-321.708927064982)) ;
#39350 = CARTESIAN_POINT('Ctrl Pts',(15.3557472153486,10.4360420491688,-321.710495688647)) ;
#39351 = CARTESIAN_POINT('Ctrl Pts',(15.5166920065175,10.195781518194,-321.714121827195)) ;
#39352 = CARTESIAN_POINT('Ctrl Pts',(15.606637338683,10.0575624627969,-321.716171458557)) ;
#39353 = CARTESIAN_POINT('Ctrl Pts',(15.947789220838,9.51771589421415,-321.724067305245)) ;
#39354 = CARTESIAN_POINT('Ctrl Pts',(16.1854305052835,9.10772953941646,-321.729836908404)) ;
#39355 = CARTESIAN_POINT('Ctrl Pts',(16.619558332862,8.28799113082099,-321.741227460931)) ;
#39356 = CARTESIAN_POINT('Ctrl Pts',(16.8172038827703,7.87922384643061,-321.74684060395)) ;
#39357 = CARTESIAN_POINT('Ctrl Pts',(17.0601641895699,7.32584067329485,-321.754453178995)) ;
#39358 = CARTESIAN_POINT('Ctrl Pts',(17.1189807615024,7.18732504816598,-321.756359315207)) ;
#39359 = CARTESIAN_POINT('Ctrl Pts',(17.2241639269202,6.93099571682241,-321.759890517585)) ;
#39360 = CARTESIAN_POINT('Ctrl Pts',(17.2710218928518,6.81339323178998,-321.761512060175)) ;
#39361 = CARTESIAN_POINT('Ctrl Pts',(17.3653397988709,6.56945087033152,-321.764879568934)) ;
#39362 = CARTESIAN_POINT('Ctrl Pts',(17.4126323144763,6.4430541580304,-321.766626583935)) ;
#39363 = CARTESIAN_POINT('Ctrl Pts',(17.536135750312,6.10167707020369,-321.771351182546)) ;
#39364 = CARTESIAN_POINT('Ctrl Pts',(17.6097700097935,5.88578966891215,-321.774345770545)) ;
#39365 = CARTESIAN_POINT('Ctrl Pts',(17.7278471320026,5.51752708258251,-321.779461643665)) ;
#39366 = CARTESIAN_POINT('Ctrl Pts',(17.7743478961441,5.36583878138583,-321.781570987735)) ;
#39367 = CARTESIAN_POINT('Ctrl Pts',(17.980342379388,4.66179289272225,-321.791362889235)) ;
#39368 = CARTESIAN_POINT('Ctrl Pts',(18.1160691307113,4.10281149643404,-321.799152294138)) ;
#39369 = CARTESIAN_POINT('Ctrl Pts',(18.2810278126606,3.25314908045536,-321.810755460361)) ;
#39370 = CARTESIAN_POINT('Ctrl Pts',(18.329709487072,2.96659865032559,-321.814626626024)) ;
#39371 = CARTESIAN_POINT('Ctrl Pts',(18.3839772162613,2.59445281438515,-321.819554738078)) ;
#39372 = CARTESIAN_POINT('Ctrl Pts',(18.3957255439917,2.50979788652768,-321.820669101697)) ;
#39373 = CARTESIAN_POINT('Ctrl Pts',(18.4156441742154,2.35861016756145,-321.822645565276)) ;
#39374 = CARTESIAN_POINT('Ctrl Pts',(18.4240394792799,2.29210854448195,-321.823510161527)) ;
#39375 = CARTESIAN_POINT('Ctrl Pts',(18.4414328394865,2.14805701475749,-321.825371913067)) ;
#39376 = CARTESIAN_POINT('Ctrl Pts',(18.4503022430775,2.07049300244084,-321.826367641172)) ;
#39377 = CARTESIAN_POINT('Ctrl Pts',(18.4762201475247,1.83043264255559,-321.82943154835)) ;
#39378 = CARTESIAN_POINT('Ctrl Pts',(18.4916130632767,1.66776529323097,-321.831482444235)) ;
#39379 = CARTESIAN_POINT('Ctrl Pts',(18.5457559521328,1.00200950645863,-321.839806348449)) ;
#39380 = CARTESIAN_POINT('Ctrl Pts',(18.5661369063153,0.497643941982251,-321.845955161873)) ;
#39381 = CARTESIAN_POINT('Ctrl Pts',(18.5658389860298,-0.30109714749415,-321.855747028671)) ;
#39382 = CARTESIAN_POINT('Ctrl Pts',(18.558737673329,-0.595198509947113,-321.859362734055)) ;
#39383 = CARTESIAN_POINT('Ctrl Pts',(18.5446545931659,-0.888979990027978,
-321.863010318849)) ;
#39384 = CARTESIAN_POINT('Origin',(0.,0.,-315.477129595899)) ;
#39385 = CARTESIAN_POINT('',(18.5446550725491,-0.888969989752756,-323.660107772569)) ;
#39386 = CARTESIAN_POINT('',(18.5446545937424,-0.888979978001647,-323.364389984898)) ;
#39387 = CARTESIAN_POINT('',(18.544654593745,-0.888979977948782,-315.477129595899)) ;
#39388 = CARTESIAN_POINT('Ctrl Pts',(18.5446545937669,-0.88897997749115,-323.660107898464)) ;
#39389 = CARTESIAN_POINT('Ctrl Pts',(18.5503237782399,-0.770717395047024,
-323.658617203796)) ;
#39390 = CARTESIAN_POINT('Ctrl Pts',(18.5548612046501,-0.652413378015465,
-323.65712004335)) ;
#39391 = CARTESIAN_POINT('Ctrl Pts',(18.561366413947,-0.426362988663961,-323.654246572906)) ;
#39392 = CARTESIAN_POINT('Ctrl Pts',(18.5635281938753,-0.318636961806443,
-323.652871671419)) ;
#39393 = CARTESIAN_POINT('Ctrl Pts',(18.5661081922414,-0.091527361846506,
-323.649960657052)) ;
#39394 = CARTESIAN_POINT('Ctrl Pts',(18.566312902283,0.0278537801060046,-323.648423229591)) ;
#39395 = CARTESIAN_POINT('Ctrl Pts',(18.5640988187805,0.307047520700836,-323.644810180929)) ;
#39396 = CARTESIAN_POINT('Ctrl Pts',(18.5607677730369,0.466843337428206,-323.642728813943)) ;
#39397 = CARTESIAN_POINT('Ctrl Pts',(18.5412689196309,1.04428087719617,-323.635159590194)) ;
#39398 = CARTESIAN_POINT('Ctrl Pts',(18.5130633804492,1.46138917679022,-323.629598320572)) ;
#39399 = CARTESIAN_POINT('Ctrl Pts',(18.422992305004,2.34765365123846,-323.617647715205)) ;
#39400 = CARTESIAN_POINT('Ctrl Pts',(18.357221770728,2.81611993049503,-323.611249064971)) ;
#39401 = CARTESIAN_POINT('Ctrl Pts',(18.2715782248556,3.29303270247428,-323.604758360695)) ;
#39402 = CARTESIAN_POINT('Ctrl Pts',(18.2695076501888,3.30450078322009,-323.60460229901)) ;
#39403 = CARTESIAN_POINT('Ctrl Pts',(18.2197144195942,3.57880815554623,-323.600869883175)) ;
#39404 = CARTESIAN_POINT('Ctrl Pts',(18.1663351722883,3.84058957172962,-323.597317434124)) ;
#39405 = CARTESIAN_POINT('Ctrl Pts',(18.0913798123934,4.17153293123352,-323.592873557643)) ;
#39406 = CARTESIAN_POINT('Ctrl Pts',(18.0750233309047,4.24184418810534,-323.591932178512)) ;
#39407 = CARTESIAN_POINT('Ctrl Pts',(18.0441972742068,4.37093911678392,-323.590209957139)) ;
#39408 = CARTESIAN_POINT('Ctrl Pts',(18.0298494527621,4.42975086872242,-323.589427739595)) ;
#39409 = CARTESIAN_POINT('Ctrl Pts',(18.0000796385871,4.54923635417858,-323.587844139034)) ;
#39410 = CARTESIAN_POINT('Ctrl Pts',(17.9846378925075,4.60990436874624,-323.58704300336)) ;
#39411 = CARTESIAN_POINT('Ctrl Pts',(17.9395429453599,4.78339913642182,-323.584758949733)) ;
#39412 = CARTESIAN_POINT('Ctrl Pts',(17.909132764943,4.89602614968282,-323.583284690565)) ;
#39413 = CARTESIAN_POINT('Ctrl Pts',(17.7172790410817,5.58086046772953,-323.57435363134)) ;
#39414 = CARTESIAN_POINT('Ctrl Pts',(17.5294870144372,6.14532911905883,-323.567122913388)) ;
#39415 = CARTESIAN_POINT('Ctrl Pts',(17.1901185608794,7.02238975020227,-323.555591254465)) ;
#39416 = CARTESIAN_POINT('Ctrl Pts',(17.0563116952428,7.34141436204539,-323.551334665066)) ;
#39417 = CARTESIAN_POINT('Ctrl Pts',(16.8390438163416,7.82137136039368,-323.544775161069)) ;
#39418 = CARTESIAN_POINT('Ctrl Pts',(16.7620097359234,7.98512843289862,-323.542509092296)) ;
#39419 = CARTESIAN_POINT('Ctrl Pts',(16.6127772081841,8.290684064121,-323.538220959871)) ;
#39420 = CARTESIAN_POINT('Ctrl Pts',(16.541125858467,8.43273170762426,-323.536202706452)) ;
#39421 = CARTESIAN_POINT('Ctrl Pts',(16.4221170690771,8.66131024987194,-323.532912066623)) ;
#39422 = CARTESIAN_POINT('Ctrl Pts',(16.3758801693497,8.7484154524514,-323.531647856911)) ;
#39423 = CARTESIAN_POINT('Ctrl Pts',(16.2798652188715,8.92586844555025,-323.529050918605)) ;
#39424 = CARTESIAN_POINT('Ctrl Pts',(16.2300237703544,9.01617809475384,-323.527717756314)) ;
#39425 = CARTESIAN_POINT('Ctrl Pts',(16.0895683212822,9.26573581046243,-323.524001354571)) ;
#39426 = CARTESIAN_POINT('Ctrl Pts',(15.9973457769208,9.42406477107794,-323.521606448748)) ;
#39427 = CARTESIAN_POINT('Ctrl Pts',(15.6224760716144,10.0462831714071,-323.512049008671)) ;
#39428 = CARTESIAN_POINT('Ctrl Pts',(15.3218733435263,10.4990360548116,-323.504760435583)) ;
#39429 = CARTESIAN_POINT('Ctrl Pts',(14.781351998349,11.2403833148442,-323.492403407264)) ;
#39430 = CARTESIAN_POINT('Ctrl Pts',(14.5517543468974,11.5360751423254,-323.487354655104)) ;
#39431 = CARTESIAN_POINT('Ctrl Pts',(14.2196282772862,11.9381044320937,-323.48040369684)) ;
#39432 = CARTESIAN_POINT('Ctrl Pts',(14.1245336638935,12.0504653290566,-323.478451423275)) ;
#39433 = CARTESIAN_POINT('Ctrl Pts',(14.0242961654838,12.1660860762444,-323.476437285097)) ;
#39434 = CARTESIAN_POINT('Ctrl Pts',(14.0204773592986,12.1704867597478,-323.47636061636)) ;
#39435 = CARTESIAN_POINT('Ctrl Pts',(14.0138723901079,12.1780909037963,-323.476228123801)) ;
#39436 = CARTESIAN_POINT('Ctrl Pts',(14.0110871988395,12.181295207566,-323.476172288845)) ;
#39437 = CARTESIAN_POINT('Ctrl Pts',(14.0062743418172,12.186828463538,-323.476075865169)) ;
#39438 = CARTESIAN_POINT('Ctrl Pts',(14.0042471937814,12.1891578656366,-323.476035270451)) ;
#39439 = CARTESIAN_POINT('Ctrl Pts',(14.0007462905928,12.1931787382118,-323.475965194816)) ;
#39440 = CARTESIAN_POINT('Ctrl Pts',(13.9992728101978,12.1948704470848,-323.475935710701)) ;
#39441 = CARTESIAN_POINT('Ctrl Pts',(13.9936473911845,12.2013266505203,-323.475823184108)) ;
#39442 = CARTESIAN_POINT('Ctrl Pts',(13.9894933263703,12.2060892923554,-323.47574016663)) ;
#39443 = CARTESIAN_POINT('Ctrl Pts',(13.9816334202048,12.2150914041549,-323.475583236027)) ;
#39444 = CARTESIAN_POINT('Ctrl Pts',(13.9779280804049,12.2193313109958,-323.475509316927)) ;
#39445 = CARTESIAN_POINT('Ctrl Pts',(13.9709152486981,12.2273485156703,-323.475369532489)) ;
#39446 = CARTESIAN_POINT('Ctrl Pts',(13.9676081523547,12.2311261587905,-323.47530366237)) ;
#39447 = CARTESIAN_POINT('Ctrl Pts',(13.9613468872955,12.2382724503911,-323.475179044985)) ;
#39448 = CARTESIAN_POINT('Ctrl Pts',(13.9583930307397,12.2416413718422,-323.475120293897)) ;
#39449 = CARTESIAN_POINT('Ctrl Pts',(13.9527983324012,12.2480175585899,-323.475009092014)) ;
#39450 = CARTESIAN_POINT('Ctrl Pts',(13.9501577371959,12.2510250398708,-323.474956638165)) ;
#39451 = CARTESIAN_POINT('Ctrl Pts',(13.9451541953384,12.2567200619548,-323.474857305444)) ;
#39452 = CARTESIAN_POINT('Ctrl Pts',(13.9427914437388,12.2594077738402,-323.474810424133)) ;
#39453 = CARTESIAN_POINT('Ctrl Pts',(13.9383123154742,12.2644999677681,-323.474721597863)) ;
#39454 = CARTESIAN_POINT('Ctrl Pts',(13.9361960933454,12.2669045855467,-323.474679650954)) ;
#39455 = CARTESIAN_POINT('Ctrl Pts',(13.932182408608,12.2714628701886,-323.474600131711)) ;
#39456 = CARTESIAN_POINT('Ctrl Pts',(13.9302850686952,12.2736166449027,-323.474562557818)) ;
#39457 = CARTESIAN_POINT('Ctrl Pts',(13.9266847846417,12.2777016147674,-323.474491290651)) ;
#39458 = CARTESIAN_POINT('Ctrl Pts',(13.9249819380804,12.2796328958226,-323.474457596128)) ;
#39459 = CARTESIAN_POINT('Ctrl Pts',(13.9217491544514,12.2832978157025,-323.474393653399)) ;
#39460 = CARTESIAN_POINT('Ctrl Pts',(13.9202192951733,12.285031523077,-323.474363404191)) ;
#39461 = CARTESIAN_POINT('Ctrl Pts',(13.9173135374517,12.2883232226044,-323.474305970111)) ;
#39462 = CARTESIAN_POINT('Ctrl Pts',(13.9159377011823,12.2898812695546,-323.474278784434)) ;
#39463 = CARTESIAN_POINT('Ctrl Pts',(13.9133232730959,12.2928409409497,-323.47422714125)) ;
#39464 = CARTESIAN_POINT('Ctrl Pts',(13.9120847310595,12.2942426093266,-323.474202683095)) ;
#39465 = CARTESIAN_POINT('Ctrl Pts',(13.909730135176,12.2969065137494,-323.47415619885)) ;
#39466 = CARTESIAN_POINT('Ctrl Pts',(13.908614121282,12.2981687850912,-323.474134172236)) ;
#39467 = CARTESIAN_POINT('Ctrl Pts',(13.9064915446121,12.3005688742403,-323.474092289978)) ;
#39468 = CARTESIAN_POINT('Ctrl Pts',(13.9054850139649,12.3017067204797,-323.474072433909)) ;
#39469 = CARTESIAN_POINT('Ctrl Pts',(13.9035698736828,12.3038711814465,-323.474034662232)) ;
#39470 = CARTESIAN_POINT('Ctrl Pts',(13.9026612899867,12.3048978190765,-323.474016746282)) ;
#39471 = CARTESIAN_POINT('Ctrl Pts',(13.9009318343427,12.3068515499615,-323.473982651062)) ;
#39472 = CARTESIAN_POINT('Ctrl Pts',(13.9001109833619,12.3077786617267,-323.473966471517)) ;
#39473 = CARTESIAN_POINT('Ctrl Pts',(13.8985479419105,12.3095436861754,-323.473935668705)) ;
#39474 = CARTESIAN_POINT('Ctrl Pts',(13.8978057684013,12.3103816138752,-323.473921045214)) ;
#39475 = CARTESIAN_POINT('Ctrl Pts',(13.8540989812646,12.3597183995863,-323.473060011453)) ;
#39476 = CARTESIAN_POINT('Ctrl Pts',(13.8108808228006,12.4079921184024,-323.472216985576)) ;
#39477 = CARTESIAN_POINT('Ctrl Pts',(13.7360751665116,12.4906733167759,-323.470772915351)) ;
#39478 = CARTESIAN_POINT('Ctrl Pts',(13.704608901706,12.5251896490504,-323.470170018341)) ;
#39479 = CARTESIAN_POINT('Ctrl Pts',(13.6307253300317,12.6056231077138,-323.46876537125)) ;
#39480 = CARTESIAN_POINT('Ctrl Pts',(13.5882056947003,12.6514454892282,-323.467965357299)) ;
#39481 = CARTESIAN_POINT('Ctrl Pts',(13.466041493772,12.7817725683267,-323.465689159943)) ;
#39482 = CARTESIAN_POINT('Ctrl Pts',(13.3858343857396,12.8657460475946,-323.464221541928)) ;
#39483 = CARTESIAN_POINT('Ctrl Pts',(13.0244927551137,13.2370186190326,-323.457714876407)) ;
#39484 = CARTESIAN_POINT('Ctrl Pts',(12.7348591372855,13.5158957433074,-323.452776803151)) ;
#39485 = CARTESIAN_POINT('Ctrl Pts',(12.0905261872447,14.0971866565799,-323.442141515355)) ;
#39486 = CARTESIAN_POINT('Ctrl Pts',(11.7330294212639,14.3960937573776,-323.436450574123)) ;
#39487 = CARTESIAN_POINT('Ctrl Pts',(11.1289644631762,14.8636973247729,-323.426981665765)) ;
#39488 = CARTESIAN_POINT('Ctrl Pts',(10.8888987088302,15.0404532029573,-323.423255361437)) ;
#39489 = CARTESIAN_POINT('Ctrl Pts',(10.52479627491,15.2952467673429,-323.417632604116)) ;
#39490 = CARTESIAN_POINT('Ctrl Pts',(10.4039228921554,15.3777208544005,-323.415770722326)) ;
#39491 = CARTESIAN_POINT('Ctrl Pts',(10.1787687630971,15.527477679217,-323.412309258019)) ;
#39492 = CARTESIAN_POINT('Ctrl Pts',(10.074763943415,15.5951604045832,-323.410712915426)) ;
#39493 = CARTESIAN_POINT('Ctrl Pts',(9.83822275615837,15.7457393468884,-323.407087450815)) ;
#39494 = CARTESIAN_POINT('Ctrl Pts',(9.70530222750609,15.82801450442,-323.405053743867)) ;
#39495 = CARTESIAN_POINT('Ctrl Pts',(9.27689476108783,16.0857644782117,-323.398510654345)) ;
#39496 = CARTESIAN_POINT('Ctrl Pts',(8.9775694101289,16.2547175245648,-323.393955252391)) ;
#39497 = CARTESIAN_POINT('Ctrl Pts',(8.07239186473413,16.7330079504755,-323.380269995338)) ;
#39498 = CARTESIAN_POINT('Ctrl Pts',(7.45405168113789,17.0174667866865,-323.371022501614)) ;
#39499 = CARTESIAN_POINT('Ctrl Pts',(6.64783929924503,17.3359625597361,-323.359494607043)) ;
#39500 = CARTESIAN_POINT('Ctrl Pts',(6.47315036202161,17.4019450013065,-323.357028879074)) ;
#39501 = CARTESIAN_POINT('Ctrl Pts',(6.22056076950735,17.4930217983991,-323.353523718497)) ;
#39502 = CARTESIAN_POINT('Ctrl Pts',(6.14344330860009,17.5202537728642,-323.352461562311)) ;
#39503 = CARTESIAN_POINT('Ctrl Pts',(6.00360291696061,17.5685978633952,-323.350551584627)) ;
#39504 = CARTESIAN_POINT('Ctrl Pts',(5.94094243979778,17.5898857811635,-323.349701717918)) ;
#39505 = CARTESIAN_POINT('Ctrl Pts',(5.78724335727805,17.6411876684146,-323.347630981698)) ;
#39506 = CARTESIAN_POINT('Ctrl Pts',(5.69608356481473,17.6708324673515,-323.346414513763)) ;
#39507 = CARTESIAN_POINT('Ctrl Pts',(5.31273200211769,17.7922221699779,-323.341340690626)) ;
#39508 = CARTESIAN_POINT('Ctrl Pts',(5.0185222094316,17.877436245743,-323.337547327287)) ;
#39509 = CARTESIAN_POINT('Ctrl Pts',(4.6345425293482,17.9784247466082,-323.332661395469)) ;
#39510 = CARTESIAN_POINT('Ctrl Pts',(4.5465777818002,18.0008714041265,-323.331546523555)) ;
#39511 = CARTESIAN_POINT('Ctrl Pts',(3.97621646159951,18.1419674929887,-323.32433902006)) ;
#39512 = CARTESIAN_POINT('Ctrl Pts',(3.48938698789912,18.2418601110935,-323.318279418466)) ;
#39513 = CARTESIAN_POINT('Ctrl Pts',(2.69512740539551,18.3718721803915,-323.30831136477)) ;
#39514 = CARTESIAN_POINT('Ctrl Pts',(2.38992447485823,18.4140614628864,-323.304463191795)) ;
#39515 = CARTESIAN_POINT('Ctrl Pts',(1.93698773644386,18.4652216581462,-323.298698053594)) ;
#39516 = CARTESIAN_POINT('Ctrl Pts',(1.78996894540428,18.4800525829168,-323.296818509563)) ;
#39517 = CARTESIAN_POINT('Ctrl Pts',(1.51926957527869,18.5040994590875,-323.293340600501)) ;
#39518 = CARTESIAN_POINT('Ctrl Pts',(1.39564348538494,18.513834180013,-323.291745706158)) ;
#39519 = CARTESIAN_POINT('Ctrl Pts',(1.11775912275271,18.5329165125479,-323.288145293981)) ;
#39520 = CARTESIAN_POINT('Ctrl Pts',(0.963462987689927,18.5415781122223,-323.286135464969)) ;
#39521 = CARTESIAN_POINT('Ctrl Pts',(0.481379714385811,18.5626065716895,-323.279822824562)) ;
#39522 = CARTESIAN_POINT('Ctrl Pts',(0.153362038502939,18.5682139266589,-323.275478842516)) ;
#39523 = CARTESIAN_POINT('Ctrl Pts',(-0.23657036804274,18.564546067458,-323.27027123668)) ;
#39524 = CARTESIAN_POINT('Ctrl Pts',(-0.298506436942952,18.5636534694313,
-323.269442804479)) ;
#39525 = CARTESIAN_POINT('Ctrl Pts',(-0.512279398028653,18.559502527546,-323.266579577389)) ;
#39526 = CARTESIAN_POINT('Ctrl Pts',(-0.664079970053959,18.5546911050701,
-323.264539580786)) ;
#39527 = CARTESIAN_POINT('Ctrl Pts',(-1.24790198818545,18.5290126458142,-323.256677432499)) ;
#39528 = CARTESIAN_POINT('Ctrl Pts',(-1.67920354976889,18.4949140176799,-323.250831618158)) ;
#39529 = CARTESIAN_POINT('Ctrl Pts',(-2.26598784024006,18.427826551131,-323.242947929109)) ;
#39530 = CARTESIAN_POINT('Ctrl Pts',(-2.42282042162764,18.4078633633876,-323.240848056056)) ;
#39531 = CARTESIAN_POINT('Ctrl Pts',(-2.69880563117029,18.3691450808065,-323.23717564102)) ;
#39532 = CARTESIAN_POINT('Ctrl Pts',(-2.81806633368682,18.351227344344,-323.235596253059)) ;
#39533 = CARTESIAN_POINT('Ctrl Pts',(-3.00641745702622,18.3210500642899,-323.233118293633)) ;
#39534 = CARTESIAN_POINT('Ctrl Pts',(-3.07562743877243,18.3095586312135,-323.232211284222)) ;
#39535 = CARTESIAN_POINT('Ctrl Pts',(-3.21593039487008,18.285445151023,-323.230380915386)) ;
#39536 = CARTESIAN_POINT('Ctrl Pts',(-3.28701818942103,18.272800117011,-323.229457814163)) ;
#39537 = CARTESIAN_POINT('Ctrl Pts',(-3.48694629915977,18.2360326352666,-323.226871670499)) ;
#39538 = CARTESIAN_POINT('Ctrl Pts',(-3.61560762441776,18.2109599516676,-323.225219085501)) ;
#39539 = CARTESIAN_POINT('Ctrl Pts',(-4.13173325787617,18.1046953976303,-323.218619682922)) ;
#39540 = CARTESIAN_POINT('Ctrl Pts',(-4.51682215079011,18.0124827318817,-323.213761822793)) ;
#39541 = CARTESIAN_POINT('Ctrl Pts',(-5.33492586574961,17.7886937945559,-323.203370040131)) ;
#39542 = CARTESIAN_POINT('Ctrl Pts',(-5.76667659037494,17.653455800313,-323.197840623271)) ;
#39543 = CARTESIAN_POINT('Ctrl Pts',(-6.46969411556895,17.404702445927,-323.188593351146)) ;
#39544 = CARTESIAN_POINT('Ctrl Pts',(-6.7439717006612,17.3002732451864,-323.184923609616)) ;
#39545 = CARTESIAN_POINT('Ctrl Pts',(-7.1505012689632,17.1343527003912,-323.179367104328)) ;
#39546 = CARTESIAN_POINT('Ctrl Pts',(-7.28469189153641,17.077733304651,-323.177513626326)) ;
#39547 = CARTESIAN_POINT('Ctrl Pts',(-7.53199853149051,16.9699412855552,-323.17405982061)) ;
#39548 = CARTESIAN_POINT('Ctrl Pts',(-7.64529435365952,16.9192016155736,-323.172462622079)) ;
#39549 = CARTESIAN_POINT('Ctrl Pts',(-7.90090977777712,16.8016321431667,-323.168824345505)) ;
#39550 = CARTESIAN_POINT('Ctrl Pts',(-8.0429064189153,16.7341230491819,-323.166778544015)) ;
#39551 = CARTESIAN_POINT('Ctrl Pts',(-8.50892601176434,16.5052626206335,-323.159982705293)) ;
#39552 = CARTESIAN_POINT('Ctrl Pts',(-8.82908736682221,16.3362398129791,-323.155180387365)) ;
#39553 = CARTESIAN_POINT('Ctrl Pts',(-9.63713570586959,15.8789498201472,-323.142757609997)) ;
#39554 = CARTESIAN_POINT('Ctrl Pts',(-10.1171392499201,15.5775134037096,-323.135078592906)) ;
#39555 = CARTESIAN_POINT('Ctrl Pts',(-10.7287977375206,15.1531863211195,-323.125119544532)) ;
#39556 = CARTESIAN_POINT('Ctrl Pts',(-10.8735232091636,15.0496727451883,-323.122750605868)) ;
#39557 = CARTESIAN_POINT('Ctrl Pts',(-11.1223052625073,14.8662714180601,-323.118670260359)) ;
#39558 = CARTESIAN_POINT('Ctrl Pts',(-11.227044548546,14.7873314367539,-323.116949847738)) ;
#39559 = CARTESIAN_POINT('Ctrl Pts',(-11.3881467606397,14.6632134305196,-323.114305175881)) ;
#39560 = CARTESIAN_POINT('Ctrl Pts',(-11.4450972070057,14.6188051731731,-323.113370580112)) ;
#39561 = CARTESIAN_POINT('Ctrl Pts',(-11.5501401343129,14.5359057672667,-323.111648507283)) ;
#39562 = CARTESIAN_POINT('Ctrl Pts',(-11.5983029280691,14.497505398825,-323.110859657134)) ;
#39563 = CARTESIAN_POINT('Ctrl Pts',(-11.7324132664571,14.3894827014484,-323.108663840561)) ;
#39564 = CARTESIAN_POINT('Ctrl Pts',(-11.8179311487339,14.3193308813554,-323.107264496208)) ;
#39565 = CARTESIAN_POINT('Ctrl Pts',(-12.3201680291789,13.8997731928975,-323.099036020632)) ;
#39566 = CARTESIAN_POINT('Ctrl Pts',(-12.7220004765878,13.5329576500112,-323.092402328526)) ;
#39567 = CARTESIAN_POINT('Ctrl Pts',(-13.4380222292776,12.8192165239113,-323.080016702163)) ;
#39568 = CARTESIAN_POINT('Ctrl Pts',(-13.7563256812105,12.4770291562704,-323.074277882653)) ;
#39569 = CARTESIAN_POINT('Ctrl Pts',(-14.2032359513814,11.9586697063806,-323.065723070661)) ;
#39570 = CARTESIAN_POINT('Ctrl Pts',(-14.3421905196898,11.7916607606686,-323.062987450998)) ;
#39571 = CARTESIAN_POINT('Ctrl Pts',(-14.5614682099217,11.5185000776005,-323.058537357585)) ;
#39572 = CARTESIAN_POINT('Ctrl Pts',(-14.6436366290522,11.4138559076622,-323.056838216513)) ;
#39573 = CARTESIAN_POINT('Ctrl Pts',(-14.8015025965645,11.2082974226561,-323.053510081082)) ;
#39574 = CARTESIAN_POINT('Ctrl Pts',(-14.8773105066636,11.1074768631553,-323.051882114371)) ;
#39575 = CARTESIAN_POINT('Ctrl Pts',(-15.0435410107717,10.8816439456824,-323.048244747554)) ;
#39576 = CARTESIAN_POINT('Ctrl Pts',(-15.133444625169,10.7562611898794,-323.046231396909)) ;
#39577 = CARTESIAN_POINT('Ctrl Pts',(-15.6941398917748,9.9533487032572,-323.033378836211)) ;
#39578 = CARTESIAN_POINT('Ctrl Pts',(-16.1208901651071,9.24619186564224,-323.022191239364)) ;
#39579 = CARTESIAN_POINT('Ctrl Pts',(-16.5979220084065,8.32164958215965,-323.008230013588)) ;
#39580 = CARTESIAN_POINT('Ctrl Pts',(-16.6933207549158,8.12858592543286,-323.005352410259)) ;
#39581 = CARTESIAN_POINT('Ctrl Pts',(-16.8492590606531,7.79867562975424,-323.000521509604)) ;
#39582 = CARTESIAN_POINT('Ctrl Pts',(-16.9115419938052,7.66267707698794,-322.998554521327)) ;
#39583 = CARTESIAN_POINT('Ctrl Pts',(-17.0028452961706,7.45677383075563,-322.995620941627)) ;
#39584 = CARTESIAN_POINT('Ctrl Pts',(-17.0330927325559,7.38742012567348,-322.994640356556)) ;
#39585 = CARTESIAN_POINT('Ctrl Pts',(-17.0893851923168,7.25616448453195,-322.992800079662)) ;
#39586 = CARTESIAN_POINT('Ctrl Pts',(-17.1155198953955,7.19430246645539,-322.99193933814)) ;
#39587 = CARTESIAN_POINT('Ctrl Pts',(-17.1827226844417,7.03279153716999,-322.989707871236)) ;
#39588 = CARTESIAN_POINT('Ctrl Pts',(-17.2232597531966,6.93292428788047,-322.988343577622)) ;
#39589 = CARTESIAN_POINT('Ctrl Pts',(-17.3533077633921,6.60435639011049,-322.983897688224)) ;
#39590 = CARTESIAN_POINT('Ctrl Pts',(-17.4391508644068,6.37423181228684,-322.980850966978)) ;
#39591 = CARTESIAN_POINT('Ctrl Pts',(-17.7149511566361,5.58755626624956,-322.970574351714)) ;
#39592 = CARTESIAN_POINT('Ctrl Pts',(-17.8830256510212,5.02371123536483,-322.963430874508)) ;
#39593 = CARTESIAN_POINT('Ctrl Pts',(-18.0625065034053,4.2972149511946,-322.954179956868)) ;
#39594 = CARTESIAN_POINT('Ctrl Pts',(-18.0989369698454,4.14109623288026,-322.952190142788)) ;
#39595 = CARTESIAN_POINT('Ctrl Pts',(-18.1826296642394,3.76021570295067,-322.947323206578)) ;
#39596 = CARTESIAN_POINT('Ctrl Pts',(-18.2277519228483,3.53501106097198,-322.944434911236)) ;
#39597 = CARTESIAN_POINT('Ctrl Pts',(-18.2927862148409,3.17596572402927,-322.939803018233)) ;
#39598 = CARTESIAN_POINT('Ctrl Pts',(-18.3154333818866,3.04264453251384,-322.93807728118)) ;
#39599 = CARTESIAN_POINT('Ctrl Pts',(-18.3564380114294,2.78418332336711,-322.934719069227)) ;
#39600 = CARTESIAN_POINT('Ctrl Pts',(-18.3749772497311,2.65907958951756,-322.93308788694)) ;
#39601 = CARTESIAN_POINT('Ctrl Pts',(-18.4126910806977,2.38532368279199,-322.929505527675)) ;
#39602 = CARTESIAN_POINT('Ctrl Pts',(-18.4313467260544,2.23660896919226,-322.927551121723)) ;
#39603 = CARTESIAN_POINT('Ctrl Pts',(-18.500287393079,1.62740246474633,-322.919511810699)) ;
#39604 = CARTESIAN_POINT('Ctrl Pts',(-18.5351306587741,1.1653332872747,-322.913332425615)) ;
#39605 = CARTESIAN_POINT('Ctrl Pts',(-18.5703583953788,0.234917139341171,
-322.900819677559)) ;
#39606 = CARTESIAN_POINT('Ctrl Pts',(-18.5703811056925,-0.233114595382776,
-322.894490033861)) ;
#39607 = CARTESIAN_POINT('Ctrl Pts',(-18.5465365329178,-0.864505845623008,
-322.88604998023)) ;
#39608 = CARTESIAN_POINT('Ctrl Pts',(-18.5381777681597,-1.0282766550428,-322.883870318959)) ;
#39609 = CARTESIAN_POINT('Ctrl Pts',(-18.5197035274377,-1.31544829007845,
-322.880076103168)) ;
#39610 = CARTESIAN_POINT('Ctrl Pts',(-18.5105211479912,-1.43889883352907,
-322.878454086882)) ;
#39611 = CARTESIAN_POINT('Ctrl Pts',(-18.4941492317929,-1.63277463555328,
-322.875925741264)) ;
#39612 = CARTESIAN_POINT('Ctrl Pts',(-18.4877903702771,-1.70326629290526,
-322.875010412893)) ;
#39613 = CARTESIAN_POINT('Ctrl Pts',(-18.4750569326367,-1.8359405784202,-322.873296233084)) ;
#39614 = CARTESIAN_POINT('Ctrl Pts',(-18.4687711084613,-1.89813071910815,
-322.872496266676)) ;
#39615 = CARTESIAN_POINT('Ctrl Pts',(-18.4499130892744,-2.07573726788903,
-322.870220402999)) ;
#39616 = CARTESIAN_POINT('Ctrl Pts',(-18.4365721890096,-2.19106918870898,
-322.868753067158)) ;
#39617 = CARTESIAN_POINT('Ctrl Pts',(-18.374737777818,-2.68499382332531,-322.862501371871)) ;
#39618 = CARTESIAN_POINT('Ctrl Pts',(-18.3156574773483,-3.0621679804896,-322.857807316607)) ;
#39619 = CARTESIAN_POINT('Ctrl Pts',(-18.1795910609839,-3.78441068004417,
-322.848796861754)) ;
#39620 = CARTESIAN_POINT('Ctrl Pts',(-18.1042934974024,-4.12963100874972,
-322.844480332318)) ;
#39621 = CARTESIAN_POINT('Ctrl Pts',(-17.9538384404681,-4.73579834774724,
-322.836788968964)) ;
#39622 = CARTESIAN_POINT('Ctrl Pts',(-17.8827205571754,-4.99764003198292,
-322.833429320777)) ;
#39623 = CARTESIAN_POINT('Ctrl Pts',(-17.7452308294695,-5.46325562450603,
-322.827358585756)) ;
#39624 = CARTESIAN_POINT('Ctrl Pts',(-17.6810207713455,-5.66761708858894,
-322.824660409652)) ;
#39625 = CARTESIAN_POINT('Ctrl Pts',(-17.5713877923288,-5.99653142922168,
-322.820254874485)) ;
#39626 = CARTESIAN_POINT('Ctrl Pts',(-17.5281418345596,-6.12178910912928,
-322.81856225096)) ;
#39627 = CARTESIAN_POINT('Ctrl Pts',(-17.4410106586243,-6.36566091493105,
-322.815236289201)) ;
#39628 = CARTESIAN_POINT('Ctrl Pts',(-17.3972470106402,-6.48431091750484,
-322.813603861435)) ;
#39629 = CARTESIAN_POINT('Ctrl Pts',(-17.2968857228202,-6.74807395571698,
-322.809942500152)) ;
#39630 = CARTESIAN_POINT('Ctrl Pts',(-17.2396672871168,-6.89294055911324,
-322.807909427544)) ;
#39631 = CARTESIAN_POINT('Ctrl Pts',(-16.9121528580071,-7.69254966820199,
-322.796565913654)) ;
#39632 = CARTESIAN_POINT('Ctrl Pts',(-16.6063815128054,-8.33212576115319,
-322.787010772789)) ;
#39633 = CARTESIAN_POINT('Ctrl Pts',(-16.1278884455994,-9.20143202801274,
-322.773653471666)) ;
#39634 = CARTESIAN_POINT('Ctrl Pts',(-15.9852671611417,-9.44702975446794,
-322.769839652861)) ;
#39635 = CARTESIAN_POINT('Ctrl Pts',(-15.7436834039316,-9.84189776200365,
-322.763688798819)) ;
#39636 = CARTESIAN_POINT('Ctrl Pts',(-15.6480959823002,-9.99317822339049,
-322.761327755182)) ;
#39637 = CARTESIAN_POINT('Ctrl Pts',(-15.5063066145703,-10.2105558021007,
-322.757941155485)) ;
#39638 = CARTESIAN_POINT('Ctrl Pts',(-15.4618375611102,-10.2777708609849,
-322.756894854923)) ;
#39639 = CARTESIAN_POINT('Ctrl Pts',(-15.3799419298375,-10.3998217753429,
-322.754998129675)) ;
#39640 = CARTESIAN_POINT('Ctrl Pts',(-15.342656288674,-10.4547503425963,-322.754145865699)) ;
#39641 = CARTESIAN_POINT('Ctrl Pts',(-15.2497074597909,-10.590112820872,-322.752048129485)) ;
#39642 = CARTESIAN_POINT('Ctrl Pts',(-15.1937016983783,-10.6703090821572,
-322.750807374841)) ;
#39643 = CARTESIAN_POINT('Ctrl Pts',(-14.950509631956,-11.0127457171388,-322.745510465112)) ;
#39644 = CARTESIAN_POINT('Ctrl Pts',(-14.7571477027636,-11.2705323340075,
-322.741524831967)) ;
#39645 = CARTESIAN_POINT('Ctrl Pts',(-14.4986398936552,-11.5971046097757,
-322.736403772201)) ;
#39646 = CARTESIAN_POINT('Ctrl Pts',(-14.4395417058521,-11.6706053582831,
-322.735246400695)) ;
#39647 = CARTESIAN_POINT('Ctrl Pts',(-14.1581689266422,-12.0151411368643,
-322.729792597873)) ;
#39648 = CARTESIAN_POINT('Ctrl Pts',(-13.928807792406,-12.2802963054764,-322.725509615492)) ;
#39649 = CARTESIAN_POINT('Ctrl Pts',(-13.5074152727782,-12.7404471859981,
-322.71782712948)) ;
#39650 = CARTESIAN_POINT('Ctrl Pts',(-13.3183201648812,-12.9379909379211,
-322.714441781986)) ;
#39651 = CARTESIAN_POINT('Ctrl Pts',(-12.9726296547381,-13.2835141636971,
-322.708331044084)) ;
#39652 = CARTESIAN_POINT('Ctrl Pts',(-12.8176911047191,-13.4330809275679,
-322.705618850601)) ;
#39653 = CARTESIAN_POINT('Ctrl Pts',(-12.5631165312608,-13.6704138326154,
-322.701196637184)) ;
#39654 = CARTESIAN_POINT('Ctrl Pts',(-12.4650794708005,-13.7598657354793,
-322.699501575298)) ;
#39655 = CARTESIAN_POINT('Ctrl Pts',(-12.2718578745426,-13.9324069953263,
-322.696174842626)) ;
#39656 = CARTESIAN_POINT('Ctrl Pts',(-12.1767674930752,-14.0155910949952,
-322.694544126557)) ;
#39657 = CARTESIAN_POINT('Ctrl Pts',(-11.9400211334082,-14.2184663120646,
-322.690499434486)) ;
#39658 = CARTESIAN_POINT('Ctrl Pts',(-11.7974068554624,-14.3370178299206,
-322.688076111243)) ;
#39659 = CARTESIAN_POINT('Ctrl Pts',(-11.277849402391,-14.7559101875759,-322.679296820116)) ;
#39660 = CARTESIAN_POINT('Ctrl Pts',(-10.891022741352,-15.0436828575766,-322.67284642717)) ;
#39661 = CARTESIAN_POINT('Ctrl Pts',(-10.0772907658551,-15.6011916367726,
-322.659571683811)) ;
#39662 = CARTESIAN_POINT('Ctrl Pts',(-9.64969442359706,-15.8692270615061,
-322.652749277622)) ;
#39663 = CARTESIAN_POINT('Ctrl Pts',(-9.06992225666922,-16.200545689302,-322.643892842789)) ;
#39664 = CARTESIAN_POINT('Ctrl Pts',(-8.92706623668201,-16.2797008244498,
-322.641741675198)) ;
#39665 = CARTESIAN_POINT('Ctrl Pts',(-8.71441540396617,-16.3938877734179,
-322.638595014131)) ;
#39666 = CARTESIAN_POINT('Ctrl Pts',(-8.64541419574475,-16.430380566699,-322.637582509809)) ;
#39667 = CARTESIAN_POINT('Ctrl Pts',(-8.51673218363405,-16.4974017876336,
-322.635711542434)) ;
#39668 = CARTESIAN_POINT('Ctrl Pts',(-8.45711235293185,-16.528044151393,-322.634851692247)) ;
#39669 = CARTESIAN_POINT('Ctrl Pts',(-8.32108678272701,-16.5970274989947,
-322.632904755465)) ;
#39670 = CARTESIAN_POINT('Ctrl Pts',(-8.24457951267131,-16.6351650347717,
-322.631820210022)) ;
#39671 = CARTESIAN_POINT('Ctrl Pts',(-7.90652348865025,-16.8007750333337,
-322.627068774591)) ;
#39672 = CARTESIAN_POINT('Ctrl Pts',(-7.64226194797811,-16.9226176588425,
-322.623460784774)) ;
#39673 = CARTESIAN_POINT('Ctrl Pts',(-6.84790706050794,-17.2664663539402,
-322.612799978036)) ;
#39674 = CARTESIAN_POINT('Ctrl Pts',(-6.31025509066353,-17.4701280287219,
-322.605815410438)) ;
#39675 = CARTESIAN_POINT('Ctrl Pts',(-5.61325079542622,-17.6977702760099,
-322.59674904727)) ;
#39676 = CARTESIAN_POINT('Ctrl Pts',(-5.46185156870605,-17.7450791659003,
-322.594779802315)) ;
#39677 = CARTESIAN_POINT('Ctrl Pts',(-5.09134551910705,-17.8556630983488,
-322.589953251791)) ;
#39678 = CARTESIAN_POINT('Ctrl Pts',(-4.87164339100633,-17.9168522423779,
-322.587084813705)) ;
#39679 = CARTESIAN_POINT('Ctrl Pts',(-4.52022852702689,-18.0077828577757,
-322.582476567261)) ;
#39680 = CARTESIAN_POINT('Ctrl Pts',(-4.38922227563307,-18.0401617825421,
-322.580754282145)) ;
#39681 = CARTESIAN_POINT('Ctrl Pts',(-4.13465534802278,-18.1001422781457,
-322.577397806033)) ;
#39682 = CARTESIAN_POINT('Ctrl Pts',(-4.01114228166471,-18.1279139141295,
-322.575764850827)) ;
#39683 = CARTESIAN_POINT('Ctrl Pts',(-3.74019654077387,-18.1859307642103,
-322.572172505606)) ;
#39684 = CARTESIAN_POINT('Ctrl Pts',(-3.59266058338345,-18.2156509015746,
-322.570209808915)) ;
#39685 = CARTESIAN_POINT('Ctrl Pts',(-2.99860315955674,-18.3278217403999,
-322.562281487074)) ;
#39686 = CARTESIAN_POINT('Ctrl Pts',(-2.5494873876402,-18.3956729327063,-322.556225851467)) ;
#39687 = CARTESIAN_POINT('Ctrl Pts',(-1.62782497544954,-18.5005116782299,
-322.54376235784)) ;
#39688 = CARTESIAN_POINT('Ctrl Pts',(-1.15543668915085,-18.5360112306732,
-322.537354945567)) ;
#39689 = CARTESIAN_POINT('Ctrl Pts',(-0.517445199277493,-18.5594701918291,
-322.528826093164)) ;
#39690 = CARTESIAN_POINT('Ctrl Pts',(-0.352607441716422,-18.5633335219827,
-322.526634240782)) ;
#39691 = CARTESIAN_POINT('Ctrl Pts',(-0.0634749710545198,-18.5662573963225,
-322.52282147745)) ;
#39692 = CARTESIAN_POINT('Ctrl Pts',(0.0607997067637385,-18.5662663519132,
-322.521193008782)) ;
#39693 = CARTESIAN_POINT('Ctrl Pts',(0.255933559320724,-18.5643211628228,
-322.518657028985)) ;
#39694 = CARTESIAN_POINT('Ctrl Pts',(0.326797348675451,-18.5632089288624,
-322.517740433064)) ;
#39695 = CARTESIAN_POINT('Ctrl Pts',(0.460077060916918,-18.5603536345706,
-322.516025840187)) ;
#39696 = CARTESIAN_POINT('Ctrl Pts',(0.522493931622624,-18.5587014105402,
-322.51522671048)) ;
#39697 = CARTESIAN_POINT('Ctrl Pts',(0.700540219090692,-18.5530894581941,
-322.512956728868)) ;
#39698 = CARTESIAN_POINT('Ctrl Pts',(0.816142665487155,-18.5483637082764,
-322.511494368653)) ;
#39699 = CARTESIAN_POINT('Ctrl Pts',(1.35586959976043,-18.5212444683981,-322.504706749635)) ;
#39700 = CARTESIAN_POINT('Ctrl Pts',(1.77919062630473,-18.485382375016,-322.499495346281)) ;
#39701 = CARTESIAN_POINT('Ctrl Pts',(2.64901054851744,-18.3815369150559,-322.488762686957)) ;
#39702 = CARTESIAN_POINT('Ctrl Pts',(3.0950123364984,-18.311719049829,-322.48324521533)) ;
#39703 = CARTESIAN_POINT('Ctrl Pts',(3.67534929554771,-18.1990624868313,-322.475914298686)) ;
#39704 = CARTESIAN_POINT('Ctrl Pts',(3.81236726688987,-18.1708536842034,-322.474172645317)) ;
#39705 = CARTESIAN_POINT('Ctrl Pts',(4.15378995607066,-18.096530934177,-322.469800717777)) ;
#39706 = CARTESIAN_POINT('Ctrl Pts',(4.35775721340732,-18.048500067951,-322.467159927168)) ;
#39707 = CARTESIAN_POINT('Ctrl Pts',(4.68852165900283,-17.9646766240867,-322.462822627848)) ;
#39708 = CARTESIAN_POINT('Ctrl Pts',(4.81582792062362,-17.9309688230722,-322.461139956664)) ;
#39709 = CARTESIAN_POINT('Ctrl Pts',(5.06519033783497,-17.8620961153777,-322.457816565212)) ;
#39710 = CARTESIAN_POINT('Ctrl Pts',(5.18726569797387,-17.8270273830884,-322.456176569192)) ;
#39711 = CARTESIAN_POINT('Ctrl Pts',(5.49071339324919,-17.7364747706402,-322.452066869102)) ;
#39712 = CARTESIAN_POINT('Ctrl Pts',(5.67161332129041,-17.6794590701848,-322.449587109017)) ;
#39713 = CARTESIAN_POINT('Ctrl Pts',(6.18912607636877,-17.5075898146768,-322.442409259899)) ;
#39714 = CARTESIAN_POINT('Ctrl Pts',(6.52335327089297,-17.3858230712936,-322.437669281679)) ;
#39715 = CARTESIAN_POINT('Ctrl Pts',(6.9370540463038,-17.2214921202381,-322.43169682807)) ;
#39716 = CARTESIAN_POINT('Ctrl Pts',(7.01999232395873,-17.1878508677771,-322.43049418813)) ;
#39717 = CARTESIAN_POINT('Ctrl Pts',(7.31943397746948,-17.0638630126255,-322.426134916864)) ;
#39718 = CARTESIAN_POINT('Ctrl Pts',(7.53446333261199,-16.9700146411905,-322.422971442112)) ;
#39719 = CARTESIAN_POINT('Ctrl Pts',(8.00025692286102,-16.7561227692663,-322.416073031352)) ;
#39720 = CARTESIAN_POINT('Ctrl Pts',(8.25022111472117,-16.6344706244798,-322.412341268799)) ;
#39721 = CARTESIAN_POINT('Ctrl Pts',(8.65435654787149,-16.4264357503732,-322.40630324816)) ;
#39722 = CARTESIAN_POINT('Ctrl Pts',(8.81019271936543,-16.3433834671654,-322.403973959314)) ;
#39723 = CARTESIAN_POINT('Ctrl Pts',(9.03507064487054,-16.2193844955481,-322.400623469226)) ;
#39724 = CARTESIAN_POINT('Ctrl Pts',(9.10506896646183,-16.1801932655979,-322.399582108493)) ;
#39725 = CARTESIAN_POINT('Ctrl Pts',(9.23259260294843,-16.107704700335,-322.39768937313)) ;
#39726 = CARTESIAN_POINT('Ctrl Pts',(9.29019716498837,-16.0745498697289,-322.396836224092)) ;
#39727 = CARTESIAN_POINT('Ctrl Pts',(9.43269765328075,-15.9915105579538,-322.394729422307)) ;
#39728 = CARTESIAN_POINT('Ctrl Pts',(9.5173771388148,-15.9412586511136,-322.393480592396)) ;
#39729 = CARTESIAN_POINT('Ctrl Pts',(9.89713389017053,-15.7117926001061,-322.387885796956)) ;
#39730 = CARTESIAN_POINT('Ctrl Pts',(10.1875781451274,-15.5250423060953,-322.383621388743)) ;
#39731 = CARTESIAN_POINT('Ctrl Pts',(11.0421017665899,-14.9412883994295,-322.370908913289)) ;
#39732 = CARTESIAN_POINT('Ctrl Pts',(11.5894384998584,-14.5208480011863,-322.362523112885)) ;
#39733 = CARTESIAN_POINT('Ctrl Pts',(12.2770699293531,-13.9289420137174,-322.351182996688)) ;
#39734 = CARTESIAN_POINT('Ctrl Pts',(12.4395159273802,-13.7840601755729,-322.348442314322)) ;
#39735 = CARTESIAN_POINT('Ctrl Pts',(12.6971494448055,-13.5460184459629,-322.343986194695)) ;
#39736 = CARTESIAN_POINT('Ctrl Pts',(12.7939475983153,-13.454632085342,-322.342286171533)) ;
#39737 = CARTESIAN_POINT('Ctrl Pts',(12.9805081825982,-13.2746678700117,-322.338957714887)) ;
#39738 = CARTESIAN_POINT('Ctrl Pts',(13.0703675598689,-13.1862007998507,-322.337330324653)) ;
#39739 = CARTESIAN_POINT('Ctrl Pts',(13.2680140228534,-12.9876112384417,-322.333696084767)) ;
#39740 = CARTESIAN_POINT('Ctrl Pts',(13.3753454511505,-12.877048410202,-322.331685309123)) ;
#39741 = CARTESIAN_POINT('Ctrl Pts',(13.9804509658335,-12.237996478676,-322.320135484392)) ;
#39742 = CARTESIAN_POINT('Ctrl Pts',(14.4482616813532,-11.6820072176031,-322.310336528142)) ;
#39743 = CARTESIAN_POINT('Ctrl Pts',(15.0470480272017,-10.8791896765663,-322.296858039948)) ;
#39744 = CARTESIAN_POINT('Ctrl Pts',(15.2068491544979,-10.6546779138979,-322.293159307168)) ;
#39745 = CARTESIAN_POINT('Ctrl Pts',(15.4602200753268,-10.2813878061923,-322.287166850157)) ;
#39746 = CARTESIAN_POINT('Ctrl Pts',(15.5567794773916,-10.1346905466541,-322.284850485168)) ;
#39747 = CARTESIAN_POINT('Ctrl Pts',(15.6943128293501,-9.91914589985208,-322.281514710889)) ;
#39748 = CARTESIAN_POINT('Ctrl Pts',(15.7369453722879,-9.85136848064576,-322.280475378158)) ;
#39749 = CARTESIAN_POINT('Ctrl Pts',(15.8141788118294,-9.72680162147317,-322.27858426035)) ;
#39750 = CARTESIAN_POINT('Ctrl Pts',(15.8489155049886,-9.67009816832151,-322.27773072761)) ;
#39751 = CARTESIAN_POINT('Ctrl Pts',(15.9344727764156,-9.52873686196501,-322.275620107367)) ;
#39752 = CARTESIAN_POINT('Ctrl Pts',(15.9849240681972,-9.44385786752175,-322.27436788692)) ;
#39753 = CARTESIAN_POINT('Ctrl Pts',(16.2026784757274,-9.07076434642673,-322.268921122029)) ;
#39754 = CARTESIAN_POINT('Ctrl Pts',(16.3628817658125,-8.77847691501777,-322.264801991637)) ;
#39755 = CARTESIAN_POINT('Ctrl Pts',(16.7605906175474,-8.00410929579952,-322.254104012751)) ;
#39756 = CARTESIAN_POINT('Ctrl Pts',(16.985188154469,-7.51575327708908,-322.247562732555)) ;
#39757 = CARTESIAN_POINT('Ctrl Pts',(17.272892710054,-6.81115001590324,-322.238145272996)) ;
#39758 = CARTESIAN_POINT('Ctrl Pts',(17.3537417272353,-6.6024415909807,-322.235359421902)) ;
#39759 = CARTESIAN_POINT('Ctrl Pts',(17.4953337785239,-6.21634369698405,-322.230197547204)) ;
#39760 = CARTESIAN_POINT('Ctrl Pts',(17.557201095437,-6.03939752916188,-322.227828831957)) ;
#39761 = CARTESIAN_POINT('Ctrl Pts',(17.6567655862335,-5.74016487002462,-322.223812955855)) ;
#39762 = CARTESIAN_POINT('Ctrl Pts',(17.6958971599025,-5.61837052473176,-322.22217564164)) ;
#39763 = CARTESIAN_POINT('Ctrl Pts',(17.7683176808687,-5.38470127482329,-322.219028114743)) ;
#39764 = CARTESIAN_POINT('Ctrl Pts',(17.8018164992113,-5.27289771504453,-322.21751941301)) ;
#39765 = CARTESIAN_POINT('Ctrl Pts',(17.8892105903719,-4.9708877310793,-322.213436400646)) ;
#39766 = CARTESIAN_POINT('Ctrl Pts',(17.9411257008595,-4.78012434667114,-322.210849175349)) ;
#39767 = CARTESIAN_POINT('Ctrl Pts',(18.0725872114106,-4.26471513382368,-322.203839597565)) ;
#39768 = CARTESIAN_POINT('Ctrl Pts',(18.1464298710929,-3.93869088019811,-322.199384311686)) ;
#39769 = CARTESIAN_POINT('Ctrl Pts',(18.311241752124,-3.10745762984853,-322.188016484232)) ;
#39770 = CARTESIAN_POINT('Ctrl Pts',(18.3901367340055,-2.60014185461628,-322.181066576659)) ;
#39771 = CARTESIAN_POINT('Ctrl Pts',(18.4756607474731,-1.8453188249167,-322.170911456651)) ;
#39772 = CARTESIAN_POINT('Ctrl Pts',(18.4985288482755,-1.59989765106995,-322.167639679005)) ;
#39773 = CARTESIAN_POINT('Ctrl Pts',(18.5230267638305,-1.26490183827105,-322.163244458239)) ;
#39774 = CARTESIAN_POINT('Ctrl Pts',(18.528904765265,-1.17566380638093,-322.162080494127)) ;
#39775 = CARTESIAN_POINT('Ctrl Pts',(18.5379858226082,-1.02073778824992,-322.160073677379)) ;
#39776 = CARTESIAN_POINT('Ctrl Pts',(18.5414850279525,-0.955069081350536,
-322.159227513438)) ;
#39777 = CARTESIAN_POINT('Ctrl Pts',(18.5446417153482,-0.889248593493978,
-322.158383873619)) ;
#39778 = CARTESIAN_POINT('Ctrl Pts',(18.5446481553962,-0.889114285759121,
-322.158382152315)) ;
#39779 = CARTESIAN_POINT('Ctrl Pts',(18.5446545937451,-0.888979977946956,
-322.15838043089)) ;
#39780 = CARTESIAN_POINT('',(0.000274526296954267,-18.5659499979704,-322.226379248718)) ;
#39781 = CARTESIAN_POINT('Ctrl Pts',(18.5446545931659,-0.888979990027976,
-321.863010318849)) ;
#39782 = CARTESIAN_POINT('Ctrl Pts',(18.535675921736,-1.07628044925217,-321.865335837486)) ;
#39783 = CARTESIAN_POINT('Ctrl Pts',(18.5238593692262,-1.26345088814058,-321.867674125245)) ;
#39784 = CARTESIAN_POINT('Ctrl Pts',(18.4947201691002,-1.63530246681083,-321.87235735625)) ;
#39785 = CARTESIAN_POINT('Ctrl Pts',(18.4774638015849,-1.8199504380384,-321.874701456261)) ;
#39786 = CARTESIAN_POINT('Ctrl Pts',(18.4438053970694,-2.12990675361984,-321.878672437106)) ;
#39787 = CARTESIAN_POINT('Ctrl Pts',(18.4288849724849,-2.25536225954101,-321.880289648314)) ;
#39788 = CARTESIAN_POINT('Ctrl Pts',(18.39566820886,-2.51227040600905,-321.883622804306)) ;
#39789 = CARTESIAN_POINT('Ctrl Pts',(18.3772404824554,-2.64369885407315,-321.885339520908)) ;
#39790 = CARTESIAN_POINT('Ctrl Pts',(18.325220281141,-2.9878372447093,-321.889865416447)) ;
#39791 = CARTESIAN_POINT('Ctrl Pts',(18.2893334714954,-3.20017978694584,-321.892689095903)) ;
#39792 = CARTESIAN_POINT('Ctrl Pts',(18.1995127783954,-3.68062481398582,-321.89914503651)) ;
#39793 = CARTESIAN_POINT('Ctrl Pts',(18.1433330176666,-3.94825670301182,-321.902789360683)) ;
#39794 = CARTESIAN_POINT('Ctrl Pts',(18.0016947012494,-4.55591348932771,-321.911151368143)) ;
#39795 = CARTESIAN_POINT('Ctrl Pts',(17.9124752699819,-4.89495548653125,-321.915880930624)) ;
#39796 = CARTESIAN_POINT('Ctrl Pts',(17.7871422360078,-5.32174430435427,-321.921868077427)) ;
#39797 = CARTESIAN_POINT('Ctrl Pts',(17.7598834962691,-5.41201714443049,-321.923136279583)) ;
#39798 = CARTESIAN_POINT('Ctrl Pts',(17.6364420973623,-5.80984049331601,-321.928728902645)) ;
#39799 = CARTESIAN_POINT('Ctrl Pts',(17.5329495202847,-6.11506486258897,-321.93303072531)) ;
#39800 = CARTESIAN_POINT('Ctrl Pts',(17.38776086875,-6.50921162407933,-321.938539205523)) ;
#39801 = CARTESIAN_POINT('Ctrl Pts',(17.3532314681898,-6.60071372259848,-321.939814602295)) ;
#39802 = CARTESIAN_POINT('Ctrl Pts',(17.2940525325771,-6.75386211403319,-321.941940950671)) ;
#39803 = CARTESIAN_POINT('Ctrl Pts',(17.2697924373257,-6.81565665666956,-321.942796558143)) ;
#39804 = CARTESIAN_POINT('Ctrl Pts',(17.2153441378235,-6.95218831295049,-321.94468119804)) ;
#39805 = CARTESIAN_POINT('Ctrl Pts',(17.1849996716115,-7.02686149238606,-321.945708348992)) ;
#39806 = CARTESIAN_POINT('Ctrl Pts',(17.0857039699265,-7.26672278496012,-321.948999371421)) ;
#39807 = CARTESIAN_POINT('Ctrl Pts',(17.0148497014702,-7.43111230012272,-321.951242150917)) ;
#39808 = CARTESIAN_POINT('Ctrl Pts',(16.825408565896,-7.85371575208497,-321.957001979528)) ;
#39809 = CARTESIAN_POINT('Ctrl Pts',(16.7032515628816,-8.11027818030459,-321.960493485417)) ;
#39810 = CARTESIAN_POINT('Ctrl Pts',(16.2563345702195,-8.9959572317637,-321.972655198958)) ;
#39811 = CARTESIAN_POINT('Ctrl Pts',(15.9015262046198,-9.60922078533316,-321.981294049578)) ;
#39812 = CARTESIAN_POINT('Ctrl Pts',(15.4269603602362,-10.3309085297965,-321.992161902245)) ;
#39813 = CARTESIAN_POINT('Ctrl Pts',(15.339716525285,-10.4600130897495,-321.994133737819)) ;
#39814 = CARTESIAN_POINT('Ctrl Pts',(15.1787308685438,-10.6918952641756,-321.997728798913)) ;
#39815 = CARTESIAN_POINT('Ctrl Pts',(15.1055440825231,-10.7950466899102,-321.999347646884)) ;
#39816 = CARTESIAN_POINT('Ctrl Pts',(14.9535443735311,-11.0047064042251,-322.00267946985)) ;
#39817 = CARTESIAN_POINT('Ctrl Pts',(14.8746337735717,-11.1111350641795,-322.004393167684)) ;
#39818 = CARTESIAN_POINT('Ctrl Pts',(14.6652579711084,-11.3872970908768,-322.00889932241)) ;
#39819 = CARTESIAN_POINT('Ctrl Pts',(14.5329845584379,-11.5556343820061,-322.011706039199)) ;
#39820 = CARTESIAN_POINT('Ctrl Pts',(14.3066820445924,-11.8336043029948,-322.016439793426)) ;
#39821 = CARTESIAN_POINT('Ctrl Pts',(14.2142314600262,-11.9444952116615,-322.018355477367)) ;
#39822 = CARTESIAN_POINT('Ctrl Pts',(13.8104663827197,-12.4174687769428,-322.026639631045)) ;
#39823 = CARTESIAN_POINT('Ctrl Pts',(13.4865405778721,-12.768544722777,-322.033084477673)) ;
#39824 = CARTESIAN_POINT('Ctrl Pts',(13.0009110167178,-13.2557564631522,-322.042344332145)) ;
#39825 = CARTESIAN_POINT('Ctrl Pts',(12.849856953625,-13.4022364946781,-322.045171633086)) ;
#39826 = CARTESIAN_POINT('Ctrl Pts',(12.5290381005741,-13.7029298211261,-322.051043866911)) ;
#39827 = CARTESIAN_POINT('Ctrl Pts',(12.3588391409912,-13.8566293465554,-322.054085050731)) ;
#39828 = CARTESIAN_POINT('Ctrl Pts',(12.1248516071538,-14.0601922805303,-322.058143468442)) ;
#39829 = CARTESIAN_POINT('Ctrl Pts',(12.0635206111987,-14.1128488955102,-322.059196123107)) ;
#39830 = CARTESIAN_POINT('Ctrl Pts',(11.9513214212688,-14.2079133331656,-322.061100185692)) ;
#39831 = CARTESIAN_POINT('Ctrl Pts',(11.9005665166872,-14.2504526809463,-322.061953481352)) ;
#39832 = CARTESIAN_POINT('Ctrl Pts',(11.8347431674475,-14.3050244755886,-322.063049517435)) ;
#39833 = CARTESIAN_POINT('Ctrl Pts',(11.8198822704366,-14.3173061083432,-322.063296290273)) ;
#39834 = CARTESIAN_POINT('Ctrl Pts',(11.8035379939324,-14.3307708734579,-322.063566966799)) ;
#39835 = CARTESIAN_POINT('Ctrl Pts',(11.8020735360014,-14.3319769485082,-322.063591213178)) ;
#39836 = CARTESIAN_POINT('Ctrl Pts',(11.7981766645179,-14.3351852698509,-322.063655714919)) ;
#39837 = CARTESIAN_POINT('Ctrl Pts',(11.7957439260656,-14.3371871215666,-322.063695964409)) ;
#39838 = CARTESIAN_POINT('Ctrl Pts',(11.7911234627865,-14.3409872361603,-322.063772376267)) ;
#39839 = CARTESIAN_POINT('Ctrl Pts',(11.7889358358678,-14.3427856178701,-322.063808540391)) ;
#39840 = CARTESIAN_POINT('Ctrl Pts',(11.7847961856874,-14.3461871117266,-322.063876947042)) ;
#39841 = CARTESIAN_POINT('Ctrl Pts',(11.7828442465864,-14.3477903261634,-322.063909191072)) ;
#39842 = CARTESIAN_POINT('Ctrl Pts',(11.779164081544,-14.350811751976,-322.063969962458)) ;
#39843 = CARTESIAN_POINT('Ctrl Pts',(11.7774359264955,-14.3522300496432,-322.063998491075)) ;
#39844 = CARTESIAN_POINT('Ctrl Pts',(11.7741893089175,-14.3548935689742,-322.064052070205)) ;
#39845 = CARTESIAN_POINT('Ctrl Pts',(11.7726709049408,-14.3561388619212,-322.064077121754)) ;
#39846 = CARTESIAN_POINT('Ctrl Pts',(11.7698281175199,-14.3584695709068,-322.06412401115)) ;
#39847 = CARTESIAN_POINT('Ctrl Pts',(11.7685037814176,-14.3595550446864,-322.064145849833)) ;
#39848 = CARTESIAN_POINT('Ctrl Pts',(11.7660323636788,-14.3615801365324,-322.064186594668)) ;
#39849 = CARTESIAN_POINT('Ctrl Pts',(11.7648853196421,-14.3625198003988,-322.064205501481)) ;
#39850 = CARTESIAN_POINT('Ctrl Pts',(11.7627512060374,-14.364267649095,-322.064240671105)) ;
#39851 = CARTESIAN_POINT('Ctrl Pts',(11.7617641657249,-14.3650758696165,-322.06425693443)) ;
#39852 = CARTESIAN_POINT('Ctrl Pts',(11.7599328145455,-14.3665751238862,-322.064287104093)) ;
#39853 = CARTESIAN_POINT('Ctrl Pts',(11.7590885260315,-14.3672661849721,-322.064301010824)) ;
#39854 = CARTESIAN_POINT('Ctrl Pts',(11.757525944384,-14.3685449482881,-322.064326745118)) ;
#39855 = CARTESIAN_POINT('Ctrl Pts',(11.7568076681107,-14.3691326710728,-322.064338572977)) ;
#39856 = CARTESIAN_POINT('Ctrl Pts',(11.755481265493,-14.3702178214666,-322.064360412094)) ;
#39857 = CARTESIAN_POINT('Ctrl Pts',(11.7548731515948,-14.3707152643725,-322.064370423571)) ;
#39858 = CARTESIAN_POINT('Ctrl Pts',(11.7537523853557,-14.3716319429916,-322.064388872954)) ;
#39859 = CARTESIAN_POINT('Ctrl Pts',(11.7532397421933,-14.3720511898476,-322.064397311019)) ;
#39860 = CARTESIAN_POINT('Ctrl Pts',(11.7513601101291,-14.3735882118087,-322.064428246823)) ;
#39861 = CARTESIAN_POINT('Ctrl Pts',(11.7499929842702,-14.374705819257,-322.064450742175)) ;
#39862 = CARTESIAN_POINT('Ctrl Pts',(11.7472982812165,-14.376908062359,-322.064495071502)) ;
#39863 = CARTESIAN_POINT('Ctrl Pts',(11.7459707131715,-14.3779927092315,-322.064516905637)) ;
#39864 = CARTESIAN_POINT('Ctrl Pts',(11.7433560711052,-14.3801283148243,-322.06455989793)) ;
#39865 = CARTESIAN_POINT('Ctrl Pts',(11.7420690061799,-14.3811792846652,-322.064581056246)) ;
#39866 = CARTESIAN_POINT('Ctrl Pts',(11.6599381424263,-14.448225948841,-322.065930918547)) ;
#39867 = CARTESIAN_POINT('Ctrl Pts',(11.5785393785103,-14.5135390742588,-322.067250013829)) ;
#39868 = CARTESIAN_POINT('Ctrl Pts',(11.3831437054603,-14.6676315234339,-322.070377291639)) ;
#39869 = CARTESIAN_POINT('Ctrl Pts',(11.2686525441204,-14.7557732788085,-322.07217844202)) ;
#39870 = CARTESIAN_POINT('Ctrl Pts',(10.8645300687677,-15.0594428120212,-322.078446466134)) ;
#39871 = CARTESIAN_POINT('Ctrl Pts',(10.5696513811148,-15.2678519043173,-322.082863099093)) ;
#39872 = CARTESIAN_POINT('Ctrl Pts',(9.79620043689015,-15.7813455004837,-322.094234261653)) ;
#39873 = CARTESIAN_POINT('Ctrl Pts',(9.30938045641168,-16.0733270658502,-322.101197275441)) ;
#39874 = CARTESIAN_POINT('Ctrl Pts',(8.64785098806182,-16.4299448522855,-322.110635313847)) ;
#39875 = CARTESIAN_POINT('Ctrl Pts',(8.48445369121153,-16.5149162871027,-322.112963614673)) ;
#39876 = CARTESIAN_POINT('Ctrl Pts',(8.20815657212574,-16.653416067908,-322.116900538467)) ;
#39877 = CARTESIAN_POINT('Ctrl Pts',(8.09593169778051,-16.708261158385,-322.118499552128)) ;
#39878 = CARTESIAN_POINT('Ctrl Pts',(7.87716299809421,-16.8124533281273,-322.121617424277)) ;
#39879 = CARTESIAN_POINT('Ctrl Pts',(7.77068756868404,-16.8619304492606,-322.123135258033)) ;
#39880 = CARTESIAN_POINT('Ctrl Pts',(7.49739174486862,-16.985787460795,-322.127032396544)) ;
#39881 = CARTESIAN_POINT('Ctrl Pts',(7.32993014003453,-17.0587215999645,-322.129421602249)) ;
#39882 = CARTESIAN_POINT('Ctrl Pts',(6.94909899666808,-17.2179407141432,-322.134856139573)) ;
#39883 = CARTESIAN_POINT('Ctrl Pts',(6.73514628559345,-17.3027530626543,-322.137910202091)) ;
#39884 = CARTESIAN_POINT('Ctrl Pts',(5.98059693556983,-17.5857453287367,-322.148667466031)) ;
#39885 = CARTESIAN_POINT('Ctrl Pts',(5.43240854829221,-17.7627394762174,-322.156468329422)) ;
#39886 = CARTESIAN_POINT('Ctrl Pts',(4.5974384296159,-17.9900510861332,-322.168068662631)) ;
#39887 = CARTESIAN_POINT('Ctrl Pts',(4.31624806872453,-18.0595786608134,-322.171926300698)) ;
#39888 = CARTESIAN_POINT('Ctrl Pts',(3.950169654302,-18.1410571669753,-322.176840643701)) ;
#39889 = CARTESIAN_POINT('Ctrl Pts',(3.86666588556886,-18.159038806875,-322.177954363148)) ;
#39890 = CARTESIAN_POINT('Ctrl Pts',(3.71742782304458,-18.1900995420399,-322.179930054271)) ;
#39891 = CARTESIAN_POINT('Ctrl Pts',(3.65174117689683,-18.2034001600166,-322.180794515968)) ;
#39892 = CARTESIAN_POINT('Ctrl Pts',(3.52534452759131,-18.2282820082814,-322.182447422676)) ;
#39893 = CARTESIAN_POINT('Ctrl Pts',(3.46464604548661,-18.2399163046955,-322.183236668903)) ;
#39894 = CARTESIAN_POINT('Ctrl Pts',(3.32561902237845,-18.2658450954218,-322.18503515042)) ;
#39895 = CARTESIAN_POINT('Ctrl Pts',(3.24725431919159,-18.2799392323626,-322.186042190625)) ;
#39896 = CARTESIAN_POINT('Ctrl Pts',(3.04055253725548,-18.3157440727528,-322.188683367376)) ;
#39897 = CARTESIAN_POINT('Ctrl Pts',(2.9120735392729,-18.3366100586124,-322.190309770728)) ;
#39898 = CARTESIAN_POINT('Ctrl Pts',(1.8622602576627,-18.4957959163459,-322.203507515841)) ;
#39899 = CARTESIAN_POINT('Ctrl Pts',(0.931937063063516,-18.5659362218982,
-322.214702258193)) ;
#39900 = CARTESIAN_POINT('Ctrl Pts',(0.000274526296958344,-18.5659499979704,
-322.226379248718)) ;
#39901 = CARTESIAN_POINT('Ctrl Pts',(0.000274526296966671,-18.5659499979704,
-322.226379248718)) ;
#39902 = CARTESIAN_POINT('Ctrl Pts',(-0.17127499577746,-18.5659525345955,
-322.228529364307)) ;
#39903 = CARTESIAN_POINT('Ctrl Pts',(-0.342816106782395,-18.5635773933165,
-322.230692607528)) ;
#39904 = CARTESIAN_POINT('Ctrl Pts',(-0.6306775490769,-18.5556002192189,-322.234349106168)) ;
#39905 = CARTESIAN_POINT('Ctrl Pts',(-0.747022644124064,-18.5512805702038,
-322.23583417216)) ;
#39906 = CARTESIAN_POINT('Ctrl Pts',(-0.982475836102893,-18.5403201072191,
-322.238855149987)) ;
#39907 = CARTESIAN_POINT('Ctrl Pts',(-1.101576030394,-18.5336250812034,-322.240391344776)) ;
#39908 = CARTESIAN_POINT('Ctrl Pts',(-1.37989345246346,-18.5152876551864,
-322.244000657076)) ;
#39909 = CARTESIAN_POINT('Ctrl Pts',(-1.53904140381831,-18.5027385633866,
-322.246079501278)) ;
#39910 = CARTESIAN_POINT('Ctrl Pts',(-2.10919646486465,-18.450373768721,-322.253580164116)) ;
#39911 = CARTESIAN_POINT('Ctrl Pts',(-2.51900994752054,-18.3989018484258,
-322.259073337982)) ;
#39912 = CARTESIAN_POINT('Ctrl Pts',(-3.3943499302506,-18.2591647059414,-322.270962533878)) ;
#39913 = CARTESIAN_POINT('Ctrl Pts',(-3.8589079977686,-18.1666600040671,-322.277369468432)) ;
#39914 = CARTESIAN_POINT('Ctrl Pts',(-4.58924822288483,-17.991950246664,-322.287431142309)) ;
#39915 = CARTESIAN_POINT('Ctrl Pts',(-4.85759603396007,-17.9213625107553,
-322.291124529114)) ;
#39916 = CARTESIAN_POINT('Ctrl Pts',(-5.19523388521698,-17.8244073322759,
-322.295728358093)) ;
#39917 = CARTESIAN_POINT('Ctrl Pts',(-5.26608432653722,-17.8036037855265,
-322.29669196258)) ;
#39918 = CARTESIAN_POINT('Ctrl Pts',(-5.39474680641894,-17.7649898805929,
-322.298436151604)) ;
#39919 = CARTESIAN_POINT('Ctrl Pts',(-5.45259950972636,-17.7473185907129,
-322.299218317454)) ;
#39920 = CARTESIAN_POINT('Ctrl Pts',(-5.56912535076216,-17.7111018449986,
-322.300788735408)) ;
#39921 = CARTESIAN_POINT('Ctrl Pts',(-5.6277946977462,-17.6925468087214,-322.301576808449)) ;
#39922 = CARTESIAN_POINT('Ctrl Pts',(-5.79128287986047,-17.6399458033243,
-322.303766836397)) ;
#39923 = CARTESIAN_POINT('Ctrl Pts',(-5.8958925296753,-17.6052576428838,-322.305161236504)) ;
#39924 = CARTESIAN_POINT('Ctrl Pts',(-6.56866592757272,-17.3754995875418,
-322.314100896557)) ;
#39925 = CARTESIAN_POINT('Ctrl Pts',(-7.12738926330805,-17.1538825171434,
-322.321407125439)) ;
#39926 = CARTESIAN_POINT('Ctrl Pts',(-7.99246583352356,-16.7611758012988,
-322.333055275585)) ;
#39927 = CARTESIAN_POINT('Ctrl Pts',(-8.30640736381268,-16.6078331092422,
-322.337353110021)) ;
#39928 = CARTESIAN_POINT('Ctrl Pts',(-8.77697786698898,-16.3613035222652,
-322.343966244176)) ;
#39929 = CARTESIAN_POINT('Ctrl Pts',(-8.9368708743613,-16.2745178813324,-322.346243932381)) ;
#39930 = CARTESIAN_POINT('Ctrl Pts',(-9.2346352756907,-16.1071877256535,-322.350550565587)) ;
#39931 = CARTESIAN_POINT('Ctrl Pts',(-9.37279342024897,-16.0271871675418,
-322.352575618555)) ;
#39932 = CARTESIAN_POINT('Ctrl Pts',(-9.593731726245,-15.8954187715121,-322.355860161626)) ;
#39933 = CARTESIAN_POINT('Ctrl Pts',(-9.67716537056744,-15.8447624381988,
-322.357111282986)) ;
#39934 = CARTESIAN_POINT('Ctrl Pts',(-9.84344097751455,-15.7420057642807,
-322.359626733205)) ;
#39935 = CARTESIAN_POINT('Ctrl Pts',(-9.9262782378198,-15.6899036351665,-322.360891048471)) ;
#39936 = CARTESIAN_POINT('Ctrl Pts',(-10.1630327761385,-15.5383667371287,
-322.364536941529)) ;
#39937 = CARTESIAN_POINT('Ctrl Pts',(-10.3158948190304,-15.437305140142,-322.366930764325)) ;
#39938 = CARTESIAN_POINT('Ctrl Pts',(-10.9580991120082,-14.9989260647076,
-322.37715583758)) ;
#39939 = CARTESIAN_POINT('Ctrl Pts',(-11.4325889155877,-14.6404790047745,
-322.38514380207)) ;
#39940 = CARTESIAN_POINT('Ctrl Pts',(-12.153093705884,-14.0397642789368,-322.397780346735)) ;
#39941 = CARTESIAN_POINT('Ctrl Pts',(-12.4109569763725,-13.8123428461418,
-322.402411493097)) ;
#39942 = CARTESIAN_POINT('Ctrl Pts',(-12.7653435244286,-13.4818520334931,
-322.408864723883)) ;
#39943 = CARTESIAN_POINT('Ctrl Pts',(-12.8672336228626,-13.3846415166313,
-322.410730718596)) ;
#39944 = CARTESIAN_POINT('Ctrl Pts',(-12.9695356351892,-13.2847901514057,
-322.412610979222)) ;
#39945 = CARTESIAN_POINT('Ctrl Pts',(-12.971063004959,-13.2832988553561,-322.412639053056)) ;
#39946 = CARTESIAN_POINT('Ctrl Pts',(-12.9772950777296,-13.2772118730777,
-322.412753607913)) ;
#39947 = CARTESIAN_POINT('Ctrl Pts',(-12.9819975960612,-13.2726139502712,
-322.412840061649)) ;
#39948 = CARTESIAN_POINT('Ctrl Pts',(-12.9908773040995,-13.2639225147793,
-322.413003337542)) ;
#39949 = CARTESIAN_POINT('Ctrl Pts',(-12.995055004569,-13.2598295251663,-322.41308016617)) ;
#39950 = CARTESIAN_POINT('Ctrl Pts',(-13.0029477592488,-13.2520894984617,
-322.413225335567)) ;
#39951 = CARTESIAN_POINT('Ctrl Pts',(-13.0066632148376,-13.2484428715525,
-322.413293681487)) ;
#39952 = CARTESIAN_POINT('Ctrl Pts',(-13.0136866047863,-13.241543787482,-322.413422892637)) ;
#39953 = CARTESIAN_POINT('Ctrl Pts',(-13.0169948548552,-13.2382916523272,
-322.413483761967)) ;
#39954 = CARTESIAN_POINT('Ctrl Pts',(-13.0232522075587,-13.2321358241763,
-322.413598904748)) ;
#39955 = CARTESIAN_POINT('Ctrl Pts',(-13.0262015588289,-13.229232384379,-322.413653181462)) ;
#39956 = CARTESIAN_POINT('Ctrl Pts',(-13.0877306517851,-13.1686205667784,
-322.414785601769)) ;
#39957 = CARTESIAN_POINT('Ctrl Pts',(-13.1459273849018,-13.1105245684571,
-322.415858673326)) ;
#39958 = CARTESIAN_POINT('Ctrl Pts',(-13.2518163449607,-13.0034049538387,
-322.41781312738)) ;
#39959 = CARTESIAN_POINT('Ctrl Pts',(-13.2996273712613,-12.9545007105393,
-322.418696343608)) ;
#39960 = CARTESIAN_POINT('Ctrl Pts',(-13.3991735811314,-12.8515463831969,
-322.420535812825)) ;
#39961 = CARTESIAN_POINT('Ctrl Pts',(-13.4508544070228,-12.7974455590814,
-322.421491259464)) ;
#39962 = CARTESIAN_POINT('Ctrl Pts',(-13.6016823651333,-12.637631944614,-322.424283491572)) ;
#39963 = CARTESIAN_POINT('Ctrl Pts',(-13.6999204367205,-12.5310687681045,
-322.426107067187)) ;
#39964 = CARTESIAN_POINT('Ctrl Pts',(-14.0202785818352,-12.1752916390353,
-322.432089187644)) ;
#39965 = CARTESIAN_POINT('Ctrl Pts',(-14.2369254060334,-11.9212370905213,
-322.436193177196)) ;
#39966 = CARTESIAN_POINT('Ctrl Pts',(-14.7471156158916,-11.2891975411636,
-322.446151181402)) ;
#39967 = CARTESIAN_POINT('Ctrl Pts',(-15.0331238700007,-10.9054383984895,
-322.451992394644)) ;
#39968 = CARTESIAN_POINT('Ctrl Pts',(-15.3858101438176,-10.3919311255983,
-322.459711562054)) ;
#39969 = CARTESIAN_POINT('Ctrl Pts',(-15.4662375685578,-10.2718489920668,
-322.461509604472)) ;
#39970 = CARTESIAN_POINT('Ctrl Pts',(-15.6623821064718,-9.97146826035132,
-322.465995508089)) ;
#39971 = CARTESIAN_POINT('Ctrl Pts',(-15.7763960030746,-9.79008281069018,
-322.46869406625)) ;
#39972 = CARTESIAN_POINT('Ctrl Pts',(-15.9558136905284,-9.49336974146189,
-322.473100055769)) ;
#39973 = CARTESIAN_POINT('Ctrl Pts',(-16.0231660738069,-9.3792434921586,-322.474792745539)) ;
#39974 = CARTESIAN_POINT('Ctrl Pts',(-16.1523929056292,-9.1548180881739,-322.478118727095)) ;
#39975 = CARTESIAN_POINT('Ctrl Pts',(-16.2143736361861,-9.0445883453869,-322.479751107198)) ;
#39976 = CARTESIAN_POINT('Ctrl Pts',(-16.3501616114037,-8.79721366450402,
-322.483412214697)) ;
#39977 = CARTESIAN_POINT('Ctrl Pts',(-16.4233790921494,-8.6597558900629,-322.485445079188)) ;
#39978 = CARTESIAN_POINT('Ctrl Pts',(-16.8200155949451,-7.89198673975013,
-322.496789695689)) ;
#39979 = CARTESIAN_POINT('Ctrl Pts',(-17.1088801753455,-7.2444868979147,-322.506346237202)) ;
#39980 = CARTESIAN_POINT('Ctrl Pts',(-17.4606946912828,-6.31658576798109,
-322.519704372618)) ;
#39981 = CARTESIAN_POINT('Ctrl Pts',(-17.5552509096346,-6.04882473553525,
-322.523517657129)) ;
#39982 = CARTESIAN_POINT('Ctrl Pts',(-17.6993226692579,-5.60896516899133,
-322.529667778063)) ;
#39983 = CARTESIAN_POINT('Ctrl Pts',(-17.752555321532,-5.43813322456599,-322.532028616482)) ;
#39984 = CARTESIAN_POINT('Ctrl Pts',(-17.8261713374102,-5.18927833875265,
-322.535414982942)) ;
#39985 = CARTESIAN_POINT('Ctrl Pts',(-17.8485288427502,-5.11185019356561,
-322.536461251682)) ;
#39986 = CARTESIAN_POINT('Ctrl Pts',(-17.8883830932591,-4.97037796290353,
-322.538357950831)) ;
#39987 = CARTESIAN_POINT('Ctrl Pts',(-17.90604175566,-4.90638109243522,-322.539210220114)) ;
#39988 = CARTESIAN_POINT('Ctrl Pts',(-17.9488695463753,-4.747857408782,-322.541308012954)) ;
#39989 = CARTESIAN_POINT('Ctrl Pts',(-17.9736355987195,-4.65322376116195,
-322.542548818255)) ;
#39990 = CARTESIAN_POINT('Ctrl Pts',(-18.0788474256281,-4.23782220772093,
-322.547953073021)) ;
#39991 = CARTESIAN_POINT('Ctrl Pts',(-18.1514627025081,-3.91513270021438,
-322.552041882715)) ;
#39992 = CARTESIAN_POINT('Ctrl Pts',(-18.3199592136442,-3.06035354488316,
-322.562750321654)) ;
#39993 = CARTESIAN_POINT('Ctrl Pts',(-18.4012883306582,-2.5257192497463,-322.569330244433)) ;
#39994 = CARTESIAN_POINT('Ctrl Pts',(-18.4756697719667,-1.83516943608711,
-322.577923842941)) ;
#39995 = CARTESIAN_POINT('Ctrl Pts',(-18.4902578423361,-1.68183983734956,
-322.579837267822)) ;
#39996 = CARTESIAN_POINT('Ctrl Pts',(-18.5213440831971,-1.30549409996041,
-322.584553638139)) ;
#39997 = CARTESIAN_POINT('Ctrl Pts',(-18.5357241108584,-1.08232754789527,
-322.587367592958)) ;
#39998 = CARTESIAN_POINT('Ctrl Pts',(-18.5522767319188,-0.724933192378983,
-322.591910955447)) ;
#39999 = CARTESIAN_POINT('Ctrl Pts',(-18.5570310056149,-0.590847073819983,
-322.593623752261)) ;
#40000 = CARTESIAN_POINT('Ctrl Pts',(-18.5634198433313,-0.331216232653277,
-322.596957510338)) ;
#40001 = CARTESIAN_POINT('Ctrl Pts',(-18.5652351146783,-0.205683145668503,
-322.598577208613)) ;
#40002 = CARTESIAN_POINT('Ctrl Pts',(-18.5665551160946,0.100111914086229,
-322.602542310271)) ;
#40003 = CARTESIAN_POINT('Ctrl Pts',(-18.5647080663818,0.280366782065616,
-322.604896206454)) ;
#40004 = CARTESIAN_POINT('Ctrl Pts',(-18.5507578581033,0.84254292289514,-322.612287715341)) ;
#40005 = CARTESIAN_POINT('Ctrl Pts',(-18.5294896603066,1.22413537569122,-322.617379052172)) ;
#40006 = CARTESIAN_POINT('Ctrl Pts',(-18.4874892441675,1.70822057316831,-322.623899669589)) ;
#40007 = CARTESIAN_POINT('Ctrl Pts',(-18.4776488158167,1.81156570632273,-322.625295162937)) ;
#40008 = CARTESIAN_POINT('Ctrl Pts',(-18.4230214451507,2.33840321713817,-322.632422301014)) ;
#40009 = CARTESIAN_POINT('Ctrl Pts',(-18.3645400967907,2.76034706622736,-322.63817689996)) ;
#40010 = CARTESIAN_POINT('Ctrl Pts',(-18.2530211510424,3.40183153295329,-322.646866894112)) ;
#40011 = CARTESIAN_POINT('Ctrl Pts',(-18.2104047343149,3.62303721675657,-322.649852002231)) ;
#40012 = CARTESIAN_POINT('Ctrl Pts',(-18.1457633707265,3.92852901673376,-322.653935055867)) ;
#40013 = CARTESIAN_POINT('Ctrl Pts',(-18.127154898035,4.01351764341147,-322.655066678312)) ;
#40014 = CARTESIAN_POINT('Ctrl Pts',(-18.0948724830815,4.15615191125085,-322.656956795723)) ;
#40015 = CARTESIAN_POINT('Ctrl Pts',(-18.0815187992598,4.21386839063102,-322.657719030513)) ;
#40016 = CARTESIAN_POINT('Ctrl Pts',(-18.0483968686338,4.35396918431943,-322.659562958909)) ;
#40017 = CARTESIAN_POINT('Ctrl Pts',(-18.0283405374,4.43628388188943,-322.660641228985)) ;
#40018 = CARTESIAN_POINT('Ctrl Pts',(-17.9607132778176,4.70580342257276,-322.664158898713)) ;
#40019 = CARTESIAN_POINT('Ctrl Pts',(-17.9107842774774,4.89240371451056,-322.666574014534)) ;
#40020 = CARTESIAN_POINT('Ctrl Pts',(-17.7797327754401,5.35325905982929,-322.672520734322)) ;
#40021 = CARTESIAN_POINT('Ctrl Pts',(-17.6951678514747,5.62648337880519,-322.676030711984)) ;
#40022 = CARTESIAN_POINT('Ctrl Pts',(-17.4584889336851,6.33296410468003,-322.685160631419)) ;
#40023 = CARTESIAN_POINT('Ctrl Pts',(-17.2965556492303,6.76272375520635,-322.6907713178)) ;
#40024 = CARTESIAN_POINT('Ctrl Pts',(-17.0641872680774,7.31628079220495,-322.698214354166)) ;
#40025 = CARTESIAN_POINT('Ctrl Pts',(-17.008030176082,7.44589559590484,-322.699972621004)) ;
#40026 = CARTESIAN_POINT('Ctrl Pts',(-16.8643437953347,7.76742531099051,-322.704378220408)) ;
#40027 = CARTESIAN_POINT('Ctrl Pts',(-16.7750128932203,7.95851304079422,-322.707036124417)) ;
#40028 = CARTESIAN_POINT('Ctrl Pts',(-16.6245439396819,8.26658603701062,-322.711393764484)) ;
#40029 = CARTESIAN_POINT('Ctrl Pts',(-16.5653802453157,8.38451448669527,-322.713079397315)) ;
#40030 = CARTESIAN_POINT('Ctrl Pts',(-16.4468822967459,8.61456035355865,-322.716403451)) ;
#40031 = CARTESIAN_POINT('Ctrl Pts',(-16.3876459925431,8.72672023939676,-322.718041091183)) ;
#40032 = CARTESIAN_POINT('Ctrl Pts',(-16.2374820082116,9.00412393773313,-322.72213442688)) ;
#40033 = CARTESIAN_POINT('Ctrl Pts',(-16.1451769541271,9.16860571733807,-322.724599998984)) ;
#40034 = CARTESIAN_POINT('Ctrl Pts',(-15.8701686067569,9.64161830692855,-322.731800958927)) ;
#40035 = CARTESIAN_POINT('Ctrl Pts',(-15.6810142629751,9.94629810015572,-322.736579492333)) ;
#40036 = CARTESIAN_POINT('Ctrl Pts',(-15.4268495051036,10.330402960371,-322.742759221398)) ;
#40037 = CARTESIAN_POINT('Ctrl Pts',(-15.3698414915035,10.4150316126359,-322.744130638706)) ;
#40038 = CARTESIAN_POINT('Ctrl Pts',(-15.0226495234136,10.9213805428511,-322.752390816278)) ;
#40039 = CARTESIAN_POINT('Ctrl Pts',(-14.7158227035902,11.3314215368165,-322.759316801468)) ;
#40040 = CARTESIAN_POINT('Ctrl Pts',(-14.2862892125413,11.8585276964675,-322.768340212243)) ;
#40041 = CARTESIAN_POINT('Ctrl Pts',(-14.1783697860248,11.9873503731716,-322.770554904133)) ;
#40042 = CARTESIAN_POINT('Ctrl Pts',(-14.0172679661198,12.1744369378905,-322.773774508957)) ;
#40043 = CARTESIAN_POINT('Ctrl Pts',(-13.9654395321194,12.2338552666865,-322.774797529725)) ;
#40044 = CARTESIAN_POINT('Ctrl Pts',(-13.8690045020727,12.3430010826833,-322.776676102596)) ;
#40045 = CARTESIAN_POINT('Ctrl Pts',(-13.8245051064762,12.3928213154934,-322.777533184753)) ;
#40046 = CARTESIAN_POINT('Ctrl Pts',(-13.7232480059677,12.504961758982,-322.77946239842)) ;
#40047 = CARTESIAN_POINT('Ctrl Pts',(-13.6663327872064,12.5671378046869,-322.780532145115)) ;
#40048 = CARTESIAN_POINT('Ctrl Pts',(-13.4180895795675,12.834646010466,-322.785140130186)) ;
#40049 = CARTESIAN_POINT('Ctrl Pts',(-13.2225424483544,13.0360131186499,-322.788623403675)) ;
#40050 = CARTESIAN_POINT('Ctrl Pts',(-12.7262919564699,13.5243746565147,-322.797204400396)) ;
#40051 = CARTESIAN_POINT('Ctrl Pts',(-12.4203739193012,13.8058512613495,-322.802272422524)) ;
#40052 = CARTESIAN_POINT('Ctrl Pts',(-11.8660443144664,14.2825431945862,-322.811249257289)) ;
#40053 = CARTESIAN_POINT('Ctrl Pts',(-11.6216155270353,14.4821303648834,-322.815141181741)) ;
#40054 = CARTESIAN_POINT('Ctrl Pts',(-11.1850639078728,14.8204219248919,-322.822028206075)) ;
#40055 = CARTESIAN_POINT('Ctrl Pts',(-10.9951508941971,14.9618587470929,-322.825003840728)) ;
#40056 = CARTESIAN_POINT('Ctrl Pts',(-10.6915989894363,15.1790260887002,-322.829739708169)) ;
#40057 = CARTESIAN_POINT('Ctrl Pts',(-10.5797409533026,15.2572016846858,-322.831480565525)) ;
#40058 = CARTESIAN_POINT('Ctrl Pts',(-10.362990608877,15.4051547558922,-322.834847136696)) ;
#40059 = CARTESIAN_POINT('Ctrl Pts',(-10.2582298959153,15.4751118497351,-322.836471315908)) ;
#40060 = CARTESIAN_POINT('Ctrl Pts',(-10.0066288968964,15.6394483378442,-322.840365630701)) ;
#40061 = CARTESIAN_POINT('Ctrl Pts',(-9.85915372314473,15.7328336264385,-322.84264317811)) ;
#40062 = CARTESIAN_POINT('Ctrl Pts',(-9.11485571303427,16.1895678359832,-322.854110567979)) ;
#40063 = CARTESIAN_POINT('Ctrl Pts',(-8.49917436234268,16.5210995062818,-322.863533905941)) ;
#40064 = CARTESIAN_POINT('Ctrl Pts',(-7.60586537404308,16.9389481578567,-322.876810365956)) ;
#40065 = CARTESIAN_POINT('Ctrl Pts',(-7.34265633256373,17.0546929343031,-322.880672368199)) ;
#40066 = CARTESIAN_POINT('Ctrl Pts',(-6.91016937762621,17.2330081523047,-322.886889241106)) ;
#40067 = CARTESIAN_POINT('Ctrl Pts',(-6.74248030187543,17.299305488436,-322.889268699919)) ;
#40068 = CARTESIAN_POINT('Ctrl Pts',(-6.49828116716997,17.3917615801095,-322.892676208916)) ;
#40069 = CARTESIAN_POINT('Ctrl Pts',(-6.42252428897695,17.4198797575881,-322.893725346132)) ;
#40070 = CARTESIAN_POINT('Ctrl Pts',(-6.28423683014801,17.4701822738495,-322.895624393359)) ;
#40071 = CARTESIAN_POINT('Ctrl Pts',(-6.22176647166556,17.4925276385599,-322.896476179755)) ;
#40072 = CARTESIAN_POINT('Ctrl Pts',(-6.06724603148982,17.5468664311816,-322.898568855612)) ;
#40073 = CARTESIAN_POINT('Ctrl Pts',(-5.97506126370977,17.5784708918308,-322.899805086393)) ;
#40074 = CARTESIAN_POINT('Ctrl Pts',(-5.5592434858207,17.7173802309106,-322.905334570043)) ;
#40075 = CARTESIAN_POINT('Ctrl Pts',(-5.23293966112374,17.8164837713082,-322.90954787855)) ;
#40076 = CARTESIAN_POINT('Ctrl Pts',(-4.82064247999461,17.9294002018915,-322.914800254231)) ;
#40077 = CARTESIAN_POINT('Ctrl Pts',(-4.73703437413505,17.9516709769095,-322.91586165429)) ;
#40078 = CARTESIAN_POINT('Ctrl Pts',(-4.19474242517839,18.0920695068885,-322.922728225468)) ;
#40079 = CARTESIAN_POINT('Ctrl Pts',(-3.73183619769794,18.1931921733634,-322.928512400127)) ;
#40080 = CARTESIAN_POINT('Ctrl Pts',(-2.96958324878344,18.3293884416981,-322.938108410506)) ;
#40081 = CARTESIAN_POINT('Ctrl Pts',(-2.67235459758366,18.3750762084813,-322.941866472777)) ;
#40082 = CARTESIAN_POINT('Ctrl Pts',(-2.22864922231542,18.432285369773,-322.947526381345)) ;
#40083 = CARTESIAN_POINT('Ctrl Pts',(-2.0829330922385,18.4493200677167,-322.949392924369)) ;
#40084 = CARTESIAN_POINT('Ctrl Pts',(-1.82608446140126,18.47626475877,-322.952698605503)) ;
#40085 = CARTESIAN_POINT('Ctrl Pts',(-1.71503582873146,18.4869033633402,-322.954132920835)) ;
#40086 = CARTESIAN_POINT('Ctrl Pts',(-1.45498158596716,18.5094535542963,-322.957504291364)) ;
#40087 = CARTESIAN_POINT('Ctrl Pts',(-1.30591466942753,18.5205677310935,-322.959446406053)) ;
#40088 = CARTESIAN_POINT('Ctrl Pts',(-0.836857992938834,18.5498486492047,
-322.965587609346)) ;
#40089 = CARTESIAN_POINT('Ctrl Pts',(-0.516523333184205,18.561530623166,-322.969826542955)) ;
#40090 = CARTESIAN_POINT('Ctrl Pts',(-0.0116220883004283,18.5668624426045,
-322.976562153599)) ;
#40091 = CARTESIAN_POINT('Ctrl Pts',(0.172822257716258,18.5660617366694,-322.979033883032)) ;
#40092 = CARTESIAN_POINT('Ctrl Pts',(0.828910724535513,18.5534357281749,-322.987851412228)) ;
#40093 = CARTESIAN_POINT('Ctrl Pts',(1.30007993527823,18.526382870547,-322.99423455782)) ;
#40094 = CARTESIAN_POINT('Ctrl Pts',(1.93355269242442,18.4657240678223,-323.002735719634)) ;
#40095 = CARTESIAN_POINT('Ctrl Pts',(2.09718390716215,18.4478565460352,-323.004923786074)) ;
#40096 = CARTESIAN_POINT('Ctrl Pts',(2.38375399823455,18.4127027462809,-323.008730791201)) ;
#40097 = CARTESIAN_POINT('Ctrl Pts',(2.50679751352192,18.3963548522265,-323.010357257756)) ;
#40098 = CARTESIAN_POINT('Ctrl Pts',(2.69979621813662,18.368740251823,-323.012890868477)) ;
#40099 = CARTESIAN_POINT('Ctrl Pts',(2.76986655090538,18.3583048609993,-323.013807070801)) ;
#40100 = CARTESIAN_POINT('Ctrl Pts',(2.90159980068149,18.3379147986977,-323.015521533172)) ;
#40101 = CARTESIAN_POINT('Ctrl Pts',(2.96327554104603,18.3280495047162,-323.016320920473)) ;
#40102 = CARTESIAN_POINT('Ctrl Pts',(3.13917304822823,18.2990028774615,-323.018592715469)) ;
#40103 = CARTESIAN_POINT('Ctrl Pts',(3.25326679488404,18.2790636784316,-323.020056609989)) ;
#40104 = CARTESIAN_POINT('Ctrl Pts',(3.59113255560094,18.2167541878368,-323.024371717465)) ;
#40105 = CARTESIAN_POINT('Ctrl Pts',(3.81431994302679,18.1713326385624,-323.027196361659)) ;
#40106 = CARTESIAN_POINT('Ctrl Pts',(4.61240152963709,17.9935608149586,-323.037277322273)) ;
#40107 = CARTESIAN_POINT('Ctrl Pts',(5.18174798887874,17.8379362034796,-323.044442918194)) ;
#40108 = CARTESIAN_POINT('Ctrl Pts',(5.89538272484891,17.6058153504855,-323.053719476534)) ;
#40109 = CARTESIAN_POINT('Ctrl Pts',(6.04739663767838,17.5541808541518,-323.055712094674)) ;
#40110 = CARTESIAN_POINT('Ctrl Pts',(6.4154111264272,17.4238297923769,-323.060584527398)) ;
#40111 = CARTESIAN_POINT('Ctrl Pts',(6.63065610970241,17.3430603940443,-323.063475520547)) ;
#40112 = CARTESIAN_POINT('Ctrl Pts',(6.97008384732953,17.2084493002973,-323.06811062586)) ;
#40113 = CARTESIAN_POINT('Ctrl Pts',(7.09527350963028,17.1572110180726,-323.06983683138)) ;
#40114 = CARTESIAN_POINT('Ctrl Pts',(7.33638888977303,17.0554357037165,-323.073195283766)) ;
#40115 = CARTESIAN_POINT('Ctrl Pts',(7.45238031752238,17.0050732587243,-323.074826230352)) ;
#40116 = CARTESIAN_POINT('Ctrl Pts',(7.70463106536363,16.8924716143047,-323.078407255877)) ;
#40117 = CARTESIAN_POINT('Ctrl Pts',(7.84066994099358,16.8297603037657,-323.080360553414)) ;
#40118 = CARTESIAN_POINT('Ctrl Pts',(8.64707379969398,16.4461237104936,-323.092070081746)) ;
#40119 = CARTESIAN_POINT('Ctrl Pts',(9.29843316531179,16.0868269538081,-323.102103331319)) ;
#40120 = CARTESIAN_POINT('Ctrl Pts',(10.1564249615511,15.5439879566535,-323.11576563641)) ;
#40121 = CARTESIAN_POINT('Ctrl Pts',(10.3831293834222,15.3934776481392,-323.119417174517)) ;
#40122 = CARTESIAN_POINT('Ctrl Pts',(10.7494435716941,15.1385044954508,-323.125344381295)) ;
#40123 = CARTESIAN_POINT('Ctrl Pts',(10.8910351422731,15.036961434136,-323.127642137074)) ;
#40124 = CARTESIAN_POINT('Ctrl Pts',(11.0954029584469,14.8859970604822,-323.130956701801)) ;
#40125 = CARTESIAN_POINT('Ctrl Pts',(11.1593226259447,14.8381398378867,-323.131993096389)) ;
#40126 = CARTESIAN_POINT('Ctrl Pts',(11.2759435874274,14.7496448798731,-323.133881892296)) ;
#40127 = CARTESIAN_POINT('Ctrl Pts',(11.3287387866487,14.7091333995547,-323.134736002419)) ;
#40128 = CARTESIAN_POINT('Ctrl Pts',(11.4596436746655,14.6075629498738,-323.136852257152)) ;
#40129 = CARTESIAN_POINT('Ctrl Pts',(11.5374842718662,14.5461604969419,-323.138109469561)) ;
#40130 = CARTESIAN_POINT('Ctrl Pts',(11.880929743985,14.2707515833488,-323.143659593439)) ;
#40131 = CARTESIAN_POINT('Ctrl Pts',(12.1410998304265,14.050072537942,-323.14787341054)) ;
#40132 = CARTESIAN_POINT('Ctrl Pts',(12.7024345516268,13.5467017464953,-323.157136124032)) ;
#40133 = CARTESIAN_POINT('Ctrl Pts',(13.0005452478334,13.2608746024258,-323.162172618686)) ;
#40134 = CARTESIAN_POINT('Ctrl Pts',(13.4834154063907,12.7659551212048,-323.170682850408)) ;
#40135 = CARTESIAN_POINT('Ctrl Pts',(13.6734401443441,12.562210611947,-323.174130195803)) ;
#40136 = CARTESIAN_POINT('Ctrl Pts',(14.0039133877789,12.1914913359547,-323.180337189452)) ;
#40137 = CARTESIAN_POINT('Ctrl Pts',(14.1461393644204,12.02617112833,-323.183082937777)) ;
#40138 = CARTESIAN_POINT('Ctrl Pts',(14.3704908693923,11.755901975186,-323.187545087618)) ;
#40139 = CARTESIAN_POINT('Ctrl Pts',(14.4544564537656,11.6525073542921,-323.189245993398)) ;
#40140 = CARTESIAN_POINT('Ctrl Pts',(14.6157098962865,11.4495158665365,-323.19257477718)) ;
#40141 = CARTESIAN_POINT('Ctrl Pts',(14.6931103241828,11.3500175461696,-323.194201596378)) ;
#40142 = CARTESIAN_POINT('Ctrl Pts',(14.8807624113691,11.1036539695857,-323.198218492017)) ;
#40143 = CARTESIAN_POINT('Ctrl Pts',(14.9898597613537,10.9559265055322,-323.200617615748)) ;
#40144 = CARTESIAN_POINT('Ctrl Pts',(15.4695628481123,10.2857848395632,-323.211455851184)) ;
#40145 = CARTESIAN_POINT('Ctrl Pts',(15.8151758419385,9.74602236574991,-323.220081414026)) ;
#40146 = CARTESIAN_POINT('Ctrl Pts',(16.2866283163094,8.91838441015143,-323.232909755593)) ;
#40147 = CARTESIAN_POINT('Ctrl Pts',(16.4341983302619,8.64343496419874,-323.237106618175)) ;
#40148 = CARTESIAN_POINT('Ctrl Pts',(16.6601418906165,8.19573522806367,-323.243777626614)) ;
#40149 = CARTESIAN_POINT('Ctrl Pts',(16.7429196169837,8.02527548860272,-323.246280497556)) ;
#40150 = CARTESIAN_POINT('Ctrl Pts',(16.857842541274,7.77910021333865,-323.249827549817)) ;
#40151 = CARTESIAN_POINT('Ctrl Pts',(16.8921165199983,7.70439191473494,-323.250895175483)) ;
#40152 = CARTESIAN_POINT('Ctrl Pts',(16.9530631418285,7.56918231525463,-323.252809870452)) ;
#40153 = CARTESIAN_POINT('Ctrl Pts',(16.9799107602422,7.50876164122818,-323.253659055251)) ;
#40154 = CARTESIAN_POINT('Ctrl Pts',(17.0446369766174,7.36097259323369,-323.255721160738)) ;
#40155 = CARTESIAN_POINT('Ctrl Pts',(17.0821672440496,7.27345375091314,-323.256929781855)) ;
#40156 = CARTESIAN_POINT('Ctrl Pts',(17.2345268554031,6.91047369566122,-323.261897793557)) ;
#40157 = CARTESIAN_POINT('Ctrl Pts',(17.3433797284869,6.63255177007683,-323.265596458817)) ;
#40158 = CARTESIAN_POINT('Ctrl Pts',(17.6398799022102,5.81824343138718,-323.276265437195)) ;
#40159 = CARTESIAN_POINT('Ctrl Pts',(17.8096636060615,5.27571823362761,-323.28317350547)) ;
#40160 = CARTESIAN_POINT('Ctrl Pts',(18.0125813401712,4.50486688160747,-323.293030837852)) ;
#40161 = CARTESIAN_POINT('Ctrl Pts',(18.0667611545328,4.28241209096131,-323.29587885209)) ;
#40162 = CARTESIAN_POINT('Ctrl Pts',(18.1584523714035,3.8731616642823,-323.301140627959)) ;
#40163 = CARTESIAN_POINT('Ctrl Pts',(18.1972293203258,3.68668125803792,-323.303546546329)) ;
#40164 = CARTESIAN_POINT('Ctrl Pts',(18.2573364685599,3.37352269437296,-323.307606043079)) ;
#40165 = CARTESIAN_POINT('Ctrl Pts',(18.2802336043302,3.24716023795198,-323.309249253836)) ;
#40166 = CARTESIAN_POINT('Ctrl Pts',(18.3213505008205,3.00601396478791,-323.312395933714)) ;
#40167 = CARTESIAN_POINT('Ctrl Pts',(18.3398070738416,2.89127663546369,-323.313897764518)) ;
#40168 = CARTESIAN_POINT('Ctrl Pts',(18.3862593058974,2.58413778391364,-323.317930746195)) ;
#40169 = CARTESIAN_POINT('Ctrl Pts',(18.4123119416186,2.39145732258099,-323.320474230439)) ;
#40170 = CARTESIAN_POINT('Ctrl Pts',(18.4772532420006,1.84687371282489,-323.327698343762)) ;
#40171 = CARTESIAN_POINT('Ctrl Pts',(18.5091097260421,1.49421755782957,-323.332419090114)) ;
#40172 = CARTESIAN_POINT('Ctrl Pts',(18.5617689159865,0.638885677969979,-323.343919950841)) ;
#40173 = CARTESIAN_POINT('Ctrl Pts',(18.5722638043924,0.135855972020733,-323.35072946396)) ;
#40174 = CARTESIAN_POINT('Ctrl Pts',(18.5599214427197,-0.488440993619338,
-323.359075417064)) ;
#40175 = CARTESIAN_POINT('Ctrl Pts',(18.5563279569996,-0.609878152566911,
-323.360693555459)) ;
#40176 = CARTESIAN_POINT('Ctrl Pts',(18.5494702386873,-0.783850857382472,
-323.363000534812)) ;
#40177 = CARTESIAN_POINT('Ctrl Pts',(18.5471741332696,-0.836420874962716,
-323.363696175323)) ;
#40178 = CARTESIAN_POINT('Ctrl Pts',(18.5446545937399,-0.88897997805457,-323.364389984898)) ;
#40179 = CARTESIAN_POINT('Origin',(0.,0.,-315.477129595899)) ;
#40180 = CARTESIAN_POINT('',(18.544654593745,-0.888979977948519,-325.159020379883)) ;
#40181 = CARTESIAN_POINT('',(18.544654593744,-0.888979977969434,-324.862668413757)) ;
#40182 = CARTESIAN_POINT('',(18.544654593745,-0.888979977948782,-315.477129595899)) ;
#40183 = CARTESIAN_POINT('Ctrl Pts',(18.544654593745,-0.888979977948194,-325.159020379883)) ;
#40184 = CARTESIAN_POINT('Ctrl Pts',(18.5446586219495,-0.888895947190053,
-325.159019247604)) ;
#40185 = CARTESIAN_POINT('Ctrl Pts',(18.5446626495217,-0.888811916393853,
-325.159018115291)) ;
#40186 = CARTESIAN_POINT('Ctrl Pts',(18.5501207282953,-0.774920754442528,
-325.157483483499)) ;
#40187 = CARTESIAN_POINT('Ctrl Pts',(18.5545270287366,-0.661065782942734,
-325.155951557284)) ;
#40188 = CARTESIAN_POINT('Ctrl Pts',(18.5668366567267,-0.243576615309611,
-325.15034869941)) ;
#40189 = CARTESIAN_POINT('Ctrl Pts',(18.568336752981,0.0601988172090561,-325.146299308515)) ;
#40190 = CARTESIAN_POINT('Ctrl Pts',(18.5605105695105,0.459437238522425,-325.141065491681)) ;
#40191 = CARTESIAN_POINT('Ctrl Pts',(18.5578993314717,0.554984340332674,-325.139819627603)) ;
#40192 = CARTESIAN_POINT('Ctrl Pts',(18.5522326295111,0.716616868973615,-325.137725830194)) ;
#40193 = CARTESIAN_POINT('Ctrl Pts',(18.5495615709723,0.782713761614237,-325.136873596225)) ;
#40194 = CARTESIAN_POINT('Ctrl Pts',(18.5427902246401,0.930670564738783,-325.134975234847)) ;
#40195 = CARTESIAN_POINT('Ctrl Pts',(18.5385010107146,1.01252027927148,-325.133931225173)) ;
#40196 = CARTESIAN_POINT('Ctrl Pts',(18.5225937283258,1.28192521596375,-325.130511636973)) ;
#40197 = CARTESIAN_POINT('Ctrl Pts',(18.5086701834537,1.46933282498183,-325.128159473866)) ;
#40198 = CARTESIAN_POINT('Ctrl Pts',(18.4644513987463,1.96295856367827,-325.122002126026)) ;
#40199 = CARTESIAN_POINT('Ctrl Pts',(18.4293845340087,2.26869080337882,-325.118226813985)) ;
#40200 = CARTESIAN_POINT('Ctrl Pts',(18.29520119118,3.22741616193632,-325.106365715861)) ;
#40201 = CARTESIAN_POINT('Ctrl Pts',(18.1688376500615,3.8760726501937,-325.09829193675)) ;
#40202 = CARTESIAN_POINT('Ctrl Pts',(17.9649544354914,4.68897527553325,-325.087755749685)) ;
#40203 = CARTESIAN_POINT('Ctrl Pts',(17.9192521112493,4.86070783313849,-325.08550709052)) ;
#40204 = CARTESIAN_POINT('Ctrl Pts',(17.8368299731006,5.15344323358092,-325.081630712099)) ;
#40205 = CARTESIAN_POINT('Ctrl Pts',(17.8013264295623,5.27477562989638,-325.080011206072)) ;
#40206 = CARTESIAN_POINT('Ctrl Pts',(17.7252528722859,5.52523549828796,-325.076640536377)) ;
#40207 = CARTESIAN_POINT('Ctrl Pts',(17.6845044116812,5.65430104833426,-325.074888245983)) ;
#40208 = CARTESIAN_POINT('Ctrl Pts',(17.5706100509652,6.00176698015689,-325.070128839152)) ;
#40209 = CARTESIAN_POINT('Ctrl Pts',(17.4948055253037,6.2192703569369,-325.067104263885)) ;
#40210 = CARTESIAN_POINT('Ctrl Pts',(17.3591704454147,6.58632068260151,-325.061926493004)) ;
#40211 = CARTESIAN_POINT('Ctrl Pts',(17.3014048055989,6.73660228565294,-325.059785319124)) ;
#40212 = CARTESIAN_POINT('Ctrl Pts',(17.021516369721,7.43739675538367,-325.049709254346)) ;
#40213 = CARTESIAN_POINT('Ctrl Pts',(16.7750281396525,7.97780161750594,-325.041661020433)) ;
#40214 = CARTESIAN_POINT('Ctrl Pts',(16.414161209679,8.67798828922514,-325.031113422437)) ;
#40215 = CARTESIAN_POINT('Ctrl Pts',(16.3225460237165,8.84910506472168,-325.028527074016)) ;
#40216 = CARTESIAN_POINT('Ctrl Pts',(16.1641261509983,9.13416435549494,-325.024221078249)) ;
#40217 = CARTESIAN_POINT('Ctrl Pts',(16.0987581958567,9.24888735681717,-325.0224888568)) ;
#40218 = CARTESIAN_POINT('Ctrl Pts',(15.9956662993177,9.42541240915578,-325.019830258873)) ;
#40219 = CARTESIAN_POINT('Ctrl Pts',(15.958795300298,9.48770741661333,-325.018893380711)) ;
#40220 = CARTESIAN_POINT('Ctrl Pts',(15.885552200875,9.60981953095132,-325.017060776327)) ;
#40221 = CARTESIAN_POINT('Ctrl Pts',(15.8492042401821,9.66964968866288,-325.016164782777)) ;
#40222 = CARTESIAN_POINT('Ctrl Pts',(15.7497347874064,9.83131260141312,-325.013747138673)) ;
#40223 = CARTESIAN_POINT('Ctrl Pts',(15.6859645031338,9.93274237134299,-325.012233891678)) ;
#40224 = CARTESIAN_POINT('Ctrl Pts',(15.5365574878551,10.1653539475783,-325.008764344738)) ;
#40225 = CARTESIAN_POINT('Ctrl Pts',(15.4502332000911,10.2960834118683,-325.006815022515)) ;
#40226 = CARTESIAN_POINT('Ctrl Pts',(15.1239853337283,10.7768092890646,-324.999623897708)) ;
#40227 = CARTESIAN_POINT('Ctrl Pts',(14.8737389543412,11.119642137153,-324.994446927006)) ;
#40228 = CARTESIAN_POINT('Ctrl Pts',(14.5814632262791,11.4925138398334,-324.988638362559)) ;
#40229 = CARTESIAN_POINT('Ctrl Pts',(14.5508047722516,11.5313062858068,-324.988031877881)) ;
#40230 = CARTESIAN_POINT('Ctrl Pts',(14.2277943107438,11.9366752607788,-324.981669927358)) ;
#40231 = CARTESIAN_POINT('Ctrl Pts',(13.9218109530843,12.292173348847,-324.975875796179)) ;
#40232 = CARTESIAN_POINT('Ctrl Pts',(13.4999940366237,12.7462713621953,-324.968069734093)) ;
#40233 = CARTESIAN_POINT('Ctrl Pts',(13.3959442022042,12.85558055762,-324.96615832901)) ;
#40234 = CARTESIAN_POINT('Ctrl Pts',(13.2021201219743,13.0542932135564,-324.962620763335)) ;
#40235 = CARTESIAN_POINT('Ctrl Pts',(13.1127410878124,13.1440696943821,-324.960998181207)) ;
#40236 = CARTESIAN_POINT('Ctrl Pts',(12.9264000006235,13.3274469657149,-324.957632171361)) ;
#40237 = CARTESIAN_POINT('Ctrl Pts',(12.8293234681424,13.4209209402564,-324.955887733289)) ;
#40238 = CARTESIAN_POINT('Ctrl Pts',(12.5660212408701,13.6689844007998,-324.951180109024)) ;
#40239 = CARTESIAN_POINT('Ctrl Pts',(12.3979640630761,13.8215958258115,-324.948200138307)) ;
#40240 = CARTESIAN_POINT('Ctrl Pts',(12.1086208105135,14.0748219111802,-324.943114343732)) ;
#40241 = CARTESIAN_POINT('Ctrl Pts',(11.9887752409198,14.1770440468635,-324.941020420206)) ;
#40242 = CARTESIAN_POINT('Ctrl Pts',(11.4322344408434,14.639640583419,-324.931361711411)) ;
#40243 = CARTESIAN_POINT('Ctrl Pts',(10.9804982276953,14.9814457691134,-324.923693041859)) ;
#40244 = CARTESIAN_POINT('Ctrl Pts',(10.2658631159338,15.4724621671584,-324.912063395682)) ;
#40245 = CARTESIAN_POINT('Ctrl Pts',(10.0137676923007,15.636799170095,-324.90805274844)) ;
#40246 = CARTESIAN_POINT('Ctrl Pts',(9.67668035855467,15.8450448459758,-324.902859757055)) ;
#40247 = CARTESIAN_POINT('Ctrl Pts',(9.59518605848538,15.8945271547578,-324.901617118573)) ;
#40248 = CARTESIAN_POINT('Ctrl Pts',(9.45652785951009,15.9772636285781,-324.899526844709)) ;
#40249 = CARTESIAN_POINT('Ctrl Pts',(9.39956094901987,16.0108440193366,-324.898674947478)) ;
#40250 = CARTESIAN_POINT('Ctrl Pts',(9.27145091723238,16.0854418908666,-324.896774935489)) ;
#40251 = CARTESIAN_POINT('Ctrl Pts',(9.20021275689051,16.1262930702718,-324.895728965662)) ;
#40252 = CARTESIAN_POINT('Ctrl Pts',(8.96415073459125,16.2595883453578,-324.892294088395)) ;
#40253 = CARTESIAN_POINT('Ctrl Pts',(8.79818623455953,16.349988708402,-324.889928880841)) ;
#40254 = CARTESIAN_POINT('Ctrl Pts',(8.35587246372056,16.5822304693836,-324.88372289411)) ;
#40255 = CARTESIAN_POINT('Ctrl Pts',(8.07729402747451,16.7196977740968,-324.879912538078)) ;
#40256 = CARTESIAN_POINT('Ctrl Pts',(7.21584002410261,17.1182338247516,-324.868283524226)) ;
#40257 = CARTESIAN_POINT('Ctrl Pts',(6.62283465587795,17.3562765795629,-324.860475030763)) ;
#40258 = CARTESIAN_POINT('Ctrl Pts',(5.843287620965,17.6234188149593,-324.85012842599)) ;
#40259 = CARTESIAN_POINT('Ctrl Pts',(5.6669368494997,17.6809142166644,-324.847783905352)) ;
#40260 = CARTESIAN_POINT('Ctrl Pts',(5.36906210827938,17.7731154764182,-324.843812434282)) ;
#40261 = CARTESIAN_POINT('Ctrl Pts',(5.2479916861208,17.809240434949,-324.842195159287)) ;
#40262 = CARTESIAN_POINT('Ctrl Pts',(4.99901978426692,17.8807692874505,-324.838862056494)) ;
#40263 = CARTESIAN_POINT('Ctrl Pts',(4.8710884173046,17.9160432764322,-324.837145458801)) ;
#40264 = CARTESIAN_POINT('Ctrl Pts',(4.53464529951934,18.0049393296381,-324.832620341877)) ;
#40265 = CARTESIAN_POINT('Ctrl Pts',(4.32556006620695,18.0563113098255,-324.829797331651)) ;
#40266 = CARTESIAN_POINT('Ctrl Pts',(3.84909137267631,18.1646279571872,-324.823343326407)) ;
#40267 = CARTESIAN_POINT('Ctrl Pts',(3.58124846766905,18.2193268871801,-324.819700280012)) ;
#40268 = CARTESIAN_POINT('Ctrl Pts',(2.96728423410764,18.3306483838568,-324.811337941607)) ;
#40269 = CARTESIAN_POINT('Ctrl Pts',(2.62056955508137,18.3834180929022,-324.806606725256)) ;
#40270 = CARTESIAN_POINT('Ctrl Pts',(2.17865847696782,18.4379201665148,-324.800613540854)) ;
#40271 = CARTESIAN_POINT('Ctrl Pts',(2.08466029269882,18.4487843582694,-324.799340964799)) ;
#40272 = CARTESIAN_POINT('Ctrl Pts',(1.67065558293275,18.4934300026517,-324.793750136042)) ;
#40273 = CARTESIAN_POINT('Ctrl Pts',(1.34988447362793,18.5196073389262,-324.789454433463)) ;
#40274 = CARTESIAN_POINT('Ctrl Pts',(0.93085666052038,18.5428581263998,-324.783950618395)) ;
#40275 = CARTESIAN_POINT('Ctrl Pts',(0.833076740527781,18.5475083179144,-324.782674022182)) ;
#40276 = CARTESIAN_POINT('Ctrl Pts',(0.668920596993591,18.5540144731446,-324.780546341371)) ;
#40277 = CARTESIAN_POINT('Ctrl Pts',(0.602563015113682,18.5562880362072,-324.77969058647)) ;
#40278 = CARTESIAN_POINT('Ctrl Pts',(0.455677815184263,18.5605319284449,-324.77780645371)) ;
#40279 = CARTESIAN_POINT('Ctrl Pts',(0.375146844164681,18.562334244577,-324.776779948186)) ;
#40280 = CARTESIAN_POINT('Ctrl Pts',(0.115963066857499,18.5664475204769,-324.773493748674)) ;
#40281 = CARTESIAN_POINT('Ctrl Pts',(-0.0627124239954405,18.5667037546687,
-324.77125506188)) ;
#40282 = CARTESIAN_POINT('Ctrl Pts',(-0.524607960403906,18.5606984412463,
-324.765509764544)) ;
#40283 = CARTESIAN_POINT('Ctrl Pts',(-0.807731001154924,18.5505339863079,
-324.762028544782)) ;
#40284 = CARTESIAN_POINT('Ctrl Pts',(-1.79941751467278,18.492184425519,-324.749849941773)) ;
#40285 = CARTESIAN_POINT('Ctrl Pts',(-2.50534814252148,18.4098348306686,-324.741184784979)) ;
#40286 = CARTESIAN_POINT('Ctrl Pts',(-3.35796935287776,18.2604139060853,-324.730292626257)) ;
#40287 = CARTESIAN_POINT('Ctrl Pts',(-3.51077446870182,18.2316520571646,-324.728324859711)) ;
#40288 = CARTESIAN_POINT('Ctrl Pts',(-3.78711653819901,18.1760343587453,-324.724734777685)) ;
#40289 = CARTESIAN_POINT('Ctrl Pts',(-3.91077492934762,18.1498296433566,-324.723116796434)) ;
#40290 = CARTESIAN_POINT('Ctrl Pts',(-4.16359234592587,18.0935508446481,-324.719784280077)) ;
#40291 = CARTESIAN_POINT('Ctrl Pts',(-4.29271619370536,18.0633515995515,-324.718068996332)) ;
#40292 = CARTESIAN_POINT('Ctrl Pts',(-4.63006398011498,17.9806317729402,-324.713552471857)) ;
#40293 = CARTESIAN_POINT('Ctrl Pts',(-4.83771938331841,17.9258774494145,-324.710736845017)) ;
#40294 = CARTESIAN_POINT('Ctrl Pts',(-5.30644125997606,17.7935474734949,-324.70430417337)) ;
#40295 = CARTESIAN_POINT('Ctrl Pts',(-5.56684477106812,17.7138050521781,-324.700675205138)) ;
#40296 = CARTESIAN_POINT('Ctrl Pts',(-6.15960132947834,17.5179250619453,-324.692309396975)) ;
#40297 = CARTESIAN_POINT('Ctrl Pts',(-6.49059479770754,17.3980046514237,-324.687560134686)) ;
#40298 = CARTESIAN_POINT('Ctrl Pts',(-6.91427674802556,17.2307282300353,-324.681428923802)) ;
#40299 = CARTESIAN_POINT('Ctrl Pts',(-7.01025532549145,17.1919032851968,-324.680036604406)) ;
#40300 = CARTESIAN_POINT('Ctrl Pts',(-7.39746459177869,17.0314889076669,-324.674410982087)) ;
#40301 = CARTESIAN_POINT('Ctrl Pts',(-7.68589844254006,16.9032855576917,-324.670199910596)) ;
#40302 = CARTESIAN_POINT('Ctrl Pts',(-8.05850070316169,16.7261612036311,-324.66479060758)) ;
#40303 = CARTESIAN_POINT('Ctrl Pts',(-8.14574970358435,16.6838444010591,-324.663526275409)) ;
#40304 = CARTESIAN_POINT('Ctrl Pts',(-8.29208214970525,16.6114498993797,-324.66141218093)) ;
#40305 = CARTESIAN_POINT('Ctrl Pts',(-8.35134317255403,16.5817357772064,-324.66055789588)) ;
#40306 = CARTESIAN_POINT('Ctrl Pts',(-8.4827396236188,16.5149690901555,-324.658668396748)) ;
#40307 = CARTESIAN_POINT('Ctrl Pts',(-8.55479385902869,16.4777600912521,-324.657635150079)) ;
#40308 = CARTESIAN_POINT('Ctrl Pts',(-8.78791755769494,16.3554331101089,-324.654298230134)) ;
#40309 = CARTESIAN_POINT('Ctrl Pts',(-8.94797872598171,16.2684161536449,-324.652016464265)) ;
#40310 = CARTESIAN_POINT('Ctrl Pts',(-9.24104346340062,16.1034583096805,-324.647835494054)) ;
#40311 = CARTESIAN_POINT('Ctrl Pts',(-9.37440697152772,16.0261894357702,-324.645931662362)) ;
#40312 = CARTESIAN_POINT('Ctrl Pts',(-10.2269894113764,15.5179315783491,-324.633713602122)) ;
#40313 = CARTESIAN_POINT('Ctrl Pts',(-10.9172736991398,15.0403009270707,-324.623554436759)) ;
#40314 = CARTESIAN_POINT('Ctrl Pts',(-11.6932872480977,14.42169310885,-324.611063023564)) ;
#40315 = CARTESIAN_POINT('Ctrl Pts',(-11.81246712061,14.3242388707555,-324.609114186389)) ;
#40316 = CARTESIAN_POINT('Ctrl Pts',(-12.0270137055586,14.1443039231261,-324.605547207702)) ;
#40317 = CARTESIAN_POINT('Ctrl Pts',(-12.1227786507147,14.0623123943508,-324.603933199599)) ;
#40318 = CARTESIAN_POINT('Ctrl Pts',(-12.3179728500818,13.8917161912039,-324.600597109432)) ;
#40319 = CARTESIAN_POINT('Ctrl Pts',(-12.4172987861137,13.8030041898748,-324.59887415615)) ;
#40320 = CARTESIAN_POINT('Ctrl Pts',(-12.6766463545541,13.5663053169609,-324.594307467427)) ;
#40321 = CARTESIAN_POINT('Ctrl Pts',(-12.8350311334094,13.416556126447,-324.591448729686)) ;
#40322 = CARTESIAN_POINT('Ctrl Pts',(-13.1896112100128,13.0692823101806,-324.584891052363)) ;
#40323 = CARTESIAN_POINT('Ctrl Pts',(-13.3840742423691,12.8700637225103,-324.581179429134)) ;
#40324 = CARTESIAN_POINT('Ctrl Pts',(-13.855668897194,12.3646838807002,-324.571912172819)) ;
#40325 = CARTESIAN_POINT('Ctrl Pts',(-14.1272057209714,12.0535067977024,-324.566333177034)) ;
#40326 = CARTESIAN_POINT('Ctrl Pts',(-14.604387175395,11.4683674374813,-324.556188007992)) ;
#40327 = CARTESIAN_POINT('Ctrl Pts',(-14.8132615854392,11.1972701353975,-324.55161468909)) ;
#40328 = CARTESIAN_POINT('Ctrl Pts',(-15.0726602483096,10.8406264039178,-324.545829816827)) ;
#40329 = CARTESIAN_POINT('Ctrl Pts',(-15.1301563148155,10.760234092299,-324.544540615264)) ;
#40330 = CARTESIAN_POINT('Ctrl Pts',(-15.2252644732489,10.6249820955699,-324.542398888305)) ;
#40331 = CARTESIAN_POINT('Ctrl Pts',(-15.2632285907929,10.5703725494005,-324.541541540812)) ;
#40332 = CARTESIAN_POINT('Ctrl Pts',(-15.3462192787946,10.4496151097457,-324.539662526114)) ;
#40333 = CARTESIAN_POINT('Ctrl Pts',(-15.3911132212989,10.3833778669287,-324.538642637158)) ;
#40334 = CARTESIAN_POINT('Ctrl Pts',(-15.5329792775945,10.1711247076182,-324.535405471684)) ;
#40335 = CARTESIAN_POINT('Ctrl Pts',(-15.6283125154668,10.0240246988668,-324.533208350041)) ;
#40336 = CARTESIAN_POINT('Ctrl Pts',(-15.8676704537504,9.64297658818647,-324.527609305558)) ;
#40337 = CARTESIAN_POINT('Ctrl Pts',(-16.0086116741577,9.4071417422158,-324.524231262496)) ;
#40338 = CARTESIAN_POINT('Ctrl Pts',(-16.5035615075361,8.53559171872297,-324.511940314212)) ;
#40339 = CARTESIAN_POINT('Ctrl Pts',(-16.825354108921,7.88234276124894,-324.503068740249)) ;
#40340 = CARTESIAN_POINT('Ctrl Pts',(-17.1677953807705,7.07000797839121,-324.491972609439)) ;
#40341 = CARTESIAN_POINT('Ctrl Pts',(-17.2258431692104,6.9273759873389,-324.490023281795)) ;
#40342 = CARTESIAN_POINT('Ctrl Pts',(-17.3281779123183,6.66668167429108,-324.486455705793)) ;
#40343 = CARTESIAN_POINT('Ctrl Pts',(-17.3730493571668,6.54885870116318,-324.484841596037)) ;
#40344 = CARTESIAN_POINT('Ctrl Pts',(-17.4628376176707,6.30567460135265,-324.481505606007)) ;
#40345 = CARTESIAN_POINT('Ctrl Pts',(-17.5076128291577,6.1802688291551,-324.479782857746)) ;
#40346 = CARTESIAN_POINT('Ctrl Pts',(-17.622081813725,5.84843550227691,-324.475217510485)) ;
#40347 = CARTESIAN_POINT('Ctrl Pts',(-17.689497652719,5.64124434915855,-324.472359925784)) ;
#40348 = CARTESIAN_POINT('Ctrl Pts',(-17.8346597107566,5.16689522803652,-324.465805605824)) ;
#40349 = CARTESIAN_POINT('Ctrl Pts',(-17.9100784961249,4.89907962085505,-324.462096207668)) ;
#40350 = CARTESIAN_POINT('Ctrl Pts',(-18.0824065841646,4.22983890984074,-324.452831294259)) ;
#40351 = CARTESIAN_POINT('Ctrl Pts',(-18.1719964825838,3.82668374190341,-324.447252366751)) ;
#40352 = CARTESIAN_POINT('Ctrl Pts',(-18.311232802637,3.08395223328582,-324.437098674596)) ;
#40353 = CARTESIAN_POINT('Ctrl Pts',(-18.3650514273055,2.74534060542625,-324.432516874476)) ;
#40354 = CARTESIAN_POINT('Ctrl Pts',(-18.4222514714943,2.30757239692762,-324.426725803979)) ;
#40355 = CARTESIAN_POINT('Ctrl Pts',(-18.4342577468173,2.20961105430747,-324.425438500317)) ;
#40356 = CARTESIAN_POINT('Ctrl Pts',(-18.4530446205108,2.04549865174853,-324.423298893235)) ;
#40357 = CARTESIAN_POINT('Ctrl Pts',(-18.4602519435972,1.97939857430754,-324.422441790582)) ;
#40358 = CARTESIAN_POINT('Ctrl Pts',(-18.4753580671253,1.83359182870452,-324.420562029993)) ;
#40359 = CARTESIAN_POINT('Ctrl Pts',(-18.4830964566858,1.75387003489079,-324.419541164246)) ;
#40360 = CARTESIAN_POINT('Ctrl Pts',(-18.5061686803337,1.49903901159186,-324.416296805358)) ;
#40361 = CARTESIAN_POINT('Ctrl Pts',(-18.5195317048159,1.32376085735172,-324.414093591029)) ;
#40362 = CARTESIAN_POINT('Ctrl Pts',(-18.5474714206386,0.87289823368202,-324.408473257293)) ;
#40363 = CARTESIAN_POINT('Ctrl Pts',(-18.5583965602283,0.597130576764395,
-324.405080234962)) ;
#40364 = CARTESIAN_POINT('Ctrl Pts',(-18.5757186892474,-0.40390227118912,
-324.392803331715)) ;
#40365 = CARTESIAN_POINT('Ctrl Pts',(-18.5457678542622,-1.12913966912419,
-324.383959403295)) ;
#40366 = CARTESIAN_POINT('Ctrl Pts',(-18.4581081514156,-2.00412035107501,
-324.37289130985)) ;
#40367 = CARTESIAN_POINT('Ctrl Pts',(-18.4408346634734,-2.15728341550672,
-324.370940228323)) ;
#40368 = CARTESIAN_POINT('Ctrl Pts',(-18.405964400338,-2.43533910379303,-324.36737051579)) ;
#40369 = CARTESIAN_POINT('Ctrl Pts',(-18.3889982929313,-2.56030150306097,
-324.365756041947)) ;
#40370 = CARTESIAN_POINT('Ctrl Pts',(-18.3515107117888,-2.8167836395877,-324.362420406641)) ;
#40371 = CARTESIAN_POINT('Ctrl Pts',(-18.3308452982443,-2.94827510013788,
-324.36069838872)) ;
#40372 = CARTESIAN_POINT('Ctrl Pts',(-18.2726810437337,-3.29407944234658,
-324.356137819817)) ;
#40373 = CARTESIAN_POINT('Ctrl Pts',(-18.2328260110372,-3.50797481310281,
-324.353284342207)) ;
#40374 = CARTESIAN_POINT('Ctrl Pts',(-18.1595860851892,-3.86597918388449,
-324.34845636185)) ;
#40375 = CARTESIAN_POINT('Ctrl Pts',(-18.1282216218701,-4.01047909801559,
-324.346493371257)) ;
#40376 = CARTESIAN_POINT('Ctrl Pts',(-17.9834342466204,-4.64109434134236,
-324.337869688728)) ;
#40377 = CARTESIAN_POINT('Ctrl Pts',(-17.8521592930299,-5.12289673776954,
-324.331126311901)) ;
#40378 = CARTESIAN_POINT('Ctrl Pts',(-17.6824483477044,-5.65946690870653,
-324.323555516011)) ;
#40379 = CARTESIAN_POINT('Ctrl Pts',(-17.6629552171256,-5.72001383393836,
-324.322700438641)) ;
#40380 = CARTESIAN_POINT('Ctrl Pts',(-17.5411251877826,-6.09186414830413,
-324.31744598544)) ;
#40381 = CARTESIAN_POINT('Ctrl Pts',(-17.4308721932401,-6.40051380852478,
-324.313070674569)) ;
#40382 = CARTESIAN_POINT('Ctrl Pts',(-17.2775081934495,-6.79644019426209,
-324.307503707819)) ;
#40383 = CARTESIAN_POINT('Ctrl Pts',(-17.2418013121382,-6.88652134542935,
-324.306240303337)) ;
#40384 = CARTESIAN_POINT('Ctrl Pts',(-17.1804835685987,-7.03774661996558,
-324.304127233201)) ;
#40385 = CARTESIAN_POINT('Ctrl Pts',(-17.1552475105334,-7.09904050021906,
-324.303273055965)) ;
#40386 = CARTESIAN_POINT('Ctrl Pts',(-17.0983926158861,-7.23505717728028,
-324.30138313462)) ;
#40387 = CARTESIAN_POINT('Ctrl Pts',(-17.0666111729221,-7.30971035693333,
-324.300349365266)) ;
#40388 = CARTESIAN_POINT('Ctrl Pts',(-16.9617763463394,-7.55155153433974,
-324.29700847943)) ;
#40389 = CARTESIAN_POINT('Ctrl Pts',(-16.8867475665012,-7.71787174250962,
-324.294723341542)) ;
#40390 = CARTESIAN_POINT('Ctrl Pts',(-16.7436822581327,-8.02293411564987,
-324.290534516993)) ;
#40391 = CARTESIAN_POINT('Ctrl Pts',(-16.676341621403,-8.16198490484776,-324.28862621689)) ;
#40392 = CARTESIAN_POINT('Ctrl Pts',(-16.2326531562394,-9.04973148786076,
-324.276410256749)) ;
#40393 = CARTESIAN_POINT('Ctrl Pts',(-15.8077181648226,-9.77306088105379,
-324.266256755699)) ;
#40394 = CARTESIAN_POINT('Ctrl Pts',(-15.2486580630856,-10.5922894917194,
-324.253772645921)) ;
#40395 = CARTESIAN_POINT('Ctrl Pts',(-15.1603597817781,-10.7182862715112,
-324.251824985247)) ;
#40396 = CARTESIAN_POINT('Ctrl Pts',(-14.9968905508428,-10.9454858624436,
-324.248259439054)) ;
#40397 = CARTESIAN_POINT('Ctrl Pts',(-14.9222353598274,-11.047048419009,-324.2466456745)) ;
#40398 = CARTESIAN_POINT('Ctrl Pts',(-14.7665680993526,-11.2543640488365,
-324.243309342443)) ;
#40399 = CARTESIAN_POINT('Ctrl Pts',(-14.6854403786343,-11.3600213203631,
-324.241585895958)) ;
#40400 = CARTESIAN_POINT('Ctrl Pts',(-14.4684654485283,-11.6363912162853,
-324.237015980035)) ;
#40401 = CARTESIAN_POINT('Ctrl Pts',(-14.3307343580113,-11.8055980564885,
-324.234154468334)) ;
#40402 = CARTESIAN_POINT('Ctrl Pts',(-14.0102986229613,-12.1853902264077,
-324.227588710751)) ;
#40403 = CARTESIAN_POINT('Ctrl Pts',(-13.8257685387155,-12.394366718756,-324.223871731209)) ;
#40404 = CARTESIAN_POINT('Ctrl Pts',(-13.3564125061291,-12.9023726681295,
-324.214598831097)) ;
#40405 = CARTESIAN_POINT('Ctrl Pts',(-13.0661829667452,-13.1962054292246,
-324.209019666932)) ;
#40406 = CARTESIAN_POINT('Ctrl Pts',(-12.5197147569701,-13.7137403820609,
-324.198907011125)) ;
#40407 = CARTESIAN_POINT('Ctrl Pts',(-12.266663020355,-13.9405492009657,-324.194365985552)) ;
#40408 = CARTESIAN_POINT('Ctrl Pts',(-11.9315651479546,-14.2247029034452,
-324.188601636262)) ;
#40409 = CARTESIAN_POINT('Ctrl Pts',(-11.8550827840547,-14.2885069827735,
-324.1873022458)) ;
#40410 = CARTESIAN_POINT('Ctrl Pts',(-11.726604724349,-14.3939458516107,-324.185149109122)) ;
#40411 = CARTESIAN_POINT('Ctrl Pts',(-11.6748917780134,-14.4359217769132,
-324.184290417989)) ;
#40412 = CARTESIAN_POINT('Ctrl Pts',(-11.5608798022477,-14.5274531238544,
-324.182415264015)) ;
#40413 = CARTESIAN_POINT('Ctrl Pts',(-11.4984857923705,-14.5768878905526,
-324.181400505901)) ;
#40414 = CARTESIAN_POINT('Ctrl Pts',(-11.2997286626254,-14.7322929507531,
-324.178200874231)) ;
#40415 = CARTESIAN_POINT('Ctrl Pts',(-11.1622037943643,-14.8367627894388,
-324.176035514997)) ;
#40416 = CARTESIAN_POINT('Ctrl Pts',(-10.80735536776,-15.0985943436397,-324.170546648979)) ;
#40417 = CARTESIAN_POINT('Ctrl Pts',(-10.5880415394942,-15.2531917289847,
-324.167245911931)) ;
#40418 = CARTESIAN_POINT('Ctrl Pts',(-9.74330876575939,-15.8216556176582,
-324.154756876079)) ;
#40419 = CARTESIAN_POINT('Ctrl Pts',(-9.0963673782391,-16.202251475044,-324.145618227089)) ;
#40420 = CARTESIAN_POINT('Ctrl Pts',(-8.28189350385132,-16.6172108619708,
-324.13410222967)) ;
#40421 = CARTESIAN_POINT('Ctrl Pts',(-8.13461693476493,-16.6898011987631,
-324.132020975683)) ;
#40422 = CARTESIAN_POINT('Ctrl Pts',(-7.87353097874972,-16.8142094815833,
-324.128330219968)) ;
#40423 = CARTESIAN_POINT('Ctrl Pts',(-7.76012460251026,-16.8668490437766,
-324.126726717366)) ;
#40424 = CARTESIAN_POINT('Ctrl Pts',(-7.5189344068974,-16.975854267733,-324.123314766404)) ;
#40425 = CARTESIAN_POINT('Ctrl Pts',(-7.39102875179493,-17.0319316770664,
-324.121504393135)) ;
#40426 = CARTESIAN_POINT('Ctrl Pts',(-7.02733059118297,-17.1865186031997,
-324.116353584985)) ;
#40427 = CARTESIAN_POINT('Ctrl Pts',(-6.79012029602376,-17.2816105409755,
-324.112990236013)) ;
#40428 = CARTESIAN_POINT('Ctrl Pts',(-6.37425972290613,-17.4384345961324,
-324.107093703077)) ;
#40429 = CARTESIAN_POINT('Ctrl Pts',(-6.19648916873253,-17.5023915518779,
-324.104573148269)) ;
#40430 = CARTESIAN_POINT('Ctrl Pts',(-5.67930316437138,-17.6795934953287,
-324.097250463925)) ;
#40431 = CARTESIAN_POINT('Ctrl Pts',(-5.33755120228227,-17.7857543381615,
-324.092423216182)) ;
#40432 = CARTESIAN_POINT('Ctrl Pts',(-4.94556263289974,-17.8952041029779,
-324.086944612391)) ;
#40433 = CARTESIAN_POINT('Ctrl Pts',(-4.89812668367064,-17.9082459954837,
-324.086282618446)) ;
#40434 = CARTESIAN_POINT('Ctrl Pts',(-4.51983041772977,-18.0106380850315,
-324.08101224688)) ;
#40435 = CARTESIAN_POINT('Ctrl Pts',(-4.18660496775709,-18.0910002714573,
-324.076422981647)) ;
#40436 = CARTESIAN_POINT('Ctrl Pts',(-3.74022423692884,-18.1856571350349,
-324.070418017646)) ;
#40437 = CARTESIAN_POINT('Ctrl Pts',(-3.62888810184296,-18.2082007342818,
-324.068932093925)) ;
#40438 = CARTESIAN_POINT('Ctrl Pts',(-3.45639137039489,-18.2414832906194,
-324.066651806675)) ;
#40439 = CARTESIAN_POINT('Ctrl Pts',(-3.39537207382562,-18.2529395561836,
-324.065849400192)) ;
#40440 = CARTESIAN_POINT('Ctrl Pts',(-3.26406129542807,-18.2769116822503,
-324.064132607734)) ;
#40441 = CARTESIAN_POINT('Ctrl Pts',(-3.19375273946748,-18.2893285890387,
-324.063219475209)) ;
#40442 = CARTESIAN_POINT('Ctrl Pts',(-2.99824571202545,-18.3226945408502,
-324.060695234254)) ;
#40443 = CARTESIAN_POINT('Ctrl Pts',(-2.87290127967153,-18.3427656285621,
-324.059093811185)) ;
#40444 = CARTESIAN_POINT('Ctrl Pts',(-2.57935373390492,-18.3866879020212,
-324.055373824097)) ;
#40445 = CARTESIAN_POINT('Ctrl Pts',(-2.41100939119533,-18.409519046888,-324.053263712518)) ;
#40446 = CARTESIAN_POINT('Ctrl Pts',(-1.73937492663051,-18.4912365486306,
-324.044903407833)) ;
#40447 = CARTESIAN_POINT('Ctrl Pts',(-1.2340795514919,-18.531818669057,-324.038737813985)) ;
#40448 = CARTESIAN_POINT('Ctrl Pts',(-0.356523487429989,-18.5662440326999,
-324.027938598878)) ;
#40449 = CARTESIAN_POINT('Ctrl Pts',(0.0150637715096853,-18.5696607071013,
-324.023339099343)) ;
#40450 = CARTESIAN_POINT('Ctrl Pts',(0.570407863445169,-18.5580971612075,
-324.016363096674)) ;
#40451 = CARTESIAN_POINT('Ctrl Pts',(0.75424625917996,-18.5515349177353,-324.014037447566)) ;
#40452 = CARTESIAN_POINT('Ctrl Pts',(1.06389874598875,-18.5358711931867,-324.010087938392)) ;
#40453 = CARTESIAN_POINT('Ctrl Pts',(1.18977267314184,-18.5282174632479,-324.008473493907)) ;
#40454 = CARTESIAN_POINT('Ctrl Pts',(1.44833023345666,-18.5098502469707,-324.005137830225)) ;
#40455 = CARTESIAN_POINT('Ctrl Pts',(1.5809963300354,-18.4989909771302,-324.003415753645)) ;
#40456 = CARTESIAN_POINT('Ctrl Pts',(1.9301902670985,-18.4666241673015,-323.998854800968)) ;
#40457 = CARTESIAN_POINT('Ctrl Pts',(2.14647637078742,-18.4427351966224,-323.996000993502)) ;
#40458 = CARTESIAN_POINT('Ctrl Pts',(2.63769967944871,-18.3797208149829,-323.989457666467)) ;
#40459 = CARTESIAN_POINT('Ctrl Pts',(2.91227948003948,-18.3382175971565,-323.985755551813)) ;
#40460 = CARTESIAN_POINT('Ctrl Pts',(3.59256440275971,-18.2197265839976,-323.976498301065)) ;
#40461 = CARTESIAN_POINT('Ctrl Pts',(3.99682786182519,-18.1353335334041,-323.970919590183)) ;
#40462 = CARTESIAN_POINT('Ctrl Pts',(4.73242512880404,-17.9559790356222,-323.960745712935)) ;
#40463 = CARTESIAN_POINT('Ctrl Pts',(5.06457753498572,-17.8651360466682,-323.95614379169)) ;
#40464 = CARTESIAN_POINT('Ctrl Pts',(5.48825912435923,-17.7364938086253,-323.950336057502)) ;
#40465 = CARTESIAN_POINT('Ctrl Pts',(5.58227728303499,-17.7071279776248,-323.949051375214)) ;
#40466 = CARTESIAN_POINT('Ctrl Pts',(5.73934250951164,-17.6566946198847,-323.946914693206)) ;
#40467 = CARTESIAN_POINT('Ctrl Pts',(5.80251807256303,-17.6360341742374,-323.946057925829)) ;
#40468 = CARTESIAN_POINT('Ctrl Pts',(5.94167881458699,-17.5896954250417,-323.944177120832)) ;
#40469 = CARTESIAN_POINT('Ctrl Pts',(6.01761114965898,-17.5638631387484,-323.943154894784)) ;
#40470 = CARTESIAN_POINT('Ctrl Pts',(6.26006913357981,-17.4796217256306,-323.939900492261)) ;
#40471 = CARTESIAN_POINT('Ctrl Pts',(6.42593054189615,-17.4193300126884,-323.937688768271)) ;
#40472 = CARTESIAN_POINT('Ctrl Pts',(6.85051227254076,-17.258102266702,-323.932038615105)) ;
#40473 = CARTESIAN_POINT('Ctrl Pts',(7.1078731598804,-17.153709563211,-323.928624588892)) ;
#40474 = CARTESIAN_POINT('Ctrl Pts',(8.02566353876108,-16.7572258646357,-323.916365743075)) ;
#40475 = CARTESIAN_POINT('Ctrl Pts',(8.67126197135678,-16.4324407654209,-323.907558988817)) ;
#40476 = CARTESIAN_POINT('Ctrl Pts',(9.42984617922406,-15.9936332031631,-323.896529035393)) ;
#40477 = CARTESIAN_POINT('Ctrl Pts',(9.56242512126461,-15.9147204722667,-323.894576072639)) ;
#40478 = CARTESIAN_POINT('Ctrl Pts',(9.80158371768117,-15.7683026041225,-323.891004067443)) ;
#40479 = CARTESIAN_POINT('Ctrl Pts',(9.90848837761735,-15.7013460699236,-323.889389202079)) ;
#40480 = CARTESIAN_POINT('Ctrl Pts',(10.1267311247918,-15.5615396700233,-323.886053941443)) ;
#40481 = CARTESIAN_POINT('Ctrl Pts',(10.2379851807161,-15.4885719016366,-323.884332702041)) ;
#40482 = CARTESIAN_POINT('Ctrl Pts',(10.5288040314402,-15.2933310829978,-323.879777226237)) ;
#40483 = CARTESIAN_POINT('Ctrl Pts',(10.7070235180935,-15.1690915044497,-323.876928126078)) ;
#40484 = CARTESIAN_POINT('Ctrl Pts',(11.4262440415811,-14.6487204933647,-323.865199757429)) ;
#40485 = CARTESIAN_POINT('Ctrl Pts',(11.9477755915366,-14.226549742773,-323.85613153917)) ;
#40486 = CARTESIAN_POINT('Ctrl Pts',(12.6944750198875,-13.5520306840359,-323.842602310485)) ;
#40487 = CARTESIAN_POINT('Ctrl Pts',(12.9374764823871,-13.3202452934011,-323.838107943541)) ;
#40488 = CARTESIAN_POINT('Ctrl Pts',(13.2537666821861,-13.0017292901879,-323.832201286496)) ;
#40489 = CARTESIAN_POINT('Ctrl Pts',(13.3327393016974,-12.9207336700945,-323.830721657337)) ;
#40490 = CARTESIAN_POINT('Ctrl Pts',(13.4538467041377,-12.7942312428942,-323.828448641825)) ;
#40491 = CARTESIAN_POINT('Ctrl Pts',(13.4965019630739,-12.7492266044238,-323.827647292065)) ;
#40492 = CARTESIAN_POINT('Ctrl Pts',(13.5805326517058,-12.6596733233988,-323.826067901992)) ;
#40493 = CARTESIAN_POINT('Ctrl Pts',(13.6219163044653,-12.6151334501198,-323.825289707207)) ;
#40494 = CARTESIAN_POINT('Ctrl Pts',(13.7126126655071,-12.5165532491704,-323.823582398383)) ;
#40495 = CARTESIAN_POINT('Ctrl Pts',(13.7618262672711,-12.4624230854013,-323.82265477762)) ;
#40496 = CARTESIAN_POINT('Ctrl Pts',(13.8859207326933,-12.3242998359823,-323.820310740166)) ;
#40497 = CARTESIAN_POINT('Ctrl Pts',(13.9603603470932,-12.2399142182297,-323.818899943423)) ;
#40498 = CARTESIAN_POINT('Ctrl Pts',(14.1852361017983,-11.9802721105117,-323.814615545179)) ;
#40499 = CARTESIAN_POINT('Ctrl Pts',(14.3331731828673,-11.8028805754952,-323.811765421478)) ;
#40500 = CARTESIAN_POINT('Ctrl Pts',(14.9774860264629,-11.0003004641634,-323.799117384957)) ;
#40501 = CARTESIAN_POINT('Ctrl Pts',(15.4365437439498,-10.3462465354409,-323.789423065738)) ;
#40502 = CARTESIAN_POINT('Ctrl Pts',(15.9395618716525,-9.52119262451529,-323.777261028321)) ;
#40503 = CARTESIAN_POINT('Ctrl Pts',(16.0250917601493,-9.37652257578823,-323.775132620822)) ;
#40504 = CARTESIAN_POINT('Ctrl Pts',(16.1699677823714,-9.12369737218593,-323.771416730385)) ;
#40505 = CARTESIAN_POINT('Ctrl Pts',(16.2302219367189,-9.0160749585012,-323.76983611921)) ;
#40506 = CARTESIAN_POINT('Ctrl Pts',(16.3489940596022,-8.79888177545719,-323.766647762129)) ;
#40507 = CARTESIAN_POINT('Ctrl Pts',(16.4074937707379,-8.68930810660271,-323.765039983652)) ;
#40508 = CARTESIAN_POINT('Ctrl Pts',(16.5285631378471,-8.45695497029693,-323.761631974288)) ;
#40509 = CARTESIAN_POINT('Ctrl Pts',(16.5908743118414,-8.33404921229807,-323.759830026894)) ;
#40510 = CARTESIAN_POINT('Ctrl Pts',(16.8590241651065,-7.79020878450014,-323.751861293062)) ;
#40511 = CARTESIAN_POINT('Ctrl Pts',(17.0502527713835,-7.36226371092268,-323.745598039847)) ;
#40512 = CARTESIAN_POINT('Ctrl Pts',(17.4441548294995,-6.38284070631251,-323.731398551454)) ;
#40513 = CARTESIAN_POINT('Ctrl Pts',(17.6372619262477,-5.82805157360503,-323.723444159015)) ;
#40514 = CARTESIAN_POINT('Ctrl Pts',(17.8402192559855,-5.14175142939186,-323.714000003907)) ;
#40515 = CARTESIAN_POINT('Ctrl Pts',(17.8753995488649,-5.01807950464265,-323.712314038899)) ;
#40516 = CARTESIAN_POINT('Ctrl Pts',(17.9281970815263,-4.8248722302068,-323.709710038425)) ;
#40517 = CARTESIAN_POINT('Ctrl Pts',(17.94670078078,-4.75558342738961,-323.708782142463)) ;
#40518 = CARTESIAN_POINT('Ctrl Pts',(17.9800914025034,-4.62757836529475,-323.70708006426)) ;
#40519 = CARTESIAN_POINT('Ctrl Pts',(17.9950933281718,-4.56889313574603,-323.706304434242)) ;
#40520 = CARTESIAN_POINT('Ctrl Pts',(18.0273296059092,-4.44016769866279,-323.704612419135)) ;
#40521 = CARTESIAN_POINT('Ctrl Pts',(18.0444435415294,-4.37009830608841,-323.703697425084)) ;
#40522 = CARTESIAN_POINT('Ctrl Pts',(18.0865627569399,-4.19318350708098,-323.701400530486)) ;
#40523 = CARTESIAN_POINT('Ctrl Pts',(18.1110299393917,-4.08621277771819,-323.700023934776)) ;
#40524 = CARTESIAN_POINT('Ctrl Pts',(18.1819948471042,-3.76278821352656,-323.695891215054)) ;
#40525 = CARTESIAN_POINT('Ctrl Pts',(18.2255707308513,-3.54571340282537,-323.693156842973)) ;
#40526 = CARTESIAN_POINT('Ctrl Pts',(18.4120929858388,-2.5219852308164,-323.680360849551)) ;
#40527 = CARTESIAN_POINT('Ctrl Pts',(18.5054305691396,-1.70722583022592,-323.670421853881)) ;
#40528 = CARTESIAN_POINT('Ctrl Pts',(18.544655072549,-0.888969989752754,-323.660107772569)) ;
#40529 = CARTESIAN_POINT('Ctrl Pts',(18.5446545937399,-0.888979978054576,
-323.364389984898)) ;
#40530 = CARTESIAN_POINT('Ctrl Pts',(18.539705026844,-0.992230906915975,-323.365752954944)) ;
#40531 = CARTESIAN_POINT('Ctrl Pts',(18.533893193385,-1.09543971499047,-323.36710886668)) ;
#40532 = CARTESIAN_POINT('Ctrl Pts',(18.5222615862343,-1.27523458707085,-323.369456552669)) ;
#40533 = CARTESIAN_POINT('Ctrl Pts',(18.5168280309002,-1.35184215659057,-323.370452303384)) ;
#40534 = CARTESIAN_POINT('Ctrl Pts',(18.5057881537854,-1.49490872800445,-323.372301954481)) ;
#40535 = CARTESIAN_POINT('Ctrl Pts',(18.5002987611782,-1.56137536642769,-323.37315711715)) ;
#40536 = CARTESIAN_POINT('Ctrl Pts',(18.4852571964577,-1.73227081279554,-323.375346393268)) ;
#40537 = CARTESIAN_POINT('Ctrl Pts',(18.4751781861318,-1.8366509812536,-323.376674557344)) ;
#40538 = CARTESIAN_POINT('Ctrl Pts',(18.4378377825636,-2.19187121817369,-323.381171357321)) ;
#40539 = CARTESIAN_POINT('Ctrl Pts',(18.406347576809,-2.44223890400711,-323.384301769558)) ;
#40540 = CARTESIAN_POINT('Ctrl Pts',(18.2846053127072,-3.27302287709881,-323.394652282921)) ;
#40541 = CARTESIAN_POINT('Ctrl Pts',(18.1719175349712,-3.84979022566562,-323.401787601913)) ;
#40542 = CARTESIAN_POINT('Ctrl Pts',(17.9939349012851,-4.57585804941936,-323.411029059352)) ;
#40543 = CARTESIAN_POINT('Ctrl Pts',(17.9537762322332,-4.73097125854654,-323.413017835529)) ;
#40544 = CARTESIAN_POINT('Ctrl Pts',(17.8512020325932,-5.10703360840786,-323.417882736566)) ;
#40545 = CARTESIAN_POINT('Ctrl Pts',(17.7866861796911,-5.32738216705103,-323.420770032646)) ;
#40546 = CARTESIAN_POINT('Ctrl Pts',(17.6777065113091,-5.67551534516244,-323.425400735559)) ;
#40547 = CARTESIAN_POINT('Ctrl Pts',(17.6359039847283,-5.80410824417468,-323.427126298822)) ;
#40548 = CARTESIAN_POINT('Ctrl Pts',(17.5522896086686,-6.05207603347171,-323.430484421345)) ;
#40549 = CARTESIAN_POINT('Ctrl Pts',(17.5106551997093,-6.17150299719148,-323.432115690835)) ;
#40550 = CARTESIAN_POINT('Ctrl Pts',(17.4170129585743,-6.43153408654003,-323.435698544326)) ;
#40551 = CARTESIAN_POINT('Ctrl Pts',(17.3645158383175,-6.57195258035621,-323.437653361151)) ;
#40552 = CARTESIAN_POINT('Ctrl Pts',(17.1426893115152,-7.14406959323832,-323.445699558237)) ;
#40553 = CARTESIAN_POINT('Ctrl Pts',(16.9589161370008,-7.56998602608412,-323.45188564002)) ;
#40554 = CARTESIAN_POINT('Ctrl Pts',(16.5582670305711,-8.41051596655,-323.464399267013)) ;
#40555 = CARTESIAN_POINT('Ctrl Pts',(16.3412801388939,-8.82471241091497,-323.470722894878)) ;
#40556 = CARTESIAN_POINT('Ctrl Pts',(16.0274062481404,-9.37249239566411,-323.479156072337)) ;
#40557 = CARTESIAN_POINT('Ctrl Pts',(15.9440384104932,-9.51362202494632,-323.481334783387)) ;
#40558 = CARTESIAN_POINT('Ctrl Pts',(15.79446681661,-9.75933561227325,-323.485127552774)) ;
#40559 = CARTESIAN_POINT('Ctrl Pts',(15.7290655845843,-9.86439605475504,-323.486749065418)) ;
#40560 = CARTESIAN_POINT('Ctrl Pts',(15.6246196813183,-10.0284977731937,-323.48927681513)) ;
#40561 = CARTESIAN_POINT('Ctrl Pts',(15.5862794515146,-10.0879829824248,-323.490192044554)) ;
#40562 = CARTESIAN_POINT('Ctrl Pts',(15.5134340208546,-10.1995966598642,-323.49190619267)) ;
#40563 = CARTESIAN_POINT('Ctrl Pts',(15.4790038351896,-10.2517728918177,-323.492706224934)) ;
#40564 = CARTESIAN_POINT('Ctrl Pts',(15.379860742541,-10.4003783147004,-323.494982551317)) ;
#40565 = CARTESIAN_POINT('Ctrl Pts',(15.314505667694,-10.4963756490633,-323.496450278512)) ;
#40566 = CARTESIAN_POINT('Ctrl Pts',(15.0193972775206,-10.921223877402,-323.502946911536)) ;
#40567 = CARTESIAN_POINT('Ctrl Pts',(14.7799215551909,-11.2431910913136,-323.50787528335)) ;
#40568 = CARTESIAN_POINT('Ctrl Pts',(14.2399015016662,-11.9221303640034,-323.518507286255)) ;
#40569 = CARTESIAN_POINT('Ctrl Pts',(13.9359500139086,-12.2760451352662,-323.524204521123)) ;
#40570 = CARTESIAN_POINT('Ctrl Pts',(13.416292843738,-12.8369209774765,-323.533682028209)) ;
#40571 = CARTESIAN_POINT('Ctrl Pts',(13.208346897629,-13.0507863954024,-323.537410496588)) ;
#40572 = CARTESIAN_POINT('Ctrl Pts',(12.8908182229612,-13.3619880043206,-323.543035786374)) ;
#40573 = CARTESIAN_POINT('Ctrl Pts',(12.7850891698389,-13.4631873166709,-323.544897986929)) ;
#40574 = CARTESIAN_POINT('Ctrl Pts',(12.5875269499987,-13.6478592261056,-323.548359743646)) ;
#40575 = CARTESIAN_POINT('Ctrl Pts',(12.4960320180572,-13.7316816131623,-323.549956055694)) ;
#40576 = CARTESIAN_POINT('Ctrl Pts',(12.2874157764585,-13.9189919752601,-323.553581045082)) ;
#40577 = CARTESIAN_POINT('Ctrl Pts',(12.1698141909309,-14.0219309129883,-323.555614302201)) ;
#40578 = CARTESIAN_POINT('Ctrl Pts',(11.7905788862626,-14.345517716308,-323.562138469836)) ;
#40579 = CARTESIAN_POINT('Ctrl Pts',(11.5241385872486,-14.5604209388132,-323.566674923889)) ;
#40580 = CARTESIAN_POINT('Ctrl Pts',(10.7099331151377,-15.1807804668337,-323.580357077851)) ;
#40581 = CARTESIAN_POINT('Ctrl Pts',(10.1456348005316,-15.563574595004,-323.589621784976)) ;
#40582 = CARTESIAN_POINT('Ctrl Pts',(9.4013627128699,-16.010740540667,-323.601168913555)) ;
#40583 = CARTESIAN_POINT('Ctrl Pts',(9.23970408350948,-16.1045739523244,-323.603637100746)) ;
#40584 = CARTESIAN_POINT('Ctrl Pts',(9.00528869496427,-16.2359467825268,-323.607145037673)) ;
#40585 = CARTESIAN_POINT('Ctrl Pts',(8.93365765930777,-16.2754709073548,-323.608207558408)) ;
#40586 = CARTESIAN_POINT('Ctrl Pts',(8.80361898002909,-16.346105687975,-323.610117848131)) ;
#40587 = CARTESIAN_POINT('Ctrl Pts',(8.74530197161909,-16.3773798798947,-323.610967667025)) ;
#40588 = CARTESIAN_POINT('Ctrl Pts',(8.60213932837005,-16.4531723017898,-323.613037816977)) ;
#40589 = CARTESIAN_POINT('Ctrl Pts',(8.51711389007415,-16.4973467817862,-323.614253753368)) ;
#40590 = CARTESIAN_POINT('Ctrl Pts',(8.18379450336982,-16.6672572715916,-323.618974526123)) ;
#40591 = CARTESIAN_POINT('Ctrl Pts',(7.93302743539708,-16.7880622397032,-323.622427635515)) ;
#40592 = CARTESIAN_POINT('Ctrl Pts',(7.01926950190053,-17.2032107219358,-323.634795144119)) ;
#40593 = CARTESIAN_POINT('Ctrl Pts',(6.34188560579116,-17.4642804977528,-323.643586853735)) ;
#40594 = CARTESIAN_POINT('Ctrl Pts',(5.42390919650671,-17.7576047969066,-323.655602086964)) ;
#40595 = CARTESIAN_POINT('Ctrl Pts',(5.19547442175171,-17.8257780846087,-323.658597318588)) ;
#40596 = CARTESIAN_POINT('Ctrl Pts',(4.83403222518032,-17.926107491275,-323.663356505027)) ;
#40597 = CARTESIAN_POINT('Ctrl Pts',(4.70187379795501,-17.9612243475874,-323.665100737526)) ;
#40598 = CARTESIAN_POINT('Ctrl Pts',(4.44734264949641,-18.0258560313336,-323.668469328127)) ;
#40599 = CARTESIAN_POINT('Ctrl Pts',(4.32503390907904,-18.0555925944412,-323.670092098988)) ;
#40600 = CARTESIAN_POINT('Ctrl Pts',(4.03312163953547,-18.1234280252547,-323.673975420308)) ;
#40601 = CARTESIAN_POINT('Ctrl Pts',(3.86326694324537,-18.1603932208046,-323.676243267535)) ;
#40602 = CARTESIAN_POINT('Ctrl Pts',(3.00433517995802,-18.3347252119986,-323.687751046602)) ;
#40603 = CARTESIAN_POINT('Ctrl Pts',(2.30837543410544,-18.4352806738096,-323.697227915984)) ;
#40604 = CARTESIAN_POINT('Ctrl Pts',(1.32339132720001,-18.5209335274373,-323.710537542992)) ;
#40605 = CARTESIAN_POINT('Ctrl Pts',(1.03784802112278,-18.5391266011936,-323.71438026684)) ;
#40606 = CARTESIAN_POINT('Ctrl Pts',(0.572383341458803,-18.557995347468,-323.720570746154)) ;
#40607 = CARTESIAN_POINT('Ctrl Pts',(0.392671647027375,-18.5626674586618,
-323.722942857314)) ;
#40608 = CARTESIAN_POINT('Ctrl Pts',(0.13220455061334,-18.5656547755997,-323.726342026205)) ;
#40609 = CARTESIAN_POINT('Ctrl Pts',(0.0514835533319589,-18.56605409768,-323.727390034011)) ;
#40610 = CARTESIAN_POINT('Ctrl Pts',(-0.0955999450868811,-18.5658224712016,
-323.729288154021)) ;
#40611 = CARTESIAN_POINT('Ctrl Pts',(-0.161961168924328,-18.5653621552626,
-323.730140127854)) ;
#40612 = CARTESIAN_POINT('Ctrl Pts',(-0.310077309297243,-18.5635405287751,
-323.732032568184)) ;
#40613 = CARTESIAN_POINT('Ctrl Pts',(-0.391828567636493,-18.561994916996,
-323.733070983871)) ;
#40614 = CARTESIAN_POINT('Ctrl Pts',(-0.714902374646459,-18.5537514986789,
-323.737154821241)) ;
#40615 = CARTESIAN_POINT('Ctrl Pts',(-0.956095187033817,-18.5428871135722,
-323.740160027758)) ;
#40616 = CARTESIAN_POINT('Ctrl Pts',(-2.00659433908352,-18.4750167774234,
-323.753168131234)) ;
#40617 = CARTESIAN_POINT('Ctrl Pts',(-2.81188197848714,-18.3697030875708,
-323.76297057117)) ;
#40618 = CARTESIAN_POINT('Ctrl Pts',(-3.82119444668937,-18.1697645171,-323.775830886454)) ;
#40619 = CARTESIAN_POINT('Ctrl Pts',(-4.03393224413369,-18.1237209208171,
-323.778571510467)) ;
#40620 = CARTESIAN_POINT('Ctrl Pts',(-4.3754003375343,-18.0435055192205,-323.783027560451)) ;
#40621 = CARTESIAN_POINT('Ctrl Pts',(-4.50465841605385,-18.0116704397114,
-323.78472757326)) ;
#40622 = CARTESIAN_POINT('Ctrl Pts',(-4.75566958478692,-17.9469776467239,
-323.788056025662)) ;
#40623 = CARTESIAN_POINT('Ctrl Pts',(-4.87745245116757,-17.9142640760013,
-323.789683422183)) ;
#40624 = CARTESIAN_POINT('Ctrl Pts',(-5.14728986616577,-17.8388242182939,
-323.793317697014)) ;
#40625 = CARTESIAN_POINT('Ctrl Pts',(-5.29516482784907,-17.7954902098312,
-323.795328501594)) ;
#40626 = CARTESIAN_POINT('Ctrl Pts',(-6.13654753101533,-17.5375111442387,
-323.806877868866)) ;
#40627 = CARTESIAN_POINT('Ctrl Pts',(-6.81753086240384,-17.284177067517,-323.816676306804)) ;
#40628 = CARTESIAN_POINT('Ctrl Pts',(-7.73411826798254,-16.8805760561065,
-323.830154568869)) ;
#40629 = CARTESIAN_POINT('Ctrl Pts',(-7.98380956548507,-16.7639261062606,
-323.833853574647)) ;
#40630 = CARTESIAN_POINT('Ctrl Pts',(-8.38823308916128,-16.5639031764877,
-323.839846408533)) ;
#40631 = CARTESIAN_POINT('Ctrl Pts',(-8.5445418843198,-16.4838146971828,-323.842162880615)) ;
#40632 = CARTESIAN_POINT('Ctrl Pts',(-8.77042729694959,-16.3640006049362,
-323.845498776788)) ;
#40633 = CARTESIAN_POINT('Ctrl Pts',(-8.8409201886417,-16.326023429215,-323.846538126273)) ;
#40634 = CARTESIAN_POINT('Ctrl Pts',(-8.96950182988737,-16.2556746449036,
-323.848429257214)) ;
#40635 = CARTESIAN_POINT('Ctrl Pts',(-9.02766639664809,-16.2234447840582,
-323.849282786557)) ;
#40636 = CARTESIAN_POINT('Ctrl Pts',(-9.17176266897457,-16.1425839918251,
-323.851393374272)) ;
#40637 = CARTESIAN_POINT('Ctrl Pts',(-9.25748198520534,-16.0935787108959,
-323.852645565963)) ;
#40638 = CARTESIAN_POINT('Ctrl Pts',(-9.63085604940103,-15.8761525650157,
-323.858093305349)) ;
#40639 = CARTESIAN_POINT('Ctrl Pts',(-9.91433687355013,-15.7006857774954,
-323.862213398769)) ;
#40640 = CARTESIAN_POINT('Ctrl Pts',(-10.6419574345238,-15.2227411481744,
-323.872911666842)) ;
#40641 = CARTESIAN_POINT('Ctrl Pts',(-11.0779611919801,-14.9084500343722,
-323.879452312755)) ;
#40642 = CARTESIAN_POINT('Ctrl Pts',(-11.62026839743,-14.4805883423499,-323.887999798035)) ;
#40643 = CARTESIAN_POINT('Ctrl Pts',(-11.7396307068311,-14.3839892647788,
-323.889907534588)) ;
#40644 = CARTESIAN_POINT('Ctrl Pts',(-12.0294923303816,-14.1433946485244,
-323.894612629072)) ;
#40645 = CARTESIAN_POINT('Ctrl Pts',(-12.1986198822566,-13.9977844897618,
-323.897420982805)) ;
#40646 = CARTESIAN_POINT('Ctrl Pts',(-12.4651022248643,-13.7598584698423,
-323.901957675155)) ;
#40647 = CARTESIAN_POINT('Ctrl Pts',(-12.5641527718401,-13.6694748856444,
-323.903669495621)) ;
#40648 = CARTESIAN_POINT('Ctrl Pts',(-12.754058873601,-13.4923775733218,-323.907002808177)) ;
#40649 = CARTESIAN_POINT('Ctrl Pts',(-12.8450308507631,-13.4057992198298,
-323.908623053695)) ;
#40650 = CARTESIAN_POINT('Ctrl Pts',(-13.0439094789223,-13.2126426236198,
-323.912217959475)) ;
#40651 = CARTESIAN_POINT('Ctrl Pts',(-13.1514027374575,-13.1056516640792,
-323.914196237261)) ;
#40652 = CARTESIAN_POINT('Ctrl Pts',(-13.5580809037679,-12.6908314864055,
-323.921816323016)) ;
#40653 = CARTESIAN_POINT('Ctrl Pts',(-13.8478670510679,-12.3739782608301,
-323.92753672665)) ;
#40654 = CARTESIAN_POINT('Ctrl Pts',(-14.4444817281997,-11.674404414738,-323.939882560336)) ;
#40655 = CARTESIAN_POINT('Ctrl Pts',(-14.7476587905868,-11.2889915689595,
-323.946517515641)) ;
#40656 = CARTESIAN_POINT('Ctrl Pts',(-15.1334564391573,-10.7564413220802,
-323.955305237844)) ;
#40657 = CARTESIAN_POINT('Ctrl Pts',(-15.2298461524232,-10.619525413575,-323.957531800775)) ;
#40658 = CARTESIAN_POINT('Ctrl Pts',(-15.3953002994273,-10.3776208024618,
-323.961397282393)) ;
#40659 = CARTESIAN_POINT('Ctrl Pts',(-15.4651754295498,-10.2731997858886,
-323.963044034665)) ;
#40660 = CARTESIAN_POINT('Ctrl Pts',(-15.5729472825247,-10.1085544643828,
-323.965601654979)) ;
#40661 = CARTESIAN_POINT('Ctrl Pts',(-15.6115668320745,-10.0488079635763,
-323.966521852004)) ;
#40662 = CARTESIAN_POINT('Ctrl Pts',(-15.6881090970104,-9.92888670684282,
-323.968351860028)) ;
#40663 = CARTESIAN_POINT('Ctrl Pts',(-15.726031330753,-9.86871303050863,-323.969261657649)) ;
#40664 = CARTESIAN_POINT('Ctrl Pts',(-15.8299415797294,-9.70171197077004,
-323.971765322999)) ;
#40665 = CARTESIAN_POINT('Ctrl Pts',(-15.8951931357065,-9.59443071984208,
-323.973349756565)) ;
#40666 = CARTESIAN_POINT('Ctrl Pts',(-16.0652294870347,-9.30837462762842,
-323.977521500787)) ;
#40667 = CARTESIAN_POINT('Ctrl Pts',(-16.1681182712859,-9.1284932204573,-323.980090796395)) ;
#40668 = CARTESIAN_POINT('Ctrl Pts',(-16.5533231895385,-8.42808472390377,
-323.989947783485)) ;
#40669 = CARTESIAN_POINT('Ctrl Pts',(-16.8136870526762,-7.89588817229777,
-323.997139857357)) ;
#40670 = CARTESIAN_POINT('Ctrl Pts',(-17.1118556839643,-7.20449547407663,
-324.00644709476)) ;
#40671 = CARTESIAN_POINT('Ctrl Pts',(-17.1736164390241,-7.05600866748605,
-324.00844305087)) ;
#40672 = CARTESIAN_POINT('Ctrl Pts',(-17.3190556277311,-6.69311413874813,
-324.013322024012)) ;
#40673 = CARTESIAN_POINT('Ctrl Pts',(-17.4006913297935,-6.47791676983834,
-324.016216225918)) ;
#40674 = CARTESIAN_POINT('Ctrl Pts',(-17.5239380314501,-6.13387352151208,
-324.020855152102)) ;
#40675 = CARTESIAN_POINT('Ctrl Pts',(-17.56817692178,-6.00599434635214,-324.022581914922)) ;
#40676 = CARTESIAN_POINT('Ctrl Pts',(-17.6510393599688,-5.75771599431401,
-324.025940655414)) ;
#40677 = CARTESIAN_POINT('Ctrl Pts',(-17.6898387211444,-5.63738325149682,
-324.027571323706)) ;
#40678 = CARTESIAN_POINT('Ctrl Pts',(-17.7718858653347,-5.37373059732031,
-324.031150771236)) ;
#40679 = CARTESIAN_POINT('Ctrl Pts',(-17.8146354597751,-5.23026491593894,
-324.033102756787)) ;
#40680 = CARTESIAN_POINT('Ctrl Pts',(-17.9817830474478,-4.64348687351731,
-324.041102768237)) ;
#40681 = CARTESIAN_POINT('Ctrl Pts',(-18.0914044770507,-4.1961379618827,-324.047244019601)) ;
#40682 = CARTESIAN_POINT('Ctrl Pts',(-18.2791698126968,-3.284465131321,-324.059751957753)) ;
#40683 = CARTESIAN_POINT('Ctrl Pts',(-18.3565138536121,-2.82031189593331,
-324.066116073327)) ;
#40684 = CARTESIAN_POINT('Ctrl Pts',(-18.4461489062061,-2.11898391226726,
-324.075560962735)) ;
#40685 = CARTESIAN_POINT('Ctrl Pts',(-18.4716596230034,-1.88369144161412,
-324.078700048023)) ;
#40686 = CARTESIAN_POINT('Ctrl Pts',(-18.5005070762339,-1.55998133948917,
-324.082951338903)) ;
#40687 = CARTESIAN_POINT('Ctrl Pts',(-18.5077205305798,-1.47193228449077,
-324.084100827533)) ;
#40688 = CARTESIAN_POINT('Ctrl Pts',(-18.5192057283192,-1.31827201937813,
-324.08609293446)) ;
#40689 = CARTESIAN_POINT('Ctrl Pts',(-18.5237578729388,-1.25268360122756,
-324.086938688335)) ;
#40690 = CARTESIAN_POINT('Ctrl Pts',(-18.5334728918954,-1.1010504402287,-324.088883524569)) ;
#40691 = CARTESIAN_POINT('Ctrl Pts',(-18.5383851002295,-1.01499133527106,
-324.089979775295)) ;
#40692 = CARTESIAN_POINT('Ctrl Pts',(-18.5508523473216,-0.766120490061058,
-324.093131830707)) ;
#40693 = CARTESIAN_POINT('Ctrl Pts',(-18.5568630394829,-0.603239336752139,
-324.095172399095)) ;
#40694 = CARTESIAN_POINT('Ctrl Pts',(-18.567355789222,-0.160920308868857,
-324.100674562745)) ;
#40695 = CARTESIAN_POINT('Ctrl Pts',(-18.567674517597,0.118573812836487,-324.104109250648)) ;
#40696 = CARTESIAN_POINT('Ctrl Pts',(-18.5541197532939,0.750782601332609,
-324.111861938473)) ;
#40697 = CARTESIAN_POINT('Ctrl Pts',(-18.5364975924869,1.10330925274586,-324.116173948557)) ;
#40698 = CARTESIAN_POINT('Ctrl Pts',(-18.4875533154418,1.7258713362352,-324.1238641765)) ;
#40699 = CARTESIAN_POINT('Ctrl Pts',(-18.4603290444846,1.99612392089792,-324.127227349924)) ;
#40700 = CARTESIAN_POINT('Ctrl Pts',(-18.4010277568686,2.47843172522886,-324.133303575734)) ;
#40701 = CARTESIAN_POINT('Ctrl Pts',(-18.3711869885596,2.69071268000922,-324.136003678311)) ;
#40702 = CARTESIAN_POINT('Ctrl Pts',(-18.3169576172568,3.03333629516447,-324.140411505258)) ;
#40703 = CARTESIAN_POINT('Ctrl Pts',(-18.2948368747106,3.16401787268748,-324.142104463582)) ;
#40704 = CARTESIAN_POINT('Ctrl Pts',(-18.2488819474081,3.41888797420616,-324.145430527637)) ;
#40705 = CARTESIAN_POINT('Ctrl Pts',(-18.225174498806,3.54309211631266,-324.147062716791)) ;
#40706 = CARTESIAN_POINT('Ctrl Pts',(-18.1694524714901,3.81965055839441,-324.150722804066)) ;
#40707 = CARTESIAN_POINT('Ctrl Pts',(-18.1367866631158,3.97186391264434,-324.15275483126)) ;
#40708 = CARTESIAN_POINT('Ctrl Pts',(-17.9447695069173,4.81479103820004,-324.164103920793)) ;
#40709 = CARTESIAN_POINT('Ctrl Pts',(-17.7478763809153,5.49634799684162,-324.173666136872)) ;
#40710 = CARTESIAN_POINT('Ctrl Pts',(-17.4182716560495,6.43263842295779,-324.187027643438)) ;
#40711 = CARTESIAN_POINT('Ctrl Pts',(-17.3179192901622,6.69811140088752,-324.190838755185)) ;
#40712 = CARTESIAN_POINT('Ctrl Pts',(-17.1444584601289,7.12699341337816,-324.196985894895)) ;
#40713 = CARTESIAN_POINT('Ctrl Pts',(-17.0750025990897,7.29182949890128,-324.199345898812)) ;
#40714 = CARTESIAN_POINT('Ctrl Pts',(-16.9708164458865,7.52943436296937,-324.20273131719)) ;
#40715 = CARTESIAN_POINT('Ctrl Pts',(-16.9379770088996,7.60302094804456,-324.203777456884)) ;
#40716 = CARTESIAN_POINT('Ctrl Pts',(-16.877209481932,7.7368409021025,-324.205674050935)) ;
#40717 = CARTESIAN_POINT('Ctrl Pts',(-16.8494354578039,7.79714253999942,-324.206526342475)) ;
#40718 = CARTESIAN_POINT('Ctrl Pts',(-16.7799334737977,7.94593631101331,-324.208624368038)) ;
#40719 = CARTESIAN_POINT('Ctrl Pts',(-16.7378283306994,8.03425006182183,-324.209865381101)) ;
#40720 = CARTESIAN_POINT('Ctrl Pts',(-16.5502105180837,8.41989361480937,-324.215273928545)) ;
#40721 = CARTESIAN_POINT('Ctrl Pts',(-16.3974585496524,8.71363476340976,-324.219366672211)) ;
#40722 = CARTESIAN_POINT('Ctrl Pts',(-15.9749446249027,9.47562833895723,-324.230075764247)) ;
#40723 = CARTESIAN_POINT('Ctrl Pts',(-15.6924550293611,9.93646032958495,-324.236652596206)) ;
#40724 = CARTESIAN_POINT('Ctrl Pts',(-15.3041482968991,10.5119576665882,-324.245242567396)) ;
#40725 = CARTESIAN_POINT('Ctrl Pts',(-15.2164399100211,10.6385227111206,-324.247155546407)) ;
#40726 = CARTESIAN_POINT('Ctrl Pts',(-14.9975448100899,10.9461470482429,-324.25187103321)) ;
#40727 = CARTESIAN_POINT('Ctrl Pts',(-14.8646425266992,11.125955591658,-324.254684549326)) ;
#40728 = CARTESIAN_POINT('Ctrl Pts',(-14.6468460369367,11.4097501970167,-324.259227389375)) ;
#40729 = CARTESIAN_POINT('Ctrl Pts',(-14.5640154354839,11.5152921248197,-324.260940109721)) ;
#40730 = CARTESIAN_POINT('Ctrl Pts',(-14.4014723224883,11.7178434954987,-324.264273832678)) ;
#40731 = CARTESIAN_POINT('Ctrl Pts',(-14.3219052730378,11.8149604543419,-324.265893573586)) ;
#40732 = CARTESIAN_POINT('Ctrl Pts',(-14.1441730244388,12.0274609142514,-324.269485656118)) ;
#40733 = CARTESIAN_POINT('Ctrl Pts',(-14.0455682798255,12.142465079025,-324.271461593137)) ;
#40734 = CARTESIAN_POINT('Ctrl Pts',(-13.6571009401313,12.5844761052013,-324.279180322461)) ;
#40735 = CARTESIAN_POINT('Ctrl Pts',(-13.3571374800356,12.9024153331622,-324.285005123218)) ;
#40736 = CARTESIAN_POINT('Ctrl Pts',(-12.9679882991646,13.2867555969037,-324.292351013689)) ;
#40737 = CARTESIAN_POINT('Ctrl Pts',(-12.889054177129,13.3633407958953,-324.293830511261)) ;
#40738 = CARTESIAN_POINT('Ctrl Pts',(-12.3927598227565,13.8363782807931,-324.303061002039)) ;
#40739 = CARTESIAN_POINT('Ctrl Pts',(-11.9578297118556,14.2139427810809,-324.310847955634)) ;
#40740 = CARTESIAN_POINT('Ctrl Pts',(-11.4223337296037,14.6368088711685,-324.319814521377)) ;
#40741 = CARTESIAN_POINT('Ctrl Pts',(-11.3380356491296,14.7022049173412,-324.32120836544)) ;
#40742 = CARTESIAN_POINT('Ctrl Pts',(-11.1999055796125,14.8074677283556,-324.323460529833)) ;
#40743 = CARTESIAN_POINT('Ctrl Pts',(-11.1464132751362,14.8477761519391,-324.324325028041)) ;
#40744 = CARTESIAN_POINT('Ctrl Pts',(-11.0317032485867,14.9332451157236,-324.326161661636)) ;
#40745 = CARTESIAN_POINT('Ctrl Pts',(-10.9704238054972,14.978320593432,-324.327132634947)) ;
#40746 = CARTESIAN_POINT('Ctrl Pts',(-10.7859849524016,15.1122496921848,-324.330027332871)) ;
#40747 = CARTESIAN_POINT('Ctrl Pts',(-10.6620104932061,15.1999702145794,-324.331936371896)) ;
#40748 = CARTESIAN_POINT('Ctrl Pts',(-10.440854319518,15.3524164002585,-324.33528914206)) ;
#40749 = CARTESIAN_POINT('Ctrl Pts',(-10.3441121145819,15.4177648460854,-324.336738292432)) ;
#40750 = CARTESIAN_POINT('Ctrl Pts',(-9.8586678692911,15.7390519865276,-324.343937122767)) ;
#40751 = CARTESIAN_POINT('Ctrl Pts',(-9.46105475063361,15.9812244114188,-324.349606968786)) ;
#40752 = CARTESIAN_POINT('Ctrl Pts',(-8.64798352947633,16.4354492379765,-324.361040018164)) ;
#40753 = CARTESIAN_POINT('Ctrl Pts',(-8.23279419330226,16.6473033605225,-324.366799601881)) ;
#40754 = CARTESIAN_POINT('Ctrl Pts',(-7.67394169943359,16.9064376973664,-324.37455946645)) ;
#40755 = CARTESIAN_POINT('Ctrl Pts',(-7.53704659592083,16.9679092804009,-324.37646039916)) ;
#40756 = CARTESIAN_POINT('Ctrl Pts',(-7.2833985956329,17.0781324382906,-324.379985327671)) ;
#40757 = CARTESIAN_POINT('Ctrl Pts',(-7.16686353865906,17.1273631843124,-324.381605854043)) ;
#40758 = CARTESIAN_POINT('Ctrl Pts',(-6.92481376661192,17.2267152193293,-324.384974901486)) ;
#40759 = CARTESIAN_POINT('Ctrl Pts',(-6.79923653214833,17.2766647667963,-324.386724509828)) ;
#40760 = CARTESIAN_POINT('Ctrl Pts',(-6.45926239258203,17.4076118813034,-324.391466209516)) ;
#40761 = CARTESIAN_POINT('Ctrl Pts',(-6.24389298369518,17.4860179049564,-324.394475527915)) ;
#40762 = CARTESIAN_POINT('Ctrl Pts',(-5.87598331878911,17.6122927295453,-324.399621774137)) ;
#40763 = CARTESIAN_POINT('Ctrl Pts',(-5.72417563663214,17.6622152730534,-324.401746720793)) ;
#40764 = CARTESIAN_POINT('Ctrl Pts',(-5.01469412694131,17.8854230643169,-324.411676302628)) ;
#40765 = CARTESIAN_POINT('Ctrl Pts',(-4.44968896443668,18.0342945881159,-324.419590888887)) ;
#40766 = CARTESIAN_POINT('Ctrl Pts',(-3.6232410265317,18.2108432910851,-324.430913897107)) ;
#40767 = CARTESIAN_POINT('Ctrl Pts',(-3.36674871518028,18.2600025312862,-324.434391390069)) ;
#40768 = CARTESIAN_POINT('Ctrl Pts',(-3.00800824240249,18.3209427403234,-324.439168998776)) ;
#40769 = CARTESIAN_POINT('Ctrl Pts',(-2.90657053032288,18.3373090795478,-324.440510325029)) ;
#40770 = CARTESIAN_POINT('Ctrl Pts',(-2.73873621216545,18.3629604668013,-324.442710885177)) ;
#40771 = CARTESIAN_POINT('Ctrl Pts',(-2.67241588457293,18.3727294250189,-324.443575571237)) ;
#40772 = CARTESIAN_POINT('Ctrl Pts',(-2.52876852843879,18.3930943735101,-324.445437153986)) ;
#40773 = CARTESIAN_POINT('Ctrl Pts',(-2.45142478384017,18.4035623577219,-324.446432627266)) ;
#40774 = CARTESIAN_POINT('Ctrl Pts',(-2.21209270934666,18.4344189125433,-324.449494752219)) ;
#40775 = CARTESIAN_POINT('Ctrl Pts',(-2.04989955283367,18.4531587208636,-324.451544149119)) ;
#40776 = CARTESIAN_POINT('Ctrl Pts',(-1.38571922609436,18.5210333123235,-324.459864273711)) ;
#40777 = CARTESIAN_POINT('Ctrl Pts',(-0.882076138796647,18.5518418666242,
-324.466010819242)) ;
#40778 = CARTESIAN_POINT('Ctrl Pts',(0.104180440712025,18.5719156590424,-324.478103884316)) ;
#40779 = CARTESIAN_POINT('Ctrl Pts',(0.586363543142085,18.5629491558235,-324.484042574201)) ;
#40780 = CARTESIAN_POINT('Ctrl Pts',(1.25279041943156,18.5245622530413,-324.492424001211)) ;
#40781 = CARTESIAN_POINT('Ctrl Pts',(1.43776148413839,18.5111245541986,-324.494768174686)) ;
#40782 = CARTESIAN_POINT('Ctrl Pts',(1.74835396756131,18.4838772703247,-324.498739241115)) ;
#40783 = CARTESIAN_POINT('Ctrl Pts',(1.87409191517363,18.4715521811394,-324.500356463428)) ;
#40784 = CARTESIAN_POINT('Ctrl Pts',(2.13163095670585,18.4436509536328,-324.503689610014)) ;
#40785 = CARTESIAN_POINT('Ctrl Pts',(2.26341058377905,18.4279430078867,-324.505406305769)) ;
#40786 = CARTESIAN_POINT('Ctrl Pts',(2.60854019359328,18.3830461036312,-324.509932064979)) ;
#40787 = CARTESIAN_POINT('Ctrl Pts',(2.82157029892458,18.3515559772245,-324.512755627286)) ;
#40788 = CARTESIAN_POINT('Ctrl Pts',(3.30374402845528,18.2716865895805,-324.519211229117)) ;
#40789 = CARTESIAN_POINT('Ctrl Pts',(3.57246364315119,18.2210526189448,-324.522855329624)) ;
#40790 = CARTESIAN_POINT('Ctrl Pts',(4.18292286917412,18.0920018566472,-324.531217395195)) ;
#40791 = CARTESIAN_POINT('Ctrl Pts',(4.52375710741976,18.0098027811781,-324.535947247355)) ;
#40792 = CARTESIAN_POINT('Ctrl Pts',(4.95311624671509,17.8932959724943,-324.541935394451)) ;
#40793 = CARTESIAN_POINT('Ctrl Pts',(5.04398375018243,17.8678938112029,-324.5432043056)) ;
#40794 = CARTESIAN_POINT('Ctrl Pts',(5.44417387341787,17.7527239473073,-324.548795550816)) ;
#40795 = CARTESIAN_POINT('Ctrl Pts',(5.75132435800101,17.6556083323244,-324.553095306633)) ;
#40796 = CARTESIAN_POINT('Ctrl Pts',(6.14829269583703,17.5186349696355,-324.558602517575)) ;
#40797 = CARTESIAN_POINT('Ctrl Pts',(6.24053867217814,17.4859872868109,-324.559878613981)) ;
#40798 = CARTESIAN_POINT('Ctrl Pts',(6.39493271446416,17.4299668053486,-324.562005739409)) ;
#40799 = CARTESIAN_POINT('Ctrl Pts',(6.45722120746729,17.4069871480101,-324.56286143272)) ;
#40800 = CARTESIAN_POINT('Ctrl Pts',(6.59482637025094,17.3553811934651,-324.564745776105)) ;
#40801 = CARTESIAN_POINT('Ctrl Pts',(6.67008251218251,17.3265977770865,-324.565772550043)) ;
#40802 = CARTESIAN_POINT('Ctrl Pts',(6.91173575077784,17.2323643012918,-324.569060754749)) ;
#40803 = CARTESIAN_POINT('Ctrl Pts',(7.0773756963453,17.1649999694861,-324.571301143092)) ;
#40804 = CARTESIAN_POINT('Ctrl Pts',(7.50317245671976,16.984620817098,-324.577052479042)) ;
#40805 = CARTESIAN_POINT('Ctrl Pts',(7.76175898468539,16.8680182324122,-324.580537972568)) ;
#40806 = CARTESIAN_POINT('Ctrl Pts',(8.65725778979356,16.4392635963865,-324.592709666869)) ;
#40807 = CARTESIAN_POINT('Ctrl Pts',(9.2788682826451,16.0965866879065,-324.601364003498)) ;
#40808 = CARTESIAN_POINT('Ctrl Pts',(10.0111014883923,15.6363858600552,-324.612246137638)) ;
#40809 = CARTESIAN_POINT('Ctrl Pts',(10.1418101823302,15.5519259870914,-324.614215550832)) ;
#40810 = CARTESIAN_POINT('Ctrl Pts',(10.37676097268,15.3958863287364,-324.617807647135)) ;
#40811 = CARTESIAN_POINT('Ctrl Pts',(10.4813631381111,15.3248657692395,-324.619425978489)) ;
#40812 = CARTESIAN_POINT('Ctrl Pts',(10.6941333593913,15.1772060166064,-324.622758210772)) ;
#40813 = CARTESIAN_POINT('Ctrl Pts',(10.8022224610996,15.1004655761914,-324.624472849874)) ;
#40814 = CARTESIAN_POINT('Ctrl Pts',(11.0830155509729,14.8965520094093,-324.628985159841)) ;
#40815 = CARTESIAN_POINT('Ctrl Pts',(11.2543537881431,14.7675324964426,-324.631797165475)) ;
#40816 = CARTESIAN_POINT('Ctrl Pts',(11.5375342631315,14.5465033115619,-324.636541548852)) ;
#40817 = CARTESIAN_POINT('Ctrl Pts',(11.6506047481779,14.4561012864183,-324.638462554768)) ;
#40818 = CARTESIAN_POINT('Ctrl Pts',(12.1338923240003,14.060350198098,-324.646784138546)) ;
#40819 = CARTESIAN_POINT('Ctrl Pts',(12.4932503784913,13.7420334794546,-324.653261774176)) ;
#40820 = CARTESIAN_POINT('Ctrl Pts',(12.9042830285731,13.3484804927794,-324.660921460213)) ;
#40821 = CARTESIAN_POINT('Ctrl Pts',(12.9682502829186,13.2863439874793,-324.66212088407)) ;
#40822 = CARTESIAN_POINT('Ctrl Pts',(13.2657618104115,12.993151715513,-324.667730379253)) ;
#40823 = CARTESIAN_POINT('Ctrl Pts',(13.493594870502,12.7563837414125,-324.672117526406)) ;
#40824 = CARTESIAN_POINT('Ctrl Pts',(13.7808787327236,12.441520269464,-324.677707071031)) ;
#40825 = CARTESIAN_POINT('Ctrl Pts',(13.8461611037519,12.3688264597231,-324.678981191469)) ;
#40826 = CARTESIAN_POINT('Ctrl Pts',(13.9548244378176,12.2458882857338,-324.681106122939)) ;
#40827 = CARTESIAN_POINT('Ctrl Pts',(13.9985151942239,12.1959205224098,-324.681961574479)) ;
#40828 = CARTESIAN_POINT('Ctrl Pts',(14.0947030561704,12.0847155884654,-324.683846758524)) ;
#40829 = CARTESIAN_POINT('Ctrl Pts',(14.1470708503968,12.0233685576739,-324.684874599791)) ;
#40830 = CARTESIAN_POINT('Ctrl Pts',(14.3145931520765,11.8245122957983,-324.68817078775)) ;
#40831 = CARTESIAN_POINT('Ctrl Pts',(14.428155485717,11.6856748895056,-324.690417951463)) ;
#40832 = CARTESIAN_POINT('Ctrl Pts',(14.7169391794318,11.3219895532334,-324.69619337261)) ;
#40833 = CARTESIAN_POINT('Ctrl Pts',(14.8890260111889,11.094712754573,-324.699695922776)) ;
#40834 = CARTESIAN_POINT('Ctrl Pts',(15.4686136549433,10.2914623185011,-324.711838576095)) ;
#40835 = CARTESIAN_POINT('Ctrl Pts',(15.8484714228753,9.69629610487714,-324.720448245434)) ;
#40836 = CARTESIAN_POINT('Ctrl Pts',(16.2699357734574,8.94472398387492,-324.731289370676)) ;
#40837 = CARTESIAN_POINT('Ctrl Pts',(16.3446127985239,8.80752687151463,-324.733265953058)) ;
#40838 = CARTESIAN_POINT('Ctrl Pts',(16.4766468524527,8.55748942413728,-324.736866828345)) ;
#40839 = CARTESIAN_POINT('Ctrl Pts',(16.5345981628697,8.44497366979848,-324.738486693089)) ;
#40840 = CARTESIAN_POINT('Ctrl Pts',(16.6507908460302,8.21359732251355,-324.741817740228)) ;
#40841 = CARTESIAN_POINT('Ctrl Pts',(16.708920711874,8.09468871279821,-324.743529615604)) ;
#40842 = CARTESIAN_POINT('Ctrl Pts',(16.8574026586591,7.78254299763999,-324.748023852401)) ;
#40843 = CARTESIAN_POINT('Ctrl Pts',(16.945704574732,7.58835266220957,-324.75082032914)) ;
#40844 = CARTESIAN_POINT('Ctrl Pts',(17.1763878301818,7.05692409235652,-324.758470612091)) ;
#40845 = CARTESIAN_POINT('Ctrl Pts',(17.3121736002563,6.71692793003951,-324.76336350778)) ;
#40846 = CARTESIAN_POINT('Ctrl Pts',(17.6630807818063,5.7567960480472,-324.777102807033)) ;
#40847 = CARTESIAN_POINT('Ctrl Pts',(17.8555056050564,5.12894167138362,-324.786010947495)) ;
#40848 = CARTESIAN_POINT('Ctrl Pts',(18.0405672410463,4.38682484279444,-324.796066011163)) ;
#40849 = CARTESIAN_POINT('Ctrl Pts',(18.0659244919529,4.28119970154073,-324.797485663999)) ;
#40850 = CARTESIAN_POINT('Ctrl Pts',(18.1054876289773,4.10978658554265,-324.799767639971)) ;
#40851 = CARTESIAN_POINT('Ctrl Pts',(18.1202652971264,4.04413323998005,-324.800636459264)) ;
#40852 = CARTESIAN_POINT('Ctrl Pts',(18.1508335401383,3.90479446948766,-324.80246842664)) ;
#40853 = CARTESIAN_POINT('Ctrl Pts',(18.1665330853654,3.8310904099575,-324.803430548767)) ;
#40854 = CARTESIAN_POINT('Ctrl Pts',(18.2117120533573,3.61246645183499,-324.80626651823)) ;
#40855 = CARTESIAN_POINT('Ctrl Pts',(18.2399091895371,3.46728750721235,-324.808126534658)) ;
#40856 = CARTESIAN_POINT('Ctrl Pts',(18.3042526298113,3.11346560450989,-324.812618060399)) ;
#40857 = CARTESIAN_POINT('Ctrl Pts',(18.3385699601185,2.90451105038135,-324.815235702515)) ;
#40858 = CARTESIAN_POINT('Ctrl Pts',(18.4602769642495,2.07495238479324,-324.825553387073)) ;
#40859 = CARTESIAN_POINT('Ctrl Pts',(18.5197942068525,1.45068150627204,-324.833167486342)) ;
#40860 = CARTESIAN_POINT('Ctrl Pts',(18.5601405522589,0.543174177248273,-324.844443663741)) ;
#40861 = CARTESIAN_POINT('Ctrl Pts',(18.5662454908204,0.261502216244568,-324.847969864823)) ;
#40862 = CARTESIAN_POINT('Ctrl Pts',(18.56578249821,-0.164059476479644,-324.853357772871)) ;
#40863 = CARTESIAN_POINT('Ctrl Pts',(18.5639539073582,-0.307913188073675,
-324.855189351218)) ;
#40864 = CARTESIAN_POINT('Ctrl Pts',(18.5574578308975,-0.57482012306736,-324.858608602313)) ;
#40865 = CARTESIAN_POINT('Ctrl Pts',(18.5532376662952,-0.69787632684319,-324.860193286471)) ;
#40866 = CARTESIAN_POINT('Ctrl Pts',(18.5467890391715,-0.843582900306995,
-324.862079777443)) ;
#40867 = CARTESIAN_POINT('Ctrl Pts',(18.5457426493003,-0.866282487621405,
-324.862373963682)) ;
#40868 = CARTESIAN_POINT('Ctrl Pts',(18.544654593743,-0.888979977990137,-324.862668413757)) ;
#40869 = CARTESIAN_POINT('Origin',(0.,0.,-315.477129595899)) ;
#40870 = CARTESIAN_POINT('',(18.5446545943314,-0.888979965716109,-326.659259832385)) ;
#40871 = CARTESIAN_POINT('',(18.5446545937382,-0.888979978089839,-326.364137692133)) ;
#40872 = CARTESIAN_POINT('',(18.544654593745,-0.888979977948782,-315.477129595899)) ;
#40873 = CARTESIAN_POINT('Ctrl Pts',(18.5446545943314,-0.888979965716149,
-326.659259832385)) ;
#40874 = CARTESIAN_POINT('Ctrl Pts',(18.5702422063668,-0.355207051375194,
-326.652714073557)) ;
#40875 = CARTESIAN_POINT('Ctrl Pts',(18.5727724921029,0.179411176510274,-326.646152532977)) ;
#40876 = CARTESIAN_POINT('Ctrl Pts',(18.5466431199678,0.858914281140881,-326.637624094489)) ;
#40877 = CARTESIAN_POINT('Ctrl Pts',(18.5393358311989,1.00435632427266,-326.635788225339)) ;
#40878 = CARTESIAN_POINT('Ctrl Pts',(18.5230476142734,1.26688270475765,-326.632452823504)) ;
#40879 = CARTESIAN_POINT('Ctrl Pts',(18.514665493499,1.38399650655875,-326.630957117559)) ;
#40880 = CARTESIAN_POINT('Ctrl Pts',(18.4951421688321,1.62468738571748,-326.627866089292)) ;
#40881 = CARTESIAN_POINT('Ctrl Pts',(18.483871920925,1.74824818218474,-326.62627000416)) ;
#40882 = CARTESIAN_POINT('Ctrl Pts',(18.45563439337,2.02691964757025,-326.622648627966)) ;
#40883 = CARTESIAN_POINT('Ctrl Pts',(18.4379485501066,2.18194804773963,-326.62061879637)) ;
#40884 = CARTESIAN_POINT('Ctrl Pts',(18.3756626173753,2.672890198652,-326.614142720018)) ;
#40885 = CARTESIAN_POINT('Ctrl Pts',(18.3238197963312,3.00781412503908,-326.609652028375)) ;
#40886 = CARTESIAN_POINT('Ctrl Pts',(18.2545435802755,3.38648249859851,-326.604507495274)) ;
#40887 = CARTESIAN_POINT('Ctrl Pts',(18.2460776868003,3.43180332816606,-326.603890697157)) ;
#40888 = CARTESIAN_POINT('Ctrl Pts',(18.1953862252423,3.69768142571455,-326.60026623038)) ;
#40889 = CARTESIAN_POINT('Ctrl Pts',(18.1493306951165,3.9174893763584,-326.597245379007)) ;
#40890 = CARTESIAN_POINT('Ctrl Pts',(18.0146054177974,4.50699442595136,-326.589101444833)) ;
#40891 = CARTESIAN_POINT('Ctrl Pts',(17.9185497858009,4.87489291921913,-326.583972460105)) ;
#40892 = CARTESIAN_POINT('Ctrl Pts',(17.7523660031536,5.43981269911378,-326.576122075417)) ;
#40893 = CARTESIAN_POINT('Ctrl Pts',(17.690091548706,5.63903557280363,-326.573359005911)) ;
#40894 = CARTESIAN_POINT('Ctrl Pts',(17.6218590374155,5.84505367837416,-326.570521465574)) ;
#40895 = CARTESIAN_POINT('Ctrl Pts',(17.619241461581,5.85293932619718,-326.570412885097)) ;
#40896 = CARTESIAN_POINT('Ctrl Pts',(17.6145941848183,5.86690823452684,-326.570220597726)) ;
#40897 = CARTESIAN_POINT('Ctrl Pts',(17.6125666240029,5.87299220527856,-326.570136868314)) ;
#40898 = CARTESIAN_POINT('Ctrl Pts',(17.6089240296833,5.88390345181218,-326.569986738948)) ;
#40899 = CARTESIAN_POINT('Ctrl Pts',(17.6073101624236,5.88873111609163,-326.569920326542)) ;
#40900 = CARTESIAN_POINT('Ctrl Pts',(17.60437781623,5.89749084827315,-326.569799844474)) ;
#40901 = CARTESIAN_POINT('Ctrl Pts',(17.6030600048481,5.90142313918915,-326.569745767603)) ;
#40902 = CARTESIAN_POINT('Ctrl Pts',(17.6006398919603,5.90863662593557,-326.56964658294)) ;
#40903 = CARTESIAN_POINT('Ctrl Pts',(17.5995379902297,5.91191795564468,-326.56960147079)) ;
#40904 = CARTESIAN_POINT('Ctrl Pts',(17.5974939402152,5.91799925262315,-326.569517875161)) ;
#40905 = CARTESIAN_POINT('Ctrl Pts',(17.5965520411652,5.92079930351666,-326.569479388944)) ;
#40906 = CARTESIAN_POINT('Ctrl Pts',(17.5947881058356,5.92603894187128,-326.56940737907)) ;
#40907 = CARTESIAN_POINT('Ctrl Pts',(17.5939662303993,5.92847858336349,-326.569373853634)) ;
#40908 = CARTESIAN_POINT('Ctrl Pts',(17.5924130576212,5.93308582828845,-326.56931054732)) ;
#40909 = CARTESIAN_POINT('Ctrl Pts',(17.5916818670251,5.93525346764398,-326.569280765255)) ;
#40910 = CARTESIAN_POINT('Ctrl Pts',(17.5902879659944,5.93938321418496,-326.56922403001)) ;
#40911 = CARTESIAN_POINT('Ctrl Pts',(17.5896253278628,5.94134534570729,-326.569197076022)) ;
#40912 = CARTESIAN_POINT('Ctrl Pts',(17.5883513407013,5.94511565588149,-326.569145287071)) ;
#40913 = CARTESIAN_POINT('Ctrl Pts',(17.5877400411056,5.9469238512234,-326.569120451551)) ;
#40914 = CARTESIAN_POINT('Ctrl Pts',(17.586554877157,5.95042772915556,-326.569072329457)) ;
#40915 = CARTESIAN_POINT('Ctrl Pts',(17.5859810463725,5.95212342309748,-326.569049042504)) ;
#40916 = CARTESIAN_POINT('Ctrl Pts',(17.5848591748378,5.95543702188073,-326.569003540073)) ;
#40917 = CARTESIAN_POINT('Ctrl Pts',(17.5843111560446,5.9570549340988,-326.568981324347)) ;
#40918 = CARTESIAN_POINT('Ctrl Pts',(17.566008770633,6.01106441208532,-326.568239764466)) ;
#40919 = CARTESIAN_POINT('Ctrl Pts',(17.5480205488011,6.06337647875357,-326.567523081235)) ;
#40920 = CARTESIAN_POINT('Ctrl Pts',(17.5078787163113,6.17843917006968,-326.565950797208)) ;
#40921 = CARTESIAN_POINT('Ctrl Pts',(17.4856210375909,6.24115250942391,-326.565096699864)) ;
#40922 = CARTESIAN_POINT('Ctrl Pts',(17.4293678128239,6.39698869552229,-326.562980569414)) ;
#40923 = CARTESIAN_POINT('Ctrl Pts',(17.3949626681717,6.48996152066947,-326.561723467072)) ;
#40924 = CARTESIAN_POINT('Ctrl Pts',(17.2351266824184,6.91148191241109,-326.556040017663)) ;
#40925 = CARTESIAN_POINT('Ctrl Pts',(17.101120758108,7.23670118052104,-326.551698157677)) ;
#40926 = CARTESIAN_POINT('Ctrl Pts',(16.7448329160087,8.0361163555858,-326.540949882988)) ;
#40927 = CARTESIAN_POINT('Ctrl Pts',(16.511574965163,8.50508600406551,-326.534571802745)) ;
#40928 = CARTESIAN_POINT('Ctrl Pts',(16.1519310108722,9.15743586826784,-326.525351560858)) ;
#40929 = CARTESIAN_POINT('Ctrl Pts',(16.0415924164435,9.34937535865893,-326.522595087342)) ;
#40930 = CARTESIAN_POINT('Ctrl Pts',(15.8384209931595,9.68861252247362,-326.517630632447)) ;
#40931 = CARTESIAN_POINT('Ctrl Pts',(15.7468988641999,9.83666448547054,-326.515431683849)) ;
#40932 = CARTESIAN_POINT('Ctrl Pts',(15.5936916158589,10.076883103105,-326.511806487052)) ;
#40933 = CARTESIAN_POINT('Ctrl Pts',(15.5332384647051,10.1698227146273,-326.510389597768)) ;
#40934 = CARTESIAN_POINT('Ctrl Pts',(15.4024648629208,10.3669851638398,-326.507352293127)) ;
#40935 = CARTESIAN_POINT('Ctrl Pts',(15.3319108663188,10.471046479457,-326.505730113518)) ;
#40936 = CARTESIAN_POINT('Ctrl Pts',(15.1735482171346,10.6995858073751,-326.502124446477)) ;
#40937 = CARTESIAN_POINT('Ctrl Pts',(15.085253538371,10.8237159764185,-326.500137257167)) ;
#40938 = CARTESIAN_POINT('Ctrl Pts',(14.5570270395417,11.5473090846212,-326.488384048818)) ;
#40939 = CARTESIAN_POINT('Ctrl Pts',(14.0829310810694,12.1209911281496,-326.478342376394)) ;
#40940 = CARTESIAN_POINT('Ctrl Pts',(13.3932588240344,12.8602745641086,-326.464739468862)) ;
#40941 = CARTESIAN_POINT('Ctrl Pts',(13.2065943173152,13.0518929900552,-326.46115082963)) ;
#40942 = CARTESIAN_POINT('Ctrl Pts',(12.8929419144747,13.360249157689,-326.455310856005)) ;
#40943 = CARTESIAN_POINT('Ctrl Pts',(12.7683518055667,13.4793694627025,-326.453038165669)) ;
#40944 = CARTESIAN_POINT('Ctrl Pts',(12.5838629515905,13.6509054922516,-326.449752206078)) ;
#40945 = CARTESIAN_POINT('Ctrl Pts',(12.5252573541044,13.7046983104199,-326.448719802299)) ;
#40946 = CARTESIAN_POINT('Ctrl Pts',(12.4169416075096,13.8028438519424,-326.446834117313)) ;
#40947 = CARTESIAN_POINT('Ctrl Pts',(12.3673351190881,13.8473087396007,-326.445979180319)) ;
#40948 = CARTESIAN_POINT('Ctrl Pts',(12.2428914497442,13.9576519756633,-326.443855069296)) ;
#40949 = CARTESIAN_POINT('Ctrl Pts',(12.1677608674609,14.0231963274567,-326.442590918102)) ;
#40950 = CARTESIAN_POINT('Ctrl Pts',(11.8247366995782,14.3176203473069,-326.436892584026)) ;
#40951 = CARTESIAN_POINT('Ctrl Pts',(11.5508880035671,14.5394510876483,-326.432542916145)) ;
#40952 = CARTESIAN_POINT('Ctrl Pts',(10.7303469441769,15.1663071700223,-326.41986282476)) ;
#40953 = CARTESIAN_POINT('Ctrl Pts',(10.1675134962265,15.5492407772484,-326.411587461683)) ;
#40954 = CARTESIAN_POINT('Ctrl Pts',(9.39869396794216,16.0126932005314,-326.400367003105)) ;
#40955 = CARTESIAN_POINT('Ctrl Pts',(9.21048987678015,16.1216831573904,-326.39762857707)) ;
#40956 = CARTESIAN_POINT('Ctrl Pts',(8.90409312310711,16.2920022347175,-326.393175143229)) ;
#40957 = CARTESIAN_POINT('Ctrl Pts',(8.78707956293618,16.355410231906,-326.391475513213)) ;
#40958 = CARTESIAN_POINT('Ctrl Pts',(8.55787312328783,16.4764441553734,-326.388147200498)) ;
#40959 = CARTESIAN_POINT('Ctrl Pts',(8.44575471700162,16.5341958258056,-326.386519554103)) ;
#40960 = CARTESIAN_POINT('Ctrl Pts',(8.19528711927791,16.6599981149077,-326.382883923964)) ;
#40961 = CARTESIAN_POINT('Ctrl Pts',(8.0566611076429,16.7274767929147,-326.380872003315)) ;
#40962 = CARTESIAN_POINT('Ctrl Pts',(7.26196858210809,17.1021368020462,-326.369341641724)) ;
#40963 = CARTESIAN_POINT('Ctrl Pts',(6.5892096713528,17.372437309749,-326.359564639076)) ;
#40964 = CARTESIAN_POINT('Ctrl Pts',(5.64032792335114,17.6906075851473,-326.346095571732)) ;
#40965 = CARTESIAN_POINT('Ctrl Pts',(5.37633879341372,17.772615938546,-326.342385124817)) ;
#40966 = CARTESIAN_POINT('Ctrl Pts',(4.94145820108379,17.8971352738967,-326.336376498875)) ;
#40967 = CARTESIAN_POINT('Ctrl Pts',(4.77161885327615,17.9431634298683,-326.334055541009)) ;
#40968 = CARTESIAN_POINT('Ctrl Pts',(4.52352632433165,18.0066273589065,-326.330714535729)) ;
#40969 = CARTESIAN_POINT('Ctrl Pts',(4.44577410134282,18.0259815797391,-326.329674481122)) ;
#40970 = CARTESIAN_POINT('Ctrl Pts',(4.30327980514069,18.0604734881682,-326.327782788929)) ;
#40971 = CARTESIAN_POINT('Ctrl Pts',(4.23857722064267,18.0757678353135,-326.326929394153)) ;
#40972 = CARTESIAN_POINT('Ctrl Pts',(4.07767718010205,18.1128898405443,-326.32482013969)) ;
#40973 = CARTESIAN_POINT('Ctrl Pts',(3.98138524884317,18.1342990242823,-326.32356913125)) ;
#40974 = CARTESIAN_POINT('Ctrl Pts',(3.54411157924823,18.2278700515585,-326.317930795708)) ;
#40975 = CARTESIAN_POINT('Ctrl Pts',(3.20130899250581,18.2911890096435,-326.313626614084)) ;
#40976 = CARTESIAN_POINT('Ctrl Pts',(2.4490191149513,18.4083467278719,-326.304275287859)) ;
#40977 = CARTESIAN_POINT('Ctrl Pts',(2.03910579866791,18.4582494188925,-326.29923915226)) ;
#40978 = CARTESIAN_POINT('Ctrl Pts',(1.35354318610097,18.5185922456493,-326.290766707481)) ;
#40979 = CARTESIAN_POINT('Ctrl Pts',(1.0787129409124,18.5366317322611,-326.28735772443)) ;
#40980 = CARTESIAN_POINT('Ctrl Pts',(0.587407543280188,18.5579166830495,-326.281210249343)) ;
#40981 = CARTESIAN_POINT('Ctrl Pts',(0.371084524128882,18.5635022362768,-326.278485220141)) ;
#40982 = CARTESIAN_POINT('Ctrl Pts',(0.0218245807144408,18.5664127883284,
-326.274047731639)) ;
#40983 = CARTESIAN_POINT('Ctrl Pts',(-0.111072437788727,18.5660933691244,
-326.272350435225)) ;
#40984 = CARTESIAN_POINT('Ctrl Pts',(-0.370170199780886,18.5626885605346,
-326.269022951226)) ;
#40985 = CARTESIAN_POINT('Ctrl Pts',(-0.496365646296472,18.559742823209,-326.267393758474)) ;
#40986 = CARTESIAN_POINT('Ctrl Pts',(-0.777119648939183,18.5503237724084,
-326.263749762074)) ;
#40987 = CARTESIAN_POINT('Ctrl Pts',(-0.931647146692736,18.5432052382465,
-326.261730955827)) ;
#40988 = CARTESIAN_POINT('Ctrl Pts',(-1.8009580869145,18.4922652173002,-326.250301564516)) ;
#40989 = CARTESIAN_POINT('Ctrl Pts',(-2.51282418618556,18.4090474805044,-326.240639439739)) ;
#40990 = CARTESIAN_POINT('Ctrl Pts',(-3.49464427836755,18.2362498565568,-326.227221123847)) ;
#40991 = CARTESIAN_POINT('Ctrl Pts',(-3.77005337844767,18.1813103295154,-326.223450586582)) ;
#40992 = CARTESIAN_POINT('Ctrl Pts',(-4.16710563498376,18.0926949732638,-326.218045736527)) ;
#40993 = CARTESIAN_POINT('Ctrl Pts',(-4.28981836909148,18.0639928917663,-326.216379755157)) ;
#40994 = CARTESIAN_POINT('Ctrl Pts',(-4.51156964292605,18.0097389750561,-326.213382695124)) ;
#40995 = CARTESIAN_POINT('Ctrl Pts',(-4.61070742624884,17.9846138592863,-326.212047730927)) ;
#40996 = CARTESIAN_POINT('Ctrl Pts',(-4.77440867459764,17.9416834694386,-326.209854408829)) ;
#40997 = CARTESIAN_POINT('Ctrl Pts',(-4.83909239497691,17.9243456991353,-326.208990675937)) ;
#40998 = CARTESIAN_POINT('Ctrl Pts',(-4.9791715631619,17.8859854668682,-326.207127255513)) ;
#40999 = CARTESIAN_POINT('Ctrl Pts',(-5.05453060564233,17.8648354583893,-326.206129032033)) ;
#41000 = CARTESIAN_POINT('Ctrl Pts',(-5.28793031347417,17.797735253399,-326.203047625619)) ;
#41001 = CARTESIAN_POINT('Ctrl Pts',(-5.44549550112615,17.7501596065228,-326.200982006097)) ;
#41002 = CARTESIAN_POINT('Ctrl Pts',(-6.21918421964404,17.5052783544626,-326.190870663147)) ;
#41003 = CARTESIAN_POINT('Ctrl Pts',(-6.82533717852088,17.2779570472,-326.183031673085)) ;
#41004 = CARTESIAN_POINT('Ctrl Pts',(-7.6708904691481,16.9094000598681,-326.171676439278)) ;
#41005 = CARTESIAN_POINT('Ctrl Pts',(-7.92091349192079,16.793733953377,-326.168266732856)) ;
#41006 = CARTESIAN_POINT('Ctrl Pts',(-8.36261070861343,16.5773361903279,-326.162118134227)) ;
#41007 = CARTESIAN_POINT('Ctrl Pts',(-8.55527150335354,16.478733637576,-326.159392713031)) ;
#41008 = CARTESIAN_POINT('Ctrl Pts',(-8.86339297025271,16.31417870092,-326.154954758)) ;
#41009 = CARTESIAN_POINT('Ctrl Pts',(-8.97994602007168,16.2503147983607,-326.153257393324)) ;
#41010 = CARTESIAN_POINT('Ctrl Pts',(-9.20584071920047,16.1233659137424,-326.149929885715)) ;
#41011 = CARTESIAN_POINT('Ctrl Pts',(-9.31524462156906,16.0604062626797,-326.148300738834)) ;
#41012 = CARTESIAN_POINT('Ctrl Pts',(-9.55726109582829,15.9178259398387,-326.144656989978)) ;
#41013 = CARTESIAN_POINT('Ctrl Pts',(-9.68953786781783,15.8376538071998,-326.142638387349)) ;
#41014 = CARTESIAN_POINT('Ctrl Pts',(-10.4286486151118,15.3769574820544,-326.131207300683)) ;
#41015 = CARTESIAN_POINT('Ctrl Pts',(-11.0140633690426,14.9632193418172,-326.121543149781)) ;
#41016 = CARTESIAN_POINT('Ctrl Pts',(-11.7936083460349,14.3416913768626,-326.10812379406)) ;
#41017 = CARTESIAN_POINT('Ctrl Pts',(-12.009114379439,14.1617259365412,-326.104354183358)) ;
#41018 = CARTESIAN_POINT('Ctrl Pts',(-12.3542122520213,13.8599966111326,-326.098264055128)) ;
#41019 = CARTESIAN_POINT('Ctrl Pts',(-12.48628243131,13.7411359670686,-326.095920057442)) ;
#41020 = CARTESIAN_POINT('Ctrl Pts',(-12.6756054536784,13.5657653318055,-326.092552832867)) ;
#41021 = CARTESIAN_POINT('Ctrl Pts',(-12.7342291392633,13.5107501978132,-326.091509176399)) ;
#41022 = CARTESIAN_POINT('Ctrl Pts',(-12.8406361853493,13.4095851697791,-326.089614595448)) ;
#41023 = CARTESIAN_POINT('Ctrl Pts',(-12.8885325897359,13.3635564034161,-326.08876186636)) ;
#41024 = CARTESIAN_POINT('Ctrl Pts',(-13.006591309621,13.2488760826904,-326.086659318651)) ;
#41025 = CARTESIAN_POINT('Ctrl Pts',(-13.0764581698007,13.1799232442338,-326.085414273528)) ;
#41026 = CARTESIAN_POINT('Ctrl Pts',(-13.3995577289955,12.8559523678614,-326.079644412894)) ;
#41027 = CARTESIAN_POINT('Ctrl Pts',(-13.6458989686736,12.5941693338738,-326.075208682264)) ;
#41028 = CARTESIAN_POINT('Ctrl Pts',(-14.2294065348734,11.9368517359364,-326.064416600158)) ;
#41029 = CARTESIAN_POINT('Ctrl Pts',(-14.5578643461038,11.5339943484771,-326.058085891049)) ;
#41030 = CARTESIAN_POINT('Ctrl Pts',(-14.9594024389937,10.9969801353638,-326.049785597036)) ;
#41031 = CARTESIAN_POINT('Ctrl Pts',(-15.0483339890011,10.8749683917046,-326.047909099209)) ;
#41032 = CARTESIAN_POINT('Ctrl Pts',(-15.2635443671719,10.5720099775238,-326.043266087132)) ;
#41033 = CARTESIAN_POINT('Ctrl Pts',(-15.3881044935754,10.3898710992468,-326.040488655063)) ;
#41034 = CARTESIAN_POINT('Ctrl Pts',(-15.582851568487,10.0939138656749,-326.035988783594)) ;
#41035 = CARTESIAN_POINT('Ctrl Pts',(-15.6551069734793,9.98148214042663,-326.034282354213)) ;
#41036 = CARTESIAN_POINT('Ctrl Pts',(-15.793012260236,9.76171556594236,-326.030951385076)) ;
#41037 = CARTESIAN_POINT('Ctrl Pts',(-15.8587974654798,9.65447408914743,-326.029328000152)) ;
#41038 = CARTESIAN_POINT('Ctrl Pts',(-16.0170810902115,9.39046023910958,-326.025335907065)) ;
#41039 = CARTESIAN_POINT('Ctrl Pts',(-16.1083736941177,9.23298039244086,-326.022958417826)) ;
#41040 = CARTESIAN_POINT('Ctrl Pts',(-16.381599723417,8.74527441109101,-326.015608539778)) ;
#41041 = CARTESIAN_POINT('Ctrl Pts',(-16.555802027992,8.41082945303235,-326.010584770084)) ;
#41042 = CARTESIAN_POINT('Ctrl Pts',(-16.939572203885,7.61585078792967,-325.998738922389)) ;
#41043 = CARTESIAN_POINT('Ctrl Pts',(-17.140740743884,7.15159393811239,-325.991890758873)) ;
#41044 = CARTESIAN_POINT('Ctrl Pts',(-17.3837722925309,6.52133204527432,-325.982861709737)) ;
#41045 = CARTESIAN_POINT('Ctrl Pts',(-17.4426667779594,6.36212909056034,-325.980603879529)) ;
#41046 = CARTESIAN_POINT('Ctrl Pts',(-17.5417503100744,6.08256443238945,-325.976691022803)) ;
#41047 = CARTESIAN_POINT('Ctrl Pts',(-17.5829039898309,5.96255661439531,-325.975027910837)) ;
#41048 = CARTESIAN_POINT('Ctrl Pts',(-17.6452860752128,5.77438083737191,-325.97245093015)) ;
#41049 = CARTESIAN_POINT('Ctrl Pts',(-17.6673567496207,5.7064963182646,-325.971527512036)) ;
#41050 = CARTESIAN_POINT('Ctrl Pts',(-17.7078934305089,5.57932481095569,-325.96981040179)) ;
#41051 = CARTESIAN_POINT('Ctrl Pts',(-17.7264545574453,5.52006919564338,-325.969015484401)) ;
#41052 = CARTESIAN_POINT('Ctrl Pts',(-17.7781449657395,5.35210023507433,-325.966775424559)) ;
#41053 = CARTESIAN_POINT('Ctrl Pts',(-17.8105738322309,5.2431741507874,-325.965338421063)) ;
#41054 = CARTESIAN_POINT('Ctrl Pts',(-17.9369822407852,4.80386800580374,-325.959594341586)) ;
#41055 = CARTESIAN_POINT('Ctrl Pts',(-18.022785547168,4.47120586104699,-325.955360058512)) ;
#41056 = CARTESIAN_POINT('Ctrl Pts',(-18.1100359699961,4.089427076147,-325.95055377847)) ;
#41057 = CARTESIAN_POINT('Ctrl Pts',(-18.1205781502291,4.04245768659571,-325.949963407682)) ;
#41058 = CARTESIAN_POINT('Ctrl Pts',(-18.2333454410775,3.53073114275622,-325.943539786307)) ;
#41059 = CARTESIAN_POINT('Ctrl Pts',(-18.3178486685681,3.06224890478948,-325.937729187379)) ;
#41060 = CARTESIAN_POINT('Ctrl Pts',(-18.4043699910721,2.44835224005511,-325.930046597674)) ;
#41061 = CARTESIAN_POINT('Ctrl Pts',(-18.4228181606848,2.3054358417705,-325.928253731138)) ;
#41062 = CARTESIAN_POINT('Ctrl Pts',(-18.4645012095539,1.94997549001014,-325.923778252274)) ;
#41063 = CARTESIAN_POINT('Ctrl Pts',(-18.4857318945998,1.73721772416478,-325.921084958796)) ;
#41064 = CARTESIAN_POINT('Ctrl Pts',(-18.51415571375,1.39214863794356,-325.916685232276)) ;
#41065 = CARTESIAN_POINT('Ctrl Pts',(-18.5236154497839,1.26004374161199,-325.914993457558)) ;
#41066 = CARTESIAN_POINT('Ctrl Pts',(-18.5393458383045,1.00157810739283,-325.911667751798)) ;
#41067 = CARTESIAN_POINT('Ctrl Pts',(-18.5457399875305,0.875232013981004,
-325.910034715701)) ;
#41068 = CARTESIAN_POINT('Ctrl Pts',(-18.5571323764447,0.593007407846611,
-325.906370108546)) ;
#41069 = CARTESIAN_POINT('Ctrl Pts',(-18.5614588160241,0.437111364842863,
-325.90433437286)) ;
#41070 = CARTESIAN_POINT('Ctrl Pts',(-18.5700970366831,-0.133194697888188,
-325.896846369808)) ;
#41071 = CARTESIAN_POINT('Ctrl Pts',(-18.5624974019311,-0.547661784826543,
-325.891323016749)) ;
#41072 = CARTESIAN_POINT('Ctrl Pts',(-18.5114109501745,-1.53275856261004,
-325.8780790217)) ;
#41073 = CARTESIAN_POINT('Ctrl Pts',(-18.4554042895828,-2.10231683343467,
-325.870323690852)) ;
#41074 = CARTESIAN_POINT('Ctrl Pts',(-18.3469444322849,-2.84912022771885,
-325.860292388118)) ;
#41075 = CARTESIAN_POINT('Ctrl Pts',(-18.3180292749973,-3.02946525953145,
-325.857881615642)) ;
#41076 = CARTESIAN_POINT('Ctrl Pts',(-18.2724276300795,-3.28929712620997,
-325.854438603977)) ;
#41077 = CARTESIAN_POINT('Ctrl Pts',(-18.2578732486684,-3.3691470049838,-325.853384689805)) ;
#41078 = CARTESIAN_POINT('Ctrl Pts',(-18.230483175355,-3.51402556500913,-325.851481682665)) ;
#41079 = CARTESIAN_POINT('Ctrl Pts',(-18.2178219990464,-3.57908564931561,
-325.850630651104)) ;
#41080 = CARTESIAN_POINT('Ctrl Pts',(-18.1858030504711,-3.73904358055901,
-325.848546263465)) ;
#41081 = CARTESIAN_POINT('Ctrl Pts',(-18.1660505832882,-3.83386042159679,
-325.847317469275)) ;
#41082 = CARTESIAN_POINT('Ctrl Pts',(-18.0768390809548,-4.24592222860317,
-325.841999027531)) ;
#41083 = CARTESIAN_POINT('Ctrl Pts',(-17.9998046331222,-4.56146915516987,
-325.837981621989)) ;
#41084 = CARTESIAN_POINT('Ctrl Pts',(-17.889963720349,-4.96512371569965,-325.832838182341)) ;
#41085 = CARTESIAN_POINT('Ctrl Pts',(-17.8647119738382,-5.05522714890954,
-325.831689867123)) ;
#41086 = CARTESIAN_POINT('Ctrl Pts',(-17.7417810987431,-5.48144268944366,
-325.826251268971)) ;
#41087 = CARTESIAN_POINT('Ctrl Pts',(-17.6352910712944,-5.81493932203858,
-325.821974450875)) ;
#41088 = CARTESIAN_POINT('Ctrl Pts',(-17.4288080493247,-6.40360223279718,
-325.814293693695)) ;
#41089 = CARTESIAN_POINT('Ctrl Pts',(-17.3324737214144,-6.6599418875261,-325.810903726065)) ;
#41090 = CARTESIAN_POINT('Ctrl Pts',(-17.1502374091235,-7.11409260197304,
-325.804785802981)) ;
#41091 = CARTESIAN_POINT('Ctrl Pts',(-17.0664920831776,-7.31271526038314,
-325.802071096228)) ;
#41092 = CARTESIAN_POINT('Ctrl Pts',(-16.9256125246196,-7.63123591231291,
-325.797645892108)) ;
#41093 = CARTESIAN_POINT('Ctrl Pts',(-16.8706170308459,-7.75205790872377,
-325.795950392814)) ;
#41094 = CARTESIAN_POINT('Ctrl Pts',(-16.7607708984117,-7.9866772665144,-325.792623516394)) ;
#41095 = CARTESIAN_POINT('Ctrl Pts',(-16.7060451800202,-8.10052524579647,
-325.790993101869)) ;
#41096 = CARTESIAN_POINT('Ctrl Pts',(-16.568180719477,-8.37998955989924,-325.786950548933)) ;
#41097 = CARTESIAN_POINT('Ctrl Pts',(-16.4837161701132,-8.54493642082568,
-325.784529086427)) ;
#41098 = CARTESIAN_POINT('Ctrl Pts',(-16.0971887345808,-9.27270188725517,
-325.77368933117)) ;
#41099 = CARTESIAN_POINT('Ctrl Pts',(-15.7686699157909,-9.82097393334736,
-325.76508662222)) ;
#41100 = CARTESIAN_POINT('Ctrl Pts',(-15.2393019446545,-10.6091816656868,
-325.752299203636)) ;
#41101 = CARTESIAN_POINT('Ctrl Pts',(-15.0596028902879,-10.8627538175177,
-325.748119529675)) ;
#41102 = CARTESIAN_POINT('Ctrl Pts',(-14.7604916413494,-11.2631308876633,
-325.741471638564)) ;
#41103 = CARTESIAN_POINT('Ctrl Pts',(-14.6450524638065,-11.4128291603238,
-325.738974913005)) ;
#41104 = CARTESIAN_POINT('Ctrl Pts',(-14.476208365781,-11.625000452875,-325.735434785477)) ;
#41105 = CARTESIAN_POINT('Ctrl Pts',(-14.4246434895597,-11.688922294351,-325.734368059087)) ;
#41106 = CARTESIAN_POINT('Ctrl Pts',(-14.330797302,-11.8036909810578,-325.732454144424)) ;
#41107 = CARTESIAN_POINT('Ctrl Pts',(-14.2886653675355,-11.8546579073339,
-325.731604852189)) ;
#41108 = CARTESIAN_POINT('Ctrl Pts',(-14.1851332911785,-11.9785466666369,
-325.729541349712)) ;
#41109 = CARTESIAN_POINT('Ctrl Pts',(-14.1234420912199,-12.0512227706054,
-325.728331455586)) ;
#41110 = CARTESIAN_POINT('Ctrl Pts',(-13.8648347674357,-12.351165157706,-325.723333613264)) ;
#41111 = CARTESIAN_POINT('Ctrl Pts',(-13.6629711230557,-12.5741061212602,
-325.719607369629)) ;
#41112 = CARTESIAN_POINT('Ctrl Pts',(-13.3635368286466,-12.8890770409518,
-325.714257690539)) ;
#41113 = CARTESIAN_POINT('Ctrl Pts',(-13.2702451301722,-12.9851075370062,
-325.712614800457)) ;
#41114 = CARTESIAN_POINT('Ctrl Pts',(-12.8433961009566,-13.4150829235332,
-325.705188382038)) ;
#41115 = CARTESIAN_POINT('Ctrl Pts',(-12.4982168866682,-13.7372430895527,
-325.699423992928)) ;
#41116 = CARTESIAN_POINT('Ctrl Pts',(-12.0326121885731,-14.139707253328,-325.691796667802)) ;
#41117 = CARTESIAN_POINT('Ctrl Pts',(-11.9230029593247,-14.2322548341958,
-325.690011675223)) ;
#41118 = CARTESIAN_POINT('Ctrl Pts',(-11.6478909787771,-14.4591343655779,
-325.685552069738)) ;
#41119 = CARTESIAN_POINT('Ctrl Pts',(-11.481126753129,-14.5919038890302,-325.682866800028)) ;
#41120 = CARTESIAN_POINT('Ctrl Pts',(-11.2071875306039,-14.8023969982428,
-325.678476618034)) ;
#41121 = CARTESIAN_POINT('Ctrl Pts',(-11.1014024729739,-14.8818974701496,
-325.676786237508)) ;
#41122 = CARTESIAN_POINT('Ctrl Pts',(-10.8927813662166,-15.0352198355038,
-325.67346093801)) ;
#41123 = CARTESIAN_POINT('Ctrl Pts',(-10.790022231546,-15.1091343756911,-325.671826888349)) ;
#41124 = CARTESIAN_POINT('Ctrl Pts',(-10.5587196351409,-15.2719469179462,
-325.668156886081)) ;
#41125 = CARTESIAN_POINT('Ctrl Pts',(-10.4297933317919,-15.3602843058016,
-325.666116726378)) ;
#41126 = CARTESIAN_POINT('Ctrl Pts',(-9.7132229859223,-15.8380803673515,-325.654809199395)) ;
#41127 = CARTESIAN_POINT('Ctrl Pts',(-9.10488067770076,-16.1954509180499,
-325.645300089706)) ;
#41128 = CARTESIAN_POINT('Ctrl Pts',(-8.10600976264098,-16.7081312894147,
-325.630186152228)) ;
#41129 = CARTESIAN_POINT('Ctrl Pts',(-7.72798763877837,-16.8863037300734,
-325.624579423746)) ;
#41130 = CARTESIAN_POINT('Ctrl Pts',(-7.25212406730502,-17.0912627823632,
-325.617780427003)) ;
#41131 = CARTESIAN_POINT('Ctrl Pts',(-7.15965064798743,-17.1302063509282,
-325.616471214611)) ;
#41132 = CARTESIAN_POINT('Ctrl Pts',(-7.00518674697434,-17.1937868704601,
-325.614307034721)) ;
#41133 = CARTESIAN_POINT('Ctrl Pts',(-6.9433710771508,-17.2188427726664,-325.613447003777)) ;
#41134 = CARTESIAN_POINT('Ctrl Pts',(-6.80784554966059,-17.272927196313,-325.611575351122)) ;
#41135 = CARTESIAN_POINT('Ctrl Pts',(-6.73408234506195,-17.301818111114,-325.610565365285)) ;
#41136 = CARTESIAN_POINT('Ctrl Pts',(-6.50115134899761,-17.3913351960528,
-325.607400274459)) ;
#41137 = CARTESIAN_POINT('Ctrl Pts',(-6.34133275225464,-17.4502437766335,
-325.605264103372)) ;
#41138 = CARTESIAN_POINT('Ctrl Pts',(-6.06650171124781,-17.5472712922293,
-325.601635355937)) ;
#41139 = CARTESIAN_POINT('Ctrl Pts',(-5.95188532901854,-17.5864787233345,
-325.600135179089)) ;
#41140 = CARTESIAN_POINT('Ctrl Pts',(-5.26415783401835,-17.8142399666871,
-325.591194184243)) ;
#41141 = CARTESIAN_POINT('Ctrl Pts',(-4.68251674137203,-17.9758877990413,
-325.583869552335)) ;
#41142 = CARTESIAN_POINT('Ctrl Pts',(-3.9358674414343,-18.1446891396433,-325.574408967758)) ;
#41143 = CARTESIAN_POINT('Ctrl Pts',(-3.77723391141671,-18.1783745256108,
-325.57239660554)) ;
#41144 = CARTESIAN_POINT('Ctrl Pts',(-3.51105965157956,-18.2312612622896,
-325.569010416946)) ;
#41145 = CARTESIAN_POINT('Ctrl Pts',(-3.40375405195838,-18.2515995303417,
-325.567642728785)) ;
#41146 = CARTESIAN_POINT('Ctrl Pts',(-3.12248502091476,-18.3023433694199,
-325.564048907471)) ;
#41147 = CARTESIAN_POINT('Ctrl Pts',(-2.94825644327139,-18.3312157078248,
-325.561813873351)) ;
#41148 = CARTESIAN_POINT('Ctrl Pts',(-2.64880250539709,-18.376460092909,-325.557953169476)) ;
#41149 = CARTESIAN_POINT('Ctrl Pts',(-2.52377325041383,-18.394048189186,-325.556335531848)) ;
#41150 = CARTESIAN_POINT('Ctrl Pts',(-2.2639905433933,-18.4278937074565,-325.552961679349)) ;
#41151 = CARTESIAN_POINT('Ctrl Pts',(-2.12921855974028,-18.4439515270494,
-325.551204263126)) ;
#41152 = CARTESIAN_POINT('Ctrl Pts',(-1.76313488556778,-18.4835036666961,
-325.546410945793)) ;
#41153 = CARTESIAN_POINT('Ctrl Pts',(-1.53153869931223,-18.5041330874849,
-325.543357138461)) ;
#41154 = CARTESIAN_POINT('Ctrl Pts',(-1.05099695682863,-18.5378537298776,
-325.53698145632)) ;
#41155 = CARTESIAN_POINT('Ctrl Pts',(-0.802051533335079,-18.5502918724665,
-325.533656708231)) ;
#41156 = CARTESIAN_POINT('Ctrl Pts',(-0.0245848552779535,-18.5734566824771,
-325.523229903037)) ;
#41157 = CARTESIAN_POINT('Ctrl Pts',(0.504192435468138,-18.5666283059729,
-325.516069508624)) ;
#41158 = CARTESIAN_POINT('Ctrl Pts',(1.15626000415832,-18.5303281581978,-325.507337090578)) ;
#41159 = CARTESIAN_POINT('Ctrl Pts',(1.28049166112913,-18.5221580816199,-325.505678197775)) ;
#41160 = CARTESIAN_POINT('Ctrl Pts',(1.56274218715176,-18.5007426625752,-325.501926275503)) ;
#41161 = CARTESIAN_POINT('Ctrl Pts',(1.72069264647002,-18.4867211579014,-325.499838798793)) ;
#41162 = CARTESIAN_POINT('Ctrl Pts',(1.95529386563328,-18.4628625149745,-325.496765555104)) ;
#41163 = CARTESIAN_POINT('Ctrl Pts',(2.03209402876608,-18.4545674624936,-325.495763848179)) ;
#41164 = CARTESIAN_POINT('Ctrl Pts',(2.17494325627519,-18.4382360315584,-325.493910226276)) ;
#41165 = CARTESIAN_POINT('Ctrl Pts',(2.24100506531518,-18.430323448347,-325.493056967061)) ;
#41166 = CARTESIAN_POINT('Ctrl Pts',(2.41002848499342,-18.4091563806101,-325.490882827947)) ;
#41167 = CARTESIAN_POINT('Ctrl Pts',(2.51292415374054,-18.39539312406,-325.489567724326)) ;
#41168 = CARTESIAN_POINT('Ctrl Pts',(2.87171676616319,-18.3443346741717,-325.485003955096)) ;
#41169 = CARTESIAN_POINT('Ctrl Pts',(3.12694585899099,-18.3025567039776,-325.481796194505)) ;
#41170 = CARTESIAN_POINT('Ctrl Pts',(3.9556834938046,-18.1490605227644,-325.471408792808)) ;
#41171 = CARTESIAN_POINT('Ctrl Pts',(4.5248053677219,-18.0156034468714,-325.464310293688)) ;
#41172 = CARTESIAN_POINT('Ctrl Pts',(5.24040308298934,-17.8117439215308,-325.455111551622)) ;
#41173 = CARTESIAN_POINT('Ctrl Pts',(5.39354816743352,-17.7659698325353,-325.453127483824)) ;
#41174 = CARTESIAN_POINT('Ctrl Pts',(5.76482770245515,-17.6497534952484,-325.448271818349)) ;
#41175 = CARTESIAN_POINT('Ctrl Pts',(5.98228536587229,-17.5772380767641,-325.445389058572)) ;
#41176 = CARTESIAN_POINT('Ctrl Pts',(6.32573835948047,-17.4555950540187,-325.440763757312)) ;
#41177 = CARTESIAN_POINT('Ctrl Pts',(6.45263589382466,-17.4090853992907,-325.439038982128)) ;
#41178 = CARTESIAN_POINT('Ctrl Pts',(6.69730699405274,-17.3163674331531,-325.435681260763)) ;
#41179 = CARTESIAN_POINT('Ctrl Pts',(6.8151384586883,-17.2703326484286,-325.434049591425)) ;
#41180 = CARTESIAN_POINT('Ctrl Pts',(7.09787392482434,-17.1565284471316,-325.43009847591)) ;
#41181 = CARTESIAN_POINT('Ctrl Pts',(7.26229007903832,-17.0875810245551,-325.427771021031)) ;
#41182 = CARTESIAN_POINT('Ctrl Pts',(7.79112692535068,-16.8568033234498,-325.420189384574)) ;
#41183 = CARTESIAN_POINT('Ctrl Pts',(8.15133335726371,-16.6855997850491,-325.414874612666)) ;
#41184 = CARTESIAN_POINT('Ctrl Pts',(8.94611242424129,-16.2759641295029,-325.402870992047)) ;
#41185 = CARTESIAN_POINT('Ctrl Pts',(9.37721659556207,-16.0314610789527,-325.396164328099)) ;
#41186 = CARTESIAN_POINT('Ctrl Pts',(9.90043763331762,-15.7063799550682,-325.387932106646)) ;
#41187 = CARTESIAN_POINT('Ctrl Pts',(10.0022285476579,-15.6417537619149,-325.386326382459)) ;
#41188 = CARTESIAN_POINT('Ctrl Pts',(10.2335904195664,-15.491682084193,-325.382672717367)) ;
#41189 = CARTESIAN_POINT('Ctrl Pts',(10.3627341090871,-15.4055940681663,-325.380630349876)) ;
#41190 = CARTESIAN_POINT('Ctrl Pts',(10.5540326016346,-15.2745792782623,-325.377609275737)) ;
#41191 = CARTESIAN_POINT('Ctrl Pts',(10.6170130197322,-15.2308703245855,-325.376615370024)) ;
#41192 = CARTESIAN_POINT('Ctrl Pts',(10.7343171680542,-15.1483790927794,-325.374766917203)) ;
#41193 = CARTESIAN_POINT('Ctrl Pts',(10.7887058639316,-15.1096915909759,-325.373911133361)) ;
#41194 = CARTESIAN_POINT('Ctrl Pts',(10.9282796977612,-15.0092727764472,-325.37171701207)) ;
#41195 = CARTESIAN_POINT('Ctrl Pts',(11.0131509902948,-14.9471091433723,-325.370384679379)) ;
#41196 = CARTESIAN_POINT('Ctrl Pts',(11.5711639756845,-14.5310618062259,-325.361622324033)) ;
#41197 = CARTESIAN_POINT('Ctrl Pts',(12.0277115105238,-14.1554849378218,-325.354430083177)) ;
#41198 = CARTESIAN_POINT('Ctrl Pts',(12.7329177717943,-13.5165619355861,-325.342766824898)) ;
#41199 = CARTESIAN_POINT('Ctrl Pts',(12.9931457553622,-13.2666048576102,-325.338331924461)) ;
#41200 = CARTESIAN_POINT('Ctrl Pts',(13.4264472849148,-12.8254195063637,-325.330638021702)) ;
#41201 = CARTESIAN_POINT('Ctrl Pts',(13.603123235126,-12.6378760115532,-325.327406543785)) ;
#41202 = CARTESIAN_POINT('Ctrl Pts',(13.8696971979593,-12.3428359670296,-325.322366760395)) ;
#41203 = CARTESIAN_POINT('Ctrl Pts',(13.9623774654911,-12.23789669478,-325.320582564457)) ;
#41204 = CARTESIAN_POINT('Ctrl Pts',(14.1355076593842,-12.0373391601769,-325.317186642055)) ;
#41205 = CARTESIAN_POINT('Ctrl Pts',(14.2161965424819,-11.9419373076176,-325.31557709674)) ;
#41206 = CARTESIAN_POINT('Ctrl Pts',(14.4002451370054,-11.7198198311237,-325.311842437595)) ;
#41207 = CARTESIAN_POINT('Ctrl Pts',(14.5029060275426,-11.592538700461,-325.30971168009)) ;
#41208 = CARTESIAN_POINT('Ctrl Pts',(14.8825971223937,-11.1088506580209,-325.301650051956)) ;
#41209 = CARTESIAN_POINT('Ctrl Pts',(15.1482794231129,-10.7437371768272,-325.295632125791)) ;
#41210 = CARTESIAN_POINT('Ctrl Pts',(15.4242032212069,-10.3339378917946,-325.288995507223)) ;
#41211 = CARTESIAN_POINT('Ctrl Pts',(15.4478948784972,-10.298488295994,-325.288422384577)) ;
#41212 = CARTESIAN_POINT('Ctrl Pts',(15.6055720106843,-10.0607891601424,-325.284586363474)) ;
#41213 = CARTESIAN_POINT('Ctrl Pts',(15.7357042727936,-9.85601173424314,-325.281314707487)) ;
#41214 = CARTESIAN_POINT('Ctrl Pts',(16.0060827453585,-9.41153047904062,-325.274312698051)) ;
#41215 = CARTESIAN_POINT('Ctrl Pts',(16.1450402359084,-9.1711104506302,-325.270585120915)) ;
#41216 = CARTESIAN_POINT('Ctrl Pts',(16.3634041503653,-8.77294935741677,-325.264552869295)) ;
#41217 = CARTESIAN_POINT('Ctrl Pts',(16.4460449192951,-8.61703211764601,-325.262225213585)) ;
#41218 = CARTESIAN_POINT('Ctrl Pts',(16.5629966772832,-8.38856799226436,-325.258876582447)) ;
#41219 = CARTESIAN_POINT('Ctrl Pts',(16.5990797915779,-8.31693946047766,-325.257835477423)) ;
#41220 = CARTESIAN_POINT('Ctrl Pts',(16.6642160099039,-8.18552516378484,-325.255942946683)) ;
#41221 = CARTESIAN_POINT('Ctrl Pts',(16.6934142628742,-8.1258130469061,-325.255089749927)) ;
#41222 = CARTESIAN_POINT('Ctrl Pts',(16.7650845084634,-7.97722653036488,-325.252982469829)) ;
#41223 = CARTESIAN_POINT('Ctrl Pts',(16.8071710884756,-7.88816846525244,-325.251733214866)) ;
#41224 = CARTESIAN_POINT('Ctrl Pts',(16.9939949698223,-7.48455263080776,-325.2461251409)) ;
#41225 = CARTESIAN_POINT('Ctrl Pts',(17.1306243216637,-7.16631736648492,-325.241848381673)) ;
#41226 = CARTESIAN_POINT('Ctrl Pts',(17.4104721685707,-6.46068100472641,-325.232523921038)) ;
#41227 = CARTESIAN_POINT('Ctrl Pts',(17.5498269439641,-6.07194487904033,-325.227487689554)) ;
#41228 = CARTESIAN_POINT('Ctrl Pts',(17.7607345986231,-5.41547361531304,-325.219000026489)) ;
#41229 = CARTESIAN_POINT('Ctrl Pts',(17.8394638390499,-5.15020170113004,-325.215575541175)) ;
#41230 = CARTESIAN_POINT('Ctrl Pts',(17.9693273399642,-4.67385171626183,-325.209403998361)) ;
#41231 = CARTESIAN_POINT('Ctrl Pts',(18.0227423254854,-4.46344863832101,-325.206670579502)) ;
#41232 = CARTESIAN_POINT('Ctrl Pts',(18.1029198227921,-4.12267946500903,-325.20222310564)) ;
#41233 = CARTESIAN_POINT('Ctrl Pts',(18.1319916077016,-3.99287770389717,-325.200524347972)) ;
#41234 = CARTESIAN_POINT('Ctrl Pts',(18.1859137182883,-3.73937923467862,-325.197196350214)) ;
#41235 = CARTESIAN_POINT('Ctrl Pts',(18.2109030017392,-3.61571938034208,-325.195568130975)) ;
#41236 = CARTESIAN_POINT('Ctrl Pts',(18.2636618278296,-3.34020713448863,-325.191929396364)) ;
#41237 = CARTESIAN_POINT('Ctrl Pts',(18.2908017598256,-3.18824370926364,-325.189914919715)) ;
#41238 = CARTESIAN_POINT('Ctrl Pts',(18.4338319645526,-2.32533783791376,-325.178435351717)) ;
#41239 = CARTESIAN_POINT('Ctrl Pts',(18.5101644333385,-1.60846537411794,-325.168715140381)) ;
#41240 = CARTESIAN_POINT('Ctrl Pts',(18.544654593745,-0.888979977948195,-325.159020379883)) ;
#41241 = CARTESIAN_POINT('Ctrl Pts',(18.544654593743,-0.888979977990129,-324.862668413757)) ;
#41242 = CARTESIAN_POINT('Ctrl Pts',(18.5381258541361,-1.02517339509664,-324.864435224152)) ;
#41243 = CARTESIAN_POINT('Ctrl Pts',(18.5300969633876,-1.16129131229351,-324.866211571098)) ;
#41244 = CARTESIAN_POINT('Ctrl Pts',(18.4922244160714,-1.70196523688201,-324.873308733905)) ;
#41245 = CARTESIAN_POINT('Ctrl Pts',(18.4506251769581,-2.10558271819744,-324.8787015583)) ;
#41246 = CARTESIAN_POINT('Ctrl Pts',(18.3400775793385,-2.9165921489683,-324.889674525018)) ;
#41247 = CARTESIAN_POINT('Ctrl Pts',(18.2706864423052,-3.32369851936604,-324.895253226547)) ;
#41248 = CARTESIAN_POINT('Ctrl Pts',(18.1186365610978,-4.06547361825138,-324.905427810891)) ;
#41249 = CARTESIAN_POINT('Ctrl Pts',(18.0401208576654,-4.40080752377932,-324.91003043826)) ;
#41250 = CARTESIAN_POINT('Ctrl Pts',(17.9272125024931,-4.82900114681951,-324.915838807011)) ;
#41251 = CARTESIAN_POINT('Ctrl Pts',(17.901342354071,-4.92403717989873,-324.917123445081)) ;
#41252 = CARTESIAN_POINT('Ctrl Pts',(17.8567493604272,-5.08285545398464,-324.919260077664)) ;
#41253 = CARTESIAN_POINT('Ctrl Pts',(17.8384380204821,-5.14675104435503,-324.920116839305)) ;
#41254 = CARTESIAN_POINT('Ctrl Pts',(17.797273715886,-5.28753069564596,-324.921997661633)) ;
#41255 = CARTESIAN_POINT('Ctrl Pts',(17.7742648936657,-5.36436763180048,-324.923019910421)) ;
#41256 = CARTESIAN_POINT('Ctrl Pts',(17.6990379175872,-5.60978628222489,-324.926274481705)) ;
#41257 = CARTESIAN_POINT('Ctrl Pts',(17.6449136201815,-5.77777369483103,-324.928486348787)) ;
#41258 = CARTESIAN_POINT('Ctrl Pts',(17.499473894113,-6.20806266031709,-324.934137004373)) ;
#41259 = CARTESIAN_POINT('Ctrl Pts',(17.4046529861399,-6.46913312500787,-324.937551384741)) ;
#41260 = CARTESIAN_POINT('Ctrl Pts',(17.2181084296283,-6.94891605348687,-324.943863349554)) ;
#41261 = CARTESIAN_POINT('Ctrl Pts',(17.1279820158107,-7.16818835494682,-324.946762713302)) ;
#41262 = CARTESIAN_POINT('Ctrl Pts',(17.0084701558398,-7.44382018113507,-324.950447884027)) ;
#41263 = CARTESIAN_POINT('Ctrl Pts',(16.9829611138028,-7.50183629094492,-324.951225840286)) ;
#41264 = CARTESIAN_POINT('Ctrl Pts',(16.7836550600635,-7.94889828041912,-324.957240520559)) ;
#41265 = CARTESIAN_POINT('Ctrl Pts',(16.5968085535664,-8.33198690246369,-324.962514623405)) ;
#41266 = CARTESIAN_POINT('Ctrl Pts',(16.3253925464621,-8.84303853742481,-324.969800174043)) ;
#41267 = CARTESIAN_POINT('Ctrl Pts',(16.2521793193965,-8.97688362698648,-324.971731869571)) ;
#41268 = CARTESIAN_POINT('Ctrl Pts',(16.1156130648748,-9.2193998176518,-324.975278018854)) ;
#41269 = CARTESIAN_POINT('Ctrl Pts',(16.0527892801765,-9.32835857630667,-324.976888520089)) ;
#41270 = CARTESIAN_POINT('Ctrl Pts',(15.9208979907835,-9.55182635565259,-324.980228375585)) ;
#41271 = CARTESIAN_POINT('Ctrl Pts',(15.851690659593,-9.66624449981995,-324.981958715949)) ;
#41272 = CARTESIAN_POINT('Ctrl Pts',(15.6648100359974,-9.96780269544494,-324.986573771121)) ;
#41273 = CARTESIAN_POINT('Ctrl Pts',(15.5450203621148,-10.1536055521247,-324.989474091266)) ;
#41274 = CARTESIAN_POINT('Ctrl Pts',(15.337645955908,-10.4629841408862,-324.994397037497)) ;
#41275 = CARTESIAN_POINT('Ctrl Pts',(15.2518152073156,-10.5877076560748,-324.996408000453)) ;
#41276 = CARTESIAN_POINT('Ctrl Pts',(14.8630810511037,-11.1380526088268,-325.00539307083)) ;
#41277 = CARTESIAN_POINT('Ctrl Pts',(14.543819364428,-11.5518271631589,-325.012456914511)) ;
#41278 = CARTESIAN_POINT('Ctrl Pts',(13.9807375303385,-12.221194882475,-325.024214133831)) ;
#41279 = CARTESIAN_POINT('Ctrl Pts',(13.7463096200732,-12.4842940911381,-325.028926108407)) ;
#41280 = CARTESIAN_POINT('Ctrl Pts',(13.4361921249088,-12.8130074460888,-325.034855195076)) ;
#41281 = CARTESIAN_POINT('Ctrl Pts',(13.367264649142,-12.8849002508042,-325.036154522666)) ;
#41282 = CARTESIAN_POINT('Ctrl Pts',(13.2512826114673,-13.0039395803706,-325.038307588683)) ;
#41283 = CARTESIAN_POINT('Ctrl Pts',(13.2045468541549,-13.0513937137986,-325.03916627127)) ;
#41284 = CARTESIAN_POINT('Ctrl Pts',(13.1013934351152,-13.1550114603232,-325.04104144792)) ;
#41285 = CARTESIAN_POINT('Ctrl Pts',(13.0448679648698,-13.2110656748541,-325.042056236811)) ;
#41286 = CARTESIAN_POINT('Ctrl Pts',(12.8645682258735,-13.3875768209156,-325.045256092971)) ;
#41287 = CARTESIAN_POINT('Ctrl Pts',(12.7394726213125,-13.5066711770952,-325.047421642113)) ;
#41288 = CARTESIAN_POINT('Ctrl Pts',(12.4158267578886,-13.8062937648796,-325.052911163064)) ;
#41289 = CARTESIAN_POINT('Ctrl Pts',(12.2149909927262,-13.9842946556543,-325.056212358608)) ;
#41290 = CARTESIAN_POINT('Ctrl Pts',(11.4385647355043,-14.6429501066623,-325.068701015128)) ;
#41291 = CARTESIAN_POINT('Ctrl Pts',(10.8378996366233,-15.0929348587716,-325.077838873132)) ;
#41292 = CARTESIAN_POINT('Ctrl Pts',(10.0745518696503,-15.5956680629472,-325.089354048055)) ;
#41293 = CARTESIAN_POINT('Ctrl Pts',(9.93623689516225,-15.6841529562926,-325.091435334465)) ;
#41294 = CARTESIAN_POINT('Ctrl Pts',(9.69056454589318,-15.8367638556577,-325.095126126287)) ;
#41295 = CARTESIAN_POINT('Ctrl Pts',(9.58369889118122,-15.9016617417581,-325.096729632167)) ;
#41296 = CARTESIAN_POINT('Ctrl Pts',(9.35609379009608,-16.0367550127542,-325.100141568057)) ;
#41297 = CARTESIAN_POINT('Ctrl Pts',(9.23520129563525,-16.1066774756576,-325.101951922738)) ;
#41298 = CARTESIAN_POINT('Ctrl Pts',(8.89090976266209,-16.3006599966445,-325.107102603623)) ;
#41299 = CARTESIAN_POINT('Ctrl Pts',(8.66572263367698,-16.4214811621469,-325.110465842043)) ;
#41300 = CARTESIAN_POINT('Ctrl Pts',(8.26984674924257,-16.6234719390595,-325.116362134229)) ;
#41301 = CARTESIAN_POINT('Ctrl Pts',(8.10027912422241,-16.7067549975803,-325.118882558934)) ;
#41302 = CARTESIAN_POINT('Ctrl Pts',(7.60594996510282,-16.9402491682121,-325.126205223727)) ;
#41303 = CARTESIAN_POINT('Ctrl Pts',(7.27807995788663,-17.0836784241801,-325.131032586518)) ;
#41304 = CARTESIAN_POINT('Ctrl Pts',(6.90056669914075,-17.2359829292881,-325.136512491861)) ;
#41305 = CARTESIAN_POINT('Ctrl Pts',(6.85478891652288,-17.2542399780111,-325.137175669494)) ;
#41306 = CARTESIAN_POINT('Ctrl Pts',(6.49016627604845,-17.397978288492,-325.142446342933)) ;
#41307 = CARTESIAN_POINT('Ctrl Pts',(6.16797525620258,-17.5147934272467,-325.147034723616)) ;
#41308 = CARTESIAN_POINT('Ctrl Pts',(5.734919285191,-17.6583720232006,-325.153038767898)) ;
#41309 = CARTESIAN_POINT('Ctrl Pts',(5.6267763662319,-17.6931283130446,-325.154524629484)) ;
#41310 = CARTESIAN_POINT('Ctrl Pts',(5.45904281214665,-17.7453432039354,-325.156804844848)) ;
#41311 = CARTESIAN_POINT('Ctrl Pts',(5.39967217022753,-17.7634989323192,-325.157607240794)) ;
#41312 = CARTESIAN_POINT('Ctrl Pts',(5.27183163679566,-17.8018928247677,-325.159324037637)) ;
#41313 = CARTESIAN_POINT('Ctrl Pts',(5.20333379095375,-17.8220345199068,-325.160237184869)) ;
#41314 = CARTESIAN_POINT('Ctrl Pts',(5.01272906233195,-17.8768890326417,-325.162761517157)) ;
#41315 = CARTESIAN_POINT('Ctrl Pts',(4.89037967544262,-17.9107454017938,-325.16436301573)) ;
#41316 = CARTESIAN_POINT('Ctrl Pts',(4.60350095171625,-17.986971412684,-325.168083219911)) ;
#41317 = CARTESIAN_POINT('Ctrl Pts',(4.43871803237274,-18.0283427960947,-325.170193471739)) ;
#41318 = CARTESIAN_POINT('Ctrl Pts',(3.78020831113551,-18.1840963547799,-325.178554893562)) ;
#41319 = CARTESIAN_POINT('Ctrl Pts',(3.28245640292659,-18.2805037230435,-325.184721444914)) ;
#41320 = CARTESIAN_POINT('Ctrl Pts',(2.41451156324132,-18.4120156269892,-325.195516034648)) ;
#41321 = CARTESIAN_POINT('Ctrl Pts',(2.04605487618976,-18.4565935155754,-325.200109836829)) ;
#41322 = CARTESIAN_POINT('Ctrl Pts',(1.49315527545507,-18.5067253303527,-325.207081930661)) ;
#41323 = CARTESIAN_POINT('Ctrl Pts',(1.30956260823679,-18.5206220401048,-325.209409581076)) ;
#41324 = CARTESIAN_POINT('Ctrl Pts',(0.999897604728933,-18.5394339867642,
-325.21336141677)) ;
#41325 = CARTESIAN_POINT('Ctrl Pts',(0.873926774540049,-18.545798977377,-325.214976158995)) ;
#41326 = CARTESIAN_POINT('Ctrl Pts',(0.614946778249287,-18.5562400667901,
-325.21831153593)) ;
#41327 = CARTESIAN_POINT('Ctrl Pts',(0.481938917505182,-18.5601707905231,
-325.220033018631)) ;
#41328 = CARTESIAN_POINT('Ctrl Pts',(0.131602864138187,-18.5667556402194,
-325.224590087067)) ;
#41329 = CARTESIAN_POINT('Ctrl Pts',(-0.0857493167577347,-18.5670240241271,
-325.227440556212)) ;
#41330 = CARTESIAN_POINT('Ctrl Pts',(-0.580212184113941,-18.5589517324173,
-325.233974174773)) ;
#41331 = CARTESIAN_POINT('Ctrl Pts',(-0.857232122236112,-18.548220622205,
-325.237669859553)) ;
#41332 = CARTESIAN_POINT('Ctrl Pts',(-1.54599096097788,-18.5060763017575,
-325.246920353621)) ;
#41333 = CARTESIAN_POINT('Ctrl Pts',(-1.95711882222,-18.4671230458694,-325.25249888158)) ;
#41334 = CARTESIAN_POINT('Ctrl Pts',(-2.70907867008816,-18.370482242093,-325.262686461108)) ;
#41335 = CARTESIAN_POINT('Ctrl Pts',(-3.05025879526739,-18.3169224265755,
-325.267302063434)) ;
#41336 = CARTESIAN_POINT('Ctrl Pts',(-3.48655755233183,-18.235901715154,-325.273122568471)) ;
#41337 = CARTESIAN_POINT('Ctrl Pts',(-3.58322389406087,-18.2171540449279,
-325.274406851151)) ;
#41338 = CARTESIAN_POINT('Ctrl Pts',(-3.74488205907087,-18.1844652169232,
-325.27654308744)) ;
#41339 = CARTESIAN_POINT('Ctrl Pts',(-3.8099563325229,-18.1709424533239,-325.277399803896)) ;
#41340 = CARTESIAN_POINT('Ctrl Pts',(-3.95341210292426,-18.1403271116726,
-325.279280769134)) ;
#41341 = CARTESIAN_POINT('Ctrl Pts',(-4.03175811277579,-18.1230753879647,
-325.280303203378)) ;
#41342 = CARTESIAN_POINT('Ctrl Pts',(-4.28218568938222,-18.0662271788778,
-325.283559146377)) ;
#41343 = CARTESIAN_POINT('Ctrl Pts',(-4.45381534758566,-18.0246832926122,
-325.285772175941)) ;
#41344 = CARTESIAN_POINT('Ctrl Pts',(-4.89402441204554,-17.9114568438308,
-325.291426913013)) ;
#41345 = CARTESIAN_POINT('Ctrl Pts',(-5.16163387062843,-17.8361794505509,
-325.294844170377)) ;
#41346 = CARTESIAN_POINT('Ctrl Pts',(-5.65180806111612,-17.6863394776365,
-325.301129018385)) ;
#41347 = CARTESIAN_POINT('Ctrl Pts',(-5.87484368838931,-17.6135104430597,
-325.303998537316)) ;
#41348 = CARTESIAN_POINT('Ctrl Pts',(-6.18086110857364,-17.507125514711,-325.307972468968)) ;
#41349 = CARTESIAN_POINT('Ctrl Pts',(-6.26507008961982,-17.4771675221502,
-325.309069857811)) ;
#41350 = CARTESIAN_POINT('Ctrl Pts',(-6.68374446566345,-17.3248061396228,
-325.314549079391)) ;
#41351 = CARTESIAN_POINT('Ctrl Pts',(-7.01485493331593,-17.1934044746438,
-325.31895796167)) ;
#41352 = CARTESIAN_POINT('Ctrl Pts',(-7.51600863644812,-16.9776327487746,
-325.325804512307)) ;
#41353 = CARTESIAN_POINT('Ctrl Pts',(-7.68887982183782,-16.9000451625378,
-325.328198292907)) ;
#41354 = CARTESIAN_POINT('Ctrl Pts',(-7.97556951367066,-16.7660643561651,
-325.332227300152)) ;
#41355 = CARTESIAN_POINT('Ctrl Pts',(-8.09005146554495,-16.7111247465066,
-325.333852164385)) ;
#41356 = CARTESIAN_POINT('Ctrl Pts',(-8.32213421134901,-16.5968049626977,
-325.337179926963)) ;
#41357 = CARTESIAN_POINT('Ctrl Pts',(-8.4396847228047,-16.5373387980106,-325.338883377208)) ;
#41358 = CARTESIAN_POINT('Ctrl Pts',(-8.74276016887112,-16.3799465676584,
-325.3433224931)) ;
#41359 = CARTESIAN_POINT('Ctrl Pts',(-8.92727581063615,-16.2801182826145,
-325.346071612035)) ;
#41360 = CARTESIAN_POINT('Ctrl Pts',(-9.23215653176139,-16.1084270001712,
-325.35069006627)) ;
#41361 = CARTESIAN_POINT('Ctrl Pts',(-9.35347079505296,-16.0382891442111,
-325.352548253763)) ;
#41362 = CARTESIAN_POINT('Ctrl Pts',(-9.8632502919117,-15.7358086830335,-325.360439330944)) ;
#41363 = CARTESIAN_POINT('Ctrl Pts',(-10.2439437333666,-15.4906745086136,
-325.366541656486)) ;
#41364 = CARTESIAN_POINT('Ctrl Pts',(-10.7846995607814,-15.113814549437,-325.375418303177)) ;
#41365 = CARTESIAN_POINT('Ctrl Pts',(-10.9521215306519,-14.9929373009771,
-325.378196399511)) ;
#41366 = CARTESIAN_POINT('Ctrl Pts',(-11.2393775048666,-14.7781613737659,
-325.382997414465)) ;
#41367 = CARTESIAN_POINT('Ctrl Pts',(-11.3601376206761,-14.6855348424388,
-325.38502658867)) ;
#41368 = CARTESIAN_POINT('Ctrl Pts',(-11.6005257561328,-14.4964105542178,
-325.389078154469)) ;
#41369 = CARTESIAN_POINT('Ctrl Pts',(-11.7201218887997,-14.3998909655259,
-325.391100128609)) ;
#41370 = CARTESIAN_POINT('Ctrl Pts',(-11.8973539200183,-14.253185784914,-325.394097570721)) ;
#41371 = CARTESIAN_POINT('Ctrl Pts',(-11.9559006636398,-14.2041111886541,
-325.39508790761)) ;
#41372 = CARTESIAN_POINT('Ctrl Pts',(-12.0657119565852,-14.1109060521385,
-325.396944301609)) ;
#41373 = CARTESIAN_POINT('Ctrl Pts',(-12.1170413620737,-14.0668540637558,
-325.397811436519)) ;
#41374 = CARTESIAN_POINT('Ctrl Pts',(-12.2486894644291,-13.952615625416,-325.400035199504)) ;
#41375 = CARTESIAN_POINT('Ctrl Pts',(-12.328646205604,-13.8820156740331,-325.401385665571)) ;
#41376 = CARTESIAN_POINT('Ctrl Pts',(-12.4604768780668,-13.7635748947493,
-325.40361593333)) ;
#41377 = CARTESIAN_POINT('Ctrl Pts',(-12.5126943527993,-13.7161203682864,
-325.404500298253)) ;
#41378 = CARTESIAN_POINT('Ctrl Pts',(-12.7189120803986,-13.5265548491555,
-325.407999261578)) ;
#41379 = CARTESIAN_POINT('Ctrl Pts',(-12.8707723011009,-13.3821385130273,
-325.410590421761)) ;
#41380 = CARTESIAN_POINT('Ctrl Pts',(-13.6203377077586,-12.6447510124986,
-325.42353187591)) ;
#41381 = CARTESIAN_POINT('Ctrl Pts',(-14.1796623771319,-12.0141793892542,
-325.43373397788)) ;
#41382 = CARTESIAN_POINT('Ctrl Pts',(-14.7870252244975,-11.2277076553842,
-325.446247094295)) ;
#41383 = CARTESIAN_POINT('Ctrl Pts',(-14.8783144395675,-11.1064527881372,
-325.448169146537)) ;
#41384 = CARTESIAN_POINT('Ctrl Pts',(-15.0424183123088,-10.8828271875925,
-325.451703619779)) ;
#41385 = CARTESIAN_POINT('Ctrl Pts',(-15.1157004314686,-10.7808105767237,
-325.45331218965)) ;
#41386 = CARTESIAN_POINT('Ctrl Pts',(-15.2650328854429,-10.5684074850552,
-325.456654401007)) ;
#41387 = CARTESIAN_POINT('Ctrl Pts',(-15.3409343614486,-10.4579251583357,
-325.458389094974)) ;
#41388 = CARTESIAN_POINT('Ctrl Pts',(-15.539843769457,-10.1615664245743,-325.463032692592)) ;
#41389 = CARTESIAN_POINT('Ctrl Pts',(-15.6607120034706,-9.9742807182039,-325.465957561625)) ;
#41390 = CARTESIAN_POINT('Ctrl Pts',(-15.8589564007482,-9.65460991424466,
-325.470930512323)) ;
#41391 = CARTESIAN_POINT('Ctrl Pts',(-15.938117947845,-9.52336006474313,-325.472966855059)) ;
#41392 = CARTESIAN_POINT('Ctrl Pts',(-16.2863959273451,-8.92940731252562,
-325.482150944488)) ;
#41393 = CARTESIAN_POINT('Ctrl Pts',(-16.5370516564231,-8.4561769104291,-325.489392466822)) ;
#41394 = CARTESIAN_POINT('Ctrl Pts',(-16.9113094864143,-7.66910562441568,
-325.501100341607)) ;
#41395 = CARTESIAN_POINT('Ctrl Pts',(-17.0474329218596,-7.36156241601446,
-325.505593215)) ;
#41396 = CARTESIAN_POINT('Ctrl Pts',(-17.2125897247166,-6.9592373934995,-325.511297848511)) ;
#41397 = CARTESIAN_POINT('Ctrl Pts',(-17.2493225080383,-6.8676854314611,-325.512584509882)) ;
#41398 = CARTESIAN_POINT('Ctrl Pts',(-17.3095885474437,-6.71394548982351,
-325.514723399839)) ;
#41399 = CARTESIAN_POINT('Ctrl Pts',(-17.3335204846647,-6.65191606726594,
-325.51558041992)) ;
#41400 = CARTESIAN_POINT('Ctrl Pts',(-17.3855572453533,-6.51485366349033,
-325.517460434453)) ;
#41401 = CARTESIAN_POINT('Ctrl Pts',(-17.4135105333851,-6.43976474069617,
-325.518481631983)) ;
#41402 = CARTESIAN_POINT('Ctrl Pts',(-17.5012921923567,-6.19921189782354,
-325.521728438355)) ;
#41403 = CARTESIAN_POINT('Ctrl Pts',(-17.5592549674642,-6.03307730220059,
-325.523933726129)) ;
#41404 = CARTESIAN_POINT('Ctrl Pts',(-17.7021711792304,-5.60392871880256,
-325.529561316627)) ;
#41405 = CARTESIAN_POINT('Ctrl Pts',(-17.7836289662406,-5.33979613123601,
-325.532959447996)) ;
#41406 = CARTESIAN_POINT('Ctrl Pts',(-18.0567477392945,-4.37847840775305,
-325.545213854333)) ;
#41407 = CARTESIAN_POINT('Ctrl Pts',(-18.2135431528933,-3.67206450362121,
-325.554030734353)) ;
#41408 = CARTESIAN_POINT('Ctrl Pts',(-18.3533975978218,-2.80557189399373,
-325.565076709102)) ;
#41409 = CARTESIAN_POINT('Ctrl Pts',(-18.3761401969136,-2.6525286818328,-325.567035056102)) ;
#41410 = CARTESIAN_POINT('Ctrl Pts',(-18.4139599137766,-2.37413450448275,
-325.570613628627)) ;
#41411 = CARTESIAN_POINT('Ctrl Pts',(-18.4296764458473,-2.24887980999691,
-325.572229619995)) ;
#41412 = CARTESIAN_POINT('Ctrl Pts',(-18.4593126680716,-1.991464982837,-325.575563840464)) ;
#41413 = CARTESIAN_POINT('Ctrl Pts',(-18.4730932747754,-1.85929603731072,
-325.577282878659)) ;
#41414 = CARTESIAN_POINT('Ctrl Pts',(-18.5055748957073,-1.51161755220164,
-325.581823957283)) ;
#41415 = CARTESIAN_POINT('Ctrl Pts',(-18.5219304598692,-1.29590957569516,
-325.584660684272)) ;
#41416 = CARTESIAN_POINT('Ctrl Pts',(-18.5505246958422,-0.80517143329906,
-325.591154405314)) ;
#41417 = CARTESIAN_POINT('Ctrl Pts',(-18.560423163618,-0.530055751092466,
-325.594823690902)) ;
#41418 = CARTESIAN_POINT('Ctrl Pts',(-18.5698672744087,0.157962337761502,
-325.604046528953)) ;
#41419 = CARTESIAN_POINT('Ctrl Pts',(-18.5617640737465,0.570821060204457,
-325.609624394886)) ;
#41420 = CARTESIAN_POINT('Ctrl Pts',(-18.5214388544416,1.33132601610996,-325.619859256568)) ;
#41421 = CARTESIAN_POINT('Ctrl Pts',(-18.493163371486,1.67899838666721,-325.62452207147)) ;
#41422 = CARTESIAN_POINT('Ctrl Pts',(-18.4443478998066,2.12373811586512,-325.630390765951)) ;
#41423 = CARTESIAN_POINT('Ctrl Pts',(-18.4328019756894,2.22172104464914,-325.631677623332)) ;
#41424 = CARTESIAN_POINT('Ctrl Pts',(-18.4121687533959,2.38557367432853,-325.63381673208)) ;
#41425 = CARTESIAN_POINT('Ctrl Pts',(-18.4035076200842,2.45149490573154,-325.634673777305)) ;
#41426 = CARTESIAN_POINT('Ctrl Pts',(-18.3836298094674,2.5967427108578,-325.636553714106)) ;
#41427 = CARTESIAN_POINT('Ctrl Pts',(-18.3722534244905,2.67604592783782,-325.637574810206)) ;
#41428 = CARTESIAN_POINT('Ctrl Pts',(-18.3342604818384,2.92922020051268,-325.640820868344)) ;
#41429 = CARTESIAN_POINT('Ctrl Pts',(-18.3056861670504,3.10278786620846,-325.643025522238)) ;
#41430 = CARTESIAN_POINT('Ctrl Pts',(-18.2259071860437,3.54783274017972,-325.648650893665)) ;
#41431 = CARTESIAN_POINT('Ctrl Pts',(-18.1711019587516,3.81862068013037,-325.652047462569)) ;
#41432 = CARTESIAN_POINT('Ctrl Pts',(-17.9516045826797,4.79099721518068,-325.664271022509)) ;
#41433 = CARTESIAN_POINT('Ctrl Pts',(-17.7521453722084,5.48407657751811,-325.67305864834)) ;
#41434 = CARTESIAN_POINT('Ctrl Pts',(-17.461219862357,6.31066888090055,-325.684084726484)) ;
#41435 = CARTESIAN_POINT('Ctrl Pts',(-17.4076840449076,6.45687826317527,-325.686055130276)) ;
#41436 = CARTESIAN_POINT('Ctrl Pts',(-17.3073481493258,6.72057948834217,-325.689648438801)) ;
#41437 = CARTESIAN_POINT('Ctrl Pts',(-17.2611745620122,6.83829959181913,-325.691266981231)) ;
#41438 = CARTESIAN_POINT('Ctrl Pts',(-17.1641515887554,7.07841532204329,-325.694599045026)) ;
#41439 = CARTESIAN_POINT('Ctrl Pts',(-17.1131869204801,7.20075666827623,-325.696313298285)) ;
#41440 = CARTESIAN_POINT('Ctrl Pts',(-16.9763933074534,7.51947447615887,-325.700823085113)) ;
#41441 = CARTESIAN_POINT('Ctrl Pts',(-16.888466523612,7.71492866839115,-325.703632922743)) ;
#41442 = CARTESIAN_POINT('Ctrl Pts',(-16.6815209950024,8.1544508698707,-325.710048888708)) ;
#41443 = CARTESIAN_POINT('Ctrl Pts',(-16.5604920599986,8.39751832532395,-325.71366684079)) ;
#41444 = CARTESIAN_POINT('Ctrl Pts',(-16.269939377822,8.95031764018592,-325.722035117324)) ;
#41445 = CARTESIAN_POINT('Ctrl Pts',(-16.0968238486783,9.25804379237521,-325.726798254232)) ;
#41446 = CARTESIAN_POINT('Ctrl Pts',(-15.7595083869069,9.81955282186625,-325.735615246477)) ;
#41447 = CARTESIAN_POINT('Ctrl Pts',(-15.5976807776198,10.074625401159,-325.739670530999)) ;
#41448 = CARTESIAN_POINT('Ctrl Pts',(-15.3382866896946,10.4622406009242,-325.745857163054)) ;
#41449 = CARTESIAN_POINT('Ctrl Pts',(-15.2450603609048,10.5976248148503,-325.748022524744)) ;
#41450 = CARTESIAN_POINT('Ctrl Pts',(-15.1048265182354,10.7955933523002,-325.751185508893)) ;
#41451 = CARTESIAN_POINT('Ctrl Pts',(-15.0592014357155,10.8591469331221,-325.752200384815)) ;
#41452 = CARTESIAN_POINT('Ctrl Pts',(-14.9737728473272,10.9765710545287,-325.754073031483)) ;
#41453 = CARTESIAN_POINT('Ctrl Pts',(-14.9340769898321,11.0305181134235,-325.754932221792)) ;
#41454 = CARTESIAN_POINT('Ctrl Pts',(-14.8329871159042,11.1663542586281,-325.757093821876)) ;
#41455 = CARTESIAN_POINT('Ctrl Pts',(-14.7712062298641,11.2479527368217,-325.758390778703)) ;
#41456 = CARTESIAN_POINT('Ctrl Pts',(-14.6317768379482,11.4289771895086,-325.761269214318)) ;
#41457 = CARTESIAN_POINT('Ctrl Pts',(-14.5537832529012,11.5281310768763,-325.762846647535)) ;
#41458 = CARTESIAN_POINT('Ctrl Pts',(-14.2986261011356,11.8457976594216,-325.76791479526)) ;
#41459 = CARTESIAN_POINT('Ctrl Pts',(-14.117505119151,12.0610812194131,-325.771372333612)) ;
#41460 = CARTESIAN_POINT('Ctrl Pts',(-13.4589551961165,12.8086777878847,-325.783587056471)) ;
#41461 = CARTESIAN_POINT('Ctrl Pts',(-12.9557499349095,13.3174413803227,-325.792309977594)) ;
#41462 = CARTESIAN_POINT('Ctrl Pts',(-12.3094244624844,13.899515673893,-325.803256205789)) ;
#41463 = CARTESIAN_POINT('Ctrl Pts',(-12.1930951745481,14.0016747762227,-325.805215728218)) ;
#41464 = CARTESIAN_POINT('Ctrl Pts',(-11.9796012462123,14.1844842552587,-325.808795735595)) ;
#41465 = CARTESIAN_POINT('Ctrl Pts',(-11.8828654969847,14.2656211618479,-325.810411973914)) ;
#41466 = CARTESIAN_POINT('Ctrl Pts',(-11.6826602031754,14.4300934928543,-325.813745973816)) ;
#41467 = CARTESIAN_POINT('Ctrl Pts',(-11.5791085836803,14.5133177454427,-325.815464536894)) ;
#41468 = CARTESIAN_POINT('Ctrl Pts',(-11.3047788072906,14.7289911341839,-325.8200025081)) ;
#41469 = CARTESIAN_POINT('Ctrl Pts',(-11.1325659111102,14.8595820833543,-325.822836564644)) ;
#41470 = CARTESIAN_POINT('Ctrl Pts',(-10.7362149370299,15.1493811813869,-325.829322545224)) ;
#41471 = CARTESIAN_POINT('Ctrl Pts',(-10.5107415592983,15.3066773929509,-325.832986713787)) ;
#41472 = CARTESIAN_POINT('Ctrl Pts',(-9.93812633263931,15.687528927325,-325.84220420679)) ;
#41473 = CARTESIAN_POINT('Ctrl Pts',(-9.58686388451546,15.9046206879937,-325.847781960742)) ;
#41474 = CARTESIAN_POINT('Ctrl Pts',(-8.92549894526548,16.2834896103077,-325.858025443599)) ;
#41475 = CARTESIAN_POINT('Ctrl Pts',(-8.61749731967721,16.4485654731905,-325.862696858116)) ;
#41476 = CARTESIAN_POINT('Ctrl Pts',(-8.21673224209315,16.649010649223,-325.868574635706)) ;
#41477 = CARTESIAN_POINT('Ctrl Pts',(-8.12809221670241,16.6924642067723,-325.869862255838)) ;
#41478 = CARTESIAN_POINT('Ctrl Pts',(-7.97917238073115,16.7640009843189,-325.872002216173)) ;
#41479 = CARTESIAN_POINT('Ctrl Pts',(-7.91908071659601,16.7924709773137,-325.872859359421)) ;
#41480 = CARTESIAN_POINT('Ctrl Pts',(-7.78628312513224,16.8545159433535,-325.874738994611)) ;
#41481 = CARTESIAN_POINT('Ctrl Pts',(-7.71351042958043,16.8879445009117,-325.875759696696)) ;
#41482 = CARTESIAN_POINT('Ctrl Pts',(-7.48039670501084,16.9932054979515,-325.87900284983)) ;
#41483 = CARTESIAN_POINT('Ctrl Pts',(-7.31925117855927,17.0632332907562,-325.881205042867)) ;
#41484 = CARTESIAN_POINT('Ctrl Pts',(-6.90270747874475,17.2372608558067,-325.886821804599)) ;
#41485 = CARTESIAN_POINT('Ctrl Pts',(-6.64594224773445,17.3378771588116,-325.89021231274)) ;
#41486 = CARTESIAN_POINT('Ctrl Pts',(-5.70570197653486,17.6823637375105,-325.902491483921)) ;
#41487 = CARTESIAN_POINT('Ctrl Pts',(-5.01032331176097,17.8918328446128,-325.911339965105)) ;
#41488 = CARTESIAN_POINT('Ctrl Pts',(-4.15456818780093,18.0957954099149,-325.922412700275)) ;
#41489 = CARTESIAN_POINT('Ctrl Pts',(-4.00422148437912,18.1296568792157,-325.924363519327)) ;
#41490 = CARTESIAN_POINT('Ctrl Pts',(-3.7301157846588,18.1878156227027,-325.927932911874)) ;
#41491 = CARTESIAN_POINT('Ctrl Pts',(-3.60649741989119,18.2127311845243,-325.929547330984)) ;
#41492 = CARTESIAN_POINT('Ctrl Pts',(-3.35188800928146,18.2613543962448,-325.932883018432)) ;
#41493 = CARTESIAN_POINT('Ctrl Pts',(-3.22087646518749,18.2849165255167,-325.934605144949)) ;
#41494 = CARTESIAN_POINT('Ctrl Pts',(-2.87505134035548,18.3432802830131,-325.939166425339)) ;
#41495 = CARTESIAN_POINT('Ctrl Pts',(-2.65985995226683,18.3757175784956,-325.942020514635)) ;
#41496 = CARTESIAN_POINT('Ctrl Pts',(-1.60793750064242,18.515415673222,-325.956040791013)) ;
#41497 = CARTESIAN_POINT('Ctrl Pts',(-0.765136275296041,18.5693466268616,
-325.967534556341)) ;
#41498 = CARTESIAN_POINT('Ctrl Pts',(0.295082724962301,18.5648694388514,-325.981678250055)) ;
#41499 = CARTESIAN_POINT('Ctrl Pts',(0.511731969816002,18.5601611468255,-325.984548649932)) ;
#41500 = CARTESIAN_POINT('Ctrl Pts',(0.814739961412343,18.5482665054331,-325.988514389729)) ;
#41501 = CARTESIAN_POINT('Ctrl Pts',(0.90120589264641,18.5442664866913,-325.989640448845)) ;
#41502 = CARTESIAN_POINT('Ctrl Pts',(1.05329278231821,18.5361645476409,-325.991609363401)) ;
#41503 = CARTESIAN_POINT('Ctrl Pts',(1.11892560309099,18.5323184553841,-325.992455060869)) ;
#41504 = CARTESIAN_POINT('Ctrl Pts',(1.27232474320629,18.5225113674957,-325.994422431458)) ;
#41505 = CARTESIAN_POINT('Ctrl Pts',(1.36007170207535,18.5162750737467,-325.995540980881)) ;
#41506 = CARTESIAN_POINT('Ctrl Pts',(1.68044435934408,18.4912161368036,-325.999604860392)) ;
#41507 = CARTESIAN_POINT('Ctrl Pts',(1.91275426063009,18.4686312162562,-326.002513243689)) ;
#41508 = CARTESIAN_POINT('Ctrl Pts',(2.59861765013032,18.3888723596994,-326.011053437748)) ;
#41509 = CARTESIAN_POINT('Ctrl Pts',(3.05055412035333,18.3193220662031,-326.016623781821)) ;
#41510 = CARTESIAN_POINT('Ctrl Pts',(3.96392214500717,18.1440207739935,-326.028037463384)) ;
#41511 = CARTESIAN_POINT('Ctrl Pts',(4.42480514575666,18.0371634867906,-326.033880074358)) ;
#41512 = CARTESIAN_POINT('Ctrl Pts',(5.02725505875044,17.8730006537474,-326.041743520987)) ;
#41513 = CARTESIAN_POINT('Ctrl Pts',(5.17291381020615,17.8313882920061,-326.043661981945)) ;
#41514 = CARTESIAN_POINT('Ctrl Pts',(5.43833184222175,17.7520367247879,-326.047192114981)) ;
#41515 = CARTESIAN_POINT('Ctrl Pts',(5.55824886622087,17.7148562114734,-326.048799973626)) ;
#41516 = CARTESIAN_POINT('Ctrl Pts',(5.80551322754323,17.635433503348,-326.052143108107)) ;
#41517 = CARTESIAN_POINT('Ctrl Pts',(5.93279840900113,17.5930213908802,-326.053879461481)) ;
#41518 = CARTESIAN_POINT('Ctrl Pts',(6.27095080348051,17.4762600228415,-326.058533947658)) ;
#41519 = CARTESIAN_POINT('Ctrl Pts',(6.48095324191959,17.3994750828928,-326.061468184024)) ;
#41520 = CARTESIAN_POINT('Ctrl Pts',(6.83316032424528,17.2634333509648,-326.066460258774)) ;
#41521 = CARTESIAN_POINT('Ctrl Pts',(6.97610744357938,17.2061656373489,-326.068506329929)) ;
#41522 = CARTESIAN_POINT('Ctrl Pts',(7.61734833547387,16.9399658512253,-326.077768270067)) ;
#41523 = CARTESIAN_POINT('Ctrl Pts',(8.10708972261343,16.7111200423497,-326.085079526092)) ;
#41524 = CARTESIAN_POINT('Ctrl Pts',(8.87959769809157,16.3081814868363,-326.096781403116)) ;
#41525 = CARTESIAN_POINT('Ctrl Pts',(9.16890049363321,16.1473001833487,-326.101201819958)) ;
#41526 = CARTESIAN_POINT('Ctrl Pts',(9.53794795938075,15.9289553766288,-326.106825278383)) ;
#41527 = CARTESIAN_POINT('Ctrl Pts',(9.62175274208957,15.8784742616224,-326.108101129311)) ;
#41528 = CARTESIAN_POINT('Ctrl Pts',(9.76175127797173,15.7926286273999,-326.110227982068)) ;
#41529 = CARTESIAN_POINT('Ctrl Pts',(9.81816133616834,15.7576208543033,-326.111083645231)) ;
#41530 = CARTESIAN_POINT('Ctrl Pts',(9.94262275716697,15.6794529767418,-326.112968092511)) ;
#41531 = CARTESIAN_POINT('Ctrl Pts',(10.0105832149865,15.6361509541529,-326.113994998619)) ;
#41532 = CARTESIAN_POINT('Ctrl Pts',(10.2284840755446,15.495309239534,-326.117284190863)) ;
#41533 = CARTESIAN_POINT('Ctrl Pts',(10.3772976687841,15.3960445636133,-326.119525417212)) ;
#41534 = CARTESIAN_POINT('Ctrl Pts',(10.7584463457597,15.1337659764524,-326.125279728585)) ;
#41535 = CARTESIAN_POINT('Ctrl Pts',(10.988519753648,14.9675473755151,-326.128767328313)) ;
#41536 = CARTESIAN_POINT('Ctrl Pts',(11.7795489237345,14.3679882462425,-326.14093556031)) ;
#41537 = CARTESIAN_POINT('Ctrl Pts',(12.3194259018141,13.9078612343114,-326.14958450643)) ;
#41538 = CARTESIAN_POINT('Ctrl Pts',(12.9441869791235,13.3104004566808,-326.160461660875)) ;
#41539 = CARTESIAN_POINT('Ctrl Pts',(13.0553449789335,13.2013902395014,-326.162431908843)) ;
#41540 = CARTESIAN_POINT('Ctrl Pts',(13.2542764973676,13.0013323334899,-326.166025026664)) ;
#41541 = CARTESIAN_POINT('Ctrl Pts',(13.3425159324755,12.9107612654248,-326.167643535874)) ;
#41542 = CARTESIAN_POINT('Ctrl Pts',(13.5108770362846,12.7343818556155,-326.170780775693)) ;
#41543 = CARTESIAN_POINT('Ctrl Pts',(13.5911236568056,12.6487010098442,-326.172298275558)) ;
#41544 = CARTESIAN_POINT('Ctrl Pts',(13.6754495458126,12.5569355938576,-326.173916846399)) ;
#41545 = CARTESIAN_POINT('Ctrl Pts',(13.6803437417049,12.5516033596181,-326.174010873231)) ;
#41546 = CARTESIAN_POINT('Ctrl Pts',(13.6901452324564,12.5409120767852,-326.174199351987)) ;
#41547 = CARTESIAN_POINT('Ctrl Pts',(13.6950525009698,12.53555300731,-326.174293804089)) ;
#41548 = CARTESIAN_POINT('Ctrl Pts',(13.7049530641626,12.5247281694731,-326.174484540396)) ;
#41549 = CARTESIAN_POINT('Ctrl Pts',(13.7099462383262,12.5192622926547,-326.174580825599)) ;
#41550 = CARTESIAN_POINT('Ctrl Pts',(13.7200913125024,12.5081434384684,-326.174776641318)) ;
#41551 = CARTESIAN_POINT('Ctrl Pts',(13.7252429912914,12.5024902611718,-326.174876173678)) ;
#41552 = CARTESIAN_POINT('Ctrl Pts',(13.7357813666331,12.4909116471868,-326.175079977581)) ;
#41553 = CARTESIAN_POINT('Ctrl Pts',(13.7411677257626,12.4849859055675,-326.175184251938)) ;
#41554 = CARTESIAN_POINT('Ctrl Pts',(13.7522590624025,12.4727680256151,-326.175399188141)) ;
#41555 = CARTESIAN_POINT('Ctrl Pts',(13.7579635594468,12.466475453678,-326.175509853983)) ;
#41556 = CARTESIAN_POINT('Ctrl Pts',(13.7697860319488,12.4534162081856,-326.175739455722)) ;
#41557 = CARTESIAN_POINT('Ctrl Pts',(13.7759033422313,12.4466489355743,-326.17585839713)) ;
#41558 = CARTESIAN_POINT('Ctrl Pts',(13.7886620368946,12.4325137051817,-326.176106758803)) ;
#41559 = CARTESIAN_POINT('Ctrl Pts',(13.795302509049,12.4251449279689,-326.176236186588)) ;
#41560 = CARTESIAN_POINT('Ctrl Pts',(13.8092391290691,12.4096548408105,-326.176508166153)) ;
#41561 = CARTESIAN_POINT('Ctrl Pts',(13.8165340253887,12.4015324100333,-326.176650728187)) ;
#41562 = CARTESIAN_POINT('Ctrl Pts',(13.8319384075838,12.384350089389,-326.176952191856)) ;
#41563 = CARTESIAN_POINT('Ctrl Pts',(13.8400461661024,12.3752886579605,-326.17711110754)) ;
#41564 = CARTESIAN_POINT('Ctrl Pts',(13.8572700143265,12.3560007622214,-326.177449227903)) ;
#41565 = CARTESIAN_POINT('Ctrl Pts',(13.8663836983411,12.3457721595809,-326.17762845198)) ;
#41566 = CARTESIAN_POINT('Ctrl Pts',(13.8858566889508,12.3238681851777,-326.178012067424)) ;
#41567 = CARTESIAN_POINT('Ctrl Pts',(13.8962126102776,12.312189818289,-326.178216485804)) ;
#41568 = CARTESIAN_POINT('Ctrl Pts',(13.9184604434533,12.2870371229628,-326.178656519844)) ;
#41569 = CARTESIAN_POINT('Ctrl Pts',(13.9303475428202,12.2735585594862,-326.178892173418)) ;
#41570 = CARTESIAN_POINT('Ctrl Pts',(14.0709232952275,12.1136949919324,-326.181685407731)) ;
#41571 = CARTESIAN_POINT('Ctrl Pts',(14.1973184996401,11.9653096903167,-326.184260854254)) ;
#41572 = CARTESIAN_POINT('Ctrl Pts',(14.5752261720363,11.5072337821234,-326.192152766329)) ;
#41573 = CARTESIAN_POINT('Ctrl Pts',(14.8191138747671,11.1914034092077,-326.197516448595)) ;
#41574 = CARTESIAN_POINT('Ctrl Pts',(15.3527935327658,10.4522321093359,-326.209796607689)) ;
#41575 = CARTESIAN_POINT('Ctrl Pts',(15.6355986834255,10.0242446196427,-326.216716594901)) ;
#41576 = CARTESIAN_POINT('Ctrl Pts',(15.9584584533486,9.48866599888211,-326.224944745217)) ;
#41577 = CARTESIAN_POINT('Ctrl Pts',(16.0157134685856,9.3917038281846,-326.226417450865)) ;
#41578 = CARTESIAN_POINT('Ctrl Pts',(16.1030809785081,9.24062317281765,-326.228682473268)) ;
#41579 = CARTESIAN_POINT('Ctrl Pts',(16.1338107161249,9.18686483055236,-326.229482666142)) ;
#41580 = CARTESIAN_POINT('Ctrl Pts',(16.1872010205725,9.09237017134847,-326.230878448429)) ;
#41581 = CARTESIAN_POINT('Ctrl Pts',(16.2099781651642,9.05170039844211,-326.231475721017)) ;
#41582 = CARTESIAN_POINT('Ctrl Pts',(16.2791371337427,8.92711524405567,-326.233295431394)) ;
#41583 = CARTESIAN_POINT('Ctrl Pts',(16.3250223182117,8.84292591551947,-326.2345113965)) ;
#41584 = CARTESIAN_POINT('Ctrl Pts',(16.4264597894673,8.65332964535442,-326.237222982068)) ;
#41585 = CARTESIAN_POINT('Ctrl Pts',(16.4816537271513,8.54773570252579,-326.238714808704)) ;
#41586 = CARTESIAN_POINT('Ctrl Pts',(16.6516040885121,8.21482915009749,-326.24337048646)) ;
#41587 = CARTESIAN_POINT('Ctrl Pts',(16.7627030274991,7.9856824519716,-326.246506423549)) ;
#41588 = CARTESIAN_POINT('Ctrl Pts',(17.1742306399231,7.09042940512117,-326.258599155768)) ;
#41589 = CARTESIAN_POINT('Ctrl Pts',(17.4399499969237,6.40909758995289,-326.267493369391)) ;
#41590 = CARTESIAN_POINT('Ctrl Pts',(17.721280986405,5.53934572549684,-326.278974606326)) ;
#41591 = CARTESIAN_POINT('Ctrl Pts',(17.7751477760869,5.3639791436072,-326.281294064475)) ;
#41592 = CARTESIAN_POINT('Ctrl Pts',(17.8616219345275,5.06683764801474,-326.28523637947)) ;
#41593 = CARTESIAN_POINT('Ctrl Pts',(17.8956040020969,4.94547664341804,-326.28684990559)) ;
#41594 = CARTESIAN_POINT('Ctrl Pts',(17.9585426420398,4.71155510929684,-326.28996734179)) ;
#41595 = CARTESIAN_POINT('Ctrl Pts',(17.9876831053392,4.59905010126032,-326.291469934847)) ;
#41596 = CARTESIAN_POINT('Ctrl Pts',(18.0329229160626,4.41737842835324,-326.293901735486)) ;
#41597 = CARTESIAN_POINT('Ctrl Pts',(18.0496851019182,4.34838001882996,-326.294826577833)) ;
#41598 = CARTESIAN_POINT('Ctrl Pts',(18.0821235892296,4.21143305954911,-326.296664634176)) ;
#41599 = CARTESIAN_POINT('Ctrl Pts',(18.0978137127823,4.14348895498113,-326.297577744657)) ;
#41600 = CARTESIAN_POINT('Ctrl Pts',(18.1497936019229,3.91246756272262,-326.300686340654)) ;
#41601 = CARTESIAN_POINT('Ctrl Pts',(18.1842648154924,3.74898962828245,-326.302892678332)) ;
#41602 = CARTESIAN_POINT('Ctrl Pts',(18.3068415174889,3.12615040494634,-326.311318420687)) ;
#41603 = CARTESIAN_POINT('Ctrl Pts',(18.3797837939384,2.66398362450672,-326.317615691143)) ;
#41604 = CARTESIAN_POINT('Ctrl Pts',(18.4898188667436,1.74174464653576,-326.330126728078)) ;
#41605 = CARTESIAN_POINT('Ctrl Pts',(18.5273692870419,1.28205479994996,-326.336335596783)) ;
#41606 = CARTESIAN_POINT('Ctrl Pts',(18.5528417082755,0.706901559720696,-326.343913581851)) ;
#41607 = CARTESIAN_POINT('Ctrl Pts',(18.5568534445105,0.592313741152011,-326.345413679559)) ;
#41608 = CARTESIAN_POINT('Ctrl Pts',(18.561405495324,0.415454051365691,-326.3477103568)) ;
#41609 = CARTESIAN_POINT('Ctrl Pts',(18.5626943817849,0.353204375563594,-326.34851515907)) ;
#41610 = CARTESIAN_POINT('Ctrl Pts',(18.564615155673,0.230651730128177,-326.35009177426)) ;
#41611 = CARTESIAN_POINT('Ctrl Pts',(18.5652664147311,0.170349815297605,-326.350863819058)) ;
#41612 = CARTESIAN_POINT('Ctrl Pts',(18.566054124091,0.0374567727573222,-326.352558003735)) ;
#41613 = CARTESIAN_POINT('Ctrl Pts',(18.5660586650683,-0.0351341711078605,
-326.353478666443)) ;
#41614 = CARTESIAN_POINT('Ctrl Pts',(18.564125770088,-0.368260060632838,-326.357685219006)) ;
#41615 = CARTESIAN_POINT('Ctrl Pts',(18.5571299447306,-0.628736687137649,
-326.360922991914)) ;
#41616 = CARTESIAN_POINT('Ctrl Pts',(18.5446545937382,-0.888979978089834,
-326.364137692133)) ;
#41617 = CARTESIAN_POINT('Origin',(0.,0.,-315.477129595899)) ;
#41618 = CARTESIAN_POINT('',(18.5446545937613,-0.888979977608419,-328.159979993775)) ;
#41619 = CARTESIAN_POINT('',(18.5446545920456,-0.888980013399066,-327.863308833241)) ;
#41620 = CARTESIAN_POINT('',(18.544654593745,-0.888979977948782,-315.477129595899)) ;
#41621 = CARTESIAN_POINT('Ctrl Pts',(18.5446545937776,-0.888979977268111,
-328.159979993775)) ;
#41622 = CARTESIAN_POINT('Ctrl Pts',(18.5514236661009,-0.74777307568927,-328.158107862953)) ;
#41623 = CARTESIAN_POINT('Ctrl Pts',(18.5565798363497,-0.606490695771115,
-328.156227426047)) ;
#41624 = CARTESIAN_POINT('Ctrl Pts',(18.5745103188236,0.108944031999928,-328.146674608869)) ;
#41625 = CARTESIAN_POINT('Ctrl Pts',(18.5622535103131,0.683406818439957,-328.138893899993)) ;
#41626 = CARTESIAN_POINT('Ctrl Pts',(18.50367512622,1.54705962925855,-328.127288829815)) ;
#41627 = CARTESIAN_POINT('Ctrl Pts',(18.4771190513928,1.8372421840355,-328.123407637824)) ;
#41628 = CARTESIAN_POINT('Ctrl Pts',(18.4339502100328,2.21162630830476,-328.118469203763)) ;
#41629 = CARTESIAN_POINT('Ctrl Pts',(18.4235685762218,2.29650434744372,-328.117354249426)) ;
#41630 = CARTESIAN_POINT('Ctrl Pts',(18.4040025166416,2.44779182979563,-328.115377077128)) ;
#41631 = CARTESIAN_POINT('Ctrl Pts',(18.3950440658625,2.51422897316266,-328.114512357129)) ;
#41632 = CARTESIAN_POINT('Ctrl Pts',(18.3748785500496,2.6578991651199,-328.112650837349)) ;
#41633 = CARTESIAN_POINT('Ctrl Pts',(18.3635439724568,2.73511288519702,-328.111655459563)) ;
#41634 = CARTESIAN_POINT('Ctrl Pts',(18.3269994879263,2.97358868234219,-328.108594002804)) ;
#41635 = CARTESIAN_POINT('Ctrl Pts',(18.3001495906628,3.13459167957558,-328.106545167952)) ;
#41636 = CARTESIAN_POINT('Ctrl Pts',(18.1816729970637,3.79151512853311,-328.09822646062)) ;
#41637 = CARTESIAN_POINT('Ctrl Pts',(18.0719816867557,4.2839584596961,-328.092080765508)) ;
#41638 = CARTESIAN_POINT('Ctrl Pts',(17.8184540203618,5.23733927215678,-328.079987070465)) ;
#41639 = CARTESIAN_POINT('Ctrl Pts',(17.6764208224042,5.6983481810062,-328.074046866786)) ;
#41640 = CARTESIAN_POINT('Ctrl Pts',(17.4551371864372,6.32827613392892,-328.065663781168)) ;
#41641 = CARTESIAN_POINT('Ctrl Pts',(17.3910537002965,6.50231836059139,-328.063319523851)) ;
#41642 = CARTESIAN_POINT('Ctrl Pts',(17.2789487160083,6.79326078428456,-328.059348359552)) ;
#41643 = CARTESIAN_POINT('Ctrl Pts',(17.2323217200021,6.9106836781064,-328.057731124369)) ;
#41644 = CARTESIAN_POINT('Ctrl Pts',(17.1342673365167,7.15045407075271,-328.054397987917)) ;
#41645 = CARTESIAN_POINT('Ctrl Pts',(17.0827192780376,7.27274450139638,-328.052681315549)) ;
#41646 = CARTESIAN_POINT('Ctrl Pts',(16.9441070096523,7.59197598657199,-328.048155710286)) ;
#41647 = CARTESIAN_POINT('Ctrl Pts',(16.8549201960559,7.78797320661865,-328.045332280427)) ;
#41648 = CARTESIAN_POINT('Ctrl Pts',(16.6447984289805,8.22921202532305,-328.038877061763)) ;
#41649 = CARTESIAN_POINT('Ctrl Pts',(16.5218144660265,8.47342266383326,-328.035233214282)) ;
#41650 = CARTESIAN_POINT('Ctrl Pts',(16.228930238702,9.02436785952236,-328.026871083059)) ;
#41651 = CARTESIAN_POINT('Ctrl Pts',(16.0556437906125,9.32918507153438,-328.022140903281)) ;
#41652 = CARTESIAN_POINT('Ctrl Pts',(15.8248668895879,9.70963443683454,-328.016151596367)) ;
#41653 = CARTESIAN_POINT('Ctrl Pts',(15.775286849698,9.78998150088528,-328.014881854905)) ;
#41654 = CARTESIAN_POINT('Ctrl Pts',(15.553944201941,10.1426312612573,-328.009291616065)) ;
#41655 = CARTESIAN_POINT('Ctrl Pts',(15.3757280793041,10.4108182152703,-328.004993680335)) ;
#41656 = CARTESIAN_POINT('Ctrl Pts',(15.1343471417449,10.7543302332678,-327.999487668842)) ;
#41657 = CARTESIAN_POINT('Ctrl Pts',(15.0774330586572,10.8339787047613,-327.998211034885)) ;
#41658 = CARTESIAN_POINT('Ctrl Pts',(14.9808635069289,10.9668881851245,-327.996083312137)) ;
#41659 = CARTESIAN_POINT('Ctrl Pts',(14.9415474705939,11.0203932369666,-327.995227552588)) ;
#41660 = CARTESIAN_POINT('Ctrl Pts',(14.8539018102926,11.1383386770644,-327.99334343574)) ;
#41661 = CARTESIAN_POINT('Ctrl Pts',(14.8054382242945,11.2026776480181,-327.99231695049)) ;
#41662 = CARTESIAN_POINT('Ctrl Pts',(14.6481407455602,11.4086979942674,-327.989030902338)) ;
#41663 = CARTESIAN_POINT('Ctrl Pts',(14.537679882563,11.5491246878927,-327.986792343972)) ;
#41664 = CARTESIAN_POINT('Ctrl Pts',(14.2468988310866,11.9080056549176,-327.981047502236)) ;
#41665 = CARTESIAN_POINT('Ctrl Pts',(14.0635753022643,12.1239669706998,-327.977566604872)) ;
#41666 = CARTESIAN_POINT('Ctrl Pts',(13.403508753563,12.8664228830841,-327.965387487122)) ;
#41667 = CARTESIAN_POINT('Ctrl Pts',(12.9015675410471,13.3696835895997,-327.956721520582)) ;
#41668 = CARTESIAN_POINT('Ctrl Pts',(12.2561133616275,13.9465535668615,-327.945828610059)) ;
#41669 = CARTESIAN_POINT('Ctrl Pts',(12.1388948400138,14.0486975587308,-327.943860965151)) ;
#41670 = CARTESIAN_POINT('Ctrl Pts',(11.9240769158918,14.2311934087864,-327.940271031904)) ;
#41671 = CARTESIAN_POINT('Ctrl Pts',(11.8269133605756,14.312043754912,-327.938653076501)) ;
#41672 = CARTESIAN_POINT('Ctrl Pts',(11.6261370864121,14.4756699593801,-327.935320539035)) ;
#41673 = CARTESIAN_POINT('Ctrl Pts',(11.5224478176042,14.5583405837799,-327.933605207558)) ;
#41674 = CARTESIAN_POINT('Ctrl Pts',(11.2485385094423,14.7719667413822,-327.929088370955)) ;
#41675 = CARTESIAN_POINT('Ctrl Pts',(11.0769165555979,14.901091885372,-327.926272475912)) ;
#41676 = CARTESIAN_POINT('Ctrl Pts',(10.6826588486031,15.1871482129532,-327.919839029859)) ;
#41677 = CARTESIAN_POINT('Ctrl Pts',(10.4587320854737,15.3422160614638,-327.916209550792)) ;
#41678 = CARTESIAN_POINT('Ctrl Pts',(9.93780994252413,15.6862451419727,-327.907843862582)) ;
#41679 = CARTESIAN_POINT('Ctrl Pts',(9.63868924464666,15.8717995960812,-327.903095249167)) ;
#41680 = CARTESIAN_POINT('Ctrl Pts',(9.25188533949489,16.0967775020261,-327.897072193654)) ;
#41681 = CARTESIAN_POINT('Ctrl Pts',(9.16892475941206,16.1441768774129,-327.895787195699)) ;
#41682 = CARTESIAN_POINT('Ctrl Pts',(8.8047346771958,16.3485434805822,-327.890180201155)) ;
#41683 = CARTESIAN_POINT('Ctrl Pts',(8.51981320106167,16.4988184557095,-327.88588078533)) ;
#41684 = CARTESIAN_POINT('Ctrl Pts',(8.1435958069966,16.6848998438459,-327.880376650738)) ;
#41685 = CARTESIAN_POINT('Ctrl Pts',(8.05572434380301,16.7275025273885,-327.879103198085)) ;
#41686 = CARTESIAN_POINT('Ctrl Pts',(7.90757405298156,16.7978920354829,-327.876979007491)) ;
#41687 = CARTESIAN_POINT('Ctrl Pts',(7.84747501658886,16.8260524228929,-327.876123637079)) ;
#41688 = CARTESIAN_POINT('Ctrl Pts',(7.71397949505441,16.887733126861,-327.874238166229)) ;
#41689 = CARTESIAN_POINT('Ctrl Pts',(7.64051302451444,16.9210983851681,-327.873209962154)) ;
#41690 = CARTESIAN_POINT('Ctrl Pts',(7.40287570612491,17.0271596825096,-327.869911056702)) ;
#41691 = CARTESIAN_POINT('Ctrl Pts',(7.23786693920372,17.0979536186422,-327.867661586251)) ;
#41692 = CARTESIAN_POINT('Ctrl Pts',(6.80785986210398,17.2750995957218,-327.861877950311)) ;
#41693 = CARTESIAN_POINT('Ctrl Pts',(6.54138851891774,17.3777518282403,-327.858369578704)) ;
#41694 = CARTESIAN_POINT('Ctrl Pts',(5.60989529042941,17.712126532224,-327.846237293141)) ;
#41695 = CARTESIAN_POINT('Ctrl Pts',(4.93413579302475,17.91213708527,-327.837643330999)) ;
#41696 = CARTESIAN_POINT('Ctrl Pts',(4.09639306218631,18.1090730846715,-327.826816509335)) ;
#41697 = CARTESIAN_POINT('Ctrl Pts',(3.94368560732016,18.1429409920813,-327.824837290935)) ;
#41698 = CARTESIAN_POINT('Ctrl Pts',(3.66662818428516,18.2007243418371,-327.821233184179)) ;
#41699 = CARTESIAN_POINT('Ctrl Pts',(3.54242670584466,18.2253049848144,-327.819612752121)) ;
#41700 = CARTESIAN_POINT('Ctrl Pts',(3.28796509167005,18.2729659013395,-327.816282120425)) ;
#41701 = CARTESIAN_POINT('Ctrl Pts',(3.15769011973695,18.2959282443259,-327.814571244279)) ;
#41702 = CARTESIAN_POINT('Ctrl Pts',(2.81714043964998,18.3522080712358,-327.810083543326)) ;
#41703 = CARTESIAN_POINT('Ctrl Pts',(2.60651869309998,18.3833044201638,-327.807292682273)) ;
#41704 = CARTESIAN_POINT('Ctrl Pts',(2.12879192037522,18.4454610256195,-327.800931345266)) ;
#41705 = CARTESIAN_POINT('Ctrl Pts',(1.86145305566809,18.4743546468227,-327.797349368403)) ;
#41706 = CARTESIAN_POINT('Ctrl Pts',(1.23914259885147,18.5279676283469,-327.788981354838)) ;
#41707 = CARTESIAN_POINT('Ctrl Pts',(0.883899345031587,18.5483093678236,-327.7841813309)) ;
#41708 = CARTESIAN_POINT('Ctrl Pts',(0.269479611282192,18.5657996939309,-327.775907362587)) ;
#41709 = CARTESIAN_POINT('Ctrl Pts',(0.0105411719020318,18.5677523316723,
-327.772429441677)) ;
#41710 = CARTESIAN_POINT('Ctrl Pts',(-0.440783130971584,18.5617145082437,
-327.766421026055)) ;
#41711 = CARTESIAN_POINT('Ctrl Pts',(-0.633161600439865,18.556148357681,-327.763877001331)) ;
#41712 = CARTESIAN_POINT('Ctrl Pts',(-0.909954411501939,18.5438303156014,
-327.76025674032)) ;
#41713 = CARTESIAN_POINT('Ctrl Pts',(-0.994463280493784,18.5394903548087,
-327.759156825267)) ;
#41714 = CARTESIAN_POINT('Ctrl Pts',(-1.13808604847684,18.5311297471719,-327.757298415554)) ;
#41715 = CARTESIAN_POINT('Ctrl Pts',(-1.19721552606026,18.5274036106528,-327.756536556009)) ;
#41716 = CARTESIAN_POINT('Ctrl Pts',(-1.34324105043619,18.5174996096544,-327.754662929474)) ;
#41717 = CARTESIAN_POINT('Ctrl Pts',(-1.43011325053917,18.5109930698828,-327.753554964077)) ;
#41718 = CARTESIAN_POINT('Ctrl Pts',(-1.74237073753988,18.4853943899725,-327.74959179762)) ;
#41719 = CARTESIAN_POINT('Ctrl Pts',(-1.96744886835411,18.4627952071018,-327.746771216131)) ;
#41720 = CARTESIAN_POINT('Ctrl Pts',(-2.61838087987808,18.3853991413432,-327.738658448875)) ;
#41721 = CARTESIAN_POINT('Ctrl Pts',(-3.04281762954468,18.3199367309319,-327.733421447103)) ;
#41722 = CARTESIAN_POINT('Ctrl Pts',(-3.68005324412878,18.1988956026787,-327.725468024274)) ;
#41723 = CARTESIAN_POINT('Ctrl Pts',(-3.89476143282105,18.1541572735682,-327.72277308522)) ;
#41724 = CARTESIAN_POINT('Ctrl Pts',(-4.43106801412754,18.0324556873001,-327.715976066692)) ;
#41725 = CARTESIAN_POINT('Ctrl Pts',(-4.75149681272042,17.9506852016331,-327.711854687536)) ;
#41726 = CARTESIAN_POINT('Ctrl Pts',(-5.21696865942547,17.8185637507548,-327.705742772273)) ;
#41727 = CARTESIAN_POINT('Ctrl Pts',(-5.36384335339008,17.7749025460605,-327.703795964642)) ;
#41728 = CARTESIAN_POINT('Ctrl Pts',(-5.6285406238717,17.6926368101363,-327.700251909802)) ;
#41729 = CARTESIAN_POINT('Ctrl Pts',(-5.74654908214465,17.6546605871006,-327.698658995785)) ;
#41730 = CARTESIAN_POINT('Ctrl Pts',(-6.00544154793853,17.5684757775857,-327.695135170074)) ;
#41731 = CARTESIAN_POINT('Ctrl Pts',(-6.1461438274027,17.5197484370892,-327.693200820047)) ;
#41732 = CARTESIAN_POINT('Ctrl Pts',(-6.58379266741056,17.3622628878616,-327.687123796617)) ;
#41733 = CARTESIAN_POINT('Ctrl Pts',(-6.87855595940369,17.2476075337035,-327.682942521881)) ;
#41734 = CARTESIAN_POINT('Ctrl Pts',(-7.65372471160755,16.9230530811344,-327.671735681111)) ;
#41735 = CARTESIAN_POINT('Ctrl Pts',(-8.12841371961347,16.7002429983047,-327.664647659642)) ;
#41736 = CARTESIAN_POINT('Ctrl Pts',(-8.90430989177654,16.2951241194049,-327.652883440994)) ;
#41737 = CARTESIAN_POINT('Ctrl Pts',(-9.21091004192311,16.1238004760479,-327.648187767002)) ;
#41738 = CARTESIAN_POINT('Ctrl Pts',(-9.59746848012484,15.8931713417723,-327.642282942083)) ;
#41739 = CARTESIAN_POINT('Ctrl Pts',(-9.68206310077038,15.8417786463616,-327.640991805535)) ;
#41740 = CARTESIAN_POINT('Ctrl Pts',(-9.82282137187132,15.7547169280661,-327.638847915492)) ;
#41741 = CARTESIAN_POINT('Ctrl Pts',(-9.87921149240667,15.7194181034803,-327.637990316585)) ;
#41742 = CARTESIAN_POINT('Ctrl Pts',(-10.002938726135,15.641039165701,-327.636112053575)) ;
#41743 = CARTESIAN_POINT('Ctrl Pts',(-10.0701896683495,15.5978257910775,-327.635093153589)) ;
#41744 = CARTESIAN_POINT('Ctrl Pts',(-10.2835872461133,15.4587477193681,-327.631863255471)) ;
#41745 = CARTESIAN_POINT('Ctrl Pts',(-10.4286603605162,15.361252910214,-327.629672287387)) ;
#41746 = CARTESIAN_POINT('Ctrl Pts',(-10.7971234600206,15.1060055067624,-327.624094693858)) ;
#41747 = CARTESIAN_POINT('Ctrl Pts',(-11.0184440805897,14.945339333836,-327.620731730159)) ;
#41748 = CARTESIAN_POINT('Ctrl Pts',(-11.8173135761429,14.338011808623,-327.608425168961)) ;
#41749 = CARTESIAN_POINT('Ctrl Pts',(-12.3719260776933,13.8622843655092,-327.599524322198)) ;
#41750 = CARTESIAN_POINT('Ctrl Pts',(-13.0077152623174,13.2483016791433,-327.588398909745)) ;
#41751 = CARTESIAN_POINT('Ctrl Pts',(-13.1170167730301,13.1400922604503,-327.586451876793)) ;
#41752 = CARTESIAN_POINT('Ctrl Pts',(-13.313418804879,12.9407597892092,-327.582887094733)) ;
#41753 = CARTESIAN_POINT('Ctrl Pts',(-13.4009600068065,12.850083853392,-327.581273459958)) ;
#41754 = CARTESIAN_POINT('Ctrl Pts',(-13.5791245074397,12.6617386793108,-327.577936997862)) ;
#41755 = CARTESIAN_POINT('Ctrl Pts',(-13.6696334386174,12.5639711223193,-327.576213287411)) ;
#41756 = CARTESIAN_POINT('Ctrl Pts',(-13.905629483459,12.3034795878385,-327.571641644171)) ;
#41757 = CARTESIAN_POINT('Ctrl Pts',(-14.0493126197095,12.1391497210655,-327.568778647713)) ;
#41758 = CARTESIAN_POINT('Ctrl Pts',(-14.3699548662752,11.7591120740141,-327.562208563336)) ;
#41759 = CARTESIAN_POINT('Ctrl Pts',(-14.5450165075369,11.5418722048661,-327.558488714931)) ;
#41760 = CARTESIAN_POINT('Ctrl Pts',(-14.9668816152219,10.9935178336856,-327.549212789759)) ;
#41761 = CARTESIAN_POINT('Ctrl Pts',(-15.2076600057518,10.6579574189557,-327.543633533081)) ;
#41762 = CARTESIAN_POINT('Ctrl Pts',(-15.624455592337,10.0341752891427,-327.533553618611)) ;
#41763 = CARTESIAN_POINT('Ctrl Pts',(-15.804183263217,9.74864495568453,-327.529045062872)) ;
#41764 = CARTESIAN_POINT('Ctrl Pts',(-16.0272596668256,9.37184924323189,-327.52329879195)) ;
#41765 = CARTESIAN_POINT('Ctrl Pts',(-16.0777832992068,9.28490683275527,-327.521986682754)) ;
#41766 = CARTESIAN_POINT('Ctrl Pts',(-16.1606556660085,9.13959302190165,-327.519819237928)) ;
#41767 = CARTESIAN_POINT('Ctrl Pts',(-16.1934004430646,9.08145001032745,-327.518958803865)) ;
#41768 = CARTESIAN_POINT('Ctrl Pts',(-16.264277714269,8.95399507604674,-327.517088144213)) ;
#41769 = CARTESIAN_POINT('Ctrl Pts',(-16.3022820381042,8.88461354037111,-327.516079534554)) ;
#41770 = CARTESIAN_POINT('Ctrl Pts',(-16.4203865304267,8.66569004043984,-327.512924339698)) ;
#41771 = CARTESIAN_POINT('Ctrl Pts',(-16.4988813123755,8.51529173302976,-327.510796523704)) ;
#41772 = CARTESIAN_POINT('Ctrl Pts',(-16.6928172863068,8.13095293246788,-327.505436187141)) ;
#41773 = CARTESIAN_POINT('Ctrl Pts',(-16.8054095773649,7.89561611429601,-327.502225172456)) ;
#41774 = CARTESIAN_POINT('Ctrl Pts',(-17.2278258307727,6.96269073945524,-327.489659864137)) ;
#41775 = CARTESIAN_POINT('Ctrl Pts',(-17.4994703596249,6.24864647875538,-327.480364867702)) ;
#41776 = CARTESIAN_POINT('Ctrl Pts',(-17.7750465603044,5.36367383838616,-327.468686402988)) ;
#41777 = CARTESIAN_POINT('Ctrl Pts',(-17.8216310066909,5.20679800042396,-327.466611903218)) ;
#41778 = CARTESIAN_POINT('Ctrl Pts',(-17.9001204887222,4.92907708628152,-327.462928705667)) ;
#41779 = CARTESIAN_POINT('Ctrl Pts',(-17.9328905953612,4.80848721286577,-327.46132592238)) ;
#41780 = CARTESIAN_POINT('Ctrl Pts',(-17.999772577633,4.55217191135093,-327.45791093117)) ;
#41781 = CARTESIAN_POINT('Ctrl Pts',(-18.0335723387819,4.41637301256079,-327.456096748898)) ;
#41782 = CARTESIAN_POINT('Ctrl Pts',(-18.125137586258,4.02989561841148,-327.450919595292)) ;
#41783 = CARTESIAN_POINT('Ctrl Pts',(-18.1792328514543,3.77838109901227,-327.447533319043)) ;
#41784 = CARTESIAN_POINT('Ctrl Pts',(-18.3858176098867,2.71036293994219,-327.433098767163)) ;
#41785 = CARTESIAN_POINT('Ctrl Pts',(-18.4886508985518,1.88524103443056,-327.42176657293)) ;
#41786 = CARTESIAN_POINT('Ctrl Pts',(-18.5459508936432,0.8794732821184,-327.408380839249)) ;
#41787 = CARTESIAN_POINT('Ctrl Pts',(-18.5534860873437,0.702795843586862,
-327.406047453231)) ;
#41788 = CARTESIAN_POINT('Ctrl Pts',(-18.560801208355,0.444719893812653,-327.402677620649)) ;
#41789 = CARTESIAN_POINT('Ctrl Pts',(-18.5625716581819,0.363387863963918,
-327.401621231686)) ;
#41790 = CARTESIAN_POINT('Ctrl Pts',(-18.5648043497484,0.216436144751031,
-327.39972427871)) ;
#41791 = CARTESIAN_POINT('Ctrl Pts',(-18.5654533534118,0.150820847200539,
-327.398881658952)) ;
#41792 = CARTESIAN_POINT('Ctrl Pts',(-18.5661951426942,-0.010814504401239,
-327.396816064613)) ;
#41793 = CARTESIAN_POINT('Ctrl Pts',(-18.5658909149383,-0.106834464789306,
-327.39559759206)) ;
#41794 = CARTESIAN_POINT('Ctrl Pts',(-18.5613098599187,-0.526097339364414,
-327.390307267628)) ;
#41795 = CARTESIAN_POINT('Ctrl Pts',(-18.5493358889197,-0.849200302216394,
-327.386307360137)) ;
#41796 = CARTESIAN_POINT('Ctrl Pts',(-18.4903713354712,-1.78154877808444,
-327.37481959073)) ;
#41797 = CARTESIAN_POINT('Ctrl Pts',(-18.4217384227802,-2.38899615268031,
-327.367391771039)) ;
#41798 = CARTESIAN_POINT('Ctrl Pts',(-18.278030612562,-3.26908998607008,-327.3563214251)) ;
#41799 = CARTESIAN_POINT('Ctrl Pts',(-18.2264960909448,-3.54516462091775,
-327.352806162819)) ;
#41800 = CARTESIAN_POINT('Ctrl Pts',(-18.1391487804232,-3.96061068414821,
-327.347431129771)) ;
#41801 = CARTESIAN_POINT('Ctrl Pts',(-18.1079456588277,-4.1009095832651,-327.345601253152)) ;
#41802 = CARTESIAN_POINT('Ctrl Pts',(-18.0469886325038,-4.36071836482692,
-327.342183470692)) ;
#41803 = CARTESIAN_POINT('Ctrl Pts',(-18.0176685178356,-4.48032191818991,
-327.340598530517)) ;
#41804 = CARTESIAN_POINT('Ctrl Pts',(-17.9476992302533,-4.75394180504,-327.33694539926)) ;
#41805 = CARTESIAN_POINT('Ctrl Pts',(-17.9062535225901,-4.9077443926778,-327.33487202255)) ;
#41806 = CARTESIAN_POINT('Ctrl Pts',(-17.7516327893757,-5.45347992247736,
-327.327444334254)) ;
#41807 = CARTESIAN_POINT('Ctrl Pts',(-17.6275265602583,-5.84219272007735,
-327.322020430568)) ;
#41808 = CARTESIAN_POINT('Ctrl Pts',(-17.352243789891,-6.61548316633229,-327.311015217826)) ;
#41809 = CARTESIAN_POINT('Ctrl Pts',(-17.2008326364957,-6.99973844019897,
-327.30543590737)) ;
#41810 = CARTESIAN_POINT('Ctrl Pts',(-16.9040824459968,-7.68491421727396,
-327.295403607562)) ;
#41811 = CARTESIAN_POINT('Ctrl Pts',(-16.7631922313316,-7.98757139911168,
-327.290942221022)) ;
#41812 = CARTESIAN_POINT('Ctrl Pts',(-16.568632917638,-8.37766884585339,-327.285219499371)) ;
#41813 = CARTESIAN_POINT('Ctrl Pts',(-16.5222925780093,-8.46869411787894,
-327.283886265325)) ;
#41814 = CARTESIAN_POINT('Ctrl Pts',(-16.4443388788663,-8.61874122268755,
-327.281694909126)) ;
#41815 = CARTESIAN_POINT('Ctrl Pts',(-16.4131531957676,-8.67798269406289,
-327.280831432953)) ;
#41816 = CARTESIAN_POINT('Ctrl Pts',(-16.3447854262572,-8.80616968498797,
-327.278967499968)) ;
#41817 = CARTESIAN_POINT('Ctrl Pts',(-16.3074861233423,-8.8750510708676,-327.27796851838)) ;
#41818 = CARTESIAN_POINT('Ctrl Pts',(-16.1902920340095,-9.08824247517432,
-327.274881778293)) ;
#41819 = CARTESIAN_POINT('Ctrl Pts',(-16.1089091245678,-9.23172542978836,
-327.272811669052)) ;
#41820 = CARTESIAN_POINT('Ctrl Pts',(-15.7696201586022,-9.81176136129259,
-327.264439331465)) ;
#41821 = CARTESIAN_POINT('Ctrl Pts',(-15.4957938578941,-10.2387477706868,
-327.258261456983)) ;
#41822 = CARTESIAN_POINT('Ctrl Pts',(-15.1886577808932,-10.6770767949344,
-327.251699502731)) ;
#41823 = CARTESIAN_POINT('Ctrl Pts',(-15.1724285996487,-10.7001263758161,
-327.25135379923)) ;
#41824 = CARTESIAN_POINT('Ctrl Pts',(-15.1283131277772,-10.7624794407218,
-327.25041679795)) ;
#41825 = CARTESIAN_POINT('Ctrl Pts',(-15.1003262046303,-10.8017114531394,
-327.249825284613)) ;
#41826 = CARTESIAN_POINT('Ctrl Pts',(-14.8081418481186,-11.2079400880309,
-327.24367873995)) ;
#41827 = CARTESIAN_POINT('Ctrl Pts',(-14.5307733859594,-11.5652760229603,
-327.238082952568)) ;
#41828 = CARTESIAN_POINT('Ctrl Pts',(-14.1367958958321,-12.0362658004772,
-327.230343472799)) ;
#41829 = CARTESIAN_POINT('Ctrl Pts',(-14.0313367934658,-12.1590410930342,
-327.228291120769)) ;
#41830 = CARTESIAN_POINT('Ctrl Pts',(-13.8417648553699,-12.3739892405408,
-327.224632574078)) ;
#41831 = CARTESIAN_POINT('Ctrl Pts',(-13.7583026999586,-12.4667225364614,
-327.223032017125)) ;
#41832 = CARTESIAN_POINT('Ctrl Pts',(-13.5785951187415,-12.662389588663,-327.219606332395)) ;
#41833 = CARTESIAN_POINT('Ctrl Pts',(-13.482099601088,-12.7650830692869,-327.217779062408)) ;
#41834 = CARTESIAN_POINT('Ctrl Pts',(-13.2020702005939,-13.0563813268648,
-327.212510596744)) ;
#41835 = CARTESIAN_POINT('Ctrl Pts',(-13.0156833401025,-13.2421953495966,
-327.209044717675)) ;
#41836 = CARTESIAN_POINT('Ctrl Pts',(-12.5552806087895,-13.6820687703149,
-327.2005905873)) ;
#41837 = CARTESIAN_POINT('Ctrl Pts',(-12.2774229119273,-13.931940381478,-327.195574786715)) ;
#41838 = CARTESIAN_POINT('Ctrl Pts',(-11.5712185273036,-14.5294710303161,
-327.18311892877)) ;
#41839 = CARTESIAN_POINT('Ctrl Pts',(-11.1345579301039,-14.8667497180024,
-327.175663153653)) ;
#41840 = CARTESIAN_POINT('Ctrl Pts',(-10.5900922646953,-15.249836031741,-327.166901032792)) ;
#41841 = CARTESIAN_POINT('Ctrl Pts',(-10.4960458064753,-15.3147176160413,
-327.165406303006)) ;
#41842 = CARTESIAN_POINT('Ctrl Pts',(-10.3498883158809,-15.4135712760725,
-327.163115835329)) ;
#41843 = CARTESIAN_POINT('Ctrl Pts',(-10.2981954558067,-15.4481564596052,
-327.162311942901)) ;
#41844 = CARTESIAN_POINT('Ctrl Pts',(-10.1869326175048,-15.5217903759263,
-327.160595785637)) ;
#41845 = CARTESIAN_POINT('Ctrl Pts',(-10.1273097168511,-15.560757389801,-327.159684743718)) ;
#41846 = CARTESIAN_POINT('Ctrl Pts',(-9.96153345483602,-15.6677453926956,
-327.157173408724)) ;
#41847 = CARTESIAN_POINT('Ctrl Pts',(-9.85490913579416,-15.7350297256176,
-327.155582643134)) ;
#41848 = CARTESIAN_POINT('Ctrl Pts',(-9.60441023937502,-15.8895598517041,
-327.151893241897)) ;
#41849 = CARTESIAN_POINT('Ctrl Pts',(-9.46001842968493,-15.9759462870097,
-327.149802871131)) ;
#41850 = CARTESIAN_POINT('Ctrl Pts',(-8.88572465180983,-16.3090175303576,
-327.141597846437)) ;
#41851 = CARTESIAN_POINT('Ctrl Pts',(-8.44719131233928,-16.5404085669056,
-327.135565105366)) ;
#41852 = CARTESIAN_POINT('Ctrl Pts',(-7.64130406698794,-16.9252150392383,
-327.124589088361)) ;
#41853 = CARTESIAN_POINT('Ctrl Pts',(-7.27727737228563,-17.0848958171024,
-327.119670921124)) ;
#41854 = CARTESIAN_POINT('Ctrl Pts',(-6.74251446880614,-17.2992757539046,
-327.11242913343)) ;
#41855 = CARTESIAN_POINT('Ctrl Pts',(-6.57566939725639,-17.3633814336151,
-327.110167814012)) ;
#41856 = CARTESIAN_POINT('Ctrl Pts',(-6.2891347346609,-17.4687521912117,-327.106276837682)) ;
#41857 = CARTESIAN_POINT('Ctrl Pts',(-6.16990099998421,-17.5112204150779,
-327.104655563008)) ;
#41858 = CARTESIAN_POINT('Ctrl Pts',(-5.92261114097204,-17.5964599248182,
-327.101287654776)) ;
#41859 = CARTESIAN_POINT('Ctrl Pts',(-5.79450390610891,-17.6390603216107,
-327.099539962321)) ;
#41860 = CARTESIAN_POINT('Ctrl Pts',(-5.44847080802769,-17.7499525848289,
-327.094810899392)) ;
#41861 = CARTESIAN_POINT('Ctrl Pts',(-5.22973104848556,-17.8156269541973,
-327.091812466516)) ;
#41862 = CARTESIAN_POINT('Ctrl Pts',(-4.85678299514989,-17.9201401541632,
-327.086688671639)) ;
#41863 = CARTESIAN_POINT('Ctrl Pts',(-4.70318576815724,-17.9610636587855,
-327.084575261249)) ;
#41864 = CARTESIAN_POINT('Ctrl Pts',(-3.98942674238782,-18.1414495858339,
-327.07474776227)) ;
#41865 = CARTESIAN_POINT('Ctrl Pts',(-3.42348088469581,-18.2567109658516,
-327.066926043834)) ;
#41866 = CARTESIAN_POINT('Ctrl Pts',(-2.56878330767499,-18.3896339221145,
-327.055331943312)) ;
#41867 = CARTESIAN_POINT('Ctrl Pts',(-2.28348873981796,-18.4272342807755,
-327.051499995821)) ;
#41868 = CARTESIAN_POINT('Ctrl Pts',(-1.91256883872709,-18.4673730273998,
-327.046611292322)) ;
#41869 = CARTESIAN_POINT('Ctrl Pts',(-1.82763975579113,-18.4759713965464,
-327.045498301421)) ;
#41870 = CARTESIAN_POINT('Ctrl Pts',(-1.675941986275,-18.4902733337497,-327.043523483468)) ;
#41871 = CARTESIAN_POINT('Ctrl Pts',(-1.60919600971362,-18.4962017111698,
-327.042659173489)) ;
#41872 = CARTESIAN_POINT('Ctrl Pts',(-1.46455463878849,-18.5082598894619,
-327.040796877442)) ;
#41873 = CARTESIAN_POINT('Ctrl Pts',(-1.38664982029901,-18.5142595510569,
-327.039800330669)) ;
#41874 = CARTESIAN_POINT('Ctrl Pts',(-1.14533825512362,-18.5313119635857,
-327.036730692307)) ;
#41875 = CARTESIAN_POINT('Ctrl Pts',(-0.981821245929157,-18.5406944316804,
-327.034674975439)) ;
#41876 = CARTESIAN_POINT('Ctrl Pts',(-0.313506704967963,-18.5701756938317,
-327.026338916175)) ;
#41877 = CARTESIAN_POINT('Ctrl Pts',(0.191887371361827,-18.5718306373701,
-327.020182809343)) ;
#41878 = CARTESIAN_POINT('Ctrl Pts',(1.22062211292943,-18.5331983854704,-327.007562259969)) ;
#41879 = CARTESIAN_POINT('Ctrl Pts',(1.74345568850655,-18.4913417950225,-327.001099473812)) ;
#41880 = CARTESIAN_POINT('Ctrl Pts',(2.41291219286764,-18.4090988322846,-326.992603213681)) ;
#41881 = CARTESIAN_POINT('Ctrl Pts',(2.56178206666474,-18.3889732618692,-326.990700301306)) ;
#41882 = CARTESIAN_POINT('Ctrl Pts',(2.83557243895069,-18.3485705150837,-326.987172986941)) ;
#41883 = CARTESIAN_POINT('Ctrl Pts',(2.96056149595839,-18.3288184719743,-326.985552074971)) ;
#41884 = CARTESIAN_POINT('Ctrl Pts',(3.21852982610359,-18.2853440999976,-326.982183619128)) ;
#41885 = CARTESIAN_POINT('Ctrl Pts',(3.35147185961615,-18.2614451620175,-326.980435002656)) ;
#41886 = CARTESIAN_POINT('Ctrl Pts',(3.70883502945817,-18.193168289506,-326.975699847009)) ;
#41887 = CARTESIAN_POINT('Ctrl Pts',(3.93271592844854,-18.1460897939941,-326.972696166128)) ;
#41888 = CARTESIAN_POINT('Ctrl Pts',(4.31098450706341,-18.0592166810187,-326.967561551573)) ;
#41889 = CARTESIAN_POINT('Ctrl Pts',(4.46583391836849,-18.0215488203166,-326.965442583824)) ;
#41890 = CARTESIAN_POINT('Ctrl Pts',(5.18238885029603,-17.837440716041,-326.955566115804)) ;
#41891 = CARTESIAN_POINT('Ctrl Pts',(5.73751336929836,-17.6667026820205,-326.947699876506)) ;
#41892 = CARTESIAN_POINT('Ctrl Pts',(6.55027754241457,-17.3743663462364,-326.936124556613)) ;
#41893 = CARTESIAN_POINT('Ctrl Pts',(6.8146020496616,-17.2724040391494,-326.932352769708)) ;
#41894 = CARTESIAN_POINT('Ctrl Pts',(7.15545619310193,-17.1318779350348,-326.927521645893)) ;
#41895 = CARTESIAN_POINT('Ctrl Pts',(7.23419666587833,-17.0987775451559,-326.926407967078)) ;
#41896 = CARTESIAN_POINT('Ctrl Pts',(7.37430694715388,-17.0387378622034,-326.924432324568)) ;
#41897 = CARTESIAN_POINT('Ctrl Pts',(7.43576460007991,-17.0120073988872,-326.923567871249)) ;
#41898 = CARTESIAN_POINT('Ctrl Pts',(7.56852706755423,-16.9534066570074,-326.921705848671)) ;
#41899 = CARTESIAN_POINT('Ctrl Pts',(7.63977811235016,-16.9214180749242,-326.920709712633)) ;
#41900 = CARTESIAN_POINT('Ctrl Pts',(7.85963152476459,-16.8210419030549,-326.917642951098)) ;
#41901 = CARTESIAN_POINT('Ctrl Pts',(8.00753364832913,-16.751139168346,-326.915589654346)) ;
#41902 = CARTESIAN_POINT('Ctrl Pts',(8.60806260536747,-16.4575410123078,-326.907259696739)) ;
#41903 = CARTESIAN_POINT('Ctrl Pts',(9.05239930101172,-16.2173816356411,-326.901107251101)) ;
#41904 = CARTESIAN_POINT('Ctrl Pts',(9.89992404181671,-15.7136065167819,-326.889020299012)) ;
#41905 = CARTESIAN_POINT('Ctrl Pts',(10.3037426475419,-15.4518222876854,-326.883093875213)) ;
#41906 = CARTESIAN_POINT('Ctrl Pts',(10.8485254486814,-15.0677932309612,-326.874725006155)) ;
#41907 = CARTESIAN_POINT('Ctrl Pts',(10.9985043757455,-14.9586696802507,-326.872380608035)) ;
#41908 = CARTESIAN_POINT('Ctrl Pts',(11.2478581320256,-14.7714640001729,-326.868409279703)) ;
#41909 = CARTESIAN_POINT('Ctrl Pts',(11.3481163179081,-14.6945812205917,-326.866792023233)) ;
#41910 = CARTESIAN_POINT('Ctrl Pts',(11.5520577639608,-14.5348571101698,-326.863458904786)) ;
#41911 = CARTESIAN_POINT('Ctrl Pts',(11.6556532728351,-14.4519153234459,-326.861742272353)) ;
#41912 = CARTESIAN_POINT('Ctrl Pts',(11.763731802875,-14.3634662190082,-326.859926218642)) ;
#41913 = CARTESIAN_POINT('Ctrl Pts',(11.7691105724771,-14.3590593037066,-326.859835772614)) ;
#41914 = CARTESIAN_POINT('Ctrl Pts',(11.7800085429609,-14.3501201783384,-326.859652385209)) ;
#41915 = CARTESIAN_POINT('Ctrl Pts',(11.7855276071371,-14.3455878034463,-326.859559442508)) ;
#41916 = CARTESIAN_POINT('Ctrl Pts',(11.7967823836165,-14.336334258935,-326.859369766371)) ;
#41917 = CARTESIAN_POINT('Ctrl Pts',(11.8025178801671,-14.3316128289402,-326.859273030844)) ;
#41918 = CARTESIAN_POINT('Ctrl Pts',(11.8142881235422,-14.3219117701261,-326.859074357513)) ;
#41919 = CARTESIAN_POINT('Ctrl Pts',(11.8203225595079,-14.3169317664967,-326.858972416703)) ;
#41920 = CARTESIAN_POINT('Ctrl Pts',(11.8327834897189,-14.3066349592115,-326.858761738745)) ;
#41921 = CARTESIAN_POINT('Ctrl Pts',(11.839209552689,-14.3013176364348,-326.85865299744)) ;
#41922 = CARTESIAN_POINT('Ctrl Pts',(11.8525610819794,-14.2902545875103,-326.858426865741)) ;
#41923 = CARTESIAN_POINT('Ctrl Pts',(11.8594859585686,-14.2845081531149,-326.85830946969)) ;
#41924 = CARTESIAN_POINT('Ctrl Pts',(11.873962138257,-14.2724776774405,-326.858063825591)) ;
#41925 = CARTESIAN_POINT('Ctrl Pts',(11.8815126369119,-14.2661926726326,-326.85793556987)) ;
#41926 = CARTESIAN_POINT('Ctrl Pts',(11.897393025874,-14.2529525485445,-326.857665540604)) ;
#41927 = CARTESIAN_POINT('Ctrl Pts',(11.9057218138867,-14.2459961130658,-326.857523756618)) ;
#41928 = CARTESIAN_POINT('Ctrl Pts',(12.0403021745294,-14.1333903992495,-326.855230131147)) ;
#41929 = CARTESIAN_POINT('Ctrl Pts',(12.1651490286888,-14.0260739208042,-326.853065065705)) ;
#41930 = CARTESIAN_POINT('Ctrl Pts',(12.5064518450368,-13.7247098460763,-326.847044538442)) ;
#41931 = CARTESIAN_POINT('Ctrl Pts',(12.7198026667733,-13.5272176649301,-326.843164512395)) ;
#41932 = CARTESIAN_POINT('Ctrl Pts',(13.1628326807557,-13.0973663741485,-326.834881612142)) ;
#41933 = CARTESIAN_POINT('Ctrl Pts',(13.3911950303763,-12.8637889274182,-326.830474597117)) ;
#41934 = CARTESIAN_POINT('Ctrl Pts',(13.7269862903283,-12.5016923535573,-326.823828835522)) ;
#41935 = CARTESIAN_POINT('Ctrl Pts',(13.8390341276396,-12.3775441339682,-326.821581974367)) ;
#41936 = CARTESIAN_POINT('Ctrl Pts',(14.0543795370975,-12.1323627985403,-326.817216788125)) ;
#41937 = CARTESIAN_POINT('Ctrl Pts',(14.1578288525864,-12.0114817374491,-326.815097712751)) ;
#41938 = CARTESIAN_POINT('Ctrl Pts',(14.3503056822411,-11.7806298485435,-326.811123284633)) ;
#41939 = CARTESIAN_POINT('Ctrl Pts',(14.4396548652993,-11.6709417049327,-326.809264867421)) ;
#41940 = CARTESIAN_POINT('Ctrl Pts',(14.5739290938495,-11.5021994631817,-326.80645799936)) ;
#41941 = CARTESIAN_POINT('Ctrl Pts',(14.6197681828415,-11.4438795879201,-326.805497219165)) ;
#41942 = CARTESIAN_POINT('Ctrl Pts',(14.6922250685337,-11.3505487071763,-326.803975518865)) ;
#41943 = CARTESIAN_POINT('Ctrl Pts',(14.7190700372476,-11.315715207371,-326.803411103947)) ;
#41944 = CARTESIAN_POINT('Ctrl Pts',(14.7465703595737,-11.2797678911374,-326.802832107947)) ;
#41945 = CARTESIAN_POINT('Ctrl Pts',(14.7473496241855,-11.2787490489783,-326.802815700517)) ;
#41946 = CARTESIAN_POINT('Ctrl Pts',(14.7499434648194,-11.2753570281298,-326.802761084904)) ;
#41947 = CARTESIAN_POINT('Ctrl Pts',(14.7517575736512,-11.2729834921988,-326.80272288356)) ;
#41948 = CARTESIAN_POINT('Ctrl Pts',(14.7552181175223,-11.2684535348797,-326.802650004615)) ;
#41949 = CARTESIAN_POINT('Ctrl Pts',(14.7568646529083,-11.266297190255,-326.802615325555)) ;
#41950 = CARTESIAN_POINT('Ctrl Pts',(14.8120457641581,-11.1939977526916,-326.801453005475)) ;
#41951 = CARTESIAN_POINT('Ctrl Pts',(14.8650801360856,-11.1234741867984,-326.800332600198)) ;
#41952 = CARTESIAN_POINT('Ctrl Pts',(15.0667076902149,-10.8513384060217,-326.796055070246)) ;
#41953 = CARTESIAN_POINT('Ctrl Pts',(15.2117186656336,-10.6471048429403,-326.792940333628)) ;
#41954 = CARTESIAN_POINT('Ctrl Pts',(15.6654335182437,-9.97989396203828,-326.782978132254)) ;
#41955 = CARTESIAN_POINT('Ctrl Pts',(15.9574719049475,-9.50595512145185,-326.776216220472)) ;
#41956 = CARTESIAN_POINT('Ctrl Pts',(16.4067733843464,-8.69758742689565,-326.764815534732)) ;
#41957 = CARTESIAN_POINT('Ctrl Pts',(16.5761363768627,-8.37030118178966,-326.760236085769)) ;
#41958 = CARTESIAN_POINT('Ctrl Pts',(16.8046679886038,-7.89449467826937,-326.753577494318)) ;
#41959 = CARTESIAN_POINT('Ctrl Pts',(16.8718333958693,-7.74991291513527,-326.751554341734)) ;
#41960 = CARTESIAN_POINT('Ctrl Pts',(16.9880338624197,-7.49110480250484,-326.747930339098)) ;
#41961 = CARTESIAN_POINT('Ctrl Pts',(17.0377995300502,-7.3772171443979,-326.746334788592)) ;
#41962 = CARTESIAN_POINT('Ctrl Pts',(17.1375013357732,-7.14266054272902,-326.743046238123)) ;
#41963 = CARTESIAN_POINT('Ctrl Pts',(17.1873153957241,-7.02194710112931,-326.741352487818)) ;
#41964 = CARTESIAN_POINT('Ctrl Pts',(17.2512928246325,-6.86215134762048,-326.739108567134)) ;
#41965 = CARTESIAN_POINT('Ctrl Pts',(17.2666043842565,-6.82353268289879,-326.738566132553)) ;
#41966 = CARTESIAN_POINT('Ctrl Pts',(17.3969646713326,-6.49149080947905,-326.733901199319)) ;
#41967 = CARTESIAN_POINT('Ctrl Pts',(17.504653881744,-6.19523401088165,-326.729730585535)) ;
#41968 = CARTESIAN_POINT('Ctrl Pts',(17.7802828379706,-5.37229208113595,-326.718150431057)) ;
#41969 = CARTESIAN_POINT('Ctrl Pts',(17.9323257840963,-4.84062702754272,-326.710668038348)) ;
#41970 = CARTESIAN_POINT('Ctrl Pts',(18.1335910854552,-3.99587740362943,-326.699012057862)) ;
#41971 = CARTESIAN_POINT('Ctrl Pts',(18.1989139221187,-3.68696279482137,-326.694799579853)) ;
#41972 = CARTESIAN_POINT('Ctrl Pts',(18.2739658323541,-3.28117010923824,-326.689388751037)) ;
#41973 = CARTESIAN_POINT('Ctrl Pts',(18.2908558466787,-3.18567056729326,-326.688124258517)) ;
#41974 = CARTESIAN_POINT('Ctrl Pts',(18.318030577803,-3.02467354618739,-326.686009986932)) ;
#41975 = CARTESIAN_POINT('Ctrl Pts',(18.3287141013367,-2.95924546727753,-326.685155683198)) ;
#41976 = CARTESIAN_POINT('Ctrl Pts',(18.3488092341081,-2.83189371192019,-326.683502828001)) ;
#41977 = CARTESIAN_POINT('Ctrl Pts',(18.358258345277,-2.76997704770864,-326.682703671237)) ;
#41978 = CARTESIAN_POINT('Ctrl Pts',(18.3794314212705,-2.62636838494424,-326.68085926728)) ;
#41979 = CARTESIAN_POINT('Ctrl Pts',(18.390924367199,-2.54464363024246,-326.679816501654)) ;
#41980 = CARTESIAN_POINT('Ctrl Pts',(18.4717828128968,-1.94048590755105,-326.672150349244)) ;
#41981 = CARTESIAN_POINT('Ctrl Pts',(18.5194196832725,-1.41539532641382,-326.665715364132)) ;
#41982 = CARTESIAN_POINT('Ctrl Pts',(18.5446545943314,-0.888979965716119,
-326.659259832385)) ;
#41983 = CARTESIAN_POINT('Ctrl Pts',(18.5446545937382,-0.888979978089846,
-326.364137692133)) ;
#41984 = CARTESIAN_POINT('Ctrl Pts',(18.5026962120991,-1.76425694043673,-326.374949702051)) ;
#41985 = CARTESIAN_POINT('Ctrl Pts',(18.3988248501205,-2.63545455372144,-326.385538532625)) ;
#41986 = CARTESIAN_POINT('Ctrl Pts',(18.2084207684801,-3.62851206867422,-326.398258197816)) ;
#41987 = CARTESIAN_POINT('Ctrl Pts',(18.1815835253599,-3.76067908291487,-326.399963143586)) ;
#41988 = CARTESIAN_POINT('Ctrl Pts',(18.128961717625,-4.00608682932487,-326.403153455714)) ;
#41989 = CARTESIAN_POINT('Ctrl Pts',(18.1035499750231,-4.11940079429492,-326.404636346405)) ;
#41990 = CARTESIAN_POINT('Ctrl Pts',(18.0483068395658,-4.35534687042108,-326.407745495943)) ;
#41991 = CARTESIAN_POINT('Ctrl Pts',(18.0182847216749,-4.47792829015448,-326.409372954154)) ;
#41992 = CARTESIAN_POINT('Ctrl Pts',(17.9433558844881,-4.77090422569198,-326.413292452849)) ;
#41993 = CARTESIAN_POINT('Ctrl Pts',(17.8972686136077,-4.94098406780114,-326.415592169263)) ;
#41994 = CARTESIAN_POINT('Ctrl Pts',(17.7373329291751,-5.49958319063575,-326.423224370962)) ;
#41995 = CARTESIAN_POINT('Ctrl Pts',(17.6131984992922,-5.88503457085696,-326.428620443018)) ;
#41996 = CARTESIAN_POINT('Ctrl Pts',(17.309708388988,-6.73148591367984,-326.440692778461)) ;
#41997 = CARTESIAN_POINT('Ctrl Pts',(17.1243324833767,-7.19000303772743,-326.447385220849)) ;
#41998 = CARTESIAN_POINT('Ctrl Pts',(16.8517138762357,-7.79374650243736,-326.456238127008)) ;
#41999 = CARTESIAN_POINT('Ctrl Pts',(16.7804723441072,-7.94597339193071,-326.458473238092)) ;
#42000 = CARTESIAN_POINT('Ctrl Pts',(16.6666552553487,-8.18081494621922,-326.461915464164)) ;
#42001 = CARTESIAN_POINT('Ctrl Pts',(16.625509751875,-8.26411254194308,-326.46313522741)) ;
#42002 = CARTESIAN_POINT('Ctrl Pts',(16.5807153724435,-8.35310854842434,-326.464435810253)) ;
#42003 = CARTESIAN_POINT('Ctrl Pts',(16.5776867415473,-8.35911759594778,-326.464523613226)) ;
#42004 = CARTESIAN_POINT('Ctrl Pts',(16.5722108395581,-8.36996754564659,-326.464682126233)) ;
#42005 = CARTESIAN_POINT('Ctrl Pts',(16.5697647126626,-8.37480902426757,-326.464752849388)) ;
#42006 = CARTESIAN_POINT('Ctrl Pts',(16.565283052362,-8.38366966755605,-326.464882267086)) ;
#42007 = CARTESIAN_POINT('Ctrl Pts',(16.563248177161,-8.38768916456408,-326.464940969271)) ;
#42008 = CARTESIAN_POINT('Ctrl Pts',(16.5594714288274,-8.39514265672645,-326.465049810981)) ;
#42009 = CARTESIAN_POINT('Ctrl Pts',(16.5577299500929,-8.39857685139204,-326.465099955133)) ;
#42010 = CARTESIAN_POINT('Ctrl Pts',(16.5544564280303,-8.40502725870876,-326.465194131407)) ;
#42011 = CARTESIAN_POINT('Ctrl Pts',(16.5529246284303,-8.4080435948383,-326.465238166413)) ;
#42012 = CARTESIAN_POINT('Ctrl Pts',(16.5500087060112,-8.41378158479565,-326.465321927329)) ;
#42013 = CARTESIAN_POINT('Ctrl Pts',(16.5486247360639,-8.41650331614191,-326.465361655061)) ;
#42014 = CARTESIAN_POINT('Ctrl Pts',(16.5459564834907,-8.4217475301289,-326.465438196262)) ;
#42015 = CARTESIAN_POINT('Ctrl Pts',(16.5446722953049,-8.42427006070976,-326.465475010864)) ;
#42016 = CARTESIAN_POINT('Ctrl Pts',(16.5421637659266,-8.42919477846355,-326.465546878501)) ;
#42017 = CARTESIAN_POINT('Ctrl Pts',(16.5409394782403,-8.43159699281256,-326.465581932181)) ;
#42018 = CARTESIAN_POINT('Ctrl Pts',(16.5385146740669,-8.43635221858807,-326.465651316676)) ;
#42019 = CARTESIAN_POINT('Ctrl Pts',(16.5373141785866,-8.43870524068253,-326.465685647746)) ;
#42020 = CARTESIAN_POINT('Ctrl Pts',(16.5349005514442,-8.44343355928576,-326.465754630053)) ;
#42021 = CARTESIAN_POINT('Ctrl Pts',(16.533687409984,-8.44580885085371,-326.465789281171)) ;
#42022 = CARTESIAN_POINT('Ctrl Pts',(16.5017146899841,-8.50837710952026,-326.466701971268)) ;
#42023 = CARTESIAN_POINT('Ctrl Pts',(16.4706270833373,-8.56840196580296,-326.467575970412)) ;
#42024 = CARTESIAN_POINT('Ctrl Pts',(16.4101781619319,-8.68357387096116,-326.469248870667)) ;
#42025 = CARTESIAN_POINT('Ctrl Pts',(16.3808649389626,-8.73874512399434,-326.470048445458)) ;
#42026 = CARTESIAN_POINT('Ctrl Pts',(16.296372807625,-8.89585116376364,-326.47232155885)) ;
#42027 = CARTESIAN_POINT('Ctrl Pts',(16.2405169806811,-8.99741867849112,-326.473786568648)) ;
#42028 = CARTESIAN_POINT('Ctrl Pts',(15.9975510284008,-9.42958993405747,-326.480013466453)) ;
#42029 = CARTESIAN_POINT('Ctrl Pts',(15.8012688538205,-9.75493255524212,-326.484685869259)) ;
#42030 = CARTESIAN_POINT('Ctrl Pts',(15.3341720318717,-10.4780241237083,-326.495240181844)) ;
#42031 = CARTESIAN_POINT('Ctrl Pts',(15.0575995565262,-10.8717301703389,-326.501111465497)) ;
#42032 = CARTESIAN_POINT('Ctrl Pts',(14.6367784555695,-11.4238652213471,-326.509713084837)) ;
#42033 = CARTESIAN_POINT('Ctrl Pts',(14.5045911362948,-11.59123875736,-326.512371249507)) ;
#42034 = CARTESIAN_POINT('Ctrl Pts',(14.2614378024571,-11.8884415061596,-326.517195995861)) ;
#42035 = CARTESIAN_POINT('Ctrl Pts',(14.1515081331023,-12.019087614111,-326.519354620518)) ;
#42036 = CARTESIAN_POINT('Ctrl Pts',(13.9687765969683,-12.2302722403605,-326.522910025976)) ;
#42037 = CARTESIAN_POINT('Ctrl Pts',(13.897042669628,-12.3117213944365,-326.524297759316)) ;
#42038 = CARTESIAN_POINT('Ctrl Pts',(13.7401835510086,-12.486706904515,-326.527315879451)) ;
#42039 = CARTESIAN_POINT('Ctrl Pts',(13.6548084335803,-12.5800119206167,-326.528948397727)) ;
#42040 = CARTESIAN_POINT('Ctrl Pts',(13.4621564747937,-12.7862860172731,-326.532610243105)) ;
#42041 = CARTESIAN_POINT('Ctrl Pts',(13.3543976250305,-12.8987918442656,-326.53464371311)) ;
#42042 = CARTESIAN_POINT('Ctrl Pts',(12.7490140392894,-13.5151248703991,-326.545985127595)) ;
#42043 = CARTESIAN_POINT('Ctrl Pts',(12.2242964354032,-13.9915162817371,-326.555537600353)) ;
#42044 = CARTESIAN_POINT('Ctrl Pts',(11.4527875671398,-14.6153630220403,-326.568893310128)) ;
#42045 = CARTESIAN_POINT('Ctrl Pts',(11.2278484966696,-14.7888673594368,-326.572708144822)) ;
#42046 = CARTESIAN_POINT('Ctrl Pts',(10.8548365340942,-15.0631687530199,-326.578860392525)) ;
#42047 = CARTESIAN_POINT('Ctrl Pts',(10.7091298846897,-15.1671047458488,-326.581221826115)) ;
#42048 = CARTESIAN_POINT('Ctrl Pts',(10.4956586715981,-15.3147688324228,-326.584608868726)) ;
#42049 = CARTESIAN_POINT('Ctrl Pts',(10.4290762321194,-15.3601876391559,-326.585655229476)) ;
#42050 = CARTESIAN_POINT('Ctrl Pts',(10.3071154311353,-15.4422238713289,-326.58755200359)) ;
#42051 = CARTESIAN_POINT('Ctrl Pts',(10.2518325376521,-15.4789804643998,-326.588404257032)) ;
#42052 = CARTESIAN_POINT('Ctrl Pts',(10.1146168702492,-15.5691551216043,-326.590501884071)) ;
#42053 = CARTESIAN_POINT('Ctrl Pts',(10.0324568471083,-15.6222237624314,-326.591742541342)) ;
#42054 = CARTESIAN_POINT('Ctrl Pts',(9.67087666360603,-15.8517460809997,-326.59714376199)) ;
#42055 = CARTESIAN_POINT('Ctrl Pts',(9.38719244648079,-16.0213709846403,-326.601229792122)) ;
#42056 = CARTESIAN_POINT('Ctrl Pts',(8.62781128111609,-16.4483355053427,-326.611937772282)) ;
#42057 = CARTESIAN_POINT('Ctrl Pts',(8.14513905944076,-16.6926204848564,-326.618519881164)) ;
#42058 = CARTESIAN_POINT('Ctrl Pts',(7.51214651626492,-16.9789835706538,-326.627116045082)) ;
#42059 = CARTESIAN_POINT('Ctrl Pts',(7.37101364914425,-17.0407272758858,-326.62902978514)) ;
#42060 = CARTESIAN_POINT('Ctrl Pts',(7.0231418137628,-17.1877861238651,-326.633746779964)) ;
#42061 = CARTESIAN_POINT('Ctrl Pts',(6.81559850700049,-17.2711357330323,-326.636561044861)) ;
#42062 = CARTESIAN_POINT('Ctrl Pts',(6.48121165108943,-17.3984596098192,-326.641104776613)) ;
#42063 = CARTESIAN_POINT('Ctrl Pts',(6.3553090705216,-17.4448430149358,-326.642817627475)) ;
#42064 = CARTESIAN_POINT('Ctrl Pts',(6.1106503911945,-17.5319768345413,-326.646151410397)) ;
#42065 = CARTESIAN_POINT('Ctrl Pts',(5.99196181511737,-17.5728954211767,-326.647771078563)) ;
#42066 = CARTESIAN_POINT('Ctrl Pts',(5.72918665287508,-17.6605169583859,-326.651362753569)) ;
#42067 = CARTESIAN_POINT('Ctrl Pts',(5.58492510840863,-17.7066668343848,-326.653338352609)) ;
#42068 = CARTESIAN_POINT('Ctrl Pts',(4.9892194111868,-17.8892311497806,-326.66151084462)) ;
#42069 = CARTESIAN_POINT('Ctrl Pts',(4.53322359772509,-18.0101855339538,-326.66780567846)) ;
#42070 = CARTESIAN_POINT('Ctrl Pts',(3.82116789865146,-18.1703017263502,-326.677617122839)) ;
#42071 = CARTESIAN_POINT('Ctrl Pts',(3.56806143119564,-18.2216938428152,-326.681100049528)) ;
#42072 = CARTESIAN_POINT('Ctrl Pts',(3.04089049258729,-18.3173280946925,-326.688310880042)) ;
#42073 = CARTESIAN_POINT('Ctrl Pts',(2.76673857958043,-18.3607374976121,-326.692036801902)) ;
#42074 = CARTESIAN_POINT('Ctrl Pts',(2.31690557091818,-18.4216602786168,-326.698066771517)) ;
#42075 = CARTESIAN_POINT('Ctrl Pts',(2.14176562914686,-18.4428430298319,-326.700393780918)) ;
#42076 = CARTESIAN_POINT('Ctrl Pts',(1.88660611214707,-18.4700202503915,-326.703741676239)) ;
#42077 = CARTESIAN_POINT('Ctrl Pts',(1.80680769534469,-18.477997095145,-326.704782679929)) ;
#42078 = CARTESIAN_POINT('Ctrl Pts',(1.66077834452336,-18.4916395416229,-326.706675129455)) ;
#42079 = CARTESIAN_POINT('Ctrl Pts',(1.59456405899212,-18.4974669374542,-326.707528344996)) ;
#42080 = CARTESIAN_POINT('Ctrl Pts',(1.43014041887756,-18.5110481265793,-326.70963581415)) ;
#42081 = CARTESIAN_POINT('Ctrl Pts',(1.33189791211798,-18.5183760722902,-326.710885237192)) ;
#42082 = CARTESIAN_POINT('Ctrl Pts',(0.887849653158683,-18.5479458957626,
-326.716496754199)) ;
#42083 = CARTESIAN_POINT('Ctrl Pts',(0.541519906217356,-18.5612858197278,
-326.720776662602)) ;
#42084 = CARTESIAN_POINT('Ctrl Pts',(-0.333091452918507,-18.5704733806766,
-326.731520456152)) ;
#42085 = CARTESIAN_POINT('Ctrl Pts',(-0.861198435910072,-18.5534840155664,
-326.737953188577)) ;
#42086 = CARTESIAN_POINT('Ctrl Pts',(-1.60943875228085,-18.4973938370672,
-326.747239588024)) ;
#42087 = CARTESIAN_POINT('Ctrl Pts',(-1.83069987676984,-18.4768073435676,
-326.750006020787)) ;
#42088 = CARTESIAN_POINT('Ctrl Pts',(-2.23688642803872,-18.4316471665521,
-326.755136618579)) ;
#42089 = CARTESIAN_POINT('Ctrl Pts',(-2.42191376619061,-18.4082484695159,
-326.757493638808)) ;
#42090 = CARTESIAN_POINT('Ctrl Pts',(-2.73306140678452,-18.3641280738278,
-326.761495834665)) ;
#42091 = CARTESIAN_POINT('Ctrl Pts',(-2.85937722285068,-18.344884475177,-326.763131325918)) ;
#42092 = CARTESIAN_POINT('Ctrl Pts',(-3.11651859208449,-18.3029898389316,
-326.766483647797)) ;
#42093 = CARTESIAN_POINT('Ctrl Pts',(-3.24732008033496,-18.2802362515444,
-326.768201065447)) ;
#42094 = CARTESIAN_POINT('Ctrl Pts',(-3.58989884209959,-18.2168499665864,
-326.772731545598)) ;
#42095 = CARTESIAN_POINT('Ctrl Pts',(-3.80123163847965,-18.1739273185073,
-326.775559164704)) ;
#42096 = CARTESIAN_POINT('Ctrl Pts',(-4.29407840478718,-18.0648551749294,
-326.782226721592)) ;
#42097 = CARTESIAN_POINT('Ctrl Pts',(-4.57488985058449,-17.9957907359514,
-326.786082570072)) ;
#42098 = CARTESIAN_POINT('Ctrl Pts',(-5.35702463897054,-17.7839369634897,
-326.79694886986)) ;
#42099 = CARTESIAN_POINT('Ctrl Pts',(-5.85411482890597,-17.6265556957852,
-326.804008011476)) ;
#42100 = CARTESIAN_POINT('Ctrl Pts',(-6.57716100012093,-17.3636702188845,
-326.814294057897)) ;
#42101 = CARTESIAN_POINT('Ctrl Pts',(-6.80867522810172,-17.2742013523003,
-326.817589055323)) ;
#42102 = CARTESIAN_POINT('Ctrl Pts',(-7.12125133463936,-17.146145616605,-326.822009364928)) ;
#42103 = CARTESIAN_POINT('Ctrl Pts',(-7.20392927243562,-17.1115730763335,
-326.823175777074)) ;
#42104 = CARTESIAN_POINT('Ctrl Pts',(-7.34684338374057,-17.0505928598623,
-326.825185104049)) ;
#42105 = CARTESIAN_POINT('Ctrl Pts',(-7.40719534712128,-17.0244612744748,
-326.82603136068)) ;
#42106 = CARTESIAN_POINT('Ctrl Pts',(-7.54526879173654,-16.9638041328658,
-326.827962184028)) ;
#42107 = CARTESIAN_POINT('Ctrl Pts',(-7.62289428577533,-16.9290641954369,
-326.829044106759)) ;
#42108 = CARTESIAN_POINT('Ctrl Pts',(-7.87580453842161,-16.8137863853595,
-326.832561264233)) ;
#42109 = CARTESIAN_POINT('Ctrl Pts',(-8.05007343311089,-16.731049808631,-326.83497250127)) ;
#42110 = CARTESIAN_POINT('Ctrl Pts',(-8.82008018878329,-16.3506623567819,
-326.845629698817)) ;
#42111 = CARTESIAN_POINT('Ctrl Pts',(-9.40083792657956,-16.0238018113441,
-326.853694057912)) ;
#42112 = CARTESIAN_POINT('Ctrl Pts',(-10.105358910533,-15.5757751482347,-326.864003435448)) ;
#42113 = CARTESIAN_POINT('Ctrl Pts',(-10.2466955456567,-15.4831611917713,
-326.866098384733)) ;
#42114 = CARTESIAN_POINT('Ctrl Pts',(-10.5838325823997,-15.255606349652,-326.871169956836)) ;
#42115 = CARTESIAN_POINT('Ctrl Pts',(-10.778343027701,-15.1188081045015,-326.8741579211)) ;
#42116 = CARTESIAN_POINT('Ctrl Pts',(-11.0804064847131,-14.8975756927966,
-326.87890846046)) ;
#42117 = CARTESIAN_POINT('Ctrl Pts',(-11.1897462746621,-14.8156251178051,
-326.880651442179)) ;
#42118 = CARTESIAN_POINT('Ctrl Pts',(-11.398079710107,-14.6558565226824,-326.884019278324)) ;
#42119 = CARTESIAN_POINT('Ctrl Pts',(-11.4972059978724,-14.5782236805645,
-326.885642564963)) ;
#42120 = CARTESIAN_POINT('Ctrl Pts',(-11.7314942634099,-14.3908598995086,
-326.889529925693)) ;
#42121 = CARTESIAN_POINT('Ctrl Pts',(-11.8659174741564,-14.2802243910504,
-326.891801338814)) ;
#42122 = CARTESIAN_POINT('Ctrl Pts',(-12.5338390519738,-13.7145556238068,
-326.903294233929)) ;
#42123 = CARTESIAN_POINT('Ctrl Pts',(-13.0428104244999,-13.2314491202778,
-326.91275138245)) ;
#42124 = CARTESIAN_POINT('Ctrl Pts',(-13.7196024215848,-12.5119602908376,
-326.926048790745)) ;
#42125 = CARTESIAN_POINT('Ctrl Pts',(-13.9111127046318,-12.2986822287112,
-326.929898613203)) ;
#42126 = CARTESIAN_POINT('Ctrl Pts',(-14.2147134096491,-11.94440493153,-326.936098814283)) ;
#42127 = CARTESIAN_POINT('Ctrl Pts',(-14.3298250477942,-11.8060578002989,
-326.938473634115)) ;
#42128 = CARTESIAN_POINT('Ctrl Pts',(-14.4936486020641,-11.6032396571846,
-326.941875877965)) ;
#42129 = CARTESIAN_POINT('Ctrl Pts',(-14.5439796222735,-11.5400899958964,
-326.9429243025)) ;
#42130 = CARTESIAN_POINT('Ctrl Pts',(-14.6349155734363,-11.4244539798501,
-326.944822764228)) ;
#42131 = CARTESIAN_POINT('Ctrl Pts',(-14.6756540450582,-11.3720746094886,
-326.945674668497)) ;
#42132 = CARTESIAN_POINT('Ctrl Pts',(-14.7755808518664,-11.2421627898323,
-326.947768605728)) ;
#42133 = CARTESIAN_POINT('Ctrl Pts',(-14.8344406618585,-11.1643801436847,
-326.949005965313)) ;
#42134 = CARTESIAN_POINT('Ctrl Pts',(-15.0972407780093,-10.8113447057897,
-326.95455682066)) ;
#42135 = CARTESIAN_POINT('Ctrl Pts',(-15.2941525851511,-10.530942562824,-326.958789604085)) ;
#42136 = CARTESIAN_POINT('Ctrl Pts',(-15.8466543919673,-9.69597122318395,
-326.971090584124)) ;
#42137 = CARTESIAN_POINT('Ctrl Pts',(-16.1806276098271,-9.12773818663991,
-326.979100068229)) ;
#42138 = CARTESIAN_POINT('Ctrl Pts',(-16.5930126794276,-8.33203864512454,
-326.990274897359)) ;
#42139 = CARTESIAN_POINT('Ctrl Pts',(-16.698268692159,-8.11903689758766,-326.993260292732)) ;
#42140 = CARTESIAN_POINT('Ctrl Pts',(-16.8575634849551,-7.7804699637858,-326.998007775332)) ;
#42141 = CARTESIAN_POINT('Ctrl Pts',(-16.9143530068844,-7.65622764805146,
-326.999750314675)) ;
#42142 = CARTESIAN_POINT('Ctrl Pts',(-17.0208454958791,-7.41627759587268,
-327.003117885688)) ;
#42143 = CARTESIAN_POINT('Ctrl Pts',(-17.0707525642146,-7.30066857292239,
-327.004741356466)) ;
#42144 = CARTESIAN_POINT('Ctrl Pts',(-17.1868844039221,-7.02394788102239,
-327.008630155542)) ;
#42145 = CARTESIAN_POINT('Ctrl Pts',(-17.2520254418457,-6.86239443382043,
-327.010902837924)) ;
#42146 = CARTESIAN_POINT('Ctrl Pts',(-17.5677373359511,-6.04649045394342,
-327.022390462494)) ;
#42147 = CARTESIAN_POINT('Ctrl Pts',(-17.7833957758326,-5.37924426551951,
-327.031840621406)) ;
#42148 = CARTESIAN_POINT('Ctrl Pts',(-18.0334467181512,-4.42397398597466,
-327.045133693862)) ;
#42149 = CARTESIAN_POINT('Ctrl Pts',(-18.0996311539107,-4.14488827056821,
-327.048986028345)) ;
#42150 = CARTESIAN_POINT('Ctrl Pts',(-18.1967973663554,-3.6882892700022,-327.055189668817)) ;
#42151 = CARTESIAN_POINT('Ctrl Pts',(-18.2317072643957,-3.51166093957875,
-327.057565446302)) ;
#42152 = CARTESIAN_POINT('Ctrl Pts',(-18.2785483351576,-3.25510259237579,
-327.060968777187)) ;
#42153 = CARTESIAN_POINT('Ctrl Pts',(-18.2925353483904,-3.17555864058567,
-327.062017348951)) ;
#42154 = CARTESIAN_POINT('Ctrl Pts',(-18.3170676758039,-3.03050062812811,
-327.06391593152)) ;
#42155 = CARTESIAN_POINT('Ctrl Pts',(-18.327781604383,-2.96501665321094,-327.064767811325)) ;
#42156 = CARTESIAN_POINT('Ctrl Pts',(-18.3533745148706,-2.80315071780301,
-327.06686148744)) ;
#42157 = CARTESIAN_POINT('Ctrl Pts',(-18.3678455800112,-2.70670626748359,
-327.068098613414)) ;
#42158 = CARTESIAN_POINT('Ctrl Pts',(-18.4266432688807,-2.29263347197853,
-327.073373475872)) ;
#42159 = CARTESIAN_POINT('Ctrl Pts',(-18.4634958561383,-1.97399900787125,
-327.077341255139)) ;
#42160 = CARTESIAN_POINT('Ctrl Pts',(-18.5030135767353,-1.5323345106877,-327.082793833516)) ;
#42161 = CARTESIAN_POINT('Ctrl Pts',(-18.5127382627211,-1.40999379632923,
-327.084299084285)) ;
#42162 = CARTESIAN_POINT('Ctrl Pts',(-18.5533492189315,-0.825817260896462,
-327.091475289535)) ;
#42163 = CARTESIAN_POINT('Ctrl Pts',(-18.5681703565681,-0.363029938491348,
-327.097130875431)) ;
#42164 = CARTESIAN_POINT('Ctrl Pts',(-18.5640843027216,0.396896815357878,
-327.106551427455)) ;
#42165 = CARTESIAN_POINT('Ctrl Pts',(-18.5553570354474,0.693886034294105,
-327.110265519233)) ;
#42166 = CARTESIAN_POINT('Ctrl Pts',(-18.5317084776999,1.13650706957426,-327.115873980792)) ;
#42167 = CARTESIAN_POINT('Ctrl Pts',(-18.5221858862663,1.28237956002616,-327.117734058904)) ;
#42168 = CARTESIAN_POINT('Ctrl Pts',(-18.5013960050624,1.55185211176864,-327.121193869744)) ;
#42169 = CARTESIAN_POINT('Ctrl Pts',(-18.4906101098028,1.67548107396545,-327.122790386258)) ;
#42170 = CARTESIAN_POINT('Ctrl Pts',(-18.4634203347717,1.95476438800068,-327.126418548748)) ;
#42171 = CARTESIAN_POINT('Ctrl Pts',(-18.4462860008254,2.11033811174323,-327.128454808903)) ;
#42172 = CARTESIAN_POINT('Ctrl Pts',(-18.3832618999616,2.62292537810659,-327.135213831997)) ;
#42173 = CARTESIAN_POINT('Ctrl Pts',(-18.3289574902738,2.97882054939017,-327.139988317052)) ;
#42174 = CARTESIAN_POINT('Ctrl Pts',(-18.1620591775996,3.89342281347032,-327.15242546214)) ;
#42175 = CARTESIAN_POINT('Ctrl Pts',(-18.034028215192,4.44892790261231,-327.160149022747)) ;
#42176 = CARTESIAN_POINT('Ctrl Pts',(-17.8326523521079,5.16941109731806,-327.170157496103)) ;
#42177 = CARTESIAN_POINT('Ctrl Pts',(-17.7821766148177,5.34045840603847,-327.172531939782)) ;
#42178 = CARTESIAN_POINT('Ctrl Pts',(-17.6902536574805,5.63619382684467,-327.176620549269)) ;
#42179 = CARTESIAN_POINT('Ctrl Pts',(-17.6499325210346,5.76121839637051,-327.178343767465)) ;
#42180 = CARTESIAN_POINT('Ctrl Pts',(-17.5853805816548,5.9543354302579,-327.180991748596)) ;
#42181 = CARTESIAN_POINT('Ctrl Pts',(-17.5620733474982,6.02273196921081,-327.18192688721)) ;
#42182 = CARTESIAN_POINT('Ctrl Pts',(-17.5181663749925,6.14915747970571,-327.183649224433)) ;
#42183 = CARTESIAN_POINT('Ctrl Pts',(-17.4976761029815,6.20722336074041,-327.184437803244)) ;
#42184 = CARTESIAN_POINT('Ctrl Pts',(-17.4396190547559,6.36917498239749,-327.186631602611)) ;
#42185 = CARTESIAN_POINT('Ctrl Pts',(-17.4014133526989,6.47282906581619,-327.188029224547)) ;
#42186 = CARTESIAN_POINT('Ctrl Pts',(-17.1330418640408,7.18138225824297,-327.197556223597)) ;
#42187 = CARTESIAN_POINT('Ctrl Pts',(-16.8723068090042,7.77422948273606,-327.205409134126)) ;
#42188 = CARTESIAN_POINT('Ctrl Pts',(-16.414745052828,8.68259534562688,-327.217892846295)) ;
#42189 = CARTESIAN_POINT('Ctrl Pts',(-16.2385086945559,9.00789386068396,-327.222456063144)) ;
#42190 = CARTESIAN_POINT('Ctrl Pts',(-15.9450883743921,9.51286031466355,-327.229758971463)) ;
#42191 = CARTESIAN_POINT('Ctrl Pts',(-15.8343081786906,9.69613525615551,-327.232456441772)) ;
#42192 = CARTESIAN_POINT('Ctrl Pts',(-15.6498904154397,9.98964390931654,-327.236861137074)) ;
#42193 = CARTESIAN_POINT('Ctrl Pts',(-15.5781992798387,10.1010772983335,-327.238553637698)) ;
#42194 = CARTESIAN_POINT('Ctrl Pts',(-15.4357616099646,10.317352218216,-327.241879561534)) ;
#42195 = CARTESIAN_POINT('Ctrl Pts',(-15.3651243927596,10.422257222664,-327.243512076517)) ;
#42196 = CARTESIAN_POINT('Ctrl Pts',(-15.205097691635,10.6547534424509,-327.247173904312)) ;
#42197 = CARTESIAN_POINT('Ctrl Pts',(-15.1151630069123,10.78195779568,-327.24920735989)) ;
#42198 = CARTESIAN_POINT('Ctrl Pts',(-14.6075830372634,11.4810490383051,-327.260548850363)) ;
#42199 = CARTESIAN_POINT('Ctrl Pts',(-14.1590846361893,12.029808121566,-327.270101419741)) ;
#42200 = CARTESIAN_POINT('Ctrl Pts',(-13.4883170949134,12.7608965101675,-327.283457187197)) ;
#42201 = CARTESIAN_POINT('Ctrl Pts',(-13.2915129389356,12.9657572823715,-327.287271985153)) ;
#42202 = CARTESIAN_POINT('Ctrl Pts',(-12.9631718759001,13.2922046179026,-327.293424182454)) ;
#42203 = CARTESIAN_POINT('Ctrl Pts',(-12.8344393436325,13.4165455918345,-327.295785601942)) ;
#42204 = CARTESIAN_POINT('Ctrl Pts',(-12.6451545137902,13.5941554587708,-327.299172628531)) ;
#42205 = CARTESIAN_POINT('Ctrl Pts',(-12.5860213624277,13.6489216278637,-327.300218987101)) ;
#42206 = CARTESIAN_POINT('Ctrl Pts',(-12.4775341519483,13.7480925256658,-327.302115759438)) ;
#42207 = CARTESIAN_POINT('Ctrl Pts',(-12.4282950909574,13.7926207710403,-327.302968013255)) ;
#42208 = CARTESIAN_POINT('Ctrl Pts',(-12.3059240241778,13.9020969497038,-327.305065644221)) ;
#42209 = CARTESIAN_POINT('Ctrl Pts',(-12.2325155889292,13.9667329069638,-327.306306304998)) ;
#42210 = CARTESIAN_POINT('Ctrl Pts',(-11.9088512763747,14.247209345247,-327.311707597338)) ;
#42211 = CARTESIAN_POINT('Ctrl Pts',(-11.6533681354822,14.4569265386785,-327.315793693139)) ;
#42212 = CARTESIAN_POINT('Ctrl Pts',(-11.3160158334268,14.7190913095114,-327.321045077913)) ;
#42213 = CARTESIAN_POINT('Ctrl Pts',(-11.2391450643087,14.7778713471007,-327.322232242831)) ;
#42214 = CARTESIAN_POINT('Ctrl Pts',(-10.7836140355556,15.1205875912917,-327.32921989856)) ;
#42215 = CARTESIAN_POINT('Ctrl Pts',(-10.3946676928102,15.3905615276053,-327.334999765208)) ;
#42216 = CARTESIAN_POINT('Ctrl Pts',(-9.74255522591668,15.8071961913074,-327.344589915789)) ;
#42217 = CARTESIAN_POINT('Ctrl Pts',(-9.48538686340759,15.962840262847,-327.348346524811)) ;
#42218 = CARTESIAN_POINT('Ctrl Pts',(-9.09725479145342,16.185053954308,-327.354004734061)) ;
#42219 = CARTESIAN_POINT('Ctrl Pts',(-8.96909631280644,16.2564241915321,-327.355871064678)) ;
#42220 = CARTESIAN_POINT('Ctrl Pts',(-8.73100961321056,16.3853398486178,-327.359336627715)) ;
#42221 = CARTESIAN_POINT('Ctrl Pts',(-8.62132429740078,16.4433165185368,-327.360932561846)) ;
#42222 = CARTESIAN_POINT('Ctrl Pts',(-8.37255369134558,16.5716364457552,-327.364551483376)) ;
#42223 = CARTESIAN_POINT('Ctrl Pts',(-8.23314714668496,16.6413364176688,-327.36657898461)) ;
#42224 = CARTESIAN_POINT('Ctrl Pts',(-7.77101354237626,16.8651637331876,-327.373298307512)) ;
#42225 = CARTESIAN_POINT('Ctrl Pts',(-7.4447110436268,17.011721713048,-327.37804117831)) ;
#42226 = CARTESIAN_POINT('Ctrl Pts',(-6.4915130660272,17.4071678944539,-327.39184386748)) ;
#42227 = CARTESIAN_POINT('Ctrl Pts',(-5.85503157798774,17.63144458984,-327.401011812333)) ;
#42228 = CARTESIAN_POINT('Ctrl Pts',(-5.03320326071529,17.8716098370464,-327.412392217371)) ;
#42229 = CARTESIAN_POINT('Ctrl Pts',(-4.85790180804087,17.9200547838885,-327.414792555504)) ;
#42230 = CARTESIAN_POINT('Ctrl Pts',(-4.60349059050028,17.9863543319882,-327.418223744202)) ;
#42231 = CARTESIAN_POINT('Ctrl Pts',(-4.52493135780387,18.0062784607028,-327.419276073064)) ;
#42232 = CARTESIAN_POINT('Ctrl Pts',(-4.3818718642458,18.0415657378047,-327.421177759206)) ;
#42233 = CARTESIAN_POINT('Ctrl Pts',(-4.31741515098008,18.0570989285555,-327.422029034469)) ;
#42234 = CARTESIAN_POINT('Ctrl Pts',(-4.15840922618506,18.094517135811,-327.424116140612)) ;
#42235 = CARTESIAN_POINT('Ctrl Pts',(-4.06376897908579,18.1160067176638,-327.425347377813)) ;
#42236 = CARTESIAN_POINT('Ctrl Pts',(-3.64925344153182,18.2067174105727,-327.430699812288)) ;
#42237 = CARTESIAN_POINT('Ctrl Pts',(-3.32774746855397,18.2682157669594,-327.434747644332)) ;
#42238 = CARTESIAN_POINT('Ctrl Pts',(-2.94221135230492,18.3314459983211,-327.439550610788)) ;
#42239 = CARTESIAN_POINT('Ctrl Pts',(-2.87958670530254,18.341387636713,-327.44032914674)) ;
#42240 = CARTESIAN_POINT('Ctrl Pts',(-2.32333073306962,18.4267739161208,-327.447233298347)) ;
#42241 = CARTESIAN_POINT('Ctrl Pts',(-1.82689297607741,18.482595183797,-327.453323740944)) ;
#42242 = CARTESIAN_POINT('Ctrl Pts',(-1.18129924394719,18.528920723854,-327.461339653355)) ;
#42243 = CARTESIAN_POINT('Ctrl Pts',(-1.0336666203417,18.5377426983824,-327.463178642747)) ;
#42244 = CARTESIAN_POINT('Ctrl Pts',(-0.668600962928266,18.5551830542013,
-327.467746756184)) ;
#42245 = CARTESIAN_POINT('Ctrl Pts',(-0.451092023478368,18.5617445615631,
-327.47048669689)) ;
#42246 = CARTESIAN_POINT('Ctrl Pts',(-0.100421704298765,18.5661555636103,
-327.474941933505)) ;
#42247 = CARTESIAN_POINT('Ctrl Pts',(0.0326889975123691,18.5663983663657,
-327.476641827251)) ;
#42248 = CARTESIAN_POINT('Ctrl Pts',(0.291888208747056,18.5640836707535,-327.479970235944)) ;
#42249 = CARTESIAN_POINT('Ctrl Pts',(0.417970888513894,18.5616729187842,-327.481597709921)) ;
#42250 = CARTESIAN_POINT('Ctrl Pts',(0.698066611530982,18.5534620337248,-327.485232405255)) ;
#42251 = CARTESIAN_POINT('Ctrl Pts',(0.852051747604905,18.5470282836666,-327.487243556183)) ;
#42252 = CARTESIAN_POINT('Ctrl Pts',(1.73037390432249,18.4993690987665,-327.498787336571)) ;
#42253 = CARTESIAN_POINT('Ctrl Pts',(2.45188011015524,18.417630848513,-327.508579452566)) ;
#42254 = CARTESIAN_POINT('Ctrl Pts',(3.43850796223524,18.246841682233,-327.522054971141)) ;
#42255 = CARTESIAN_POINT('Ctrl Pts',(3.70919064984514,18.1937481957733,-327.525757320784)) ;
#42256 = CARTESIAN_POINT('Ctrl Pts',(4.15022834907698,18.0969881956845,-327.53175477119)) ;
#42257 = CARTESIAN_POINT('Ctrl Pts',(4.32132374179857,18.0568972530956,-327.534072555319)) ;
#42258 = CARTESIAN_POINT('Ctrl Pts',(4.56953163687006,17.9950074706845,-327.537409945969)) ;
#42259 = CARTESIAN_POINT('Ctrl Pts',(4.64711278089576,17.9751288194487,-327.538449501795)) ;
#42260 = CARTESIAN_POINT('Ctrl Pts',(4.78886740905989,17.937827898694,-327.540340796771)) ;
#42261 = CARTESIAN_POINT('Ctrl Pts',(4.85308038608426,17.9205616972291,-327.541194286532)) ;
#42262 = CARTESIAN_POINT('Ctrl Pts',(5.01238333547499,17.8768077733177,-327.543304483155)) ;
#42263 = CARTESIAN_POINT('Ctrl Pts',(5.1073574751163,17.8499059529265,-327.544556327861)) ;
#42264 = CARTESIAN_POINT('Ctrl Pts',(5.5229852149516,17.7285889158883,-327.550015502966)) ;
#42265 = CARTESIAN_POINT('Ctrl Pts',(5.84127073784943,17.6262811682561,-327.554146905572)) ;
#42266 = CARTESIAN_POINT('Ctrl Pts',(6.21423960057419,17.4951837852178,-327.559005076501)) ;
#42267 = CARTESIAN_POINT('Ctrl Pts',(6.2717580172002,17.4746468023733,-327.559754739108)) ;
#42268 = CARTESIAN_POINT('Ctrl Pts',(6.79328737485886,17.2855278087406,-327.566559205747)) ;
#42269 = CARTESIAN_POINT('Ctrl Pts',(7.2505034418735,17.0987843074423,-327.572582062372)) ;
#42270 = CARTESIAN_POINT('Ctrl Pts',(7.97917523155449,16.7666803996104,-327.582500772623)) ;
#42271 = CARTESIAN_POINT('Ctrl Pts',(8.25541536673911,16.6324058853837,-327.586337238701)) ;
#42272 = CARTESIAN_POINT('Ctrl Pts',(8.65932541936638,16.4235311542488,-327.592088721186)) ;
#42273 = CARTESIAN_POINT('Ctrl Pts',(8.7896400763428,16.3541590899349,-327.59396659497)) ;
#42274 = CARTESIAN_POINT('Ctrl Pts',(9.02787781480226,16.2236648296563,-327.597442929561)) ;
#42275 = CARTESIAN_POINT('Ctrl Pts',(9.1360425072938,16.1630011321562,-327.599037941398)) ;
#42276 = CARTESIAN_POINT('Ctrl Pts',(9.37775044366371,16.0242387259504,-327.602640619275)) ;
#42277 = CARTESIAN_POINT('Ctrl Pts',(9.51094167171217,15.9455454139893,-327.604652621432)) ;
#42278 = CARTESIAN_POINT('Ctrl Pts',(9.92438533091768,15.6942473979743,-327.610982267279)) ;
#42279 = CARTESIAN_POINT('Ctrl Pts',(10.2010407735134,15.5158496992859,-327.61534141355)) ;
#42280 = CARTESIAN_POINT('Ctrl Pts',(10.6465809743406,15.2114793249099,-327.622547823724)) ;
#42281 = CARTESIAN_POINT('Ctrl Pts',(10.8183237480652,15.0898197753552,-327.625372646545)) ;
#42282 = CARTESIAN_POINT('Ctrl Pts',(11.3376586949367,14.708508028158,-327.634040386302)) ;
#42283 = CARTESIAN_POINT('Ctrl Pts',(11.6782493725886,14.439570795678,-327.639904276368)) ;
#42284 = CARTESIAN_POINT('Ctrl Pts',(12.1825226967449,14.0118645377211,-327.648730915036)) ;
#42285 = CARTESIAN_POINT('Ctrl Pts',(12.3532230572227,13.8616047963072,-327.651744912699)) ;
#42286 = CARTESIAN_POINT('Ctrl Pts',(12.5855486714897,13.6493984568164,-327.655859633654)) ;
#42287 = CARTESIAN_POINT('Ctrl Pts',(12.6495613593273,13.5900960644816,-327.656994698044)) ;
#42288 = CARTESIAN_POINT('Ctrl Pts',(12.7563363115265,13.4897699886671,-327.658888432341)) ;
#42289 = CARTESIAN_POINT('Ctrl Pts',(12.7993244058282,13.4489890031938,-327.659650881673)) ;
#42290 = CARTESIAN_POINT('Ctrl Pts',(12.9031332530454,13.3495614185935,-327.661492099007)) ;
#42291 = CARTESIAN_POINT('Ctrl Pts',(12.9637502358049,13.2907041824549,-327.66256748137)) ;
#42292 = CARTESIAN_POINT('Ctrl Pts',(13.1588941240561,13.0986201928476,-327.666034089572)) ;
#42293 = CARTESIAN_POINT('Ctrl Pts',(13.2917855787146,12.9637487588066,-327.668402144939)) ;
#42294 = CARTESIAN_POINT('Ctrl Pts',(13.9816952881079,12.2417973267069,-327.680800581413)) ;
#42295 = CARTESIAN_POINT('Ctrl Pts',(14.5019485357546,11.6207960967083,-327.690558961953)) ;
#42296 = CARTESIAN_POINT('Ctrl Pts',(15.1321367858446,10.7600761107374,-327.703831788143)) ;
#42297 = CARTESIAN_POINT('Ctrl Pts',(15.2799114300906,10.5491756989865,-327.707061586475)) ;
#42298 = CARTESIAN_POINT('Ctrl Pts',(15.5011751572282,10.2189853926499,-327.712099378994)) ;
#42299 = CARTESIAN_POINT('Ctrl Pts',(15.577781184385,10.1018229548233,-327.71388329619)) ;
#42300 = CARTESIAN_POINT('Ctrl Pts',(15.7202469001488,9.87845886226319,-327.717279008874)) ;
#42301 = CARTESIAN_POINT('Ctrl Pts',(15.7863736765702,9.77243665554591,-327.718888627197)) ;
#42302 = CARTESIAN_POINT('Ctrl Pts',(15.9365768448127,9.52610988181825,-327.722623930781)) ;
#42303 = CARTESIAN_POINT('Ctrl Pts',(16.0198794350881,9.38534569325051,-327.724755266258)) ;
#42304 = CARTESIAN_POINT('Ctrl Pts',(16.3262567709777,8.85166503843979,-327.732822955998)) ;
#42305 = CARTESIAN_POINT('Ctrl Pts',(16.5368235853489,8.45175116541721,-327.738846542318)) ;
#42306 = CARTESIAN_POINT('Ctrl Pts',(16.7506682402526,8.00695656437228,-327.745476492103)) ;
#42307 = CARTESIAN_POINT('Ctrl Pts',(16.7686183518665,7.96929598443489,-327.746037275166)) ;
#42308 = CARTESIAN_POINT('Ctrl Pts',(16.977320344606,7.52759762502785,-327.75260701353)) ;
#42309 = CARTESIAN_POINT('Ctrl Pts',(17.1535540572944,7.1168613365757,-327.758648384927)) ;
#42310 = CARTESIAN_POINT('Ctrl Pts',(17.3980817636596,6.48494469835063,-327.76769570092)) ;
#42311 = CARTESIAN_POINT('Ctrl Pts',(17.4773452329137,6.26818640182485,-327.770755396221)) ;
#42312 = CARTESIAN_POINT('Ctrl Pts',(17.5811133620001,5.96712970882221,-327.774920111553)) ;
#42313 = CARTESIAN_POINT('Ctrl Pts',(17.6090920645608,5.88405138501024,-327.776060534989)) ;
#42314 = CARTESIAN_POINT('Ctrl Pts',(17.6550017536798,5.74446918030818,-327.777959924947)) ;
#42315 = CARTESIAN_POINT('Ctrl Pts',(17.6732523491538,5.68807212539553,-327.778722732515)) ;
#42316 = CARTESIAN_POINT('Ctrl Pts',(17.7167530087117,5.55141791192916,-327.780559848186)) ;
#42317 = CARTESIAN_POINT('Ctrl Pts',(17.7417281824127,5.47107476944672,-327.781630828508)) ;
#42318 = CARTESIAN_POINT('Ctrl Pts',(17.8190216128348,5.21633203255912,-327.785001496962)) ;
#42319 = CARTESIAN_POINT('Ctrl Pts',(17.869321017044,5.04133094593128,-327.787280094054)) ;
#42320 = CARTESIAN_POINT('Ctrl Pts',(18.1493968771512,4.00998616637852,-327.800557620631)) ;
#42321 = CARTESIAN_POINT('Ctrl Pts',(18.3201663051196,3.13880782650356,-327.811224976039)) ;
#42322 = CARTESIAN_POINT('Ctrl Pts',(18.4545114030542,2.04275991416404,-327.825026810529)) ;
#42323 = CARTESIAN_POINT('Ctrl Pts',(18.4771878039784,1.82630496046092,-327.827767140321)) ;
#42324 = CARTESIAN_POINT('Ctrl Pts',(18.5075934141066,1.47689012193679,-327.83222284008)) ;
#42325 = CARTESIAN_POINT('Ctrl Pts',(18.5177065724591,1.344158342134,-327.833922801622)) ;
#42326 = CARTESIAN_POINT('Ctrl Pts',(18.5346187715303,1.08549871134924,-327.83725123519)) ;
#42327 = CARTESIAN_POINT('Ctrl Pts',(18.5415639066461,0.959587567914242,-327.838878665049)) ;
#42328 = CARTESIAN_POINT('Ctrl Pts',(18.5541448691738,0.679672026233069,-327.842513120881)) ;
#42329 = CARTESIAN_POINT('Ctrl Pts',(18.5591470564903,0.525648485061498,-327.844524074546)) ;
#42330 = CARTESIAN_POINT('Ctrl Pts',(18.5706458829459,-0.0487728198690466,
-327.852064087765)) ;
#42331 = CARTESIAN_POINT('Ctrl Pts',(18.5647775975318,-0.469202087608817,
-327.857666110766)) ;
#42332 = CARTESIAN_POINT('Ctrl Pts',(18.5446545920453,-0.888980013405447,
-327.863308832765)) ;
#42333 = CARTESIAN_POINT('Origin',(0.,0.,-315.477129595899)) ;
#42334 = CARTESIAN_POINT('',(18.5446545937453,-0.888979977940784,-329.658408769442)) ;
#42335 = CARTESIAN_POINT('',(18.5446545935817,-0.888979981355556,-329.363119887734)) ;
#42336 = CARTESIAN_POINT('',(18.544654593745,-0.888979977948782,-315.477129595899)) ;
#42337 = CARTESIAN_POINT('Ctrl Pts',(18.5446545937457,-0.888979977932787,
-329.658408769442)) ;
#42338 = CARTESIAN_POINT('Ctrl Pts',(18.5464056157976,-0.852452609550874,
-329.657945483223)) ;
#42339 = CARTESIAN_POINT('Ctrl Pts',(18.548048719277,-0.81591999982208,-329.657483285843)) ;
#42340 = CARTESIAN_POINT('Ctrl Pts',(18.5630941390681,-0.457833654916934,
-329.652963311734)) ;
#42341 = CARTESIAN_POINT('Ctrl Pts',(18.5682412777646,-0.13598693597125,-329.648982036948)) ;
#42342 = CARTESIAN_POINT('Ctrl Pts',(18.5640719297102,0.280542107439365,-329.643860347317)) ;
#42343 = CARTESIAN_POINT('Ctrl Pts',(18.5623991451796,0.375244544935029,-329.642698014782)) ;
#42344 = CARTESIAN_POINT('Ctrl Pts',(18.5511258441397,0.820486321522968,-329.63723744753)) ;
#42345 = CARTESIAN_POINT('Ctrl Pts',(18.5323198928692,1.17072082538506,-329.632952652673)) ;
#42346 = CARTESIAN_POINT('Ctrl Pts',(18.48122711744,1.79260822178519,-329.625269663356)) ;
#42347 = CARTESIAN_POINT('Ctrl Pts',(18.4528354240194,2.06447680806557,-329.621885679587)) ;
#42348 = CARTESIAN_POINT('Ctrl Pts',(18.3913704034129,2.5491836723963,-329.615777062905)) ;
#42349 = CARTESIAN_POINT('Ctrl Pts',(18.3605761713517,2.76226087358939,-329.613065611654)) ;
#42350 = CARTESIAN_POINT('Ctrl Pts',(18.3048216159088,3.10573890129734,-329.608644281449)) ;
#42351 = CARTESIAN_POINT('Ctrl Pts',(18.2821560091663,3.23649194477292,-329.606949348729)) ;
#42352 = CARTESIAN_POINT('Ctrl Pts',(18.2351779117158,3.49123882555864,-329.603622658193)) ;
#42353 = CARTESIAN_POINT('Ctrl Pts',(18.2109975284144,3.61524978047479,-329.601991852761)) ;
#42354 = CARTESIAN_POINT('Ctrl Pts',(18.1481982967582,3.92068907093482,-329.597946527125)) ;
#42355 = CARTESIAN_POINT('Ctrl Pts',(18.1081227649738,4.10180374629958,-329.595522652821)) ;
#42356 = CARTESIAN_POINT('Ctrl Pts',(17.9544386770753,4.75013842607234,-329.586757648808)) ;
#42357 = CARTESIAN_POINT('Ctrl Pts',(17.8254049329426,5.2135036140851,-329.580322648283)) ;
#42358 = CARTESIAN_POINT('Ctrl Pts',(17.5242735712885,6.15218208866002,-329.567056188216)) ;
#42359 = CARTESIAN_POINT('Ctrl Pts',(17.3504621607203,6.62653542863033,-329.560226365094)) ;
#42360 = CARTESIAN_POINT('Ctrl Pts',(17.0950067691068,7.24444783859639,-329.551357988226)) ;
#42361 = CARTESIAN_POINT('Ctrl Pts',(17.0304862722755,7.39485080357388,-329.549202283536)) ;
#42362 = CARTESIAN_POINT('Ctrl Pts',(16.9322439963063,7.6157543493639,-329.546050403293)) ;
#42363 = CARTESIAN_POINT('Ctrl Pts',(16.9000521322515,7.6869264995685,-329.545037139498)) ;
#42364 = CARTESIAN_POINT('Ctrl Pts',(16.8394093829016,7.81877752980614,-329.543165636627)) ;
#42365 = CARTESIAN_POINT('Ctrl Pts',(16.8110773286262,7.87950946866018,-329.542306000018)) ;
#42366 = CARTESIAN_POINT('Ctrl Pts',(16.7458959506702,8.01727887965723,-329.540360393077)) ;
#42367 = CARTESIAN_POINT('Ctrl Pts',(16.7088426612801,8.09421823106599,-329.539276952249)) ;
#42368 = CARTESIAN_POINT('Ctrl Pts',(16.5463595160849,8.42573605378673,-329.534616865767)) ;
#42369 = CARTESIAN_POINT('Ctrl Pts',(16.4156321655984,8.67767610317607,-329.531096045575)) ;
#42370 = CARTESIAN_POINT('Ctrl Pts',(16.0002642668367,9.43517719972528,-329.520451921263)) ;
#42371 = CARTESIAN_POINT('Ctrl Pts',(15.6976608899925,9.9304818258345,-329.513402326031)) ;
#42372 = CARTESIAN_POINT('Ctrl Pts',(15.2830317075343,10.5427141580516,-329.504260368031)) ;
#42373 = CARTESIAN_POINT('Ctrl Pts',(15.1920033812151,10.673467720669,-329.502282615644)) ;
#42374 = CARTESIAN_POINT('Ctrl Pts',(14.966220685514,10.9890421840235,-329.497439347552)) ;
#42375 = CARTESIAN_POINT('Ctrl Pts',(14.8297121852846,11.17257561876,-329.49456268219)) ;
#42376 = CARTESIAN_POINT('Ctrl Pts',(14.6072544258106,11.4604039708628,-329.489944638299)) ;
#42377 = CARTESIAN_POINT('Ctrl Pts',(14.5234973425004,11.5663635561837,-329.488220922475)) ;
#42378 = CARTESIAN_POINT('Ctrl Pts',(14.359042603586,11.769809148002,-329.484863735291)) ;
#42379 = CARTESIAN_POINT('Ctrl Pts',(14.2784896241219,11.8674026590362,-329.483231523347)) ;
#42380 = CARTESIAN_POINT('Ctrl Pts',(14.1001314241273,12.0790464822641,-329.479643353384)) ;
#42381 = CARTESIAN_POINT('Ctrl Pts',(14.0019267739386,12.1927485263665,-329.477684121172)) ;
#42382 = CARTESIAN_POINT('Ctrl Pts',(13.5549776628183,12.6977074958631,-329.468840954069)) ;
#42383 = CARTESIAN_POINT('Ctrl Pts',(13.1911404705956,13.0752822146579,-329.461831737615)) ;
#42384 = CARTESIAN_POINT('Ctrl Pts',(12.4461530609739,13.7856100631217,-329.447979225795)) ;
#42385 = CARTESIAN_POINT('Ctrl Pts',(12.0664070907128,14.1191922952866,-329.441145797908)) ;
#42386 = CARTESIAN_POINT('Ctrl Pts',(11.5461471190198,14.539870063039,-329.432271616335)) ;
#42387 = CARTESIAN_POINT('Ctrl Pts',(11.4174068721334,14.6411801169166,-329.430113706025)) ;
#42388 = CARTESIAN_POINT('Ctrl Pts',(11.2253013397838,14.7882796570412,-329.426959289101)) ;
#42389 = CARTESIAN_POINT('Ctrl Pts',(11.162960688388,14.8353939642875,-329.425945656568)) ;
#42390 = CARTESIAN_POINT('Ctrl Pts',(11.0466133096676,14.922175567033,-329.424073892906)) ;
#42391 = CARTESIAN_POINT('Ctrl Pts',(10.9926858132041,14.9619466604146,-329.423214359202)) ;
#42392 = CARTESIAN_POINT('Ctrl Pts',(10.8695786363941,15.0517123522689,-329.421269395023)) ;
#42393 = CARTESIAN_POINT('Ctrl Pts',(10.8002670835109,15.1015236125255,-329.420186488422)) ;
#42394 = CARTESIAN_POINT('Ctrl Pts',(10.4970057537607,15.3163088751214,-329.415495752473)) ;
#42395 = CARTESIAN_POINT('Ctrl Pts',(10.2596010859597,15.4763378610795,-329.411944833104)) ;
#42396 = CARTESIAN_POINT('Ctrl Pts',(9.53167290427586,15.9429044066923,-329.401293244489)) ;
#42397 = CARTESIAN_POINT('Ctrl Pts',(9.03043783209601,16.2320726682406,-329.394264483782)) ;
#42398 = CARTESIAN_POINT('Ctrl Pts',(8.3751603521555,16.5703499645443,-329.385146734879)) ;
#42399 = CARTESIAN_POINT('Ctrl Pts',(8.23286420762254,16.6415070152318,-329.383171694541)) ;
#42400 = CARTESIAN_POINT('Ctrl Pts',(7.88400204667147,16.8103903565124,-329.378333753632)) ;
#42401 = CARTESIAN_POINT('Ctrl Pts',(7.67651260857948,16.906148766256,-329.375459708821)) ;
#42402 = CARTESIAN_POINT('Ctrl Pts',(7.34368745221428,17.0523601169786,-329.370844785587)) ;
#42403 = CARTESIAN_POINT('Ctrl Pts',(7.21947736706305,17.1053172270247,-329.369121525399)) ;
#42404 = CARTESIAN_POINT('Ctrl Pts',(6.97774843408016,17.2052766012387,-329.36576456597)) ;
#42405 = CARTESIAN_POINT('Ctrl Pts',(6.86030474969144,17.2524414162647,-329.364132118633)) ;
#42406 = CARTESIAN_POINT('Ctrl Pts',(6.60233316493429,17.3529908531503,-329.360542624641)) ;
#42407 = CARTESIAN_POINT('Ctrl Pts',(6.46162055661302,17.4058770093359,-329.358582293492)) ;
#42408 = CARTESIAN_POINT('Ctrl Pts',(5.88015319146191,17.6163958362378,-329.350472649438)) ;
#42409 = CARTESIAN_POINT('Ctrl Pts',(5.43415750933693,17.7590409006545,-329.34422669434)) ;
#42410 = CARTESIAN_POINT('Ctrl Pts',(4.72798379895485,17.9558037517669,-329.334373393803)) ;
#42411 = CARTESIAN_POINT('Ctrl Pts',(4.47122392841441,18.0214559813872,-329.330799308776)) ;
#42412 = CARTESIAN_POINT('Ctrl Pts',(3.94290922258713,18.1445573024967,-329.323498428541)) ;
#42413 = CARTESIAN_POINT('Ctrl Pts',(3.67129333729694,18.201458688249,-329.319773261476)) ;
#42414 = CARTESIAN_POINT('Ctrl Pts',(3.22509943348238,18.2845384068916,-329.313744332418)) ;
#42415 = CARTESIAN_POINT('Ctrl Pts',(3.05124300540132,18.3143530439589,-329.311417617706)) ;
#42416 = CARTESIAN_POINT('Ctrl Pts',(2.79776490737793,18.3541123904302,-329.30807005776)) ;
#42417 = CARTESIAN_POINT('Ctrl Pts',(2.71846207337928,18.3660255389394,-329.307029100146)) ;
#42418 = CARTESIAN_POINT('Ctrl Pts',(2.57328881674885,18.3868731004828,-329.305136687279)) ;
#42419 = CARTESIAN_POINT('Ctrl Pts',(2.507443016451,18.3959682338385,-329.304283462929)) ;
#42420 = CARTESIAN_POINT('Ctrl Pts',(2.34388534797976,18.417665624753,-329.302175906683)) ;
#42421 = CARTESIAN_POINT('Ctrl Pts',(2.24611929529175,18.4298441051964,-329.300926406365)) ;
#42422 = CARTESIAN_POINT('Ctrl Pts',(1.80395475097615,18.4813528207075,-329.295313348593)) ;
#42423 = CARTESIAN_POINT('Ctrl Pts',(1.45859197412777,18.5118115108392,-329.291032032854)) ;
#42424 = CARTESIAN_POINT('Ctrl Pts',(0.70047964845604,18.5573237698163,-329.281703112689)) ;
#42425 = CARTESIAN_POINT('Ctrl Pts',(0.287669937373465,18.568311270573,-329.276666901431)) ;
#42426 = CARTESIAN_POINT('Ctrl Pts',(-0.401620203831488,18.5636643251038,
-329.26818172439)) ;
#42427 = CARTESIAN_POINT('Ctrl Pts',(-0.678001836750486,18.5556257005605,
-329.264759766599)) ;
#42428 = CARTESIAN_POINT('Ctrl Pts',(-1.17076365192046,18.5302692686968,-329.258592146341)) ;
#42429 = CARTESIAN_POINT('Ctrl Pts',(-1.38721458448472,18.5153234418784,-329.255860093777)) ;
#42430 = CARTESIAN_POINT('Ctrl Pts',(-1.73585090042897,18.485102340234,-329.251414246141)) ;
#42431 = CARTESIAN_POINT('Ctrl Pts',(-1.86822093544779,18.4721936258859,-329.249715726479)) ;
#42432 = CARTESIAN_POINT('Ctrl Pts',(-2.12587391853036,18.4442695105792,-329.246387813588)) ;
#42433 = CARTESIAN_POINT('Ctrl Pts',(-2.25116517340885,18.429396978869,-329.244759436983)) ;
#42434 = CARTESIAN_POINT('Ctrl Pts',(-2.55914005515718,18.3896517289511,-329.240731392047)) ;
#42435 = CARTESIAN_POINT('Ctrl Pts',(-2.74162325887527,18.3633327660953,-329.238322556326)) ;
#42436 = CARTESIAN_POINT('Ctrl Pts',(-3.55913171485046,18.2329685694546,-329.227434458451)) ;
#42437 = CARTESIAN_POINT('Ctrl Pts',(-4.18887996161352,18.0986695754916,-329.218767089537)) ;
#42438 = CARTESIAN_POINT('Ctrl Pts',(-5.10880081888335,17.851893967093,-329.205939961591)) ;
#42439 = CARTESIAN_POINT('Ctrl Pts',(-5.40517869083605,17.7644028235072,-329.201784448889)) ;
#42440 = CARTESIAN_POINT('Ctrl Pts',(-5.87852276361185,17.6117278472674,-329.195169087521)) ;
#42441 = CARTESIAN_POINT('Ctrl Pts',(-6.05692033955571,17.5511738601811,-329.19268103426)) ;
#42442 = CARTESIAN_POINT('Ctrl Pts',(-6.31163349007251,17.4603697318797,-329.18915068319)) ;
#42443 = CARTESIAN_POINT('Ctrl Pts',(-6.38871801374282,17.4323122577922,-329.18808522974)) ;
#42444 = CARTESIAN_POINT('Ctrl Pts',(-6.52761399040505,17.3807114214591,-329.186172416622)) ;
#42445 = CARTESIAN_POINT('Ctrl Pts',(-6.58949019849059,17.3573469414404,-329.18532296933)) ;
#42446 = CARTESIAN_POINT('Ctrl Pts',(-6.7403769903966,17.2994489114451,-329.183257475283)) ;
#42447 = CARTESIAN_POINT('Ctrl Pts',(-6.82924856698833,17.2645584554089,-329.182045768209)) ;
#42448 = CARTESIAN_POINT('Ctrl Pts',(-7.1986597147558,17.1162310874814,-329.177022338809)) ;
#42449 = CARTESIAN_POINT('Ctrl Pts',(-7.47667439477461,16.9966293456523,-329.173273115701)) ;
#42450 = CARTESIAN_POINT('Ctrl Pts',(-7.86038173036401,16.8203216160385,-329.168075559127)) ;
#42451 = CARTESIAN_POINT('Ctrl Pts',(-7.96863608411152,16.7693070575595,-329.166606680282)) ;
#42452 = CARTESIAN_POINT('Ctrl Pts',(-8.3931139416433,16.5642345309535,-329.16082698426)) ;
#42453 = CARTESIAN_POINT('Ctrl Pts',(-8.70542577721187,16.4022495177638,-329.156528976738)) ;
#42454 = CARTESIAN_POINT('Ctrl Pts',(-9.25116814710385,16.0992122255411,-329.148842393761)) ;
#42455 = CARTESIAN_POINT('Ctrl Pts',(-9.48644819297611,15.9617056333788,-329.145468430242)) ;
#42456 = CARTESIAN_POINT('Ctrl Pts',(-9.90166242926357,15.7066143058814,-329.13937540489)) ;
#42457 = CARTESIAN_POINT('Ctrl Pts',(-10.0827427968709,15.5909893617076,-329.136669412829)) ;
#42458 = CARTESIAN_POINT('Ctrl Pts',(-10.372297608971,15.3989457461736,-329.132254578447)) ;
#42459 = CARTESIAN_POINT('Ctrl Pts',(-10.4820310121135,15.3244612819719,-329.130560595582)) ;
#42460 = CARTESIAN_POINT('Ctrl Pts',(-10.6947658527859,15.1767077278296,-329.12723421047)) ;
#42461 = CARTESIAN_POINT('Ctrl Pts',(-10.7978358104002,15.103549776777,-329.125602743423)) ;
#42462 = CARTESIAN_POINT('Ctrl Pts',(-11.0259778671037,14.9380879582892,-329.12194652051)) ;
#42463 = CARTESIAN_POINT('Ctrl Pts',(-11.1506539870435,14.8452543036172,-329.119917665964)) ;
#42464 = CARTESIAN_POINT('Ctrl Pts',(-11.8386155483028,14.3194423654408,-329.108551088841)) ;
#42465 = CARTESIAN_POINT('Ctrl Pts',(-12.3778508949711,13.8559751316625,-329.098966796857)) ;
#42466 = CARTESIAN_POINT('Ctrl Pts',(-13.0929840002629,13.1661854156127,-329.085592315766)) ;
#42467 = CARTESIAN_POINT('Ctrl Pts',(-13.2922505309425,12.9649814718804,-329.081789784805)) ;
#42468 = CARTESIAN_POINT('Ctrl Pts',(-13.6095902916943,12.629546918324,-329.075654422096)) ;
#42469 = CARTESIAN_POINT('Ctrl Pts',(-13.7304644292381,12.4980298455889,-329.073297717164)) ;
#42470 = CARTESIAN_POINT('Ctrl Pts',(-13.9030628198843,12.3047076648567,-329.069916047151)) ;
#42471 = CARTESIAN_POINT('Ctrl Pts',(-13.9563120411438,12.2442778768537,-329.068870417922)) ;
#42472 = CARTESIAN_POINT('Ctrl Pts',(-14.0527384690571,12.133402226157,-329.066974238976)) ;
#42473 = CARTESIAN_POINT('Ctrl Pts',(-14.0960413757827,12.083067722556,-329.066121858766)) ;
#42474 = CARTESIAN_POINT('Ctrl Pts',(-14.2025233464681,11.9579435874088,-329.064022909729)) ;
#42475 = CARTESIAN_POINT('Ctrl Pts',(-14.2653826326845,11.882884440652,-329.062781072598)) ;
#42476 = CARTESIAN_POINT('Ctrl Pts',(-14.5322876758576,11.559007637291,-329.057488347771)) ;
#42477 = CARTESIAN_POINT('Ctrl Pts',(-14.7304400882219,11.305404830605,-329.053507742861)) ;
#42478 = CARTESIAN_POINT('Ctrl Pts',(-14.9781817664607,10.9707573718264,-329.048388273981)) ;
#42479 = CARTESIAN_POINT('Ctrl Pts',(-15.0338802013486,10.8943055051733,-329.047227507275)) ;
#42480 = CARTESIAN_POINT('Ctrl Pts',(-15.2932833251524,10.5324699147148,-329.041769034841)) ;
#42481 = CARTESIAN_POINT('Ctrl Pts',(-15.4894613038502,10.2417784519133,-329.037484771849)) ;
#42482 = CARTESIAN_POINT('Ctrl Pts',(-15.8237208744952,9.71488938933557,-329.02980192998)) ;
#42483 = CARTESIAN_POINT('Ctrl Pts',(-15.9650364158651,9.48086652552187,-329.026417545776)) ;
#42484 = CARTESIAN_POINT('Ctrl Pts',(-16.2083253132601,9.05709892187497,-329.020308306214)) ;
#42485 = CARTESIAN_POINT('Ctrl Pts',(-16.3122615459554,8.86853840066222,-329.017596637)) ;
#42486 = CARTESIAN_POINT('Ctrl Pts',(-16.4749233654184,8.56090003707979,-329.013175047433)) ;
#42487 = CARTESIAN_POINT('Ctrl Pts',(-16.5356923678803,8.44292527474377,-329.011480076782)) ;
#42488 = CARTESIAN_POINT('Ctrl Pts',(-16.6518382379373,8.2113789844864,-329.008153373888)) ;
#42489 = CARTESIAN_POINT('Ctrl Pts',(-16.7073309067011,8.09787351404136,-329.006522594713)) ;
#42490 = CARTESIAN_POINT('Ctrl Pts',(-16.8414186598449,7.81636214904177,-329.002477455215)) ;
#42491 = CARTESIAN_POINT('Ctrl Pts',(-16.9186628695807,7.64772817650856,-329.000053742808)) ;
#42492 = CARTESIAN_POINT('Ctrl Pts',(-17.1870954909235,7.03772613870586,-328.991286762151)) ;
#42493 = CARTESIAN_POINT('Ctrl Pts',(-17.3636423636545,6.59012611138508,-328.984849540912)) ;
#42494 = CARTESIAN_POINT('Ctrl Pts',(-17.6894863660748,5.65963865569467,-328.971581794006)) ;
#42495 = CARTESIAN_POINT('Ctrl Pts',(-17.8368548722474,5.17648975658616,-328.964752948045)) ;
#42496 = CARTESIAN_POINT('Ctrl Pts',(-18.0056575068686,4.52963178282796,-328.955886144614)) ;
#42497 = CARTESIAN_POINT('Ctrl Pts',(-18.0448740885557,4.37078775806497,-328.953731037755)) ;
#42498 = CARTESIAN_POINT('Ctrl Pts',(-18.0997033642613,4.13537640533821,-328.950579845134)) ;
#42499 = CARTESIAN_POINT('Ctrl Pts',(-18.1169404239192,4.0591956822157,-328.949566681338)) ;
#42500 = CARTESIAN_POINT('Ctrl Pts',(-18.1480733524763,3.91745125482738,-328.947695249101)) ;
#42501 = CARTESIAN_POINT('Ctrl Pts',(-18.1620958938704,3.85191685695051,-328.946835584497)) ;
#42502 = CARTESIAN_POINT('Ctrl Pts',(-18.1931811372667,3.70269549523105,-328.944889802918)) ;
#42503 = CARTESIAN_POINT('Ctrl Pts',(-18.2100218289735,3.61896377970072,-328.943806216979)) ;
#42504 = CARTESIAN_POINT('Ctrl Pts',(-18.2802550542846,3.25685693041649,-328.939150435351)) ;
#42505 = CARTESIAN_POINT('Ctrl Pts',(-18.3278466238248,2.97739495370585,-328.935633908894)) ;
#42506 = CARTESIAN_POINT('Ctrl Pts',(-18.4533248128601,2.12275947188802,-328.924990978)) ;
#42507 = CARTESIAN_POINT('Ctrl Pts',(-18.5106590836004,1.54492913503653,-328.91793853273)) ;
#42508 = CARTESIAN_POINT('Ctrl Pts',(-18.549120541585,0.806236216037114,-328.908793263879)) ;
#42509 = CARTESIAN_POINT('Ctrl Pts',(-18.555356898997,0.64700848545377,-328.906815141501)) ;
#42510 = CARTESIAN_POINT('Ctrl Pts',(-18.5655517874979,0.259055709987912,
-328.901971146802)) ;
#42511 = CARTESIAN_POINT('Ctrl Pts',(-18.5673343449506,0.0302998911234719,
-328.899094124089)) ;
#42512 = CARTESIAN_POINT('Ctrl Pts',(-18.5634460026754,-0.333489004622157,
-328.894475654654)) ;
#42513 = CARTESIAN_POINT('Ctrl Pts',(-18.5605286509434,-0.468528060685627,
-328.892751876703)) ;
#42514 = CARTESIAN_POINT('Ctrl Pts',(-18.5520246752332,-0.72999434392318,
-328.88939465837)) ;
#42515 = CARTESIAN_POINT('Ctrl Pts',(-18.5466184483464,-0.856420089644797,
-328.887762478429)) ;
#42516 = CARTESIAN_POINT('Ctrl Pts',(-18.5319681614582,-1.13279424658688,
-328.884174488593)) ;
#42517 = CARTESIAN_POINT('Ctrl Pts',(-18.5221956767152,-1.28270572131308,
-328.882215405908)) ;
#42518 = CARTESIAN_POINT('Ctrl Pts',(-18.4701576356817,-1.95514396538228,
-328.873370955207)) ;
#42519 = CARTESIAN_POINT('Ctrl Pts',(-18.4075919403145,-2.47585677836037,
-328.866360241071)) ;
#42520 = CARTESIAN_POINT('Ctrl Pts',(-18.2416270395859,-3.49181508586461,
-328.852506770226)) ;
#42521 = CARTESIAN_POINT('Ctrl Pts',(-18.1398605465809,-3.9868771384187,-328.845673908469)) ;
#42522 = CARTESIAN_POINT('Ctrl Pts',(-17.9785332538672,-4.63612643559636,
-328.836800638558)) ;
#42523 = CARTESIAN_POINT('Ctrl Pts',(-17.9369337740724,-4.79455245330044,
-328.834643074665)) ;
#42524 = CARTESIAN_POINT('Ctrl Pts',(-17.8724007767717,-5.0277127184577,-328.831489056131)) ;
#42525 = CARTESIAN_POINT('Ctrl Pts',(-17.8510829284046,-5.10288575321948,
-328.830475481492)) ;
#42526 = CARTESIAN_POINT('Ctrl Pts',(-17.8106031098457,-5.24227110247202,
-328.828603758811)) ;
#42527 = CARTESIAN_POINT('Ctrl Pts',(-17.7915668699794,-5.30651842072874,
-328.827744208984)) ;
#42528 = CARTESIAN_POINT('Ctrl Pts',(-17.7474909134409,-5.45237121802005,
-328.825799144012)) ;
#42529 = CARTESIAN_POINT('Ctrl Pts',(-17.7222353661028,-5.53390994477335,
-328.824716153623)) ;
#42530 = CARTESIAN_POINT('Ctrl Pts',(-17.6094535757236,-5.88933954250445,
-328.820009324466)) ;
#42531 = CARTESIAN_POINT('Ctrl Pts',(-17.5161334821473,-6.16135082649842,
-328.81644294422)) ;
#42532 = CARTESIAN_POINT('Ctrl Pts',(-17.2165290404984,-6.97273345663403,
-328.805788189731)) ;
#42533 = CARTESIAN_POINT('Ctrl Pts',(-16.9913657990118,-7.5047567311333,-328.798770765493)) ;
#42534 = CARTESIAN_POINT('Ctrl Pts',(-16.6730612774619,-8.16876965722278,
-328.789666193618)) ;
#42535 = CARTESIAN_POINT('Ctrl Pts',(-16.6025068884232,-8.31122945310268,
-328.787692634373)) ;
#42536 = CARTESIAN_POINT('Ctrl Pts',(-16.426152040784,-8.65610698255043,-328.78285760357)) ;
#42537 = CARTESIAN_POINT('Ctrl Pts',(-16.3184293129125,-8.85751226058293,
-328.779984990748)) ;
#42538 = CARTESIAN_POINT('Ctrl Pts',(-16.1411606873682,-9.17472926637017,
-328.775371772794)) ;
#42539 = CARTESIAN_POINT('Ctrl Pts',(-16.0740194161147,-9.29185800541385,
-328.773648761616)) ;
#42540 = CARTESIAN_POINT('Ctrl Pts',(-15.9414694901437,-9.51735619637811,
-328.770291926144)) ;
#42541 = CARTESIAN_POINT('Ctrl Pts',(-15.8762182696884,-9.62580967363088,
-328.768659349646)) ;
#42542 = CARTESIAN_POINT('Ctrl Pts',(-15.7310325555191,-9.86162882263915,
-328.765069129831)) ;
#42543 = CARTESIAN_POINT('Ctrl Pts',(-15.6506493638892,-9.98870775917945,
-328.763108196374)) ;
#42544 = CARTESIAN_POINT('Ctrl Pts',(-15.3136145829547,-10.5074729380746,
-328.754995433068)) ;
#42545 = CARTESIAN_POINT('Ctrl Pts',(-15.0437335571463,-10.8903561710446,
-328.748746886634)) ;
#42546 = CARTESIAN_POINT('Ctrl Pts',(-14.5991096858575,-11.4730356627758,
-328.738895259044)) ;
#42547 = CARTESIAN_POINT('Ctrl Pts',(-14.4340709491049,-11.6799891570014,
-328.735325465672)) ;
#42548 = CARTESIAN_POINT('Ctrl Pts',(-14.0870600507345,-12.0965380945556,
-328.728028813372)) ;
#42549 = CARTESIAN_POINT('Ctrl Pts',(-13.9046982746158,-12.3057247224738,
-328.724303599432)) ;
#42550 = CARTESIAN_POINT('Ctrl Pts',(-13.5988577892126,-12.6410710945822,
-328.718274605746)) ;
#42551 = CARTESIAN_POINT('Ctrl Pts',(-13.4781475948639,-12.7696965190413,
-328.715947872727)) ;
#42552 = CARTESIAN_POINT('Ctrl Pts',(-13.2999185419667,-12.9542694479112,
-328.712600291941)) ;
#42553 = CARTESIAN_POINT('Ctrl Pts',(-13.2438410796647,-13.0115949688152,
-328.711559331459)) ;
#42554 = CARTESIAN_POINT('Ctrl Pts',(-13.1406053442828,-13.1157694752277,
-328.709666916299)) ;
#42555 = CARTESIAN_POINT('Ctrl Pts',(-13.0935636344892,-13.1627318245329,
-328.708813692487)) ;
#42556 = CARTESIAN_POINT('Ctrl Pts',(-12.9761752210364,-13.2786701949695,
-328.706706141617)) ;
#42557 = CARTESIAN_POINT('Ctrl Pts',(-12.9055297468071,-13.347340840367,-328.705456646075)) ;
#42558 = CARTESIAN_POINT('Ctrl Pts',(-12.5857859767026,-13.6532345523095,
-328.699877049147)) ;
#42559 = CARTESIAN_POINT('Ctrl Pts',(-12.3306698682767,-13.8840701561186,
-328.695627838695)) ;
#42560 = CARTESIAN_POINT('Ctrl Pts',(-11.7555642434101,-14.3760796811826,
-328.686330342133)) ;
#42561 = CARTESIAN_POINT('Ctrl Pts',(-11.4329749027445,-14.6339346302631,
-328.681293973119)) ;
#42562 = CARTESIAN_POINT('Ctrl Pts',(-10.8794061765004,-15.0469328399117,
-328.67279305177)) ;
#42563 = CARTESIAN_POINT('Ctrl Pts',(-10.6530545787562,-15.2080273029687,
-328.669355118658)) ;
#42564 = CARTESIAN_POINT('Ctrl Pts',(-10.2430598536589,-15.4861743613712,
-328.663162715513)) ;
#42565 = CARTESIAN_POINT('Ctrl Pts',(-10.0608111167187,-15.6051898722756,
-328.660422037533)) ;
#42566 = CARTESIAN_POINT('Ctrl Pts',(-9.76379299575491,-15.7917879317515,
-328.655965923129)) ;
#42567 = CARTESIAN_POINT('Ctrl Pts',(-9.65031544826297,-15.8613880676517,
-328.654265900731)) ;
#42568 = CARTESIAN_POINT('Ctrl Pts',(-9.42790727304879,-15.9945291958675,
-328.650937444367)) ;
#42569 = CARTESIAN_POINT('Ctrl Pts',(-9.31905829555421,-16.0581926809078,
-328.649310053635)) ;
#42570 = CARTESIAN_POINT('Ctrl Pts',(-9.07577720059422,-16.1971759899021,
-328.645675811051)) ;
#42571 = CARTESIAN_POINT('Ctrl Pts',(-8.94103888968603,-16.2719410434213,
-328.643665033185)) ;
#42572 = CARTESIAN_POINT('Ctrl Pts',(-8.16624016252996,-16.6893404449532,
-328.632115243328)) ;
#42573 = CARTESIAN_POINT('Ctrl Pts',(-7.50745051015065,-16.99587423295,-328.62231632661)) ;
#42574 = CARTESIAN_POINT('Ctrl Pts',(-6.57620695891841,-17.3644442820637,
-328.608837855675)) ;
#42575 = CARTESIAN_POINT('Ctrl Pts',(-6.31777513304963,-17.4601300357293,
-328.605139102085)) ;
#42576 = CARTESIAN_POINT('Ctrl Pts',(-5.89130357674038,-17.607324679776,-328.599146616342)) ;
#42577 = CARTESIAN_POINT('Ctrl Pts',(-5.72449280064397,-17.6622626685687,
-328.596830243184)) ;
#42578 = CARTESIAN_POINT('Ctrl Pts',(-5.48052838521918,-17.7387913681375,
-328.593494459601)) ;
#42579 = CARTESIAN_POINT('Ctrl Pts',(-5.40397488888692,-17.762262412417,-328.592455125585)) ;
#42580 = CARTESIAN_POINT('Ctrl Pts',(-5.26357100298485,-17.8043180596652,
-328.590564006756)) ;
#42581 = CARTESIAN_POINT('Ctrl Pts',(-5.19976818953087,-17.8230561925155,
-328.589710474263)) ;
#42582 = CARTESIAN_POINT('Ctrl Pts',(-5.04098000197888,-17.8687651904691,
-328.587599856457)) ;
#42583 = CARTESIAN_POINT('Ctrl Pts',(-4.9458775032724,-17.895321862883,-328.586347638173)) ;
#42584 = CARTESIAN_POINT('Ctrl Pts',(-4.52888527505385,-18.0081858549682,
-328.580900799466)) ;
#42585 = CARTESIAN_POINT('Ctrl Pts',(-4.20491615651792,-18.0865762584199,
-328.576781596143)) ;
#42586 = CARTESIAN_POINT('Ctrl Pts',(-3.35359937336498,-18.2684572519014,
-328.566083595378)) ;
#42587 = CARTESIAN_POINT('Ctrl Pts',(-2.82356143339785,-18.3578501042474,
-328.559542363239)) ;
#42588 = CARTESIAN_POINT('Ctrl Pts',(-2.13801239771499,-18.4430740797816,
-328.550994189361)) ;
#42589 = CARTESIAN_POINT('Ctrl Pts',(-1.98540137606864,-18.4601262139273,
-328.549086367512)) ;
#42590 = CARTESIAN_POINT('Ctrl Pts',(-1.61052370376827,-18.497311003647,-328.544381103787)) ;
#42591 = CARTESIAN_POINT('Ctrl Pts',(-1.38807211177403,-18.515333011359,-328.541572665903)) ;
#42592 = CARTESIAN_POINT('Ctrl Pts',(-1.03152679946578,-18.5377569132546,
-328.537035873159)) ;
#42593 = CARTESIAN_POINT('Ctrl Pts',(-0.897616386720214,-18.5447233377103,
-328.53532403784)) ;
#42594 = CARTESIAN_POINT('Ctrl Pts',(-0.638166876905006,-18.5554038820657,
-328.53199071814)) ;
#42595 = CARTESIAN_POINT('Ctrl Pts',(-0.512642296336732,-18.5592959999148,
-328.530370480575)) ;
#42596 = CARTESIAN_POINT('Ctrl Pts',(-0.206612362929484,-18.5656779127097,
-328.52640140547)) ;
#42597 = CARTESIAN_POINT('Ctrl Pts',(-0.0260916677088571,-18.5668092061987,
-328.524044032784)) ;
#42598 = CARTESIAN_POINT('Ctrl Pts',(0.546633240945437,-18.562045578941,-328.516515573085)) ;
#42599 = CARTESIAN_POINT('Ctrl Pts',(0.938647088542706,-18.5463550145626,
-328.5112870223)) ;
#42600 = CARTESIAN_POINT('Ctrl Pts',(1.42083879473946,-18.511726954916,-328.504797286631)) ;
#42601 = CARTESIAN_POINT('Ctrl Pts',(1.51176001042452,-18.5045237549564,-328.503571157027)) ;
#42602 = CARTESIAN_POINT('Ctrl Pts',(2.02827754624916,-18.4597705925993,-328.496595098937)) ;
#42603 = CARTESIAN_POINT('Ctrl Pts',(2.45253075023639,-18.4082083095043,-328.490821385096)) ;
#42604 = CARTESIAN_POINT('Ctrl Pts',(3.09753698460728,-18.307120845082,-328.482107449655)) ;
#42605 = CARTESIAN_POINT('Ctrl Pts',(3.31979263256119,-18.2681248689671,-328.479117246763)) ;
#42606 = CARTESIAN_POINT('Ctrl Pts',(3.62673095271924,-18.2084842618855,-328.475028604905)) ;
#42607 = CARTESIAN_POINT('Ctrl Pts',(3.71206171352296,-18.1912801743966,-328.473896372299)) ;
#42608 = CARTESIAN_POINT('Ctrl Pts',(3.85525920304587,-18.1613596856957,-328.472005614508)) ;
#42609 = CARTESIAN_POINT('Ctrl Pts',(3.91319157136291,-18.1489652844169,-328.471243342477)) ;
#42610 = CARTESIAN_POINT('Ctrl Pts',(4.05378445159341,-18.1181815250775,-328.469399898643)) ;
#42611 = CARTESIAN_POINT('Ctrl Pts',(4.13638026507514,-18.0995035425218,-328.468322143613)) ;
#42612 = CARTESIAN_POINT('Ctrl Pts',(4.40666692614469,-18.0364348928172,-328.464808567297)) ;
#42613 = CARTESIAN_POINT('Ctrl Pts',(4.59379440455133,-17.9896845511195,-328.462396952489)) ;
#42614 = CARTESIAN_POINT('Ctrl Pts',(5.55815924320325,-17.7327274188438,-328.450009668671)) ;
#42615 = CARTESIAN_POINT('Ctrl Pts',(6.32185088266296,-17.4750383503712,-328.440298918956)) ;
#42616 = CARTESIAN_POINT('Ctrl Pts',(7.30456042364226,-17.0705660517323,-328.42707676386)) ;
#42617 = CARTESIAN_POINT('Ctrl Pts',(7.5406545988373,-16.9675972416591,-328.423846330296)) ;
#42618 = CARTESIAN_POINT('Ctrl Pts',(7.90165322635368,-16.8011300932219,-328.418807784695)) ;
#42619 = CARTESIAN_POINT('Ctrl Pts',(8.02810946329015,-16.7410738751505,-328.417023761954)) ;
#42620 = CARTESIAN_POINT('Ctrl Pts',(8.26612797264323,-16.6247177409206,-328.413627969681)) ;
#42621 = CARTESIAN_POINT('Ctrl Pts',(8.37782473529209,-16.5687103987615,-328.41201837882)) ;
#42622 = CARTESIAN_POINT('Ctrl Pts',(8.63439394422414,-16.4368028183087,-328.408283318582)) ;
#42623 = CARTESIAN_POINT('Ctrl Pts',(8.77884580640209,-16.3601073304837,-328.406152201459)) ;
#42624 = CARTESIAN_POINT('Ctrl Pts',(9.31834730278332,-16.0644606446752,-328.398086808872)) ;
#42625 = CARTESIAN_POINT('Ctrl Pts',(9.70637582814352,-15.8330274582888,-328.392065368304)) ;
#42626 = CARTESIAN_POINT('Ctrl Pts',(10.4874606551575,-15.3276480093299,-328.37956772038)) ;
#42627 = CARTESIAN_POINT('Ctrl Pts',(10.8791377499119,-15.052175458738,-328.373090201535)) ;
#42628 = CARTESIAN_POINT('Ctrl Pts',(11.4494675720051,-14.6171521429595,-328.363506708102)) ;
#42629 = CARTESIAN_POINT('Ctrl Pts',(11.6363972174771,-14.4687837996989,-328.360340819286)) ;
#42630 = CARTESIAN_POINT('Ctrl Pts',(11.8887125632867,-14.2604648310821,-328.356060377687)) ;
#42631 = CARTESIAN_POINT('Ctrl Pts',(11.9566057895535,-14.2035883365874,-328.354907897514)) ;
#42632 = CARTESIAN_POINT('Ctrl Pts',(12.0741854825223,-14.1036472968745,-328.352912770747)) ;
#42633 = CARTESIAN_POINT('Ctrl Pts',(12.124054816179,-14.0608007229688,-328.35206695204)) ;
#42634 = CARTESIAN_POINT('Ctrl Pts',(12.2386179580455,-13.9613080939858,-328.350124700544)) ;
#42635 = CARTESIAN_POINT('Ctrl Pts',(12.3031477988333,-13.9044758076888,-328.349031065243)) ;
#42636 = CARTESIAN_POINT('Ctrl Pts',(12.5170677159015,-13.7134185429096,-328.345402700363)) ;
#42637 = CARTESIAN_POINT('Ctrl Pts',(12.6646746446081,-13.5772180047355,-328.342894194451)) ;
#42638 = CARTESIAN_POINT('Ctrl Pts',(13.0723537452098,-13.188608507693,-328.335910739251)) ;
#42639 = CARTESIAN_POINT('Ctrl Pts',(13.3272877573692,-12.9309407435477,-328.331477571104)) ;
#42640 = CARTESIAN_POINT('Ctrl Pts',(13.6716924255063,-12.5618316713683,-328.325294185121)) ;
#42641 = CARTESIAN_POINT('Ctrl Pts',(13.7676658131387,-12.4565712281782,-328.323549083842)) ;
#42642 = CARTESIAN_POINT('Ctrl Pts',(14.1714561070906,-12.0033395108717,-328.316097143368)) ;
#42643 = CARTESIAN_POINT('Ctrl Pts',(14.4673645688335,-11.6449855591653,-328.31035414592)) ;
#42644 = CARTESIAN_POINT('Ctrl Pts',(14.8405968572803,-11.1567769770391,-328.302612721226)) ;
#42645 = CARTESIAN_POINT('Ctrl Pts',(14.930227647745,-11.0365433854141,-328.300712988741)) ;
#42646 = CARTESIAN_POINT('Ctrl Pts',(15.0927541056352,-10.8129214907698,-328.297189505664)) ;
#42647 = CARTESIAN_POINT('Ctrl Pts',(15.1660687413496,-10.7098485767933,-328.29556921202)) ;
#42648 = CARTESIAN_POINT('Ctrl Pts',(15.3155519383036,-10.495077127003,-328.292199800722)) ;
#42649 = CARTESIAN_POINT('Ctrl Pts',(15.3915652597502,-10.3832795332514,-328.290449586867)) ;
#42650 = CARTESIAN_POINT('Ctrl Pts',(15.5932737224311,-10.0795314522182,-328.285703892322)) ;
#42651 = CARTESIAN_POINT('Ctrl Pts',(15.7166426708738,-9.88606506816518,-328.282691132402)) ;
#42652 = CARTESIAN_POINT('Ctrl Pts',(15.91994059827,-9.55382711934579,-328.277537781082)) ;
#42653 = CARTESIAN_POINT('Ctrl Pts',(16.0017178072763,-9.41621730906551,-328.27540918009)) ;
#42654 = CARTESIAN_POINT('Ctrl Pts',(16.374593806261,-8.7698752602981,-328.265446911579)) ;
#42655 = CARTESIAN_POINT('Ctrl Pts',(16.6432759292471,-8.24859979153521,-328.257502542392)) ;
#42656 = CARTESIAN_POINT('Ctrl Pts',(16.9967428638843,-7.47496883062772,-328.246107920495)) ;
#42657 = CARTESIAN_POINT('Ctrl Pts',(17.1014849951204,-7.23212544342308,-328.24258742481)) ;
#42658 = CARTESIAN_POINT('Ctrl Pts',(17.2385552231785,-6.89468411734399,-328.237808681688)) ;
#42659 = CARTESIAN_POINT('Ctrl Pts',(17.2753603700098,-6.80193938442706,-328.23650690668)) ;
#42660 = CARTESIAN_POINT('Ctrl Pts',(17.3354922338592,-6.64677723454865,-328.234351092859)) ;
#42661 = CARTESIAN_POINT('Ctrl Pts',(17.3592337645261,-6.58452289402169,-328.233492080366)) ;
#42662 = CARTESIAN_POINT('Ctrl Pts',(17.4105707678609,-6.44770087281997,-328.231617795872)) ;
#42663 = CARTESIAN_POINT('Ctrl Pts',(17.4380233350864,-6.37308113836966,-328.230604211704)) ;
#42664 = CARTESIAN_POINT('Ctrl Pts',(17.5233819428517,-6.13638381895745,-328.227413109422)) ;
#42665 = CARTESIAN_POINT('Ctrl Pts',(17.5795141043454,-5.97367601426046,-328.2252549615)) ;
#42666 = CARTESIAN_POINT('Ctrl Pts',(17.7955709324368,-5.31796640424708,-328.216661298885)) ;
#42667 = CARTESIAN_POINT('Ctrl Pts',(17.9370832417971,-4.81914500214567,-328.210350747289)) ;
#42668 = CARTESIAN_POINT('Ctrl Pts',(18.0812017706597,-4.21604149813619,-328.202745004273)) ;
#42669 = CARTESIAN_POINT('Ctrl Pts',(18.1040479370264,-4.11683272308126,-328.201494912535)) ;
#42670 = CARTESIAN_POINT('Ctrl Pts',(18.1918934735261,-3.72048715949355,-328.196500223587)) ;
#42671 = CARTESIAN_POINT('Ctrl Pts',(18.2504025878971,-3.42196110445181,-328.19273633045)) ;
#42672 = CARTESIAN_POINT('Ctrl Pts',(18.3367832991858,-2.91560824751373,-328.18630929247)) ;
#42673 = CARTESIAN_POINT('Ctrl Pts',(18.3685167968437,-2.70850211029244,-328.183668784849)) ;
#42674 = CARTESIAN_POINT('Ctrl Pts',(18.4144768576802,-2.37041822269271,-328.179331821818)) ;
#42675 = CARTESIAN_POINT('Ctrl Pts',(18.4308266120378,-2.23974793885727,-328.177649199558)) ;
#42676 = CARTESIAN_POINT('Ctrl Pts',(18.460382338211,-1.98123652937086,-328.174306576125)) ;
#42677 = CARTESIAN_POINT('Ctrl Pts',(18.4736538075379,-1.85341015449862,-328.172647099705)) ;
#42678 = CARTESIAN_POINT('Ctrl Pts',(18.503350011706,-1.53526125336713,-328.168499772076)) ;
#42679 = CARTESIAN_POINT('Ctrl Pts',(18.5181665293139,-1.34480369755538,-328.166001802841)) ;
#42680 = CARTESIAN_POINT('Ctrl Pts',(18.5355446920298,-1.06579525390036,-328.162321368704)) ;
#42681 = CARTESIAN_POINT('Ctrl Pts',(18.54041586422,-0.977402413736633,-328.161152304525)) ;
#42682 = CARTESIAN_POINT('Ctrl Pts',(18.5446545937776,-0.888979977268102,
-328.159979993775)) ;
#42683 = CARTESIAN_POINT('Ctrl Pts',(18.5446545920453,-0.888980013405418,
-327.863308832765)) ;
#42684 = CARTESIAN_POINT('Ctrl Pts',(18.5300411021301,-1.19382615029684,-327.86740662328)) ;
#42685 = CARTESIAN_POINT('Ctrl Pts',(18.5079099903433,-1.49832879568963,-327.871525005959)) ;
#42686 = CARTESIAN_POINT('Ctrl Pts',(18.4515131040269,-2.07657284262969,-327.879343913353)) ;
#42687 = CARTESIAN_POINT('Ctrl Pts',(18.4186468305415,-2.35030632805528,-327.88304433689)) ;
#42688 = CARTESIAN_POINT('Ctrl Pts',(18.3548778686956,-2.7971084657546,-327.88903912823)) ;
#42689 = CARTESIAN_POINT('Ctrl Pts',(18.3275911514274,-2.97064978009094,-327.891356156708)) ;
#42690 = CARTESIAN_POINT('Ctrl Pts',(18.28428621462,-3.22269909291187,-327.894692686652)) ;
#42691 = CARTESIAN_POINT('Ctrl Pts',(18.2702161846501,-3.30153182803569,-327.895732123652)) ;
#42692 = CARTESIAN_POINT('Ctrl Pts',(18.2435298564916,-3.44565515112731,-327.89762332415)) ;
#42693 = CARTESIAN_POINT('Ctrl Pts',(18.2310719907671,-3.51097352680301,-327.89847683669)) ;
#42694 = CARTESIAN_POINT('Ctrl Pts',(18.1992467755902,-3.67309989608745,-327.900587258458)) ;
#42695 = CARTESIAN_POINT('Ctrl Pts',(18.179457648151,-3.76982303372699,-327.901839302926)) ;
#42696 = CARTESIAN_POINT('Ctrl Pts',(18.0861215898884,-4.20818612488769,-327.907490334085)) ;
#42697 = CARTESIAN_POINT('Ctrl Pts',(18.0037089712388,-4.54786642968076,-327.911805742765)) ;
#42698 = CARTESIAN_POINT('Ctrl Pts',(17.8031390693265,-5.28329039476061,-327.921168085715)) ;
#42699 = CARTESIAN_POINT('Ctrl Pts',(17.6812663451557,-5.67782869885497,-327.926204200426)) ;
#42700 = CARTESIAN_POINT('Ctrl Pts',(17.4565186356168,-6.32771602072079,-327.934670107157)) ;
#42701 = CARTESIAN_POINT('Ctrl Pts',(17.360937536812,-6.585429403447,-327.938072408383)) ;
#42702 = CARTESIAN_POINT('Ctrl Pts',(17.1800510866933,-7.04180633717154,-327.944209502882)) ;
#42703 = CARTESIAN_POINT('Ctrl Pts',(17.096930504747,-7.24128157937077,-327.946930908755)) ;
#42704 = CARTESIAN_POINT('Ctrl Pts',(16.957118206431,-7.5609713981056,-327.951364084896)) ;
#42705 = CARTESIAN_POINT('Ctrl Pts',(16.9025846175058,-7.6821077535088,-327.953060750205)) ;
#42706 = CARTESIAN_POINT('Ctrl Pts',(16.7936939753774,-7.91721434561734,-327.956388017307)) ;
#42707 = CARTESIAN_POINT('Ctrl Pts',(16.7394649849125,-8.03123603800784,-327.958017635552)) ;
#42708 = CARTESIAN_POINT('Ctrl Pts',(16.6029471078683,-8.31088734902738,-327.962054531688)) ;
#42709 = CARTESIAN_POINT('Ctrl Pts',(16.5193384520843,-8.47585736883879,-327.964471072519)) ;
#42710 = CARTESIAN_POINT('Ctrl Pts',(16.060666427503,-9.34829690839901,-327.977436107054)) ;
#42711 = CARTESIAN_POINT('Ctrl Pts',(15.6425934124493,-10.0321942133913,-327.988297401468)) ;
#42712 = CARTESIAN_POINT('Ctrl Pts',(15.0601413375938,-10.8596144489829,-328.001872417451)) ;
#42713 = CARTESIAN_POINT('Ctrl Pts',(14.9356630150683,-11.0301882844288,-328.004693081071)) ;
#42714 = CARTESIAN_POINT('Ctrl Pts',(14.7192684500912,-11.3163343740757,-328.009441228138)) ;
#42715 = CARTESIAN_POINT('Ctrl Pts',(14.6288336241622,-11.4330011058988,-328.011381841904)) ;
#42716 = CARTESIAN_POINT('Ctrl Pts',(14.4901743610848,-11.6075414027722,-328.014284714688)) ;
#42717 = CARTESIAN_POINT('Ctrl Pts',(14.4429732637068,-11.6662202000395,-328.015260555245)) ;
#42718 = CARTESIAN_POINT('Ctrl Pts',(14.3529034727887,-11.7768074282067,-328.017098137781)) ;
#42719 = CARTESIAN_POINT('Ctrl Pts',(14.3101069772804,-11.8287729536979,-328.017960861672)) ;
#42720 = CARTESIAN_POINT('Ctrl Pts',(14.1974279317006,-11.9640866670007,-328.020206721017)) ;
#42721 = CARTESIAN_POINT('Ctrl Pts',(14.1270938372403,-12.0470556327372,-328.021583259906)) ;
#42722 = CARTESIAN_POINT('Ctrl Pts',(13.6621538989957,-12.5858465790156,-328.03053504908)) ;
#42723 = CARTESIAN_POINT('Ctrl Pts',(13.2462722157463,-13.022836119876,-328.03786763444)) ;
#42724 = CARTESIAN_POINT('Ctrl Pts',(12.7464603394436,-13.499256330604,-328.046333525624)) ;
#42725 = CARTESIAN_POINT('Ctrl Pts',(12.6826256525536,-13.5592470113239,-328.047408414561)) ;
#42726 = CARTESIAN_POINT('Ctrl Pts',(12.3091365662166,-13.905300165218,-328.053665206647)) ;
#42727 = CARTESIAN_POINT('Ctrl Pts',(11.9902360437277,-14.1812007319378,-328.058883035034)) ;
#42728 = CARTESIAN_POINT('Ctrl Pts',(11.5425052184215,-14.5426526229642,-328.066125984913)) ;
#42729 = CARTESIAN_POINT('Ctrl Pts',(11.421592132145,-14.6378073872467,-328.068073750817)) ;
#42730 = CARTESIAN_POINT('Ctrl Pts',(11.1994958747663,-14.8081625993823,-328.071639424932)) ;
#42731 = CARTESIAN_POINT('Ctrl Pts',(11.0987027881309,-14.8838564823262,-328.073253211064)) ;
#42732 = CARTESIAN_POINT('Ctrl Pts',(10.8898248611445,-15.0374185680877,-328.076589520777)) ;
#42733 = CARTESIAN_POINT('Ctrl Pts',(10.7816570062692,-15.1151617534979,-328.078312922642)) ;
#42734 = CARTESIAN_POINT('Ctrl Pts',(10.494166538148,-15.3171326791413,-328.082882547602)) ;
#42735 = CARTESIAN_POINT('Ctrl Pts',(10.313475159575,-15.4393754637695,-328.08574380936)) ;
#42736 = CARTESIAN_POINT('Ctrl Pts',(9.89710472921494,-15.710490149969,-328.092308838859)) ;
#42737 = CARTESIAN_POINT('Ctrl Pts',(9.66014276590698,-15.8572956107436,-328.096025335753)) ;
#42738 = CARTESIAN_POINT('Ctrl Pts',(9.0641721815128,-16.2082003149744,-328.105297726627)) ;
#42739 = CARTESIAN_POINT('Ctrl Pts',(8.70148898974456,-16.4057631244973,-328.110876874917)) ;
#42740 = CARTESIAN_POINT('Ctrl Pts',(8.02863736007048,-16.7436889677968,-328.120993598246)) ;
#42741 = CARTESIAN_POINT('Ctrl Pts',(7.72061629001675,-16.8879312833566,-328.12553866059)) ;
#42742 = CARTESIAN_POINT('Ctrl Pts',(7.31758164856354,-17.0633348633018,-328.131305388436)) ;
#42743 = CARTESIAN_POINT('Ctrl Pts',(7.22603793407603,-17.1023031682322,-328.13260332491)) ;
#42744 = CARTESIAN_POINT('Ctrl Pts',(7.07270743065675,-17.1661219642137,-328.134754830337)) ;
#42745 = CARTESIAN_POINT('Ctrl Pts',(7.01109226694358,-17.1913792044578,-328.135613326673)) ;
#42746 = CARTESIAN_POINT('Ctrl Pts',(6.87547202374067,-17.2461221661343,-328.137489016636)) ;
#42747 = CARTESIAN_POINT('Ctrl Pts',(6.80141049907751,-17.2754641200991,-328.138504495179)) ;
#42748 = CARTESIAN_POINT('Ctrl Pts',(6.56586482811938,-17.3670339241863,-328.141709372429)) ;
#42749 = CARTESIAN_POINT('Ctrl Pts',(6.40369816402056,-17.427481122392,-328.143879167906)) ;
#42750 = CARTESIAN_POINT('Ctrl Pts',(5.98718969388352,-17.5761349162628,-328.149383342238)) ;
#42751 = CARTESIAN_POINT('Ctrl Pts',(5.73173121889971,-17.6610933021273,-328.152694798589)) ;
#42752 = CARTESIAN_POINT('Ctrl Pts',(4.8028988737558,-17.9477208913343,-328.164617420204)) ;
#42753 = CARTESIAN_POINT('Ctrl Pts',(4.1200536227653,-18.1166685940836,-328.173183881467)) ;
#42754 = CARTESIAN_POINT('Ctrl Pts',(3.24703152559254,-18.2807459702496,-328.184337347047)) ;
#42755 = CARTESIAN_POINT('Ctrl Pts',(3.06428077691759,-18.3122655649673,-328.186681402715)) ;
#42756 = CARTESIAN_POINT('Ctrl Pts',(2.75628331494997,-18.3606471141197,-328.190652331906)) ;
#42757 = CARTESIAN_POINT('Ctrl Pts',(2.6312811088735,-18.378977660206,-328.192269536412)) ;
#42758 = CARTESIAN_POINT('Ctrl Pts',(2.37460497552077,-18.4139447946416,-328.195602698083)) ;
#42759 = CARTESIAN_POINT('Ctrl Pts',(2.24292011651937,-18.4304482034063,-328.197319427269)) ;
#42760 = CARTESIAN_POINT('Ctrl Pts',(1.89712336973055,-18.4700242269768,-328.201845405104)) ;
#42761 = CARTESIAN_POINT('Ctrl Pts',(1.68276749404526,-18.4907859576921,-328.204669155278)) ;
#42762 = CARTESIAN_POINT('Ctrl Pts',(1.19551382079149,-18.5294364864431,-328.211125300394)) ;
#42763 = CARTESIAN_POINT('Ctrl Pts',(0.922484303747169,-18.5450341628335,
-328.214769759589)) ;
#42764 = CARTESIAN_POINT('Ctrl Pts',(0.298923316332265,-18.5668520646512,
-328.223131731931)) ;
#42765 = CARTESIAN_POINT('Ctrl Pts',(-0.0516405535188888,-18.5691864029257,
-328.227861119503)) ;
#42766 = CARTESIAN_POINT('Ctrl Pts',(-0.496303570331408,-18.5595546361347,
-328.233847674073)) ;
#42767 = CARTESIAN_POINT('Ctrl Pts',(-0.590530806398523,-18.5567954911413,
-328.235115459867)) ;
#42768 = CARTESIAN_POINT('Ctrl Pts',(-1.00686034382319,-18.5414303397882,
-328.240709138117)) ;
#42769 = CARTESIAN_POINT('Ctrl Pts',(-1.32862416231878,-18.5211545368095,
-328.245012417834)) ;
#42770 = CARTESIAN_POINT('Ctrl Pts',(-1.74706959872887,-18.4838254727084,
-328.250521759801)) ;
#42771 = CARTESIAN_POINT('Ctrl Pts',(-1.84437221848916,-18.4743700149249,
-328.251796631625)) ;
#42772 = CARTESIAN_POINT('Ctrl Pts',(-2.00761282017689,-18.4572044637966,
-328.253922397132)) ;
#42773 = CARTESIAN_POINT('Ctrl Pts',(-2.07359224684668,-18.4499084302036,
-328.254777940366)) ;
#42774 = CARTESIAN_POINT('Ctrl Pts',(-2.21961930991149,-18.4329674747788,
-328.256662803563)) ;
#42775 = CARTESIAN_POINT('Ctrl Pts',(-2.29964595744679,-18.4231546783294,
-328.257690238041)) ;
#42776 = CARTESIAN_POINT('Ctrl Pts',(-2.55727460430077,-18.3898596861652,
-328.260983381068)) ;
#42777 = CARTESIAN_POINT('Ctrl Pts',(-2.73460166564056,-18.3643281012017,
-328.263227960304)) ;
#42778 = CARTESIAN_POINT('Ctrl Pts',(-3.19250922378791,-18.2916189331276,
-328.268994186409)) ;
#42779 = CARTESIAN_POINT('Ctrl Pts',(-3.47242460788392,-18.2405511455486,
-328.272490222804)) ;
#42780 = CARTESIAN_POINT('Ctrl Pts',(-4.44341021501702,-18.0402427783326,
-328.284644224652)) ;
#42781 = CARTESIAN_POINT('Ctrl Pts',(-5.12704238812446,-17.857986721414,-328.293271213128)) ;
#42782 = CARTESIAN_POINT('Ctrl Pts',(-5.94677606926052,-17.588481445232,-328.304128174259)) ;
#42783 = CARTESIAN_POINT('Ctrl Pts',(-6.09432117181592,-17.5379039377096,
-328.306101912922)) ;
#42784 = CARTESIAN_POINT('Ctrl Pts',(-6.36035732933423,-17.4429458067768,
-328.309699304335)) ;
#42785 = CARTESIAN_POINT('Ctrl Pts',(-6.47906545194072,-17.3992015503873,
-328.31131855925)) ;
#42786 = CARTESIAN_POINT('Ctrl Pts',(-6.72110733833275,-17.307187933771,-328.314650067024)) ;
#42787 = CARTESIAN_POINT('Ctrl Pts',(-6.84439038447217,-17.2588052376531,
-328.316363030721)) ;
#42788 = CARTESIAN_POINT('Ctrl Pts',(-7.16528736218257,-17.1288893906088,
-328.320864384644)) ;
#42789 = CARTESIAN_POINT('Ctrl Pts',(-7.36202910186227,-17.0452551167199,
-328.323666976467)) ;
#42790 = CARTESIAN_POINT('Ctrl Pts',(-7.68887080011427,-16.8996011641234,
-328.32839244557)) ;
#42791 = CARTESIAN_POINT('Ctrl Pts',(-7.81977206796812,-16.8394304662703,
-328.330303983716)) ;
#42792 = CARTESIAN_POINT('Ctrl Pts',(-8.37980858284826,-16.5740629583676,
-328.338559108074)) ;
#42793 = CARTESIAN_POINT('Ctrl Pts',(-8.80167077259434,-16.3539397399262,
-328.344978545542)) ;
#42794 = CARTESIAN_POINT('Ctrl Pts',(-9.25795781762861,-16.0930795496178,
-328.352053823519)) ;
#42795 = CARTESIAN_POINT('Ctrl Pts',(-9.30120339852626,-16.0681239627868,
-328.352725684207)) ;
#42796 = CARTESIAN_POINT('Ctrl Pts',(-9.64002042099114,-15.8707777536731,
-328.35799855157)) ;
#42797 = CARTESIAN_POINT('Ctrl Pts',(-9.93087616425577,-15.690419993574,-328.362580423341)) ;
#42798 = CARTESIAN_POINT('Ctrl Pts',(-10.3113965535809,-15.4396403800449,
-328.368577700864)) ;
#42799 = CARTESIAN_POINT('Ctrl Pts',(-10.4056364256555,-15.3762844857714,
-328.37006310627)) ;
#42800 = CARTESIAN_POINT('Ctrl Pts',(-10.5504878085151,-15.2769617446286,
-328.372342794491)) ;
#42801 = CARTESIAN_POINT('Ctrl Pts',(-10.6015100480348,-15.2415989272808,
-328.373145113702)) ;
#42802 = CARTESIAN_POINT('Ctrl Pts',(-10.7108373304059,-15.1650111078859,
-328.374861945164)) ;
#42803 = CARTESIAN_POINT('Ctrl Pts',(-10.7690838588645,-15.1237042776915,
-328.37577520215)) ;
#42804 = CARTESIAN_POINT('Ctrl Pts',(-10.930250398835,-15.0080062587773,-328.378300212675)) ;
#42805 = CARTESIAN_POINT('Ctrl Pts',(-11.0326477365926,-14.9328935456325,
-328.379902271404)) ;
#42806 = CARTESIAN_POINT('Ctrl Pts',(-11.2702824385203,-14.7548000481966,
-328.383624085673)) ;
#42807 = CARTESIAN_POINT('Ctrl Pts',(-11.4048922717077,-14.6510007545022,
-328.385735377501)) ;
#42808 = CARTESIAN_POINT('Ctrl Pts',(-11.935562562396,-14.2300485528917,-328.394105085832)) ;
#42809 = CARTESIAN_POINT('Ctrl Pts',(-12.3199746369712,-13.898566895034,-328.400278739922)) ;
#42810 = CARTESIAN_POINT('Ctrl Pts',(-12.9586844536724,-13.3004572974636,
-328.411038976111)) ;
#42811 = CARTESIAN_POINT('Ctrl Pts',(-13.2195184557534,-13.0412422003547,
-328.415590473488)) ;
#42812 = CARTESIAN_POINT('Ctrl Pts',(-13.5999938872799,-12.6399766178496,
-328.42253362296)) ;
#42813 = CARTESIAN_POINT('Ctrl Pts',(-13.7254835432438,-12.5035972417051,
-328.424876205074)) ;
#42814 = CARTESIAN_POINT('Ctrl Pts',(-13.9330405005951,-12.271138408274,-328.428845417767)) ;
#42815 = CARTESIAN_POINT('Ctrl Pts',(-14.0162068410048,-12.1760585233152,
-328.430462399685)) ;
#42816 = CARTESIAN_POINT('Ctrl Pts',(-14.1847665037495,-11.9793371741802,
-328.433795751021)) ;
#42817 = CARTESIAN_POINT('Ctrl Pts',(-14.2700530545605,-11.8776136347428,
-328.435512899211)) ;
#42818 = CARTESIAN_POINT('Ctrl Pts',(-14.4909285692868,-11.6083563393389,
-328.440041617174)) ;
#42819 = CARTESIAN_POINT('Ctrl Pts',(-14.6247038614405,-11.4393611890232,
-328.442867721984)) ;
#42820 = CARTESIAN_POINT('Ctrl Pts',(-14.9216640739547,-11.0504928091501,
-328.449330678095)) ;
#42821 = CARTESIAN_POINT('Ctrl Pts',(-15.0829884461214,-10.829261710037,-328.452979634677)) ;
#42822 = CARTESIAN_POINT('Ctrl Pts',(-15.4393140253402,-10.3172006602097,
-328.461340421536)) ;
#42823 = CARTESIAN_POINT('Ctrl Pts',(-15.6310996846999,-10.0242590429054,
-328.466063967434)) ;
#42824 = CARTESIAN_POINT('Ctrl Pts',(-15.8635246395246,-9.64633854319791,
-328.472035762359)) ;
#42825 = CARTESIAN_POINT('Ctrl Pts',(-15.9119573890841,-9.56623611115411,
-328.473294653642)) ;
#42826 = CARTESIAN_POINT('Ctrl Pts',(-16.1136842163482,-9.22683130098725,
-328.478595920781)) ;
#42827 = CARTESIAN_POINT('Ctrl Pts',(-16.2612618798849,-8.96418415413755,
-328.482618768823)) ;
#42828 = CARTESIAN_POINT('Ctrl Pts',(-16.4531047761469,-8.6024161426674,-328.488001709626)) ;
#42829 = CARTESIAN_POINT('Ctrl Pts',(-16.5029879489438,-8.50632759046972,
-328.489416548204)) ;
#42830 = CARTESIAN_POINT('Ctrl Pts',(-16.5824833880533,-8.34986614679401,
-328.4916929519)) ;
#42831 = CARTESIAN_POINT('Ctrl Pts',(-16.612613124818,-8.28975905493632,-328.492560953636)) ;
#42832 = CARTESIAN_POINT('Ctrl Pts',(-16.6758754122883,-8.16182435190642,
-328.494393726641)) ;
#42833 = CARTESIAN_POINT('Ctrl Pts',(-16.7089221054919,-8.09395574551899,
-328.495357447176)) ;
#42834 = CARTESIAN_POINT('Ctrl Pts',(-16.805792235911,-7.89189005093344,-328.498203958701)) ;
#42835 = CARTESIAN_POINT('Ctrl Pts',(-16.8684195068632,-7.75712606026524,
-328.500072767121)) ;
#42836 = CARTESIAN_POINT('Ctrl Pts',(-16.9758350311224,-7.51853089790636,
-328.503340405499)) ;
#42837 = CARTESIAN_POINT('Ctrl Pts',(-17.0213051862685,-7.41501528383948,
-328.504744662579)) ;
#42838 = CARTESIAN_POINT('Ctrl Pts',(-17.238453484798,-6.90813943944556,-328.511567805263)) ;
#42839 = CARTESIAN_POINT('Ctrl Pts',(-17.3967545149665,-6.4992001338689,-328.516913380959)) ;
#42840 = CARTESIAN_POINT('Ctrl Pts',(-17.5875866470013,-5.94911710476848,
-328.524054601083)) ;
#42841 = CARTESIAN_POINT('Ctrl Pts',(-17.6331593371579,-5.81264915114521,
-328.52582193637)) ;
#42842 = CARTESIAN_POINT('Ctrl Pts',(-17.6970635788206,-5.61361622194164,
-328.528397919647)) ;
#42843 = CARTESIAN_POINT('Ctrl Pts',(-17.7166590866234,-5.55146261848974,
-328.529202109731)) ;
#42844 = CARTESIAN_POINT('Ctrl Pts',(-17.8322655254533,-5.17793192505153,
-328.534035291402)) ;
#42845 = CARTESIAN_POINT('Ctrl Pts',(-17.9203926605644,-4.86417506054375,
-328.538096889836)) ;
#42846 = CARTESIAN_POINT('Ctrl Pts',(-18.0379962809472,-4.39874661896167,
-328.544159415084)) ;
#42847 = CARTESIAN_POINT('Ctrl Pts',(-18.073911256405,-4.24876610931386,-328.54611846898)) ;
#42848 = CARTESIAN_POINT('Ctrl Pts',(-18.1353247548754,-3.97742002685228,
-328.549675052812)) ;
#42849 = CARTESIAN_POINT('Ctrl Pts',(-18.1614837852016,-3.85621325964894,
-328.55126809418)) ;
#42850 = CARTESIAN_POINT('Ctrl Pts',(-18.2162043384155,-3.58975088525467,
-328.554780569166)) ;
#42851 = CARTESIAN_POINT('Ctrl Pts',(-18.2442467337896,-3.44439732723533,
-328.556703304959)) ;
#42852 = CARTESIAN_POINT('Ctrl Pts',(-18.3256220108535,-2.99368643591197,
-328.562686016426)) ;
#42853 = CARTESIAN_POINT('Ctrl Pts',(-18.3730482421428,-2.68731802043421,
-328.566782804346)) ;
#42854 = CARTESIAN_POINT('Ctrl Pts',(-18.4772598861388,-1.88105690670342,
-328.577619199434)) ;
#42855 = CARTESIAN_POINT('Ctrl Pts',(-18.5214383058594,-1.37979326884387,
-328.584415474029)) ;
#42856 = CARTESIAN_POINT('Ctrl Pts',(-18.5478080794076,-0.822400084664782,
-328.591921380662)) ;
#42857 = CARTESIAN_POINT('Ctrl Pts',(-18.5501637490318,-0.767431648842084,
-328.5926609585)) ;
#42858 = CARTESIAN_POINT('Ctrl Pts',(-18.5648983072,-0.3837440720037,-328.597817545063)) ;
#42859 = CARTESIAN_POINT('Ctrl Pts',(-18.5687832443194,-0.0547564736898822,
-328.602210508713)) ;
#42860 = CARTESIAN_POINT('Ctrl Pts',(-18.5624825356949,0.371876246913001,
-328.607805992132)) ;
#42861 = CARTESIAN_POINT('Ctrl Pts',(-18.560267922656,0.469579078038605,-328.609080423994)) ;
#42862 = CARTESIAN_POINT('Ctrl Pts',(-18.5552539304723,0.633606287483184,
-328.611205701108)) ;
#42863 = CARTESIAN_POINT('Ctrl Pts',(-18.5528700633289,0.699941283239329,
-328.612061190616)) ;
#42864 = CARTESIAN_POINT('Ctrl Pts',(-18.5468021102246,0.846837874634305,
-328.613946241504)) ;
#42865 = CARTESIAN_POINT('Ctrl Pts',(-18.5429487651842,0.927390973420635,
-328.614973914033)) ;
#42866 = CARTESIAN_POINT('Ctrl Pts',(-18.5288384642232,1.18692122152031,-328.618268838595)) ;
#42867 = CARTESIAN_POINT('Ctrl Pts',(-18.5165140650109,1.36577593317995,-328.620514929925)) ;
#42868 = CARTESIAN_POINT('Ctrl Pts',(-18.4779088790104,1.82825102881213,-328.626286534595)) ;
#42869 = CARTESIAN_POINT('Ctrl Pts',(-18.4476883614047,2.11149541768433,-328.629786380863)) ;
#42870 = CARTESIAN_POINT('Ctrl Pts',(-18.3199193544384,3.09412571405806,-328.641933780138)) ;
#42871 = CARTESIAN_POINT('Ctrl Pts',(-18.189005040234,3.78855569794481,-328.650550674341)) ;
#42872 = CARTESIAN_POINT('Ctrl Pts',(-17.9812435580324,4.62533750497072,-328.661398396789)) ;
#42873 = CARTESIAN_POINT('Ctrl Pts',(-17.9417187268702,4.77635802261492,-328.66337378415)) ;
#42874 = CARTESIAN_POINT('Ctrl Pts',(-17.8667146293908,5.04886320284028,-328.666973195146)) ;
#42875 = CARTESIAN_POINT('Ctrl Pts',(-17.831888752175,5.17051784308506,-328.668592803368)) ;
#42876 = CARTESIAN_POINT('Ctrl Pts',(-17.7580880797287,5.41870219075343,-328.671924042578)) ;
#42877 = CARTESIAN_POINT('Ctrl Pts',(-17.7189980363364,5.54519018662917,-328.67363637404)) ;
#42878 = CARTESIAN_POINT('Ctrl Pts',(-17.6133418642507,5.87454422732882,-328.678133593473)) ;
#42879 = CARTESIAN_POINT('Ctrl Pts',(-17.5446234386492,6.07669891100858,-328.680932632896)) ;
#42880 = CARTESIAN_POINT('Ctrl Pts',(-17.4238113801289,6.41295368059579,-328.685650970359)) ;
#42881 = CARTESIAN_POINT('Ctrl Pts',(-17.3736182306027,6.54771467256947,-328.687558941679)) ;
#42882 = CARTESIAN_POINT('Ctrl Pts',(-17.1512422601802,7.12419421678658,-328.695789179788)) ;
#42883 = CARTESIAN_POINT('Ctrl Pts',(-16.9637408314788,7.55981149840204,-328.7021868489)) ;
#42884 = CARTESIAN_POINT('Ctrl Pts',(-16.7276368943837,8.05519971772877,-328.70957449565)) ;
#42885 = CARTESIAN_POINT('Ctrl Pts',(-16.6950941938299,8.12243242048359,-328.710579445948)) ;
#42886 = CARTESIAN_POINT('Ctrl Pts',(-16.5080197939169,8.50305073414986,-328.716279204931)) ;
#42887 = CARTESIAN_POINT('Ctrl Pts',(-16.3450707909111,8.81222168432377,-328.720951089118)) ;
#42888 = CARTESIAN_POINT('Ctrl Pts',(-16.1250190204767,9.20260868500017,-328.726829367449)) ;
#42889 = CARTESIAN_POINT('Ctrl Pts',(-16.0758584792548,9.28821937813447,-328.728117033713)) ;
#42890 = CARTESIAN_POINT('Ctrl Pts',(-15.9924461305286,9.43083176086942,-328.730257045562)) ;
#42891 = CARTESIAN_POINT('Ctrl Pts',(-15.9585666988887,9.48804879271938,-328.731114194747)) ;
#42892 = CARTESIAN_POINT('Ctrl Pts',(-15.883209712241,9.61376937102261,-328.73299381174)) ;
#42893 = CARTESIAN_POINT('Ctrl Pts',(-15.8415949268799,9.68218893011981,-328.73401449003)) ;
#42894 = CARTESIAN_POINT('Ctrl Pts',(-15.7072750772852,9.89984208749577,-328.737257467807)) ;
#42895 = CARTESIAN_POINT('Ctrl Pts',(-15.6128938346539,10.0480301556232,-328.739459512306)) ;
#42896 = CARTESIAN_POINT('Ctrl Pts',(-15.365026618945,10.4252804577153,-328.745075754619)) ;
#42897 = CARTESIAN_POINT('Ctrl Pts',(-15.2085154515834,10.6523036836069,-328.748465897187)) ;
#42898 = CARTESIAN_POINT('Ctrl Pts',(-14.6219127355575,11.463889924009,-328.760745400854)) ;
#42899 = CARTESIAN_POINT('Ctrl Pts',(-14.1627020257357,12.0265945057044,-328.769594546679)) ;
#42900 = CARTESIAN_POINT('Ctrl Pts',(-13.5674789939611,12.6744530893621,-328.780667958738)) ;
#42901 = CARTESIAN_POINT('Ctrl Pts',(-13.4618098873805,12.7866305894679,-328.782618738671)) ;
#42902 = CARTESIAN_POINT('Ctrl Pts',(-13.2671565738272,12.9881852914467,-328.786188083558)) ;
#42903 = CARTESIAN_POINT('Ctrl Pts',(-13.1786347926589,13.0779962405622,-328.78780249454)) ;
#42904 = CARTESIAN_POINT('Ctrl Pts',(-12.9948032493127,13.2607430577359,-328.791138189861)) ;
#42905 = CARTESIAN_POINT('Ctrl Pts',(-12.8993950554435,13.3535697501581,-328.792860332634)) ;
#42906 = CARTESIAN_POINT('Ctrl Pts',(-12.6454029647254,13.595427120094,-328.79742171938)) ;
#42907 = CARTESIAN_POINT('Ctrl Pts',(-12.4851830147489,13.7427093233366,-328.80027590009)) ;
#42908 = CARTESIAN_POINT('Ctrl Pts',(-11.6792555938629,14.4578291143289,-328.814511544614)) ;
#42909 = CARTESIAN_POINT('Ctrl Pts',(-10.9972362895098,14.9831443320925,-328.826236017318)) ;
#42910 = CARTESIAN_POINT('Ctrl Pts',(-10.1132759228889,15.5710261995572,-328.840382677265)) ;
#42911 = CARTESIAN_POINT('Ctrl Pts',(-9.94346552073621,15.6800095821046,-328.843052746969)) ;
#42912 = CARTESIAN_POINT('Ctrl Pts',(-9.69877822552249,15.8314749290872,-328.846815580553)) ;
#42913 = CARTESIAN_POINT('Ctrl Pts',(-9.6253302380238,15.8762374426617,-328.847934382164)) ;
#42914 = CARTESIAN_POINT('Ctrl Pts',(-9.49519481938215,15.9543128166624,-328.849896042747)) ;
#42915 = CARTESIAN_POINT('Ctrl Pts',(-9.43863672459305,15.9878378433132,-328.850741656057)) ;
#42916 = CARTESIAN_POINT('Ctrl Pts',(-9.30549724544581,16.0658040537127,-328.852716157355)) ;
#42917 = CARTESIAN_POINT('Ctrl Pts',(-9.22877381539913,16.1099991549433,-328.853841827688)) ;
#42918 = CARTESIAN_POINT('Ctrl Pts',(-8.94431747867649,16.2711559596593,-328.857975609634)) ;
#42919 = CARTESIAN_POINT('Ctrl Pts',(-8.73465328176057,16.3846624589636,-328.860945111996)) ;
#42920 = CARTESIAN_POINT('Ctrl Pts',(-8.09849647217279,16.7133785583656,-328.869797976526)) ;
#42921 = CARTESIAN_POINT('Ctrl Pts',(-7.66582690318696,16.9161983608373,-328.87561514106)) ;
#42922 = CARTESIAN_POINT('Ctrl Pts',(-6.80882715397221,17.2782896736915,-328.887041281656)) ;
#42923 = CARTESIAN_POINT('Ctrl Pts',(-6.3855329231001,17.4391625152545,-328.892641207699)) ;
#42924 = CARTESIAN_POINT('Ctrl Pts',(-5.80178697817189,17.63690869026,-328.900406749879)) ;
#42925 = CARTESIAN_POINT('Ctrl Pts',(-5.64610285607817,17.6873627971359,-328.902481363536)) ;
#42926 = CARTESIAN_POINT('Ctrl Pts',(-5.37039885622113,17.7727018436518,-328.90616468816)) ;
#42927 = CARTESIAN_POINT('Ctrl Pts',(-5.25065557123506,17.8084454885514,-328.907767483206)) ;
#42928 = CARTESIAN_POINT('Ctrl Pts',(-4.99607695718351,17.8816468937493,-328.911182421605)) ;
#42929 = CARTESIAN_POINT('Ctrl Pts',(-4.86116049450667,17.9187945791184,-328.912996538463)) ;
#42930 = CARTESIAN_POINT('Ctrl Pts',(-4.47709968718839,18.0198844211697,-328.918173239851)) ;
#42931 = CARTESIAN_POINT('Ctrl Pts',(-4.22702904635217,18.0801792353798,-328.921559122564)) ;
#42932 = CARTESIAN_POINT('Ctrl Pts',(-3.16194626012095,18.3136769929548,-328.93602764114)) ;
#42933 = CARTESIAN_POINT('Ctrl Pts',(-2.33702352660584,18.4371087597631,-328.947396428164)) ;
#42934 = CARTESIAN_POINT('Ctrl Pts',(-1.33002530105114,18.5190961091707,-328.960818447185)) ;
#42935 = CARTESIAN_POINT('Ctrl Pts',(-1.15324428054706,18.5309448172915,-328.96315568684)) ;
#42936 = CARTESIAN_POINT('Ctrl Pts',(-0.896116445282131,18.5444850363538,
-328.966515224425)) ;
#42937 = CARTESIAN_POINT('Ctrl Pts',(-0.815885649505258,18.5481880672469,
-328.967557827648)) ;
#42938 = CARTESIAN_POINT('Ctrl Pts',(-0.675949258570448,18.5537370841316,
-328.96936493221)) ;
#42939 = CARTESIAN_POINT('Ctrl Pts',(-0.616254274080633,18.5558157420915,
-328.970132091641)) ;
#42940 = CARTESIAN_POINT('Ctrl Pts',(-0.463829799070343,18.5603870144338,
-328.972081981578)) ;
#42941 = CARTESIAN_POINT('Ctrl Pts',(-0.371089758064073,18.5624728049455,
-328.973260042188)) ;
#42942 = CARTESIAN_POINT('Ctrl Pts',(0.00228856765034612,18.5680710652833,
-328.977975801849)) ;
#42943 = CARTESIAN_POINT('Ctrl Pts',(0.282975029303099,18.5659148470277,-328.981459516529)) ;
#42944 = CARTESIAN_POINT('Ctrl Pts',(1.27669570988853,18.5357400067762,-328.993713250721)) ;
#42945 = CARTESIAN_POINT('Ctrl Pts',(1.98804470223297,18.4729881337875,-329.00236209498)) ;
#42946 = CARTESIAN_POINT('Ctrl Pts',(2.93652311281207,18.3338868430283,-329.014301394551)) ;
#42947 = CARTESIAN_POINT('Ctrl Pts',(3.17830329243401,18.2935224223884,-329.017378159301)) ;
#42948 = CARTESIAN_POINT('Ctrl Pts',(3.55594556526066,18.2227633116825,-329.022249201092)) ;
#42949 = CARTESIAN_POINT('Ctrl Pts',(3.69238576582513,18.1956076805139,-329.024022479073)) ;
#42950 = CARTESIAN_POINT('Ctrl Pts',(3.9509737619485,18.1411126930506,-329.027410377427)) ;
#42951 = CARTESIAN_POINT('Ctrl Pts',(4.0731755640644,18.1140664728138,-329.029022974264)) ;
#42952 = CARTESIAN_POINT('Ctrl Pts',(4.35900190358412,18.0477675329933,-329.032822590077)) ;
#42953 = CARTESIAN_POINT('Ctrl Pts',(4.5223847500422,18.0075219441354,-329.035016032389)) ;
#42954 = CARTESIAN_POINT('Ctrl Pts',(5.25148165400773,17.8173771320086,-329.044899707635)) ;
#42955 = CARTESIAN_POINT('Ctrl Pts',(5.81046424766624,17.6430011113935,-329.052747661673)) ;
#42956 = CARTESIAN_POINT('Ctrl Pts',(6.85645229004998,17.2615900142105,-329.067742915159)) ;
#42957 = CARTESIAN_POINT('Ctrl Pts',(7.34468565292565,17.0595727237352,-329.074874526586)) ;
#42958 = CARTESIAN_POINT('Ctrl Pts',(7.9245127595969,16.7901449959315,-329.083284559573)) ;
#42959 = CARTESIAN_POINT('Ctrl Pts',(8.02496124031148,16.7423674732572,-329.084738960207)) ;
#42960 = CARTESIAN_POINT('Ctrl Pts',(8.18044979104515,16.6666897480717,-329.08698287885)) ;
#42961 = CARTESIAN_POINT('Ctrl Pts',(8.2357903151535,16.6394129657847,-329.087780043204)) ;
#42962 = CARTESIAN_POINT('Ctrl Pts',(8.35545007685986,16.5796906765487,-329.089499641702)) ;
#42963 = CARTESIAN_POINT('Ctrl Pts',(8.41971851920079,16.5471456448645,-329.090420707702)) ;
#42964 = CARTESIAN_POINT('Ctrl Pts',(8.59963278005804,16.4547189241417,-329.09299416176)) ;
#42965 = CARTESIAN_POINT('Ctrl Pts',(8.71484042633788,16.3939932674618,-329.094636252659)) ;
#42966 = CARTESIAN_POINT('Ctrl Pts',(8.98435137553112,16.2482908982507,-329.098473780236)) ;
#42967 = CARTESIAN_POINT('Ctrl Pts',(9.13810320178457,16.1623202780274,-329.100660024386)) ;
#42968 = CARTESIAN_POINT('Ctrl Pts',(9.76896591725543,15.797692010374,-329.109657145919)) ;
#42969 = CARTESIAN_POINT('Ctrl Pts',(10.2347432684803,15.4999935391241,-329.116372281035)) ;
#42970 = CARTESIAN_POINT('Ctrl Pts',(10.9929088910055,14.9663225903865,-329.127799103793)) ;
#42971 = CARTESIAN_POINT('Ctrl Pts',(11.2926693610923,14.7414543228634,-329.132454969548)) ;
#42972 = CARTESIAN_POINT('Ctrl Pts',(11.7095960125738,14.4085083748425,-329.13918631324)) ;
#42973 = CARTESIAN_POINT('Ctrl Pts',(11.8324933234658,14.3077550305541,-329.141203265931)) ;
#42974 = CARTESIAN_POINT('Ctrl Pts',(12.0491469448274,14.1254378499473,-329.144820629031)) ;
#42975 = CARTESIAN_POINT('Ctrl Pts',(12.1434064800096,14.0444870166558,-329.146415818328)) ;
#42976 = CARTESIAN_POINT('Ctrl Pts',(12.3454699763002,13.8673981785719,-329.1498828556)) ;
#42977 = CARTESIAN_POINT('Ctrl Pts',(12.4529789662129,13.7709359146698,-329.151757431808)) ;
#42978 = CARTESIAN_POINT('Ctrl Pts',(12.7695739339482,13.4801320824121,-329.157367841748)) ;
#42979 = CARTESIAN_POINT('Ctrl Pts',(12.975314933628,13.282212964119,-329.161133860241)) ;
#42980 = CARTESIAN_POINT('Ctrl Pts',(13.4793091616763,12.7744895006594,-329.170651052562)) ;
#42981 = CARTESIAN_POINT('Ctrl Pts',(13.7715163973202,12.4589201957367,-329.176441162765)) ;
#42982 = CARTESIAN_POINT('Ctrl Pts',(14.3510761117434,11.7876983772191,-329.188386762579)) ;
#42983 = CARTESIAN_POINT('Ctrl Pts',(14.6367837320738,11.4310009021824,-329.1945385908)) ;
#42984 = CARTESIAN_POINT('Ctrl Pts',(14.9782260159731,10.9709034303299,-329.202082268983)) ;
#42985 = CARTESIAN_POINT('Ctrl Pts',(15.0465334193819,10.8770312487457,-329.203601530243)) ;
#42986 = CARTESIAN_POINT('Ctrl Pts',(15.1502571554111,10.7316408090449,-329.205920398291)) ;
#42987 = CARTESIAN_POINT('Ctrl Pts',(15.186301185109,10.6805740789779,-329.206728472808)) ;
#42988 = CARTESIAN_POINT('Ctrl Pts',(15.2626087439176,10.5712952550637,-329.208443205451)) ;
#42989 = CARTESIAN_POINT('Ctrl Pts',(15.3027986705916,10.5130329543827,-329.209348722788)) ;
#42990 = CARTESIAN_POINT('Ctrl Pts',(15.4123644716266,10.3522387090938,-329.211825935384)) ;
#42991 = CARTESIAN_POINT('Ctrl Pts',(15.4810495936202,10.2492403841038,-329.213388516475)) ;
#42992 = CARTESIAN_POINT('Ctrl Pts',(15.6383142709665,10.0082225836565,-329.216997455965)) ;
#42993 = CARTESIAN_POINT('Ctrl Pts',(15.7261055415446,9.8697009649993,-329.219036032986)) ;
#42994 = CARTESIAN_POINT('Ctrl Pts',(16.0572964014171,9.33149048201659,-329.226850446068)) ;
#42995 = CARTESIAN_POINT('Ctrl Pts',(16.2873872022798,8.92381653580239,-329.23255105411)) ;
#42996 = CARTESIAN_POINT('Ctrl Pts',(16.7140540836628,8.09625673332628,-329.243981840361)) ;
#42997 = CARTESIAN_POINT('Ctrl Pts',(16.910802054966,7.67683199633442,-329.249707312655)) ;
#42998 = CARTESIAN_POINT('Ctrl Pts',(17.1501885421993,7.11252366918415,-329.257429386254)) ;
#42999 = CARTESIAN_POINT('Ctrl Pts',(17.2070433723845,6.97385247009293,-329.259327983806)) ;
#43000 = CARTESIAN_POINT('Ctrl Pts',(17.3087674904143,6.71692346791216,-329.262850100218)) ;
#43001 = CARTESIAN_POINT('Ctrl Pts',(17.354119337829,6.59886618032869,-329.264470173927)) ;
#43002 = CARTESIAN_POINT('Ctrl Pts',(17.445462819266,6.35362995455593,-329.267839930924)) ;
#43003 = CARTESIAN_POINT('Ctrl Pts',(17.4912782154418,6.22639324986314,-329.269590718873)) ;
#43004 = CARTESIAN_POINT('Ctrl Pts',(17.6111456056611,5.88173459720228,-329.274340204026)) ;
#43005 = CARTESIAN_POINT('Ctrl Pts',(17.6825596771967,5.66342073081232,-329.277356230039)) ;
#43006 = CARTESIAN_POINT('Ctrl Pts',(17.7969144682316,5.29056127808998,-329.282516327658)) ;
#43007 = CARTESIAN_POINT('Ctrl Pts',(17.8419366818134,5.13668167059828,-329.284648400138)) ;
#43008 = CARTESIAN_POINT('Ctrl Pts',(18.042799180619,4.41563673193793,-329.29464188041)) ;
#43009 = CARTESIAN_POINT('Ctrl Pts',(18.1736234602727,3.84185607541159,-329.302614709956)) ;
#43010 = CARTESIAN_POINT('Ctrl Pts',(18.3199072260667,3.02243807143412,-329.3137642967)) ;
#43011 = CARTESIAN_POINT('Ctrl Pts',(18.3580764716915,2.78121579374912,-329.317016213756)) ;
#43012 = CARTESIAN_POINT('Ctrl Pts',(18.4063010161381,2.43193968077421,-329.32165132707)) ;
#43013 = CARTESIAN_POINT('Ctrl Pts',(18.4201852004245,2.32444078064242,-329.32306785437)) ;
#43014 = CARTESIAN_POINT('Ctrl Pts',(18.4411578397834,2.15005124098106,-329.325346212118)) ;
#43015 = CARTESIAN_POINT('Ctrl Pts',(18.4488255373903,2.0832328580525,-329.326214500059)) ;
#43016 = CARTESIAN_POINT('Ctrl Pts',(18.4643232872109,1.94137997269128,-329.328046987204)) ;
#43017 = CARTESIAN_POINT('Ctrl Pts',(18.4720594048526,1.86633652293836,-329.329010144397)) ;
#43018 = CARTESIAN_POINT('Ctrl Pts',(18.4936505815662,1.64359201073278,-329.331852937352)) ;
#43019 = CARTESIAN_POINT('Ctrl Pts',(18.5061930156225,1.49576960810489,-329.333718644129)) ;
#43020 = CARTESIAN_POINT('Ctrl Pts',(18.5324048286394,1.13565786237487,-329.338227834286)) ;
#43021 = CARTESIAN_POINT('Ctrl Pts',(18.5441999416556,0.923253083740634,-329.340857311212)) ;
#43022 = CARTESIAN_POINT('Ctrl Pts',(18.5727651835436,0.177568840775042,-329.350039598519)) ;
#43023 = CARTESIAN_POINT('Ctrl Pts',(18.5701969915469,-0.356150271044903,
-329.35653102772)) ;
#43024 = CARTESIAN_POINT('Ctrl Pts',(18.5446545934183,-0.888979984762296,
-329.363119887734)) ;
#43025 = CARTESIAN_POINT('Origin',(0.,0.,-315.477129595899)) ;
#43026 = CARTESIAN_POINT('',(18.5446545937517,-0.888979977808743,-331.160160528407)) ;
#43027 = CARTESIAN_POINT('',(18.544654593742,-0.888979978010901,-330.86430516735)) ;
#43028 = CARTESIAN_POINT('',(18.544654593745,-0.888979977948782,-315.477129595899)) ;
#43029 = CARTESIAN_POINT('',(4.76165266723923E-5,-18.5659499999389,-330.021951923812)) ;
#43030 = CARTESIAN_POINT('Ctrl Pts',(18.5446545937584,-0.888979977668659,
-331.160160528407)) ;
#43031 = CARTESIAN_POINT('Ctrl Pts',(18.5481227871158,-0.8166313877202,-331.15924327645)) ;
#43032 = CARTESIAN_POINT('Ctrl Pts',(18.5511676134064,-0.744262185559457,
-331.158323422676)) ;
#43033 = CARTESIAN_POINT('Ctrl Pts',(18.558360962383,-0.545618593590704,-331.155791736724)) ;
#43034 = CARTESIAN_POINT('Ctrl Pts',(18.5616441554253,-0.419317843523367,
-331.154174480573)) ;
#43035 = CARTESIAN_POINT('Ctrl Pts',(18.5657321922503,-0.160305871188285,
-331.150841361856)) ;
#43036 = CARTESIAN_POINT('Ctrl Pts',(18.566403744436,-0.0275996911559258,
-331.149124728823)) ;
#43037 = CARTESIAN_POINT('Ctrl Pts',(18.5644336733073,0.320401348695704,-331.144599380799)) ;
#43038 = CARTESIAN_POINT('Ctrl Pts',(18.5594698156593,0.5356627145399,-331.141776171986)) ;
#43039 = CARTESIAN_POINT('Ctrl Pts',(18.5397085601776,1.02393110241196,-331.135321592516)) ;
#43040 = CARTESIAN_POINT('Ctrl Pts',(18.5226226293287,1.29679563580841,-331.131678167029)) ;
#43041 = CARTESIAN_POINT('Ctrl Pts',(18.4698853880767,1.91852915750099,-331.123315926543)) ;
#43042 = CARTESIAN_POINT('Ctrl Pts',(18.4303631454727,2.26696589651703,-331.118585200598)) ;
#43043 = CARTESIAN_POINT('Ctrl Pts',(18.3676904974804,2.70765197174233,-331.112593889649)) ;
#43044 = CARTESIAN_POINT('Ctrl Pts',(18.3536677345799,2.8011272923186,-331.111322693582)) ;
#43045 = CARTESIAN_POINT('Ctrl Pts',(18.2887605515523,3.2123665089465,-331.105732855716)) ;
#43046 = CARTESIAN_POINT('Ctrl Pts',(18.2303329455754,3.52888403516724,-331.101436761758)) ;
#43047 = CARTESIAN_POINT('Ctrl Pts',(18.1434367596884,3.93951637247554,-331.095932209225)) ;
#43048 = CARTESIAN_POINT('Ctrl Pts',(18.1224078808916,4.03514799492262,-331.094655267207)) ;
#43049 = CARTESIAN_POINT('Ctrl Pts',(18.0858508053869,4.19534371405165,-331.092527202141)) ;
#43050 = CARTESIAN_POINT('Ctrl Pts',(18.0707309758703,4.25999885758617,-331.091671404628)) ;
#43051 = CARTESIAN_POINT('Ctrl Pts',(18.0365054747331,4.40289173015556,-331.089787417524)) ;
#43052 = CARTESIAN_POINT('Ctrl Pts',(18.0172369557155,4.48108891154186,-331.08876109764)) ;
#43053 = CARTESIAN_POINT('Ctrl Pts',(17.9536095144795,4.73226078727507,-331.085476283827)) ;
#43054 = CARTESIAN_POINT('Ctrl Pts',(17.907263607486,4.90472191333748,-331.083238772763)) ;
#43055 = CARTESIAN_POINT('Ctrl Pts',(17.7810499760305,5.34872538204143,-331.077497645468)) ;
#43056 = CARTESIAN_POINT('Ctrl Pts',(17.6974479174435,5.61915821806239,-331.074019376348)) ;
#43057 = CARTESIAN_POINT('Ctrl Pts',(17.3823049679693,6.56164169255582,-331.061836096526)) ;
#43058 = CARTESIAN_POINT('Ctrl Pts',(17.1183917639599,7.22221092963999,-331.053163563286)) ;
#43059 = CARTESIAN_POINT('Ctrl Pts',(16.7514236715618,8.00677534518241,-331.042264547455)) ;
#43060 = CARTESIAN_POINT('Ctrl Pts',(16.683822211145,8.14670011640386,-331.040297880446)) ;
#43061 = CARTESIAN_POINT('Ctrl Pts',(16.5580696337901,8.39885716748686,-331.036709143154)) ;
#43062 = CARTESIAN_POINT('Ctrl Pts',(16.5005137505024,8.51137577795021,-331.035091395404)) ;
#43063 = CARTESIAN_POINT('Ctrl Pts',(16.3802080948564,8.74075938453084,-331.031758687381)) ;
#43064 = CARTESIAN_POINT('Ctrl Pts',(16.3173457164775,8.85755725670296,-331.030042971464)) ;
#43065 = CARTESIAN_POINT('Ctrl Pts',(16.1493586234133,9.1618177944381,-331.025523620874)) ;
#43066 = CARTESIAN_POINT('Ctrl Pts',(16.0422210325689,9.34814598392815,-331.022705565621)) ;
#43067 = CARTESIAN_POINT('Ctrl Pts',(15.7918845169414,9.76653565176752,-331.016265880712)) ;
#43068 = CARTESIAN_POINT('Ctrl Pts',(15.6467596053445,9.99738709261697,-331.012632285647)) ;
#43069 = CARTESIAN_POINT('Ctrl Pts',(15.3029980488245,10.5183805756114,-331.004267580816)) ;
#43070 = CARTESIAN_POINT('Ctrl Pts',(15.1010977328267,10.8062447754485,-330.999524212466)) ;
#43071 = CARTESIAN_POINT('Ctrl Pts',(14.8301535264014,11.1701152944837,-330.993417828854)) ;
#43072 = CARTESIAN_POINT('Ctrl Pts',(14.768485087998,11.2515233423899,-330.992044398152)) ;
#43073 = CARTESIAN_POINT('Ctrl Pts',(14.5129480704408,11.5831352791013,-330.986424909322)) ;
#43074 = CARTESIAN_POINT('Ctrl Pts',(14.3133677336897,11.82887101243,-330.982201151328)) ;
#43075 = CARTESIAN_POINT('Ctrl Pts',(14.0444958234674,12.1431486907464,-330.976778100764)) ;
#43076 = CARTESIAN_POINT('Ctrl Pts',(13.9808111620209,12.2164169195587,-330.975512336279)) ;
#43077 = CARTESIAN_POINT('Ctrl Pts',(13.8726664350371,12.3388825131193,-330.973396659304)) ;
#43078 = CARTESIAN_POINT('Ctrl Pts',(13.8285121955437,12.3883471933111,-330.972542206843)) ;
#43079 = CARTESIAN_POINT('Ctrl Pts',(13.7298114853869,12.497733460438,-330.970653355)) ;
#43080 = CARTESIAN_POINT('Ctrl Pts',(13.6751359040282,12.5575365061447,-330.969620911739)) ;
#43081 = CARTESIAN_POINT('Ctrl Pts',(13.4965550335862,12.7503151345888,-330.966290078243)) ;
#43082 = CARTESIAN_POINT('Ctrl Pts',(13.3710880204971,12.8818298064171,-330.964013486387)) ;
#43083 = CARTESIAN_POINT('Ctrl Pts',(13.0395948188231,13.2192394990963,-330.958132687744)) ;
#43084 = CARTESIAN_POINT('Ctrl Pts',(12.8306187566375,13.4221663202339,-330.954555309347)) ;
#43085 = CARTESIAN_POINT('Ctrl Pts',(12.110658413272,14.0891006456218,-330.942526560241)) ;
#43086 = CARTESIAN_POINT('Ctrl Pts',(11.5786033490314,14.5295130016241,-330.934099782661)) ;
#43087 = CARTESIAN_POINT('Ctrl Pts',(10.88187683553,15.043607686256,-330.923210606501)) ;
#43088 = CARTESIAN_POINT('Ctrl Pts',(10.739010985984,15.1459241576935,-330.920986416848)) ;
#43089 = CARTESIAN_POINT('Ctrl Pts',(10.4911360566456,15.3181745940061,-330.917138160645)) ;
#43090 = CARTESIAN_POINT('Ctrl Pts',(10.3868269519003,15.3890946604943,-330.915521982655)) ;
#43091 = CARTESIAN_POINT('Ctrl Pts',(10.1685346175898,15.53428171424,-330.912145433226)) ;
#43092 = CARTESIAN_POINT('Ctrl Pts',(10.054441419404,15.6083699444631,-330.910383799769)) ;
#43093 = CARTESIAN_POINT('Ctrl Pts',(9.74165779318092,15.8066281923907,-330.905562511127)) ;
#43094 = CARTESIAN_POINT('Ctrl Pts',(9.5414149554891,15.9283015948812,-330.902484577182)) ;
#43095 = CARTESIAN_POINT('Ctrl Pts',(9.07062412638347,16.2023036967203,-330.895273673872)) ;
#43096 = CARTESIAN_POINT('Ctrl Pts',(8.79845109259639,16.3517009799672,-330.891123625488)) ;
#43097 = CARTESIAN_POINT('Ctrl Pts',(8.15395552397445,16.6847159826388,-330.88137809388)) ;
#43098 = CARTESIAN_POINT('Ctrl Pts',(7.77896601033168,16.8628119159217,-330.875768151297)) ;
#43099 = CARTESIAN_POINT('Ctrl Pts',(7.13421472922153,17.14294025996,-330.86634533474)) ;
#43100 = CARTESIAN_POINT('Ctrl Pts',(6.86747076873449,17.2515293928735,-330.862510163059)) ;
#43101 = CARTESIAN_POINT('Ctrl Pts',(6.51851579755499,17.3842094617561,-330.857618278281)) ;
#43102 = CARTESIAN_POINT('Ctrl Pts',(6.43851423539279,17.413997854622,-330.856505231405)) ;
#43103 = CARTESIAN_POINT('Ctrl Pts',(6.29535314917866,17.4661821340035,-330.854530346371)) ;
#43104 = CARTESIAN_POINT('Ctrl Pts',(6.23227244016171,17.4887898347052,-330.853666024741)) ;
#43105 = CARTESIAN_POINT('Ctrl Pts',(6.09537792271287,17.537017191739,-330.851803751006)) ;
#43106 = CARTESIAN_POINT('Ctrl Pts',(6.02152211482329,17.5625133579141,-330.850807237702)) ;
#43107 = CARTESIAN_POINT('Ctrl Pts',(5.79237513587827,17.6400030567689,-330.847737833842)) ;
#43108 = CARTESIAN_POINT('Ctrl Pts',(5.63655520357092,17.6904087898536,-330.845682314259)) ;
#43109 = CARTESIAN_POINT('Ctrl Pts',(4.99743586894677,17.8878540050492,-330.83734675238)) ;
#43110 = CARTESIAN_POINT('Ctrl Pts',(4.50889759314673,18.0172009728816,-330.831190943995)) ;
#43111 = CARTESIAN_POINT('Ctrl Pts',(3.5037655121286,18.239875513533,-330.818569888844)) ;
#43112 = CARTESIAN_POINT('Ctrl Pts',(2.98726399128732,18.3315488636272,-330.812106284076)) ;
#43113 = CARTESIAN_POINT('Ctrl Pts',(2.31869805305841,18.4212025245819,-330.80360924413)) ;
#43114 = CARTESIAN_POINT('Ctrl Pts',(2.16958182819799,18.4393594715001,-330.801706411908)) ;
#43115 = CARTESIAN_POINT('Ctrl Pts',(1.89447760420637,18.4694738764635,-330.798179194162)) ;
#43116 = CARTESIAN_POINT('Ctrl Pts',(1.76855599578412,18.4819566145575,-330.796558297825)) ;
#43117 = CARTESIAN_POINT('Ctrl Pts',(1.5079741875116,18.5051008575434,-330.793189818168)) ;
#43118 = CARTESIAN_POINT('Ctrl Pts',(1.37330536849315,18.5155819837578,-330.791441161656)) ;
#43119 = CARTESIAN_POINT('Ctrl Pts',(1.01026884317501,18.5398542148108,-330.786705741932)) ;
#43120 = CARTESIAN_POINT('Ctrl Pts',(0.781741177960401,18.5508953388265,-330.783701833575)) ;
#43121 = CARTESIAN_POINT('Ctrl Pts',(0.393762692635999,18.5624581118883,-330.77856674986)) ;
#43122 = CARTESIAN_POINT('Ctrl Pts',(0.234402720213039,18.5651543353626,-330.776447541044)) ;
#43123 = CARTESIAN_POINT('Ctrl Pts',(-0.505578151244105,18.5681447403556,
-330.766568940198)) ;
#43124 = CARTESIAN_POINT('Ctrl Pts',(-1.08597317809753,18.5432539875002,-330.758700760651)) ;
#43125 = CARTESIAN_POINT('Ctrl Pts',(-1.94616852480889,18.4658347306011,-330.747126442984)) ;
#43126 = CARTESIAN_POINT('Ctrl Pts',(-2.22747569809587,18.4340168386924,-330.743357457767)) ;
#43127 = CARTESIAN_POINT('Ctrl Pts',(-2.59258420454397,18.3842406262605,-330.738528940324)) ;
#43128 = CARTESIAN_POINT('Ctrl Pts',(-2.67714234873171,18.3721176006886,-330.737415156243)) ;
#43129 = CARTESIAN_POINT('Ctrl Pts',(-2.82788844212664,18.3494424454694,-330.735439387527)) ;
#43130 = CARTESIAN_POINT('Ctrl Pts',(-2.89410860984592,18.3391146595194,-330.734574912243)) ;
#43131 = CARTESIAN_POINT('Ctrl Pts',(-3.0373689639651,18.3159763113108,-330.73271293137)) ;
#43132 = CARTESIAN_POINT('Ctrl Pts',(-3.11438704382568,18.3030377758217,-330.731716858073)) ;
#43133 = CARTESIAN_POINT('Ctrl Pts',(-3.35243871359538,18.2615005751385,-330.728650535774)) ;
#43134 = CARTESIAN_POINT('Ctrl Pts',(-3.51317791850914,18.2312596836872,-330.726597608503)) ;
#43135 = CARTESIAN_POINT('Ctrl Pts',(-4.16834361696844,18.0990127242423,-330.71826858247)) ;
#43136 = CARTESIAN_POINT('Ctrl Pts',(-4.65891161228077,17.9789848134266,-330.712116695807)) ;
#43137 = CARTESIAN_POINT('Ctrl Pts',(-5.60631444422846,17.705797534222,-330.700029043485)) ;
#43138 = CARTESIAN_POINT('Ctrl Pts',(-6.0632929631573,17.5545579600269,-330.69410133502)) ;
#43139 = CARTESIAN_POINT('Ctrl Pts',(-6.68754920369072,17.3206691725551,-330.68573120314)) ;
#43140 = CARTESIAN_POINT('Ctrl Pts',(-6.86023510701914,17.2530017405025,-330.683386882274)) ;
#43141 = CARTESIAN_POINT('Ctrl Pts',(-7.1488047929945,17.1349073837524,-330.679415643943)) ;
#43142 = CARTESIAN_POINT('Ctrl Pts',(-7.26524002350625,17.0858639923686,-330.677798399152)) ;
#43143 = CARTESIAN_POINT('Ctrl Pts',(-7.50293288297232,16.982876916992,-330.674465270829)) ;
#43144 = CARTESIAN_POINT('Ctrl Pts',(-7.62413098073381,16.9288138081309,-330.672748616487)) ;
#43145 = CARTESIAN_POINT('Ctrl Pts',(-7.94042244954395,16.7836393492035,-330.668223129106)) ;
#43146 = CARTESIAN_POINT('Ctrl Pts',(-8.13452843294813,16.6904255608455,-330.665399800544)) ;
#43147 = CARTESIAN_POINT('Ctrl Pts',(-8.5713127002809,16.4712427019942,-330.6589448748)) ;
#43148 = CARTESIAN_POINT('Ctrl Pts',(-8.81291808194992,16.3432466794557,-330.655301220707)) ;
#43149 = CARTESIAN_POINT('Ctrl Pts',(-9.35769946137628,16.0390419219058,-330.646939039377)) ;
#43150 = CARTESIAN_POINT('Ctrl Pts',(-9.65888775124047,15.8594858701113,-330.642208609274)) ;
#43151 = CARTESIAN_POINT('Ctrl Pts',(-10.0345449264861,15.6208620217748,-330.636218394612)) ;
#43152 = CARTESIAN_POINT('Ctrl Pts',(-10.1138912993197,15.5696058067745,-330.634947997204)) ;
#43153 = CARTESIAN_POINT('Ctrl Pts',(-10.4618678354267,15.3410371631397,-330.629358139101)) ;
#43154 = CARTESIAN_POINT('Ctrl Pts',(-10.7262523806301,15.1573615927871,-330.625061231587)) ;
#43155 = CARTESIAN_POINT('Ctrl Pts',(-11.0646575803404,14.9089717355814,-330.619555972283)) ;
#43156 = CARTESIAN_POINT('Ctrl Pts',(-11.1431273433813,14.8504140895884,-330.618279106394)) ;
#43157 = CARTESIAN_POINT('Ctrl Pts',(-11.2740289729751,14.7511077164518,-330.616151125927)) ;
#43158 = CARTESIAN_POINT('Ctrl Pts',(-11.3267119954395,14.7106935102792,-330.6152953378)) ;
#43159 = CARTESIAN_POINT('Ctrl Pts',(-11.4428152845252,14.6206348775338,-330.613411318656)) ;
#43160 = CARTESIAN_POINT('Ctrl Pts',(-11.506131481596,14.5708587327633,-330.612384957924)) ;
#43161 = CARTESIAN_POINT('Ctrl Pts',(-11.7088004846587,14.4093853266332,-330.609099839252)) ;
#43162 = CARTESIAN_POINT('Ctrl Pts',(-11.8468663500648,14.2960887015532,-330.606862069528)) ;
#43163 = CARTESIAN_POINT('Ctrl Pts',(-12.1994926333109,13.998107423612,-330.601120024997)) ;
#43164 = CARTESIAN_POINT('Ctrl Pts',(-12.4115023274802,13.8104758185935,-330.597641106901)) ;
#43165 = CARTESIAN_POINT('Ctrl Pts',(-13.1403739580981,13.1350693645033,-330.585458849114)) ;
#43166 = CARTESIAN_POINT('Ctrl Pts',(-13.6334491296713,12.6225409245384,-330.576787931616)) ;
#43167 = CARTESIAN_POINT('Ctrl Pts',(-14.1970743797401,11.9650211676568,-330.565890419424)) ;
#43168 = CARTESIAN_POINT('Ctrl Pts',(-14.2967337182456,11.8457611567692,-330.563923513226)) ;
#43169 = CARTESIAN_POINT('Ctrl Pts',(-14.4747024500922,11.6272723275276,-330.560334483434)) ;
#43170 = CARTESIAN_POINT('Ctrl Pts',(-14.5535182835272,11.5284681686224,-330.558716684917)) ;
#43171 = CARTESIAN_POINT('Ctrl Pts',(-14.7129634481555,11.3243453046729,-330.555384018751)) ;
#43172 = CARTESIAN_POINT('Ctrl Pts',(-14.7934854104544,11.2189517939363,-330.553668396983)) ;
#43173 = CARTESIAN_POINT('Ctrl Pts',(-15.0014874186071,10.9405688843869,-330.549149662067)) ;
#43174 = CARTESIAN_POINT('Ctrl Pts',(-15.1271054431131,10.7662134915783,-330.546332135851)) ;
#43175 = CARTESIAN_POINT('Ctrl Pts',(-15.4051392015674,10.3658323904254,-330.539893979086)) ;
#43176 = CARTESIAN_POINT('Ctrl Pts',(-15.5556604518152,10.1385513002385,-330.536261392284)) ;
#43177 = CARTESIAN_POINT('Ctrl Pts',(-15.8887788265828,9.61066354740706,-330.527896443821)) ;
#43178 = CARTESIAN_POINT('Ctrl Pts',(-16.0679484860358,9.30801684241158,-330.523151787894)) ;
#43179 = CARTESIAN_POINT('Ctrl Pts',(-16.4345551275127,8.6465942956125,-330.512972881649)) ;
#43180 = CARTESIAN_POINT('Ctrl Pts',(-16.6190757736095,8.28640553254775,-330.50754460659)) ;
#43181 = CARTESIAN_POINT('Ctrl Pts',(-16.8359631109392,7.82659694602327,-330.500867992627)) ;
#43182 = CARTESIAN_POINT('Ctrl Pts',(-16.8794570831303,7.73234778411225,-330.499512656652)) ;
#43183 = CARTESIAN_POINT('Ctrl Pts',(-16.9495285523412,7.57709757966394,-330.497304656267)) ;
#43184 = CARTESIAN_POINT('Ctrl Pts',(-16.976572543636,7.51630963893987,-330.496446285057)) ;
#43185 = CARTESIAN_POINT('Ctrl Pts',(-17.0343102757226,7.3846286654148,-330.49460094204)) ;
#43186 = CARTESIAN_POINT('Ctrl Pts',(-17.0648894297572,7.31368688606125,-330.493615351778)) ;
#43187 = CARTESIAN_POINT('Ctrl Pts',(-17.1568918581588,7.09652822671324,-330.490621677507)) ;
#43188 = CARTESIAN_POINT('Ctrl Pts',(-17.216885234924,6.94971323560982,-330.488629773962)) ;
#43189 = CARTESIAN_POINT('Ctrl Pts',(-17.320615197322,6.68627671113947,-330.485099226433)) ;
#43190 = CARTESIAN_POINT('Ctrl Pts',(-17.3650732086083,6.56994973935645,-330.483555222653)) ;
#43191 = CARTESIAN_POINT('Ctrl Pts',(-17.5921832066087,5.95728908999621,-330.475484419714)) ;
#43192 = CARTESIAN_POINT('Ctrl Pts',(-17.7547359256516,5.45376538662723,-330.469052942221)) ;
#43193 = CARTESIAN_POINT('Ctrl Pts',(-17.9615360641349,4.7052188834405,-330.459493536434)) ;
#43194 = CARTESIAN_POINT('Ctrl Pts',(-18.0227157703569,4.4651515706854,-330.456429312891)) ;
#43195 = CARTESIAN_POINT('Ctrl Pts',(-18.1321167239935,3.99689883884166,-330.450430420117)) ;
#43196 = CARTESIAN_POINT('Ctrl Pts',(-18.180878700416,3.76888665422343,-330.44749929868)) ;
#43197 = CARTESIAN_POINT('Ctrl Pts',(-18.2512334933319,3.40667383168276,-330.442816414543)) ;
#43198 = CARTESIAN_POINT('Ctrl Pts',(-18.2756693639819,3.27305054294396,-330.441083248898)) ;
#43199 = CARTESIAN_POINT('Ctrl Pts',(-18.3199766457208,3.01477764874225,-330.437721076734)) ;
#43200 = CARTESIAN_POINT('Ctrl Pts',(-18.3400476331296,2.89016977562543,-330.436093483044)) ;
#43201 = CARTESIAN_POINT('Ctrl Pts',(-18.385101952996,2.59106107712134,-330.43217295651)) ;
#43202 = CARTESIAN_POINT('Ctrl Pts',(-18.4088736582348,2.41639024584107,-330.429872336945)) ;
#43203 = CARTESIAN_POINT('Ctrl Pts',(-18.4549308116001,2.03768160184106,-330.424861169367)) ;
#43204 = CARTESIAN_POINT('Ctrl Pts',(-18.4763275208731,1.83355902970655,-330.422145656844)) ;
#43205 = CARTESIAN_POINT('Ctrl Pts',(-18.5332057502782,1.18785921698701,-330.41351900801)) ;
#43206 = CARTESIAN_POINT('Ctrl Pts',(-18.556270749547,0.745345250572032,-330.407549723034)) ;
#43207 = CARTESIAN_POINT('Ctrl Pts',(-18.5661659217633,0.137972571028798,
-330.39936793353)) ;
#43208 = CARTESIAN_POINT('Ctrl Pts',(-18.5666596468405,-0.0265151922384639,
-330.39715378097)) ;
#43209 = CARTESIAN_POINT('Ctrl Pts',(-18.5617637765965,-0.502418275354446,
-330.390766967386)) ;
#43210 = CARTESIAN_POINT('Ctrl Pts',(-18.5507239721748,-0.813719501713166,
-330.386612423732)) ;
#43211 = CARTESIAN_POINT('Ctrl Pts',(-18.5260150512544,-1.22089003075575,
-330.381264624084)) ;
#43212 = CARTESIAN_POINT('Ctrl Pts',(-18.519421025374,-1.31713745310965,-330.380006904576)) ;
#43213 = CARTESIAN_POINT('Ctrl Pts',(-18.5070346377355,-1.47937691227361,
-330.377900100957)) ;
#43214 = CARTESIAN_POINT('Ctrl Pts',(-18.5016387044778,-1.54539716995087,
-330.377046573637)) ;
#43215 = CARTESIAN_POINT('Ctrl Pts',(-18.4888248747068,-1.69247737064019,
-330.375154013099)) ;
#43216 = CARTESIAN_POINT('Ctrl Pts',(-18.4812269988148,-1.77352009874664,
-330.374117000095)) ;
#43217 = CARTESIAN_POINT('Ctrl Pts',(-18.4547007146308,-2.03775298220845,
-330.370751393486)) ;
#43218 = CARTESIAN_POINT('Ctrl Pts',(-18.43357950976,-2.22071212794997,-330.36844522484)) ;
#43219 = CARTESIAN_POINT('Ctrl Pts',(-18.3712162345436,-2.69842144769139,
-330.362457231648)) ;
#43220 = CARTESIAN_POINT('Ctrl Pts',(-18.3256029734356,-2.99254746964278,
-330.358803398109)) ;
#43221 = CARTESIAN_POINT('Ctrl Pts',(-18.152853151092,-3.95334343820715,-330.346840201097)) ;
#43222 = CARTESIAN_POINT('Ctrl Pts',(-17.9962387990633,-4.6141510789431,-330.338550169864)) ;
#43223 = CARTESIAN_POINT('Ctrl Pts',(-17.7537576672823,-5.43412654378801,
-330.327798057687)) ;
#43224 = CARTESIAN_POINT('Ctrl Pts',(-17.7013031497934,-5.60263413637229,
-330.325564522393)) ;
#43225 = CARTESIAN_POINT('Ctrl Pts',(-17.6072185883051,-5.89035562974297,
-330.321705540435)) ;
#43226 = CARTESIAN_POINT('Ctrl Pts',(-17.5667600813921,-6.00993977097595,
-330.320088106029)) ;
#43227 = CARTESIAN_POINT('Ctrl Pts',(-17.4802659474733,-6.25725448271785,
-330.316713889588)) ;
#43228 = CARTESIAN_POINT('Ctrl Pts',(-17.4340424561258,-6.3849114972118,-330.314955897886)) ;
#43229 = CARTESIAN_POINT('Ctrl Pts',(-17.3047896226676,-6.73000167159116,
-330.310158767569)) ;
#43230 = CARTESIAN_POINT('Ctrl Pts',(-17.2190653054668,-6.94639878461507,
-330.307101672136)) ;
#43231 = CARTESIAN_POINT('Ctrl Pts',(-17.0662084342514,-7.31202987185582,
-330.301856478411)) ;
#43232 = CARTESIAN_POINT('Ctrl Pts',(-17.0011300618483,-7.46209271586618,
-330.299680484895)) ;
#43233 = CARTESIAN_POINT('Ctrl Pts',(-16.6818399371303,-8.17247081362076,
-330.289277685478)) ;
#43234 = CARTESIAN_POINT('Ctrl Pts',(-16.4018621393915,-8.72077856422216,
-330.280929701705)) ;
#43235 = CARTESIAN_POINT('Ctrl Pts',(-16.0733130669516,-9.29220270212986,
-330.272116864638)) ;
#43236 = CARTESIAN_POINT('Ctrl Pts',(-16.0513112420454,-9.33015709506135,
-330.271531033282)) ;
#43237 = CARTESIAN_POINT('Ctrl Pts',(-15.9224575611999,-9.55063221266623,
-330.268125851353)) ;
#43238 = CARTESIAN_POINT('Ctrl Pts',(-15.8126274595549,-9.7313947390057,-330.265325370099)) ;
#43239 = CARTESIAN_POINT('Ctrl Pts',(-15.6538431031587,-9.98293976836074,
-330.261435821128)) ;
#43240 = CARTESIAN_POINT('Ctrl Pts',(-15.6074488623538,-10.055318510847,-330.26031757548)) ;
#43241 = CARTESIAN_POINT('Ctrl Pts',(-15.5246894087672,-10.1824771507967,
-330.258356467414)) ;
#43242 = CARTESIAN_POINT('Ctrl Pts',(-15.4885329145412,-10.2373907971327,
-330.257510857388)) ;
#43243 = CARTESIAN_POINT('Ctrl Pts',(-15.402977510373,-10.3658396011438,-330.255535795351)) ;
#43244 = CARTESIAN_POINT('Ctrl Pts',(-15.3533425793521,-10.439215415613,-330.254409568327)) ;
#43245 = CARTESIAN_POINT('Ctrl Pts',(-15.1679775989655,-10.7090605002199,
-330.250270245683)) ;
#43246 = CARTESIAN_POINT('Ctrl Pts',(-15.0289857881028,-10.9032613399288,
-330.247295892746)) ;
#43247 = CARTESIAN_POINT('Ctrl Pts',(-14.5998346278338,-11.4790724443462,
-330.238417635867)) ;
#43248 = CARTESIAN_POINT('Ctrl Pts',(-14.2986049567674,-11.8521800859017,
-330.232580318352)) ;
#43249 = CARTESIAN_POINT('Ctrl Pts',(-13.6866204068814,-12.5528596604249,
-330.221153965526)) ;
#43250 = CARTESIAN_POINT('Ctrl Pts',(-13.3776906313024,-12.8815859226233,
-330.215574760798)) ;
#43251 = CARTESIAN_POINT('Ctrl Pts',(-12.9408872331305,-13.3137019414541,
-330.207832918695)) ;
#43252 = CARTESIAN_POINT('Ctrl Pts',(-12.8231616266427,-13.4271273008815,
-330.20576051094)) ;
#43253 = CARTESIAN_POINT('Ctrl Pts',(-12.6128424213714,-13.6244748728398,
-330.202079650693)) ;
#43254 = CARTESIAN_POINT('Ctrl Pts',(-12.5208706443765,-13.7090447428699,
-330.200477086502)) ;
#43255 = CARTESIAN_POINT('Ctrl Pts',(-12.3415802175801,-13.8705964389887,
-330.197365757672)) ;
#43256 = CARTESIAN_POINT('Ctrl Pts',(-12.2543773493398,-13.9476981462261,
-330.195858143505)) ;
#43257 = CARTESIAN_POINT('Ctrl Pts',(-12.0613442653694,-14.1151633935476,
-330.192533040218)) ;
#43258 = CARTESIAN_POINT('Ctrl Pts',(-11.9552114711779,-14.2051674303664,
-330.19071268553)) ;
#43259 = CARTESIAN_POINT('Ctrl Pts',(-11.507816985023,-14.5760066319688,-330.183072911309)) ;
#43260 = CARTESIAN_POINT('Ctrl Pts',(-11.1575957720371,-14.8458033078795,
-330.177169594897)) ;
#43261 = CARTESIAN_POINT('Ctrl Pts',(-10.2802959771581,-15.4730464530979,
-330.162670534322)) ;
#43262 = CARTESIAN_POINT('Ctrl Pts',(-9.74381415641788,-15.8163756113584,
-330.154035235311)) ;
#43263 = CARTESIAN_POINT('Ctrl Pts',(-9.09445342691111,-16.1863430845461,
-330.14420122367)) ;
#43264 = CARTESIAN_POINT('Ctrl Pts',(-8.99765519925968,-16.2403505675189,
-330.142751260244)) ;
#43265 = CARTESIAN_POINT('Ctrl Pts',(-8.84060289792843,-16.3261409772042,
-330.140427907386)) ;
#43266 = CARTESIAN_POINT('Ctrl Pts',(-8.78064740648805,-16.3584647800832,
-330.139547754509)) ;
#43267 = CARTESIAN_POINT('Ctrl Pts',(-8.66699183473694,-16.4189350337465,
-330.137893068336)) ;
#43268 = CARTESIAN_POINT('Ctrl Pts',(-8.61332917160136,-16.4471497742988,
-330.137117508219)) ;
#43269 = CARTESIAN_POINT('Ctrl Pts',(-8.51851504977828,-16.4964098206519,
-330.135756444397)) ;
#43270 = CARTESIAN_POINT('Ctrl Pts',(-8.47742141704833,-16.5175652487354,
-330.135169581176)) ;
#43271 = CARTESIAN_POINT('Ctrl Pts',(-8.25302042359775,-16.6320311936333,
-330.131980365758)) ;
#43272 = CARTESIAN_POINT('Ctrl Pts',(-8.06825073589355,-16.7224441421848,
-330.129410400277)) ;
#43273 = CARTESIAN_POINT('Ctrl Pts',(-7.55652235598144,-16.9623910329631,
-330.122401888033)) ;
#43274 = CARTESIAN_POINT('Ctrl Pts',(-7.22666328815681,-17.1055277045896,
-330.118003464492)) ;
#43275 = CARTESIAN_POINT('Ctrl Pts',(-6.77224408864678,-17.2872231012085,
-330.112009214102)) ;
#43276 = CARTESIAN_POINT('Ctrl Pts',(-6.65112866273107,-17.334181839662,-330.110417930318)) ;
#43277 = CARTESIAN_POINT('Ctrl Pts',(-6.08298750655138,-17.5476296909381,
-330.102970501915)) ;
#43278 = CARTESIAN_POINT('Ctrl Pts',(-5.63014569610861,-17.6981214484734,
-330.097078592974)) ;
#43279 = CARTESIAN_POINT('Ctrl Pts',(-5.02651697669581,-17.8732083462247,
-330.089163627025)) ;
#43280 = CARTESIAN_POINT('Ctrl Pts',(-4.88051007119133,-17.9136280764974,
-330.087245015188)) ;
#43281 = CARTESIAN_POINT('Ctrl Pts',(-4.6126268096025,-17.9842691166204,-330.083714699708)) ;
#43282 = CARTESIAN_POINT('Ctrl Pts',(-4.49090713243562,-18.0150496757352,
-330.082106811078)) ;
#43283 = CARTESIAN_POINT('Ctrl Pts',(-4.25599254292782,-18.0719262563996,
-330.078995453635)) ;
#43284 = CARTESIAN_POINT('Ctrl Pts',(-4.14284643128943,-18.0981992073007,
-330.077493245856)) ;
#43285 = CARTESIAN_POINT('Ctrl Pts',(-3.89958097867066,-18.1522855413034,
-330.074255462553)) ;
#43286 = CARTESIAN_POINT('Ctrl Pts',(-3.76939409285071,-18.1797654081152,
-330.072517815642)) ;
#43287 = CARTESIAN_POINT('Ctrl Pts',(-3.44614278234465,-18.2443758006867,
-330.068191690622)) ;
#43288 = CARTESIAN_POINT('Ctrl Pts',(-3.25276274937905,-18.279843619488,-330.065593379781)) ;
#43289 = CARTESIAN_POINT('Ctrl Pts',(-2.59873184162833,-18.3890922535926,
-330.056779016735)) ;
#43290 = CARTESIAN_POINT('Ctrl Pts',(-2.1358748411174,-18.4485814695994,-330.05049265788)) ;
#43291 = CARTESIAN_POINT('Ctrl Pts',(-1.25835765446653,-18.5278958790408,
-330.038625383331)) ;
#43292 = CARTESIAN_POINT('Ctrl Pts',(-0.844309466275273,-18.5513754769053,
-330.033048159475)) ;
#43293 = CARTESIAN_POINT('Ctrl Pts',(-0.347385170617471,-18.5628829276712,
-330.026490566988)) ;
#43294 = CARTESIAN_POINT('Ctrl Pts',(-0.264935466496756,-18.5642427333547,
-330.025407121129)) ;
#43295 = CARTESIAN_POINT('Ctrl Pts',(-0.121638931265175,-18.5656512218572,
-330.023533604446)) ;
#43296 = CARTESIAN_POINT('Ctrl Pts',(-0.0607958602491681,-18.5659501559856,
-330.022741094051)) ;
#43297 = CARTESIAN_POINT('Ctrl Pts',(4.7616526672392E-5,-18.5659499999389,
-330.021951923812)) ;
#43298 = CARTESIAN_POINT('Ctrl Pts',(4.7616526672392E-5,-18.5659499999389,
-330.021951923812)) ;
#43299 = CARTESIAN_POINT('Ctrl Pts',(0.0581026652593616,-18.5659498510438,
-330.021198920875)) ;
#43300 = CARTESIAN_POINT('Ctrl Pts',(0.116157458008613,-18.5656773981162,
-330.020448967975)) ;
#43301 = CARTESIAN_POINT('Ctrl Pts',(0.238776255328645,-18.5645267771815,
-330.018872109095)) ;
#43302 = CARTESIAN_POINT('Ctrl Pts',(0.303338885232825,-18.5635840853691,
-330.018045992598)) ;
#43303 = CARTESIAN_POINT('Ctrl Pts',(0.482556376936524,-18.5600320868817,
-330.015762822773)) ;
#43304 = CARTESIAN_POINT('Ctrl Pts',(0.5971940506329,-18.5566972020742,-330.014313757867)) ;
#43305 = CARTESIAN_POINT('Ctrl Pts',(1.14093747068827,-18.5358354727858,-330.007480944841)) ;
#43306 = CARTESIAN_POINT('Ctrl Pts',(1.56938204509395,-18.5044853166008,-330.002213255011)) ;
#43307 = CARTESIAN_POINT('Ctrl Pts',(2.44542892588963,-18.4097366682375,-329.991418195119)) ;
#43308 = CARTESIAN_POINT('Ctrl Pts',(2.89258184393477,-18.3447948133597,-329.985894367478)) ;
#43309 = CARTESIAN_POINT('Ctrl Pts',(3.61850126273996,-18.2121630512013,-329.976739501948)) ;
#43310 = CARTESIAN_POINT('Ctrl Pts',(3.89885481970043,-18.1542106685303,-329.973158524709)) ;
#43311 = CARTESIAN_POINT('Ctrl Pts',(4.29470509939096,-18.0627908734934,-329.968016979546)) ;
#43312 = CARTESIAN_POINT('Ctrl Pts',(4.41138966644285,-18.0346485188035,-329.966490890444)) ;
#43313 = CARTESIAN_POINT('Ctrl Pts',(4.64822465796194,-17.9750918739856,-329.963370685704)) ;
#43314 = CARTESIAN_POINT('Ctrl Pts',(4.76834929538207,-17.9435995635043,-329.961776120625)) ;
#43315 = CARTESIAN_POINT('Ctrl Pts',(5.02813844237762,-17.8726992907168,-329.958300786899)) ;
#43316 = CARTESIAN_POINT('Ctrl Pts',(5.16767517679351,-17.8328542112097,-329.956417181022)) ;
#43317 = CARTESIAN_POINT('Ctrl Pts',(5.58452383535151,-17.7085185091262,-329.950739043784)) ;
#43318 = CARTESIAN_POINT('Ctrl Pts',(5.86033803906599,-17.6191648989292,-329.946913172611)) ;
#43319 = CARTESIAN_POINT('Ctrl Pts',(6.72237998229648,-17.3174128455323,-329.934758298425)) ;
#43320 = CARTESIAN_POINT('Ctrl Pts',(7.30006480442918,-17.0819270201348,-329.926308519757)) ;
#43321 = CARTESIAN_POINT('Ctrl Pts',(8.05186736080542,-16.7303489825553,-329.915177829223)) ;
#43322 = CARTESIAN_POINT('Ctrl Pts',(8.23745903168308,-16.6397540236598,-329.912420321007)) ;
#43323 = CARTESIAN_POINT('Ctrl Pts',(8.55107951538355,-16.4801298182743,-329.907764321705)) ;
#43324 = CARTESIAN_POINT('Ctrl Pts',(8.6798791879029,-16.4126578317965,-329.905853311936)) ;
#43325 = CARTESIAN_POINT('Ctrl Pts',(8.86300255001428,-16.3139696930125,-329.903144822235)) ;
#43326 = CARTESIAN_POINT('Ctrl Pts',(8.91798132454375,-16.2839807925675,-329.902332775988)) ;
#43327 = CARTESIAN_POINT('Ctrl Pts',(9.01563574848838,-16.2300710019763,-329.900893132544)) ;
#43328 = CARTESIAN_POINT('Ctrl Pts',(9.05837042646113,-16.206258602737,-329.900264126856)) ;
#43329 = CARTESIAN_POINT('Ctrl Pts',(9.17226394750052,-16.1422041985057,-329.898590273108)) ;
#43330 = CARTESIAN_POINT('Ctrl Pts',(9.24325189405584,-16.1016606831915,-329.897549499824)) ;
#43331 = CARTESIAN_POINT('Ctrl Pts',(9.46753213888617,-15.9715949959989,-329.894265852192)) ;
#43332 = CARTESIAN_POINT('Ctrl Pts',(9.61980960301441,-15.8803424053068,-329.892043158918)) ;
#43333 = CARTESIAN_POINT('Ctrl Pts',(10.3521323389,-15.4270971778075,-329.881337231818)) ;
#43334 = CARTESIAN_POINT('Ctrl Pts',(10.9131900849732,-15.0354334319154,-329.873063366174)) ;
#43335 = CARTESIAN_POINT('Ctrl Pts',(11.6438500729911,-14.4628854509154,-329.861603724857)) ;
#43336 = CARTESIAN_POINT('Ctrl Pts',(11.8333358846869,-14.3082655017375,-329.858567017114)) ;
#43337 = CARTESIAN_POINT('Ctrl Pts',(12.0306921794034,-14.1406206601484,-329.855322535427)) ;
#43338 = CARTESIAN_POINT('Ctrl Pts',(12.041661690836,-14.1312805751333,-329.855141929022)) ;
#43339 = CARTESIAN_POINT('Ctrl Pts',(12.0836251204874,-14.0954661102493,-329.854449981767)) ;
#43340 = CARTESIAN_POINT('Ctrl Pts',(12.1145426859745,-14.0689024598871,-329.853937986846)) ;
#43341 = CARTESIAN_POINT('Ctrl Pts',(12.1575910910589,-14.0316691538331,-329.853221990606)) ;
#43342 = CARTESIAN_POINT('Ctrl Pts',(12.1697958698784,-14.0210851529195,-329.853018645106)) ;
#43343 = CARTESIAN_POINT('Ctrl Pts',(12.2028188356677,-13.9923719908037,-329.852467486175)) ;
#43344 = CARTESIAN_POINT('Ctrl Pts',(12.2236104255492,-13.9742123079998,-329.852119436267)) ;
#43345 = CARTESIAN_POINT('Ctrl Pts',(12.2585847206205,-13.9435274616503,-329.851532203737)) ;
#43346 = CARTESIAN_POINT('Ctrl Pts',(12.2727889219539,-13.9310268646438,-329.85129321652)) ;
#43347 = CARTESIAN_POINT('Ctrl Pts',(12.2966591671877,-13.9099546955302,-329.850890761112)) ;
#43348 = CARTESIAN_POINT('Ctrl Pts',(12.3063354200097,-13.9013947082963,-329.850727386348)) ;
#43349 = CARTESIAN_POINT('Ctrl Pts',(12.3226114437513,-13.886965997204,-329.850452188024)) ;
#43350 = CARTESIAN_POINT('Ctrl Pts',(12.3292159764595,-13.8811026509773,-329.850340408218)) ;
#43351 = CARTESIAN_POINT('Ctrl Pts',(12.3403420934771,-13.871210945365,-329.850151917511)) ;
#43352 = CARTESIAN_POINT('Ctrl Pts',(12.3448658953132,-13.8671850821132,-329.850075227037)) ;
#43353 = CARTESIAN_POINT('Ctrl Pts',(12.352498368207,-13.8603860271048,-329.849945749256)) ;
#43354 = CARTESIAN_POINT('Ctrl Pts',(12.3556080771553,-13.8576140009978,-329.849892971526)) ;
#43355 = CARTESIAN_POINT('Ctrl Pts',(12.3682870472663,-13.8463041777819,-329.849677685319)) ;
#43356 = CARTESIAN_POINT('Ctrl Pts',(12.3778483932976,-13.837757514125,-329.849515103857)) ;
#43357 = CARTESIAN_POINT('Ctrl Pts',(12.3958108145418,-13.8216678128162,-329.849209232247)) ;
#43358 = CARTESIAN_POINT('Ctrl Pts',(12.4042138795492,-13.8141270049219,-329.84906596065)) ;
#43359 = CARTESIAN_POINT('Ctrl Pts',(12.4200538272188,-13.7998863229697,-329.848795548557)) ;
#43360 = CARTESIAN_POINT('Ctrl Pts',(12.4274921805692,-13.7931880904947,-329.848668421808)) ;
#43361 = CARTESIAN_POINT('Ctrl Pts',(12.44156817291,-13.7804920388692,-329.848427581942)) ;
#43362 = CARTESIAN_POINT('Ctrl Pts',(12.4482069009987,-13.7744954312095,-329.848313879026)) ;
#43363 = CARTESIAN_POINT('Ctrl Pts',(12.4608243461033,-13.7630818172029,-329.848097559047)) ;
#43364 = CARTESIAN_POINT('Ctrl Pts',(12.4668038715921,-13.7576657074776,-329.847994949569)) ;
#43365 = CARTESIAN_POINT('Ctrl Pts',(12.5589035044516,-13.6741347357994,-329.846413063903)) ;
#43366 = CARTESIAN_POINT('Ctrl Pts',(12.6442914143989,-13.5952165335229,-329.844926974883)) ;
#43367 = CARTESIAN_POINT('Ctrl Pts',(12.8209046404516,-13.4288817663955,-329.841811320343)) ;
#43368 = CARTESIAN_POINT('Ctrl Pts',(12.9119903220531,-13.3413255400172,-329.840180553971)) ;
#43369 = CARTESIAN_POINT('Ctrl Pts',(13.1345664331528,-13.1229593516729,-329.836135505242)) ;
#43370 = CARTESIAN_POINT('Ctrl Pts',(13.2650038142331,-12.9910958420024,-329.833711871784)) ;
#43371 = CARTESIAN_POINT('Ctrl Pts',(13.8012711460205,-12.4324664276529,-329.823525269086)) ;
#43372 = CARTESIAN_POINT('Ctrl Pts',(14.1886518877783,-11.9884688715057,-329.815609336336)) ;
#43373 = CARTESIAN_POINT('Ctrl Pts',(14.8664346895102,-11.1326729274872,-329.800903558876)) ;
#43374 = CARTESIAN_POINT('Ctrl Pts',(15.162494743099,-10.7259552186097,-329.794126680316)) ;
#43375 = CARTESIAN_POINT('Ctrl Pts',(15.4983300701611,-10.2228507244519,-329.786185897481)) ;
#43376 = CARTESIAN_POINT('Ctrl Pts',(15.5542824790199,-10.1375149078137,-329.784853978497)) ;
#43377 = CARTESIAN_POINT('Ctrl Pts',(15.6457670103106,-9.99544667370517,-329.782664115815)) ;
#43378 = CARTESIAN_POINT('Ctrl Pts',(15.6817008837568,-9.93897565042121,-329.781800834034)) ;
#43379 = CARTESIAN_POINT('Ctrl Pts',(15.759047724917,-9.81595931507566,-329.779936507707)) ;
#43380 = CARTESIAN_POINT('Ctrl Pts',(15.8003461959506,-9.7493437000599,-329.778936946909)) ;
#43381 = CARTESIAN_POINT('Ctrl Pts',(15.9273908721902,-9.54148938379758,-329.775846126354)) ;
#43382 = CARTESIAN_POINT('Ctrl Pts',(16.0116744449906,-9.39936600444508,-329.773772581667)) ;
#43383 = CARTESIAN_POINT('Ctrl Pts',(16.2439874308812,-8.99543324050806,-329.767967151885)) ;
#43384 = CARTESIAN_POINT('Ctrl Pts',(16.3875685923579,-8.73112495555433,-329.764270297603)) ;
#43385 = CARTESIAN_POINT('Ctrl Pts',(16.6855842090126,-8.14925691006487,-329.756255354711)) ;
#43386 = CARTESIAN_POINT('Ctrl Pts',(16.837509005625,-7.83054270386208,-329.751942058568)) ;
#43387 = CARTESIAN_POINT('Ctrl Pts',(17.0900461926661,-7.25937569696008,-329.744251505353)) ;
#43388 = CARTESIAN_POINT('Ctrl Pts',(17.1943769443528,-7.00868144164467,-329.740889332834)) ;
#43389 = CARTESIAN_POINT('Ctrl Pts',(17.3711546394092,-6.55617371373322,-329.734814665826)) ;
#43390 = CARTESIAN_POINT('Ctrl Pts',(17.4456748971035,-6.35522261017884,-329.732115110044)) ;
#43391 = CARTESIAN_POINT('Ctrl Pts',(17.5606215531586,-6.02798756042791,-329.727707933453)) ;
#43392 = CARTESIAN_POINT('Ctrl Pts',(17.6032034765254,-5.90248173779442,-329.726015070028)) ;
#43393 = CARTESIAN_POINT('Ctrl Pts',(17.683780503254,-5.65635886994195,-329.722689034744)) ;
#43394 = CARTESIAN_POINT('Ctrl Pts',(17.7218943056158,-5.53578817508473,-329.721056777729)) ;
#43395 = CARTESIAN_POINT('Ctrl Pts',(17.8041825674143,-5.26591146070652,-329.717396328597)) ;
#43396 = CARTESIAN_POINT('Ctrl Pts',(17.847716531822,-5.11642012616933,-329.715364004563)) ;
#43397 = CARTESIAN_POINT('Ctrl Pts',(18.0789428804612,-4.28352440615334,-329.704016506059)) ;
#43398 = CARTESIAN_POINT('Ctrl Pts',(18.2292645469026,-3.59035695091203,-329.694456307325)) ;
#43399 = CARTESIAN_POINT('Ctrl Pts',(18.3837779290755,-2.60993597128431,-329.681095997685)) ;
#43400 = CARTESIAN_POINT('Ctrl Pts',(18.4215284173503,-2.32859352472789,-329.677284112108)) ;
#43401 = CARTESIAN_POINT('Ctrl Pts',(18.4725323277506,-1.8687023086486,-329.671135910529)) ;
#43402 = CARTESIAN_POINT('Ctrl Pts',(18.4896798658008,-1.69063229974774,-329.668775609301)) ;
#43403 = CARTESIAN_POINT('Ctrl Pts',(18.5108156395543,-1.43202569187897,-329.665389853047)) ;
#43404 = CARTESIAN_POINT('Ctrl Pts',(18.5168568829587,-1.3516672756189,-329.664343667278)) ;
#43405 = CARTESIAN_POINT('Ctrl Pts',(18.5269206635785,-1.20503845468096,-329.662447035533)) ;
#43406 = CARTESIAN_POINT('Ctrl Pts',(18.5311112587994,-1.13878112914995,-329.661594751771)) ;
#43407 = CARTESIAN_POINT('Ctrl Pts',(18.5384852197741,-1.01134464217916,-329.659963993967)) ;
#43408 = CARTESIAN_POINT('Ctrl Pts',(18.5417213276837,-0.950169664203256,
-329.659184854324)) ;
#43409 = CARTESIAN_POINT('Ctrl Pts',(18.5446545937457,-0.888979977932787,
-329.658408769442)) ;
#43410 = CARTESIAN_POINT('',(0.00032989125932316,-18.5659499970691,-329.726459838768)) ;
#43411 = CARTESIAN_POINT('Ctrl Pts',(18.5446545934183,-0.888979984762294,
-329.363119887734)) ;
#43412 = CARTESIAN_POINT('Ctrl Pts',(18.5408622451644,-0.96809063930157,-329.364098153425)) ;
#43413 = CARTESIAN_POINT('Ctrl Pts',(18.5365634497327,-1.04718169001174,-329.365078387839)) ;
#43414 = CARTESIAN_POINT('Ctrl Pts',(18.5141807712173,-1.41547560454857,-329.369655233095)) ;
#43415 = CARTESIAN_POINT('Ctrl Pts',(18.4898347200062,-1.70425125395901,-329.373279960535)) ;
#43416 = CARTESIAN_POINT('Ctrl Pts',(18.4431703167598,-2.13659056960382,-329.37878366536)) ;
#43417 = CARTESIAN_POINT('Ctrl Pts',(18.4259100571044,-2.28065540668142,-329.380630363209)) ;
#43418 = CARTESIAN_POINT('Ctrl Pts',(18.3907460732578,-2.54762235048005,-329.384078074143)) ;
#43419 = CARTESIAN_POINT('Ctrl Pts',(18.3732943572848,-2.67057581453395,-329.385676047891)) ;
#43420 = CARTESIAN_POINT('Ctrl Pts',(18.3308417048764,-2.949525227007,-329.389325115095)) ;
#43421 = CARTESIAN_POINT('Ctrl Pts',(18.3050805528528,-3.10539571131417,-329.391381048006)) ;
#43422 = CARTESIAN_POINT('Ctrl Pts',(18.2081303414711,-3.64879827313908,-329.398607346969)) ;
#43423 = CARTESIAN_POINT('Ctrl Pts',(18.1265978036808,-4.03437604046755,-329.403842006204)) ;
#43424 = CARTESIAN_POINT('Ctrl Pts',(17.9485203504936,-4.7613847840793,-329.413870855483)) ;
#43425 = CARTESIAN_POINT('Ctrl Pts',(17.8543368150823,-5.10321706153174,-329.418654063231)) ;
#43426 = CARTESIAN_POINT('Ctrl Pts',(17.6323803865769,-5.82716373825359,-329.428846450934)) ;
#43427 = CARTESIAN_POINT('Ctrl Pts',(17.5018397243408,-6.20824311980329,-329.434250036758)) ;
#43428 = CARTESIAN_POINT('Ctrl Pts',(17.3215687159364,-6.68347970674238,-329.440927766862)) ;
#43429 = CARTESIAN_POINT('Ctrl Pts',(17.2832861438352,-6.78186286289523,-329.442306665114)) ;
#43430 = CARTESIAN_POINT('Ctrl Pts',(17.2194123042543,-6.94195949883317,-329.444541639566)) ;
#43431 = CARTESIAN_POINT('Ctrl Pts',(17.1943233599385,-7.00387078842446,-329.445403710302)) ;
#43432 = CARTESIAN_POINT('Ctrl Pts',(17.1397825667695,-7.13640014674348,-329.447243459347)) ;
#43433 = CARTESIAN_POINT('Ctrl Pts',(17.1102272531836,-7.20697418172087,-329.448219892867)) ;
#43434 = CARTESIAN_POINT('Ctrl Pts',(17.0197339364188,-7.41936528193663,-329.451151262843)) ;
#43435 = CARTESIAN_POINT('Ctrl Pts',(16.9574627643747,-7.5606071966991,-329.453090967853)) ;
#43436 = CARTESIAN_POINT('Ctrl Pts',(16.8438312279553,-7.80987524298405,-329.456509141171)) ;
#43437 = CARTESIAN_POINT('Ctrl Pts',(16.7931746230104,-7.91821241632929,-329.457993013658)) ;
#43438 = CARTESIAN_POINT('Ctrl Pts',(16.5307112216416,-8.46568258809532,-329.465497704621)) ;
#43439 = CARTESIAN_POINT('Ctrl Pts',(16.3027122899162,-8.89684035838738,-329.471433302715)) ;
#43440 = CARTESIAN_POINT('Ctrl Pts',(15.8350492080014,-9.70273384665809,-329.482881216423)) ;
#43441 = CARTESIAN_POINT('Ctrl Pts',(15.5983736394179,-10.0788176905777,-329.488380041022)) ;
#43442 = CARTESIAN_POINT('Ctrl Pts',(15.2573006164766,-10.5799581722552,-329.496020389316)) ;
#43443 = CARTESIAN_POINT('Ctrl Pts',(15.1644146667849,-10.71266842273,-329.498074432208)) ;
#43444 = CARTESIAN_POINT('Ctrl Pts',(14.9969256411102,-10.9454232012221,-329.501734853121)) ;
#43445 = CARTESIAN_POINT('Ctrl Pts',(14.9230281291423,-11.0459630247471,-329.503335572336)) ;
#43446 = CARTESIAN_POINT('Ctrl Pts',(14.7635751202562,-11.2583828097293,-329.506760399129)) ;
#43447 = CARTESIAN_POINT('Ctrl Pts',(14.6777486453076,-11.3700496240256,-329.508586635772)) ;
#43448 = CARTESIAN_POINT('Ctrl Pts',(14.4282213567211,-11.6871695425115,-329.513847846711)) ;
#43449 = CARTESIAN_POINT('Ctrl Pts',(14.2614199290215,-11.8901389645837,-329.517307393516)) ;
#43450 = CARTESIAN_POINT('Ctrl Pts',(13.8478150729277,-12.3721973315111,-329.525740166454)) ;
#43451 = CARTESIAN_POINT('Ctrl Pts',(13.5968094094343,-12.6475302784091,-329.530740737127)) ;
#43452 = CARTESIAN_POINT('Ctrl Pts',(12.9525789206509,-13.3128391874652,-329.543210139689)) ;
#43453 = CARTESIAN_POINT('Ctrl Pts',(12.5498690664016,-13.6931287579334,-329.550695420131)) ;
#43454 = CARTESIAN_POINT('Ctrl Pts',(12.0443866403451,-14.129411549508,-329.559483518768)) ;
#43455 = CARTESIAN_POINT('Ctrl Pts',(11.9573178130261,-14.2031711619817,-329.560976326904)) ;
#43456 = CARTESIAN_POINT('Ctrl Pts',(11.8217686141987,-14.3158706151252,-329.563264572234)) ;
#43457 = CARTESIAN_POINT('Ctrl Pts',(11.7737633769682,-14.3553774103229,-329.564068139585)) ;
#43458 = CARTESIAN_POINT('Ctrl Pts',(11.6852601174995,-14.4274702281463,-329.56553638596)) ;
#43459 = CARTESIAN_POINT('Ctrl Pts',(11.6448219553146,-14.4601287281136,-329.566202234305)) ;
#43460 = CARTESIAN_POINT('Ctrl Pts',(11.6027696879068,-14.4938000039432,-329.566889777625)) ;
#43461 = CARTESIAN_POINT('Ctrl Pts',(11.6012920412161,-14.4949827857548,-329.566913930527)) ;
#43462 = CARTESIAN_POINT('Ctrl Pts',(11.5985031978816,-14.4972144148642,-329.566959503895)) ;
#43463 = CARTESIAN_POINT('Ctrl Pts',(11.5971920397567,-14.498263310301,-329.566980925055)) ;
#43464 = CARTESIAN_POINT('Ctrl Pts',(11.5947213763297,-14.5002392329097,-329.567021280542)) ;
#43465 = CARTESIAN_POINT('Ctrl Pts',(11.593561902115,-14.5011662988934,-329.567040215427)) ;
#43466 = CARTESIAN_POINT('Ctrl Pts',(11.591380316082,-14.5029101728699,-329.567075834827)) ;
#43467 = CARTESIAN_POINT('Ctrl Pts',(11.5903582291015,-14.503727011892,-329.567092519788)) ;
#43468 = CARTESIAN_POINT('Ctrl Pts',(11.5884377861092,-14.5052614730656,-329.567123864329)) ;
#43469 = CARTESIAN_POINT('Ctrl Pts',(11.5875394497845,-14.5059791198048,-329.567138524261)) ;
#43470 = CARTESIAN_POINT('Ctrl Pts',(11.5858536540197,-14.5073255814309,-329.567166030456)) ;
#43471 = CARTESIAN_POINT('Ctrl Pts',(11.5850662100155,-14.5079544156838,-329.567178876995)) ;
#43472 = CARTESIAN_POINT('Ctrl Pts',(11.5835902053199,-14.5091329215075,-329.567202953596)) ;
#43473 = CARTESIAN_POINT('Ctrl Pts',(11.5829016567055,-14.5096826081705,-329.567214183872)) ;
#43474 = CARTESIAN_POINT('Ctrl Pts',(11.5816123601113,-14.5107117376571,-329.567235209894)) ;
#43475 = CARTESIAN_POINT('Ctrl Pts',(11.5810116214779,-14.5111911921957,-329.567245005806)) ;
#43476 = CARTESIAN_POINT('Ctrl Pts',(11.5798877933608,-14.5120880145999,-329.567263329552)) ;
#43477 = CARTESIAN_POINT('Ctrl Pts',(11.5793647110713,-14.5125053914999,-329.567271857514)) ;
#43478 = CARTESIAN_POINT('Ctrl Pts',(11.577465670889,-14.5140205022649,-329.567302815329)) ;
#43479 = CARTESIAN_POINT('Ctrl Pts',(11.5760895794684,-14.5151180687207,-329.567325242815)) ;
#43480 = CARTESIAN_POINT('Ctrl Pts',(11.5733669855694,-14.517288968156,-329.567369605065)) ;
#43481 = CARTESIAN_POINT('Ctrl Pts',(11.5720204897817,-14.5183623095612,-329.567391539946)) ;
#43482 = CARTESIAN_POINT('Ctrl Pts',(11.5693572559227,-14.5204846655185,-329.567434914938)) ;
#43483 = CARTESIAN_POINT('Ctrl Pts',(11.5680405245102,-14.5215336882859,-329.567456355163)) ;
#43484 = CARTESIAN_POINT('Ctrl Pts',(11.4845382318516,-14.5880403127953,-329.56881570979)) ;
#43485 = CARTESIAN_POINT('Ctrl Pts',(11.4017985477145,-14.6527993397419,-329.570143862139)) ;
#43486 = CARTESIAN_POINT('Ctrl Pts',(11.2043066797621,-14.8046874128438,-329.573275054533)) ;
#43487 = CARTESIAN_POINT('Ctrl Pts',(11.0890811110369,-14.8911899379376,-329.575071240062)) ;
#43488 = CARTESIAN_POINT('Ctrl Pts',(10.6832227542838,-15.1885540654725,-329.581310355411)) ;
#43489 = CARTESIAN_POINT('Ctrl Pts',(10.3874896551477,-15.3923189396957,-329.585703482952)) ;
#43490 = CARTESIAN_POINT('Ctrl Pts',(9.60774151246282,-15.8968659738502,-329.597078987408)) ;
#43491 = CARTESIAN_POINT('Ctrl Pts',(9.11545812249566,-16.1841733378255,-329.60406949261)) ;
#43492 = CARTESIAN_POINT('Ctrl Pts',(8.4473955127139,-16.5339047066207,-329.613539078241)) ;
#43493 = CARTESIAN_POINT('Ctrl Pts',(8.28277959068855,-16.6169810102456,-329.615870096179)) ;
#43494 = CARTESIAN_POINT('Ctrl Pts',(8.00458619126559,-16.75221506323,-329.619810181734)) ;
#43495 = CARTESIAN_POINT('Ctrl Pts',(7.89167016808338,-16.805702946464,-329.621409602688)) ;
#43496 = CARTESIAN_POINT('Ctrl Pts',(7.66964847227156,-16.9081427045649,-329.624555744414)) ;
#43497 = CARTESIAN_POINT('Ctrl Pts',(7.56059265222892,-16.9571883314291,-329.626101702312)) ;
#43498 = CARTESIAN_POINT('Ctrl Pts',(7.29722734355125,-17.0725857512681,-329.629836868554)) ;
#43499 = CARTESIAN_POINT('Ctrl Pts',(7.14247645797602,-17.137903636772,-329.632033082205)) ;
#43500 = CARTESIAN_POINT('Ctrl Pts',(6.78299565728528,-17.283919907025,-329.63713695483)) ;
#43501 = CARTESIAN_POINT('Ctrl Pts',(6.57767479668875,-17.3630962524391,-329.640053771993)) ;
#43502 = CARTESIAN_POINT('Ctrl Pts',(5.88614552412401,-17.6157385971338,-329.649870233281)) ;
#43503 = CARTESIAN_POINT('Ctrl Pts',(5.39411955705996,-17.7725751641341,-329.656848523493)) ;
#43504 = CARTESIAN_POINT('Ctrl Pts',(4.57377480017317,-17.9968556303417,-329.668282517099)) ;
#43505 = CARTESIAN_POINT('Ctrl Pts',(4.24902635027594,-18.0762829223292,-329.672756478773)) ;
#43506 = CARTESIAN_POINT('Ctrl Pts',(3.81181733203114,-18.1707822396687,-329.678642341955)) ;
#43507 = CARTESIAN_POINT('Ctrl Pts',(3.70110790283412,-18.1936549083765,-329.680120955029)) ;
#43508 = CARTESIAN_POINT('Ctrl Pts',(3.52937242470506,-18.2275032014787,-329.682392797058)) ;
#43509 = CARTESIAN_POINT('Ctrl Pts',(3.46848873676772,-18.2391866203068,-329.683193976596)) ;
#43510 = CARTESIAN_POINT('Ctrl Pts',(3.34821219083737,-18.2616433530201,-329.684767572273)) ;
#43511 = CARTESIAN_POINT('Ctrl Pts',(3.28882304493746,-18.2724324001376,-329.685540195379)) ;
#43512 = CARTESIAN_POINT('Ctrl Pts',(3.15747565669814,-18.2956327784626,-329.687240277513)) ;
#43513 = CARTESIAN_POINT('Ctrl Pts',(3.08549464887268,-18.3079096041915,-329.688166212846)) ;
#43514 = CARTESIAN_POINT('Ctrl Pts',(2.90277885860415,-18.3379647786274,-329.690503960581)) ;
#43515 = CARTESIAN_POINT('Ctrl Pts',(2.79195189252602,-18.3551649952279,-329.691910195381)) ;
#43516 = CARTESIAN_POINT('Ctrl Pts',(1.79330179282447,-18.5009003548878,-329.70449959216)) ;
#43517 = CARTESIAN_POINT('Ctrl Pts',(0.897414458449384,-18.5659340571168,
-329.715274424528)) ;
#43518 = CARTESIAN_POINT('Ctrl Pts',(0.000329891259258086,-18.5659499970691,
-329.726459838768)) ;
#43519 = CARTESIAN_POINT('Ctrl Pts',(0.000329891259327128,-18.5659499970691,
-329.726459838768)) ;
#43520 = CARTESIAN_POINT('Ctrl Pts',(-0.136253520319998,-18.5659524239675,
-329.728162846592)) ;
#43521 = CARTESIAN_POINT('Ctrl Pts',(-0.272822686892261,-18.5644478010107,
-329.729873348739)) ;
#43522 = CARTESIAN_POINT('Ctrl Pts',(-0.52081802215839,-18.5589782610562,
-329.732996218987)) ;
#43523 = CARTESIAN_POINT('Ctrl Pts',(-0.632238875283148,-18.5555166858021,
-329.734405427499)) ;
#43524 = CARTESIAN_POINT('Ctrl Pts',(-0.859920157713469,-18.5463900473074,
-329.737298897399)) ;
#43525 = CARTESIAN_POINT('Ctrl Pts',(-0.976172098714441,-18.5406346832325,
-329.738783663845)) ;
#43526 = CARTESIAN_POINT('Ctrl Pts',(-1.21176310897569,-18.5267491937409,
-329.741808570231)) ;
#43527 = CARTESIAN_POINT('Ctrl Pts',(-1.33109318480385,-18.5185581622254,
-329.743349036822)) ;
#43528 = CARTESIAN_POINT('Ctrl Pts',(-1.61013486882489,-18.4966931552099,
-329.746971298007)) ;
#43529 = CARTESIAN_POINT('Ctrl Pts',(-1.76976501935743,-18.4821027927569,
-329.749058885577)) ;
#43530 = CARTESIAN_POINT('Ctrl Pts',(-2.34670282484013,-18.4218269524272,
-329.756659084622)) ;
#43531 = CARTESIAN_POINT('Ctrl Pts',(-2.76261892917325,-18.3640588487467,
-329.76224575829)) ;
#43532 = CARTESIAN_POINT('Ctrl Pts',(-3.65400732626134,-18.20928048276,-329.77438407974)) ;
#43533 = CARTESIAN_POINT('Ctrl Pts',(-4.1283627564002,-18.1076305916397,-329.78094748189)) ;
#43534 = CARTESIAN_POINT('Ctrl Pts',(-4.79406604446586,-17.9374553268578,
-329.790144827004)) ;
#43535 = CARTESIAN_POINT('Ctrl Pts',(-4.98910851811562,-17.8841876875475,
-329.79283702122)) ;
#43536 = CARTESIAN_POINT('Ctrl Pts',(-5.2876392560956,-17.7973928009225,-329.796935861391)) ;
#43537 = CARTESIAN_POINT('Ctrl Pts',(-5.39176778905298,-17.7661239321431,
-329.798361396359)) ;
#43538 = CARTESIAN_POINT('Ctrl Pts',(-5.5553925098561,-17.715417857826,-329.800591673918)) ;
#43539 = CARTESIAN_POINT('Ctrl Pts',(-5.61507527316497,-17.6965913526919,
-329.801403113806)) ;
#43540 = CARTESIAN_POINT('Ctrl Pts',(-5.73781484125675,-17.6571905905673,
-329.803066766056)) ;
#43541 = CARTESIAN_POINT('Ctrl Pts',(-5.80085871142923,-17.636579512741,-329.803918334821)) ;
#43542 = CARTESIAN_POINT('Ctrl Pts',(-5.95609198282375,-17.5849063459132,
-329.806008659625)) ;
#43543 = CARTESIAN_POINT('Ctrl Pts',(-6.048150285661,-17.5534566699538,-329.807242784401)) ;
#43544 = CARTESIAN_POINT('Ctrl Pts',(-6.44040665641951,-17.4159988661017,
-329.812485398895)) ;
#43545 = CARTESIAN_POINT('Ctrl Pts',(-6.73809901036303,-17.3030019658653,
-329.816424924837)) ;
#43546 = CARTESIAN_POINT('Ctrl Pts',(-7.10138855594153,-17.154307980473,-329.821252348044)) ;
#43547 = CARTESIAN_POINT('Ctrl Pts',(-7.1698693614902,-17.1257985231261,-329.822163160209)) ;
#43548 = CARTESIAN_POINT('Ctrl Pts',(-7.69652358319347,-16.9028328794199,
-329.829178972102)) ;
#43549 = CARTESIAN_POINT('Ctrl Pts',(-8.14688135666589,-16.6904331514723,
-329.83524997844)) ;
#43550 = CARTESIAN_POINT('Ctrl Pts',(-8.78016287223406,-16.360016525145,-329.844096547912)) ;
#43551 = CARTESIAN_POINT('Ctrl Pts',(-8.97039921160087,-16.2564860456305,
-329.846794763054)) ;
#43552 = CARTESIAN_POINT('Ctrl Pts',(-9.30758355962203,-16.0652622620885,
-329.851663636507)) ;
#43553 = CARTESIAN_POINT('Ctrl Pts',(-9.45521297583125,-15.9788206926722,
-329.853825743391)) ;
#43554 = CARTESIAN_POINT('Ctrl Pts',(-9.69586189517585,-15.8334103747961,
-329.85740420222)) ;
#43555 = CARTESIAN_POINT('Ctrl Pts',(-9.78958880375593,-15.7756322537419,
-329.858811633972)) ;
#43556 = CARTESIAN_POINT('Ctrl Pts',(-9.98833960575394,-15.6506586153321,
-329.861826285248)) ;
#43557 = CARTESIAN_POINT('Ctrl Pts',(-10.0932118038639,-15.5832319691426,
-329.863435222272)) ;
#43558 = CARTESIAN_POINT('Ctrl Pts',(-10.3500371588856,-15.4144281311376,
-329.867421173932)) ;
#43559 = CARTESIAN_POINT('Ctrl Pts',(-10.5011884212268,-15.3118550601952,
-329.869807235057)) ;
#43560 = CARTESIAN_POINT('Ctrl Pts',(-11.1579634310204,-14.8518597537046,
-329.880350628439)) ;
#43561 = CARTESIAN_POINT('Ctrl Pts',(-11.6470370637305,-14.4715033306896,
-329.888680715013)) ;
#43562 = CARTESIAN_POINT('Ctrl Pts',(-12.3644929425667,-13.8535629407165,
-329.901435332146)) ;
#43563 = CARTESIAN_POINT('Ctrl Pts',(-12.6070916660311,-13.6331629472015,
-329.905846986957)) ;
#43564 = CARTESIAN_POINT('Ctrl Pts',(-12.9428499074022,-13.3114979566371,
-329.91203586379)) ;
#43565 = CARTESIAN_POINT('Ctrl Pts',(-13.0409140928282,-13.2154417738512,
-329.913853806637)) ;
#43566 = CARTESIAN_POINT('Ctrl Pts',(-13.1420799039833,-13.1141248326584,
-329.915736193449)) ;
#43567 = CARTESIAN_POINT('Ctrl Pts',(-13.1462537060571,-13.1099408017435,
-329.915813867578)) ;
#43568 = CARTESIAN_POINT('Ctrl Pts',(-13.1541323861717,-13.1020352672882,
-329.915960512055)) ;
#43569 = CARTESIAN_POINT('Ctrl Pts',(-13.1578376844421,-13.0983141834389,
-329.916029487675)) ;
#43570 = CARTESIAN_POINT('Ctrl Pts',(-13.1648366365848,-13.0912794471348,
-329.916159793635)) ;
#43571 = CARTESIAN_POINT('Ctrl Pts',(-13.168130619304,-13.087966122507,-329.91622112815)) ;
#43572 = CARTESIAN_POINT('Ctrl Pts',(-13.1743569091214,-13.0816985426064,
-329.916337076405)) ;
#43573 = CARTESIAN_POINT('Ctrl Pts',(-13.1772894740584,-13.0787445439314,
-329.916391693453)) ;
#43574 = CARTESIAN_POINT('Ctrl Pts',(-13.1828364781382,-13.0731532379854,
-329.916495013334)) ;
#43575 = CARTESIAN_POINT('Ctrl Pts',(-13.185451119886,-13.0705161320538,-329.91654371879)) ;
#43576 = CARTESIAN_POINT('Ctrl Pts',(-13.1904002181376,-13.0655215163955,
-329.916635918766)) ;
#43577 = CARTESIAN_POINT('Ctrl Pts',(-13.1927348342524,-13.0631641650537,
-329.91667941537)) ;
#43578 = CARTESIAN_POINT('Ctrl Pts',(-13.19715693779,-13.0586966031236,-329.916761810844)) ;
#43579 = CARTESIAN_POINT('Ctrl Pts',(-13.1992445512787,-13.0565865174873,
-329.916800711372)) ;
#43580 = CARTESIAN_POINT('Ctrl Pts',(-13.2032014650222,-13.0525850906244,
-329.916874449564)) ;
#43581 = CARTESIAN_POINT('Ctrl Pts',(-13.2050708651241,-13.0506938482598,
-329.916909288549)) ;
#43582 = CARTESIAN_POINT('Ctrl Pts',(-13.2086164916422,-13.0471052525056,
-329.916975370551)) ;
#43583 = CARTESIAN_POINT('Ctrl Pts',(-13.2102927973626,-13.045407977568,-329.917006614624)) ;
#43584 = CARTESIAN_POINT('Ctrl Pts',(-13.2134741923686,-13.0421855438999,
-329.917065914791)) ;
#43585 = CARTESIAN_POINT('Ctrl Pts',(-13.2149793448094,-13.0406604476216,
-329.917093971731)) ;
#43586 = CARTESIAN_POINT('Ctrl Pts',(-13.2178376370418,-13.0377632789091,
-329.917147254611)) ;
#43587 = CARTESIAN_POINT('Ctrl Pts',(-13.2191908273269,-13.036391256279,-329.91717248123)) ;
#43588 = CARTESIAN_POINT('Ctrl Pts',(-13.2217620167917,-13.0337834715962,
-329.917220416279)) ;
#43589 = CARTESIAN_POINT('Ctrl Pts',(-13.2229800563898,-13.0325477494406,
-329.917243125255)) ;
#43590 = CARTESIAN_POINT('Ctrl Pts',(-13.2252957040405,-13.0301978261796,
-329.917286299576)) ;
#43591 = CARTESIAN_POINT('Ctrl Pts',(-13.2263933445529,-13.0290836571056,
-329.91730676536)) ;
#43592 = CARTESIAN_POINT('Ctrl Pts',(-13.2284811673707,-13.0269638595787,
-329.917345694697)) ;
#43593 = CARTESIAN_POINT('Ctrl Pts',(-13.2294713758394,-13.0259582568844,
-329.917364158605)) ;
#43594 = CARTESIAN_POINT('Ctrl Pts',(-13.2313557589736,-13.0240441417756,
-329.917399296822)) ;
#43595 = CARTESIAN_POINT('Ctrl Pts',(-13.2322499546895,-13.0231356502212,
-329.917415971418)) ;
#43596 = CARTESIAN_POINT('Ctrl Pts',(-13.2339523915323,-13.0214056395346,
-329.917447718652)) ;
#43597 = CARTESIAN_POINT('Ctrl Pts',(-13.2347606497656,-13.0205841372061,
-329.917462791523)) ;
#43598 = CARTESIAN_POINT('Ctrl Pts',(-13.236300120926,-13.0190191488729,-329.9174915012)) ;
#43599 = CARTESIAN_POINT('Ctrl Pts',(-13.2370313477453,-13.018275676477,-329.917505138196)) ;
#43600 = CARTESIAN_POINT('Ctrl Pts',(-13.2384246461423,-13.0168588062833,
-329.917531123067)) ;
#43601 = CARTESIAN_POINT('Ctrl Pts',(-13.2390867289481,-13.016185419611,-329.917543471096)) ;
#43602 = CARTESIAN_POINT('Ctrl Pts',(-13.240348739621,-13.0149016664813,-329.917567008425)) ;
#43603 = CARTESIAN_POINT('Ctrl Pts',(-13.2409486766587,-13.0142913090591,
-329.917578197852)) ;
#43604 = CARTESIAN_POINT('Ctrl Pts',(-13.2420926179423,-13.0131273375298,
-329.917599533895)) ;
#43605 = CARTESIAN_POINT('Ctrl Pts',(-13.2426366297038,-13.0125737307635,
-329.917609680615)) ;
#43606 = CARTESIAN_POINT('Ctrl Pts',(-13.2436742607209,-13.0115176660735,
-329.917629034472)) ;
#43607 = CARTESIAN_POINT('Ctrl Pts',(-13.2441678861307,-13.011015214141,-329.917638241694)) ;
#43608 = CARTESIAN_POINT('Ctrl Pts',(-13.2463371621554,-13.0088068978972,
-329.917678704169)) ;
#43609 = CARTESIAN_POINT('Ctrl Pts',(-13.2480125118394,-13.007100737921,-329.917709955261)) ;
#43610 = CARTESIAN_POINT('Ctrl Pts',(-13.2513002679626,-13.0037512245989,
-329.917771286414)) ;
#43611 = CARTESIAN_POINT('Ctrl Pts',(-13.2529126984094,-13.0021078949263,
-329.917801366809)) ;
#43612 = CARTESIAN_POINT('Ctrl Pts',(-13.2560781957448,-12.9988805361063,
-329.917860422972)) ;
#43613 = CARTESIAN_POINT('Ctrl Pts',(-13.2576312844977,-12.9972965284314,
-329.917889399044)) ;
#43614 = CARTESIAN_POINT('Ctrl Pts',(-13.2606814622409,-12.9941845121411,
-329.917946308983)) ;
#43615 = CARTESIAN_POINT('Ctrl Pts',(-13.2621785711241,-12.9926565230596,
-329.917974243128)) ;
#43616 = CARTESIAN_POINT('Ctrl Pts',(-13.2651199515759,-12.9896534339698,
-329.918029127914)) ;
#43617 = CARTESIAN_POINT('Ctrl Pts',(-13.2665642412228,-12.9881783517878,
-329.918056078809)) ;
#43618 = CARTESIAN_POINT('Ctrl Pts',(-13.2694029577258,-12.985278145785,-329.91810905233)) ;
#43619 = CARTESIAN_POINT('Ctrl Pts',(-13.2707974011233,-12.9838530381487,
-329.918135075188)) ;
#43620 = CARTESIAN_POINT('Ctrl Pts',(-13.2735392244,-12.9810500181953,-329.918186244628)) ;
#43621 = CARTESIAN_POINT('Ctrl Pts',(-13.2748866193577,-12.9796721206575,
-329.918211391423)) ;
#43622 = CARTESIAN_POINT('Ctrl Pts',(-13.2775369815361,-12.9769609147086,
-329.918260857706)) ;
#43623 = CARTESIAN_POINT('Ctrl Pts',(-13.2788399625216,-12.9756276197984,
-329.91828517739)) ;
#43624 = CARTESIAN_POINT('Ctrl Pts',(-13.2814039799834,-12.9730031596505,
-329.9183330356)) ;
#43625 = CARTESIAN_POINT('Ctrl Pts',(-13.2826650290461,-12.9717120067467,
-329.918356574305)) ;
#43626 = CARTESIAN_POINT('Ctrl Pts',(-13.2851475235741,-12.9691695083829,
-329.918402914072)) ;
#43627 = CARTESIAN_POINT('Ctrl Pts',(-13.286368980566,-12.9679181741924,-329.918425715298)) ;
#43628 = CARTESIAN_POINT('Ctrl Pts',(-13.2887744991332,-12.9654531193016,
-329.918470621163)) ;
#43629 = CARTESIAN_POINT('Ctrl Pts',(-13.2899585712521,-12.9642394089288,
-329.918492725953)) ;
#43630 = CARTESIAN_POINT('Ctrl Pts',(-13.2922914044472,-12.9618475276289,
-329.918536277709)) ;
#43631 = CARTESIAN_POINT('Ctrl Pts',(-13.2934401751812,-12.9606693661677,
-329.918557724815)) ;
#43632 = CARTESIAN_POINT('Ctrl Pts',(-13.2957043744873,-12.9583466207303,
-329.918599997825)) ;
#43633 = CARTESIAN_POINT('Ctrl Pts',(-13.2968198119574,-12.9572020453913,
-329.918620823859)) ;
#43634 = CARTESIAN_POINT('Ctrl Pts',(-13.2990192060026,-12.9549446148674,
-329.918661889354)) ;
#43635 = CARTESIAN_POINT('Ctrl Pts',(-13.3001031707067,-12.9538317676457,
-329.918682128934)) ;
#43636 = CARTESIAN_POINT('Ctrl Pts',(-13.3022413801625,-12.9516360337398,
-329.91872205429)) ;
#43637 = CARTESIAN_POINT('Ctrl Pts',(-13.3032956323535,-12.9505531543938,
-329.918741740175)) ;
#43638 = CARTESIAN_POINT('Ctrl Pts',(-13.3053760841499,-12.948415687916,-329.918780589174)) ;
#43639 = CARTESIAN_POINT('Ctrl Pts',(-13.3064022906626,-12.9473611074531,
-329.918799752389)) ;
#43640 = CARTESIAN_POINT('Ctrl Pts',(-13.3084282313942,-12.9452786554912,
-329.918837585468)) ;
#43641 = CARTESIAN_POINT('Ctrl Pts',(-13.3094279719604,-12.9442507901264,
-329.918856255424)) ;
#43642 = CARTESIAN_POINT('Ctrl Pts',(-13.3114024800716,-12.9422202643729,
-329.918893129899)) ;
#43643 = CARTESIAN_POINT('Ctrl Pts',(-13.312377253389,-12.9412176096938,-329.918911334502)) ;
#43644 = CARTESIAN_POINT('Ctrl Pts',(-13.314303250759,-12.9392360753006,-329.918947304783)) ;
#43645 = CARTESIAN_POINT('Ctrl Pts',(-13.3152544801854,-12.9382572007762,
-329.91896507054)) ;
#43646 = CARTESIAN_POINT('Ctrl Pts',(-13.3171347433885,-12.936321865463,-329.91900018834)) ;
#43647 = CARTESIAN_POINT('Ctrl Pts',(-13.3180637820872,-12.9353654094764,
-329.919017540455)) ;
#43648 = CARTESIAN_POINT('Ctrl Pts',(-13.3199009523127,-12.9334736139462,
-329.919051854973)) ;
#43649 = CARTESIAN_POINT('Ctrl Pts',(-13.3208090883311,-12.9325382788646,
-329.919068817442)) ;
#43650 = CARTESIAN_POINT('Ctrl Pts',(-13.3226056810972,-12.9306874873656,
-329.919102375543)) ;
#43651 = CARTESIAN_POINT('Ctrl Pts',(-13.3234941420755,-12.9297720349585,
-329.919118971238)) ;
#43652 = CARTESIAN_POINT('Ctrl Pts',(-13.3252525566396,-12.9279598261002,
-329.919151817627)) ;
#43653 = CARTESIAN_POINT('Ctrl Pts',(-13.3261225140773,-12.9270630733858,
-329.919168068379)) ;
#43654 = CARTESIAN_POINT('Ctrl Pts',(-13.3278450415625,-12.9252871322244,
-329.919200245755)) ;
#43655 = CARTESIAN_POINT('Ctrl Pts',(-13.3286976151464,-12.9244079472267,
-329.919216172431)) ;
#43656 = CARTESIAN_POINT('Ctrl Pts',(-13.3303864469596,-12.9226660570025,
-329.919247721637)) ;
#43657 = CARTESIAN_POINT('Ctrl Pts',(-13.3312227084368,-12.9218033549558,
-329.919263344215)) ;
#43658 = CARTESIAN_POINT('Ctrl Pts',(-13.3328799438208,-12.9200933896785,
-329.919294304383)) ;
#43659 = CARTESIAN_POINT('Ctrl Pts',(-13.3337009207704,-12.9192461293142,
-329.919309642019)) ;
#43660 = CARTESIAN_POINT('Ctrl Pts',(-13.3353285743212,-12.9175660463461,
-329.919340050708)) ;
#43661 = CARTESIAN_POINT('Ctrl Pts',(-13.3361352536092,-12.9167332264882,
-329.919355121802)) ;
#43662 = CARTESIAN_POINT('Ctrl Pts',(-13.3377352617355,-12.9150810601814,
-329.91938501512)) ;
#43663 = CARTESIAN_POINT('Ctrl Pts',(-13.3385285931048,-12.9142617161851,
-329.919399837382)) ;
#43664 = CARTESIAN_POINT('Ctrl Pts',(-13.3401028212343,-12.9126355707162,
-329.919429250116)) ;
#43665 = CARTESIAN_POINT('Ctrl Pts',(-13.3408837203459,-12.9118287714575,
-329.919443840624)) ;
#43666 = CARTESIAN_POINT('Ctrl Pts',(-13.3424339689639,-12.9102268148361,
-329.919472806354)) ;
#43667 = CARTESIAN_POINT('Ctrl Pts',(-13.3432033205669,-12.9094316595537,
-329.919487181609)) ;
#43668 = CARTESIAN_POINT('Ctrl Pts',(-13.3447313312106,-12.9078521176504,
-329.919515732822)) ;
#43669 = CARTESIAN_POINT('Ctrl Pts',(-13.3454899922182,-12.9070677328714,
-329.919529908811)) ;
#43670 = CARTESIAN_POINT('Ctrl Pts',(-13.3469974537501,-12.9055088831316,
-329.919558077014)) ;
#43671 = CARTESIAN_POINT('Ctrl Pts',(-13.3477462559823,-12.9047344199293,
-329.919572069255)) ;
#43672 = CARTESIAN_POINT('Ctrl Pts',(-13.3492348097786,-12.9031945861837,
-329.919599885074)) ;
#43673 = CARTESIAN_POINT('Ctrl Pts',(-13.3499745629657,-12.902429217155,-329.919613708677)) ;
#43674 = CARTESIAN_POINT('Ctrl Pts',(-13.3845269427947,-12.8666742201661,
-329.920259391737)) ;
#43675 = CARTESIAN_POINT('Ctrl Pts',(-13.4182019741192,-12.8315518452594,
-329.920889147483)) ;
#43676 = CARTESIAN_POINT('Ctrl Pts',(-13.4979550464683,-12.7477137287387,
-329.922381262118)) ;
#43677 = CARTESIAN_POINT('Ctrl Pts',(-13.5439079100178,-12.6988800396488,
-329.923241371347)) ;
#43678 = CARTESIAN_POINT('Ctrl Pts',(-13.6479130059014,-12.5871480495444,
-329.925189914056)) ;
#43679 = CARTESIAN_POINT('Ctrl Pts',(-13.7057968945739,-12.5240950551092,
-329.926275792337)) ;
#43680 = CARTESIAN_POINT('Ctrl Pts',(-13.9595612838452,-12.2438028896569,
-329.93104801048)) ;
#43681 = CARTESIAN_POINT('Ctrl Pts',(-14.1507283567185,-12.0223520217235,
-329.934674815342)) ;
#43682 = CARTESIAN_POINT('Ctrl Pts',(-14.7008339811295,-11.3537934882978,
-329.945337201584)) ;
#43683 = CARTESIAN_POINT('Ctrl Pts',(-15.0443851190424,-10.8944767595447,
-329.952305808455)) ;
#43684 = CARTESIAN_POINT('Ctrl Pts',(-15.4550558782701,-10.2888702007673,
-329.961353601538)) ;
#43685 = CARTESIAN_POINT('Ctrl Pts',(-15.5422960980164,-10.1566054436673,
-329.963320739079)) ;
#43686 = CARTESIAN_POINT('Ctrl Pts',(-15.7508580116747,-9.8314241099991,-329.968143145274)) ;
#43687 = CARTESIAN_POINT('Ctrl Pts',(-15.8703412710499,-9.63735937916694,
-329.971009542133)) ;
#43688 = CARTESIAN_POINT('Ctrl Pts',(-16.0548287586074,-9.3249758748697,-329.975615357569)) ;
#43689 = CARTESIAN_POINT('Ctrl Pts',(-16.122167415691,-9.20806273281387,-329.977337287434)) ;
#43690 = CARTESIAN_POINT('Ctrl Pts',(-16.2502161196128,-8.98003367331189,
-329.980693588445)) ;
#43691 = CARTESIAN_POINT('Ctrl Pts',(-16.3110756363759,-8.86901010474918,
-329.982326729681)) ;
#43692 = CARTESIAN_POINT('Ctrl Pts',(-16.4418118717734,-8.62461533990689,
-329.985920118333)) ;
#43693 = CARTESIAN_POINT('Ctrl Pts',(-16.5112114197094,-8.49099904327274,
-329.987883680545)) ;
#43694 = CARTESIAN_POINT('Ctrl Pts',(-16.7837122394884,-7.9503712518873,-329.995823471012)) ;
#43695 = CARTESIAN_POINT('Ctrl Pts',(-16.9734496294718,-7.53680337919305,
-330.001890058656)) ;
#43696 = CARTESIAN_POINT('Ctrl Pts',(-17.3290383100729,-6.68000499861943,
-330.014354572443)) ;
#43697 = CARTESIAN_POINT('Ctrl Pts',(-17.4935232749659,-6.2365598488215,-330.020751702949)) ;
#43698 = CARTESIAN_POINT('Ctrl Pts',(-17.6922594141145,-5.63077270183929,
-330.029268824819)) ;
#43699 = CARTESIAN_POINT('Ctrl Pts',(-17.7415310120517,-5.47354746622276,
-330.031459075067)) ;
#43700 = CARTESIAN_POINT('Ctrl Pts',(-17.8242658730452,-5.19667904602995,
-330.035269401811)) ;
#43701 = CARTESIAN_POINT('Ctrl Pts',(-17.8586332119113,-5.07731689958857,
-330.036897023388)) ;
#43702 = CARTESIAN_POINT('Ctrl Pts',(-17.9107216446587,-4.88933232942958,
-330.039432000762)) ;
#43703 = CARTESIAN_POINT('Ctrl Pts',(-17.9292519857035,-4.820938053306,-330.040348430081)) ;
#43704 = CARTESIAN_POINT('Ctrl Pts',(-17.96337531968,-4.69207269489941,-330.042062967361)) ;
#43705 = CARTESIAN_POINT('Ctrl Pts',(-17.9790556422573,-4.63162577011559,
-330.04286220575)) ;
#43706 = CARTESIAN_POINT('Ctrl Pts',(-18.0229290488223,-4.45891530031092,
-330.045132952961)) ;
#43707 = CARTESIAN_POINT('Ctrl Pts',(-18.0503776788936,-4.34646556022606,
-330.046595961024)) ;
#43708 = CARTESIAN_POINT('Ctrl Pts',(-18.1800605378239,-3.79276292687671,
-330.053738688009)) ;
#43709 = CARTESIAN_POINT('Ctrl Pts',(-18.2671756163945,-3.34812618423389,
-330.0592880579)) ;
#43710 = CARTESIAN_POINT('Ctrl Pts',(-18.4055755809194,-2.47318980316046,
-330.070138401297)) ;
#43711 = CARTESIAN_POINT('Ctrl Pts',(-18.4582342332835,-2.0433964030528,-330.075436142913)) ;
#43712 = CARTESIAN_POINT('Ctrl Pts',(-18.520702215416,-1.32671877871265,-330.084362257575)) ;
#43713 = CARTESIAN_POINT('Ctrl Pts',(-18.5389709950648,-1.04074359066319,
-330.08794737285)) ;
#43714 = CARTESIAN_POINT('Ctrl Pts',(-18.5564902974383,-0.609980587295372,
-330.093404559269)) ;
#43715 = CARTESIAN_POINT('Ctrl Pts',(-18.5606782477298,-0.465436764969228,
-330.095245224115)) ;
#43716 = CARTESIAN_POINT('Ctrl Pts',(-18.5653241829315,-0.196647865447113,
-330.09868757901)) ;
#43717 = CARTESIAN_POINT('Ctrl Pts',(-18.5662243849018,-0.0724184965304549,
-330.100286310085)) ;
#43718 = CARTESIAN_POINT('Ctrl Pts',(-18.5654349079548,0.210484620098622,
-330.103945340857)) ;
#43719 = CARTESIAN_POINT('Ctrl Pts',(-18.5629579515323,0.369146422718707,
-330.106010586646)) ;
#43720 = CARTESIAN_POINT('Ctrl Pts',(-18.548018142377,0.894501425156988,-330.112892034296)) ;
#43721 = CARTESIAN_POINT('Ctrl Pts',(-18.5267199556095,1.2608554099375,-330.117761959716)) ;
#43722 = CARTESIAN_POINT('Ctrl Pts',(-18.43265997682,2.33049874018311,-330.132134311281)) ;
#43723 = CARTESIAN_POINT('Ctrl Pts',(-18.3305742706896,3.03054813755851,-330.141754210235)) ;
#43724 = CARTESIAN_POINT('Ctrl Pts',(-18.1590066031488,3.86873181611012,-330.15307932388)) ;
#43725 = CARTESIAN_POINT('Ctrl Pts',(-18.1274416699266,4.01403354532787,-330.155034373553)) ;
#43726 = CARTESIAN_POINT('Ctrl Pts',(-18.0772217848843,4.23252317062873,-330.157954059474)) ;
#43727 = CARTESIAN_POINT('Ctrl Pts',(-18.0598600987755,4.30600198360925,-330.158932502206)) ;
#43728 = CARTESIAN_POINT('Ctrl Pts',(-18.0261927133768,4.44470418746964,-330.160771547352)) ;
#43729 = CARTESIAN_POINT('Ctrl Pts',(-18.0099800383235,4.50994878727905,-330.161633168939)) ;
#43730 = CARTESIAN_POINT('Ctrl Pts',(-17.9667452755004,4.67998666571188,-330.163871058409)) ;
#43731 = CARTESIAN_POINT('Ctrl Pts',(-17.9391606473623,4.78463439632518,-330.165240821007)) ;
#43732 = CARTESIAN_POINT('Ctrl Pts',(-17.7372999923676,5.5241378043481,-330.174884297477)) ;
#43733 = CARTESIAN_POINT('Ctrl Pts',(-17.5302788647954,6.14957228770004,-330.182868660411)) ;
#43734 = CARTESIAN_POINT('Ctrl Pts',(-17.1742018209146,7.05997079450781,-330.194869220699)) ;
#43735 = CARTESIAN_POINT('Ctrl Pts',(-17.0502806158901,7.35420466829498,-330.198805602119)) ;
#43736 = CARTESIAN_POINT('Ctrl Pts',(-16.8206005133454,7.86249384173043,-330.205759654458)) ;
#43737 = CARTESIAN_POINT('Ctrl Pts',(-16.71818463764,8.07797704599655,-330.208757252731)) ;
#43738 = CARTESIAN_POINT('Ctrl Pts',(-16.5505627479003,8.41380289599961,-330.213519254982)) ;
#43739 = CARTESIAN_POINT('Ctrl Pts',(-16.488130174181,8.53550055577084,-330.215263894579)) ;
#43740 = CARTESIAN_POINT('Ctrl Pts',(-16.3656770694023,8.76783630114897,-330.218632732258)) ;
#43741 = CARTESIAN_POINT('Ctrl Pts',(-16.3058649255907,8.87857580464569,-330.220255336782)) ;
#43742 = CARTESIAN_POINT('Ctrl Pts',(-16.1608172959327,9.14071484634711,-330.22413735203)) ;
#43743 = CARTESIAN_POINT('Ctrl Pts',(-16.0745735575623,9.29154284178438,-330.226404045859)) ;
#43744 = CARTESIAN_POINT('Ctrl Pts',(-15.5684391087905,10.1485560099807,-330.239472353046)) ;
#43745 = CARTESIAN_POINT('Ctrl Pts',(-15.1041571454183,10.8274608739033,-330.250614457625)) ;
#43746 = CARTESIAN_POINT('Ctrl Pts',(-14.4643211654238,11.6414613953628,-330.264507321033)) ;
#43747 = CARTESIAN_POINT('Ctrl Pts',(-14.3293028673811,11.8072558088925,-330.267364092716)) ;
#43748 = CARTESIAN_POINT('Ctrl Pts',(-14.145305022986,12.0253884570602,-330.27114166207)) ;
#43749 = CARTESIAN_POINT('Ctrl Pts',(-14.0988428729793,12.0798282848755,-330.272086033692)) ;
#43750 = CARTESIAN_POINT('Ctrl Pts',(-13.981638561609,12.2155595441264,-330.274443197448)) ;
#43751 = CARTESIAN_POINT('Ctrl Pts',(-13.9105011979168,12.2965063460543,-330.275851344508)) ;
#43752 = CARTESIAN_POINT('Ctrl Pts',(-13.7934508935331,12.4273815230122,-330.278128679977)) ;
#43753 = CARTESIAN_POINT('Ctrl Pts',(-13.7479619785729,12.477685704791,-330.279004137428)) ;
#43754 = CARTESIAN_POINT('Ctrl Pts',(-13.6509320763541,12.5838120293233,-330.280850419676)) ;
#43755 = CARTESIAN_POINT('Ctrl Pts',(-13.5993220767821,12.6395692495885,-330.281820210794)) ;
#43756 = CARTESIAN_POINT('Ctrl Pts',(-13.4438957033224,12.8054311976472,-330.284707014249)) ;
#43757 = CARTESIAN_POINT('Ctrl Pts',(-13.3390738058178,12.914585164464,-330.286609457279)) ;
#43758 = CARTESIAN_POINT('Ctrl Pts',(-12.7710775013925,13.4917620693357,-330.296718042306)) ;
#43759 = CARTESIAN_POINT('Ctrl Pts',(-12.2845848681025,13.9361775345369,-330.30469415982)) ;
#43760 = CARTESIAN_POINT('Ctrl Pts',(-11.5591430101337,14.531312247344,-330.316241653929)) ;
#43761 = CARTESIAN_POINT('Ctrl Pts',(-11.3387881252921,14.7039010560922,-330.319704569893)) ;
#43762 = CARTESIAN_POINT('Ctrl Pts',(-10.9394009754564,15.0023949674402,-330.325935682732)) ;
#43763 = CARTESIAN_POINT('Ctrl Pts',(-10.7618850614671,15.1302405182814,-330.328689800325)) ;
#43764 = CARTESIAN_POINT('Ctrl Pts',(-10.4726160288993,15.3309029260531,-330.333161913369)) ;
#43765 = CARTESIAN_POINT('Ctrl Pts',(-10.3622651056525,15.4057045549696,-330.334864277859)) ;
#43766 = CARTESIAN_POINT('Ctrl Pts',(-10.1460758427992,15.5488751184642,-330.338193616322)) ;
#43767 = CARTESIAN_POINT('Ctrl Pts',(-10.0403281540684,15.6173679908819,-330.339819505918)) ;
#43768 = CARTESIAN_POINT('Ctrl Pts',(-9.77912151819271,15.7828021601966,-330.343829718169)) ;
#43769 = CARTESIAN_POINT('Ctrl Pts',(-9.62290924836227,15.8785288718491,-330.346223016252)) ;
#43770 = CARTESIAN_POINT('Ctrl Pts',(-8.9415261233652,16.2823310855383,-330.356638513113)) ;
#43771 = CARTESIAN_POINT('Ctrl Pts',(-8.40279578270078,16.5667804125906,-330.364826554985)) ;
#43772 = CARTESIAN_POINT('Ctrl Pts',(-7.54849745567921,16.9654404918007,-330.377525684185)) ;
#43773 = CARTESIAN_POINT('Ctrl Pts',(-7.24217209574838,17.0984481341291,-330.382021945385)) ;
#43774 = CARTESIAN_POINT('Ctrl Pts',(-6.80380196922627,17.2748951637049,-330.388312954738)) ;
#43775 = CARTESIAN_POINT('Ctrl Pts',(-6.67460098003471,17.3252251353954,-330.390149648642)) ;
#43776 = CARTESIAN_POINT('Ctrl Pts',(-6.44220904980851,17.412767491037,-330.393415108041)) ;
#43777 = CARTESIAN_POINT('Ctrl Pts',(-6.33922911760615,17.4505215792415,-330.394848843323)) ;
#43778 = CARTESIAN_POINT('Ctrl Pts',(-6.17173349665641,17.5102498249634,-330.397155875418)) ;
#43779 = CARTESIAN_POINT('Ctrl Pts',(-6.10742075147503,17.5327851492931,-330.39803575777)) ;
#43780 = CARTESIAN_POINT('Ctrl Pts',(-5.97179533334822,17.5794717906068,-330.399877830968)) ;
#43781 = CARTESIAN_POINT('Ctrl Pts',(-5.90045696742182,17.6035444026449,-330.400839121879)) ;
#43782 = CARTESIAN_POINT('Ctrl Pts',(-5.68891678466876,17.6734967191664,-330.403669619952)) ;
#43783 = CARTESIAN_POINT('Ctrl Pts',(-5.54831225292222,17.7181401882011,-330.405525074616)) ;
#43784 = CARTESIAN_POINT('Ctrl Pts',(-5.25041902066515,17.8088308071335,-330.409414420272)) ;
#43785 = CARTESIAN_POINT('Ctrl Pts',(-5.09302234233534,17.8544806179482,-330.41144512512)) ;
#43786 = CARTESIAN_POINT('Ctrl Pts',(-4.35923786866158,18.0568076298321,-330.420834864404)) ;
#43787 = CARTESIAN_POINT('Ctrl Pts',(-3.77610759536126,18.1876955589154,-330.428088034698)) ;
#43788 = CARTESIAN_POINT('Ctrl Pts',(-2.95776386008898,18.3303191866483,-330.438355253695)) ;
#43789 = CARTESIAN_POINT('Ctrl Pts',(-2.72710853489258,18.3660514901803,-330.441257084157)) ;
#43790 = CARTESIAN_POINT('Ctrl Pts',(-2.30454491617452,18.4233775382452,-330.446605069067)) ;
#43791 = CARTESIAN_POINT('Ctrl Pts',(-2.1128557045592,18.4463440222037,-330.449042903189)) ;
#43792 = CARTESIAN_POINT('Ctrl Pts',(-1.79268696095943,18.4796475794912,-330.453139932179)) ;
#43793 = CARTESIAN_POINT('Ctrl Pts',(-1.6643952672059,18.49164377605,-330.454788306525)) ;
#43794 = CARTESIAN_POINT('Ctrl Pts',(-1.42056971561077,18.511885224267,-330.457934858882)) ;
#43795 = CARTESIAN_POINT('Ctrl Pts',(-1.3050631783048,18.5203866842054,-330.459431292795)) ;
#43796 = CARTESIAN_POINT('Ctrl Pts',(-0.998050736891243,18.540096875677,-330.463424609158)) ;
#43797 = CARTESIAN_POINT('Ctrl Pts',(-0.806438011670655,18.5494192627321,
-330.465933369702)) ;
#43798 = CARTESIAN_POINT('Ctrl Pts',(-0.265137891414773,18.5673514520463,
-330.473064661434)) ;
#43799 = CARTESIAN_POINT('Ctrl Pts',(0.0846964548702557,18.5690512321255,
-330.477726569645)) ;
#43800 = CARTESIAN_POINT('Ctrl Pts',(0.944716209138017,18.5489247062297,-330.489268022014)) ;
#43801 = CARTESIAN_POINT('Ctrl Pts',(1.45435325300007,18.5159377958033,-330.496180897783)) ;
#43802 = CARTESIAN_POINT('Ctrl Pts',(2.13144833796877,18.4439819671419,-330.505282965533)) ;
#43803 = CARTESIAN_POINT('Ctrl Pts',(2.30065958393488,18.4236399343413,-330.507550052675)) ;
#43804 = CARTESIAN_POINT('Ctrl Pts',(2.59566187134941,18.3840481175298,-330.511476914593)) ;
#43805 = CARTESIAN_POINT('Ctrl Pts',(2.72157975272574,18.3658293977838,-330.51314484999)) ;
#43806 = CARTESIAN_POINT('Ctrl Pts',(2.91790763442282,18.3353598241163,-330.515727535907)) ;
#43807 = CARTESIAN_POINT('Ctrl Pts',(2.98845094562475,18.3239942645186,-330.516651901171)) ;
#43808 = CARTESIAN_POINT('Ctrl Pts',(3.12012800451669,18.3019985444771,-330.518369393842)) ;
#43809 = CARTESIAN_POINT('Ctrl Pts',(3.18127747027054,18.2914685892794,-330.519163759142)) ;
#43810 = CARTESIAN_POINT('Ctrl Pts',(3.35400725115976,18.2608321006529,-330.521399854912)) ;
#43811 = CARTESIAN_POINT('Ctrl Pts',(3.46545789937346,18.2400097383763,-330.522833492951)) ;
#43812 = CARTESIAN_POINT('Ctrl Pts',(3.91002740191182,18.152728919914,-330.528526692099)) ;
#43813 = CARTESIAN_POINT('Ctrl Pts',(4.24148600860538,18.0781547438008,-330.532715109503)) ;
#43814 = CARTESIAN_POINT('Ctrl Pts',(4.66042007506674,17.9717431218927,-330.538020525971)) ;
#43815 = CARTESIAN_POINT('Ctrl Pts',(4.74995628512105,17.948286308442,-330.539155018645)) ;
#43816 = CARTESIAN_POINT('Ctrl Pts',(5.27296915614832,17.8070789640222,-330.54579214766)) ;
#43817 = CARTESIAN_POINT('Ctrl Pts',(5.70223304603178,17.6742978052518,-330.551284558652)) ;
#43818 = CARTESIAN_POINT('Ctrl Pts',(6.40224354314676,17.4296084892856,-330.560480792541)) ;
#43819 = CARTESIAN_POINT('Ctrl Pts',(6.67591198718012,17.3266319028515,-330.564137295782)) ;
#43820 = CARTESIAN_POINT('Ctrl Pts',(7.0819457151203,17.1628001430728,-330.569678279624)) ;
#43821 = CARTESIAN_POINT('Ctrl Pts',(7.21621285815448,17.1067804033833,-330.571529771928)) ;
#43822 = CARTESIAN_POINT('Ctrl Pts',(7.46381411742008,17.0000409174488,-330.574981784457)) ;
#43823 = CARTESIAN_POINT('Ctrl Pts',(7.57732470549655,16.9497511082243,-330.57657920176)) ;
#43824 = CARTESIAN_POINT('Ctrl Pts',(7.83362121755809,16.8331121763911,-330.580220594592)) ;
#43825 = CARTESIAN_POINT('Ctrl Pts',(7.97608468603455,16.7660776540508,-330.582269327131)) ;
#43826 = CARTESIAN_POINT('Ctrl Pts',(8.44374247239506,16.5387169922565,-330.58907612113)) ;
#43827 = CARTESIAN_POINT('Ctrl Pts',(8.76509259141467,16.3706779779518,-330.593886625509)) ;
#43828 = CARTESIAN_POINT('Ctrl Pts',(9.57457769856437,15.91671416956,-330.606304950867)) ;
#43829 = CARTESIAN_POINT('Ctrl Pts',(10.0549420818349,15.6176972135123,-330.613970637585)) ;
#43830 = CARTESIAN_POINT('Ctrl Pts',(10.6674054883339,15.1964658173426,-330.623914886536)) ;
#43831 = CARTESIAN_POINT('Ctrl Pts',(10.8124493873061,15.0936096272304,-330.626282169136)) ;
#43832 = CARTESIAN_POINT('Ctrl Pts',(11.0618242976338,14.9113288095529,-330.630360027915)) ;
#43833 = CARTESIAN_POINT('Ctrl Pts',(11.1668329019886,14.8328529516374,-330.632079595866)) ;
#43834 = CARTESIAN_POINT('Ctrl Pts',(11.3283788745497,14.7094372787573,-330.634723271198)) ;
#43835 = CARTESIAN_POINT('Ctrl Pts',(11.3854999046103,14.6652686618184,-330.635657703338)) ;
#43836 = CARTESIAN_POINT('Ctrl Pts',(11.4908750976571,14.5828009626417,-330.637379696597)) ;
#43837 = CARTESIAN_POINT('Ctrl Pts',(11.5391990744827,14.5445927804325,-330.638168628663)) ;
#43838 = CARTESIAN_POINT('Ctrl Pts',(11.6737859913536,14.4370863883866,-330.640365054213)) ;
#43839 = CARTESIAN_POINT('Ctrl Pts',(11.7596209988422,14.3672564109107,-330.641764918546)) ;
#43840 = CARTESIAN_POINT('Ctrl Pts',(12.3396772287036,13.8866781518124,-330.651236203986)) ;
#43841 = CARTESIAN_POINT('Ctrl Pts',(12.8129095368567,13.4512757650125,-330.659035247609)) ;
#43842 = CARTESIAN_POINT('Ctrl Pts',(13.5252414116801,12.7241185508863,-330.671527724634)) ;
#43843 = CARTESIAN_POINT('Ctrl Pts',(13.7796804841054,12.448122477662,-330.676156981096)) ;
#43844 = CARTESIAN_POINT('Ctrl Pts',(14.1654756076201,12.0033073898244,-330.683520318217)) ;
#43845 = CARTESIAN_POINT('Ctrl Pts',(14.3025789224492,11.8396082462023,-330.68621010401)) ;
#43846 = CARTESIAN_POINT('Ctrl Pts',(14.5200695499862,11.5706355311982,-330.690605657685)) ;
#43847 = CARTESIAN_POINT('Ctrl Pts',(14.6022074586778,11.4668026757767,-330.692296822623)) ;
#43848 = CARTESIAN_POINT('Ctrl Pts',(14.7606662782872,11.2620265454936,-330.695622348043)) ;
#43849 = CARTESIAN_POINT('Ctrl Pts',(14.837079663646,11.1611638233146,-330.697255824766)) ;
#43850 = CARTESIAN_POINT('Ctrl Pts',(15.0054393076973,10.93415089968,-330.70092278009)) ;
#43851 = CARTESIAN_POINT('Ctrl Pts',(15.0968377294883,10.8076063577771,-330.702960441803)) ;
#43852 = CARTESIAN_POINT('Ctrl Pts',(15.5928285095384,10.1023178330221,-330.714280342524)) ;
#43853 = CARTESIAN_POINT('Ctrl Pts',(15.9657426802518,9.5020092214521,-330.723805345154)) ;
#43854 = CARTESIAN_POINT('Ctrl Pts',(16.4398007717999,8.63183406651436,-330.737144509256)) ;
#43855 = CARTESIAN_POINT('Ctrl Pts',(16.5702748949346,8.37863944746278,-330.740969656312)) ;
#43856 = CARTESIAN_POINT('Ctrl Pts',(16.7732997251202,7.96134729735255,-330.747136047434)) ;
#43857 = CARTESIAN_POINT('Ctrl Pts',(16.8493878936984,7.7990231606987,-330.749501435829)) ;
#43858 = CARTESIAN_POINT('Ctrl Pts',(16.9562796271057,7.56211504431382,-330.752892970722)) ;
#43859 = CARTESIAN_POINT('Ctrl Pts',(16.9889665435267,7.48839225356145,-330.753939942318)) ;
#43860 = CARTESIAN_POINT('Ctrl Pts',(17.0476805726677,7.35360404775812,-330.755837214709)) ;
#43861 = CARTESIAN_POINT('Ctrl Pts',(17.0738624229277,7.29260771989684,-330.756689363579)) ;
#43862 = CARTESIAN_POINT('Ctrl Pts',(17.1377818994226,7.14146215730707,-330.758785892709)) ;
#43863 = CARTESIAN_POINT('Ctrl Pts',(17.1751359140834,7.05115285248894,-330.760025569413)) ;
#43864 = CARTESIAN_POINT('Ctrl Pts',(17.3324832943503,6.66207057259511,-330.765318662161)) ;
#43865 = CARTESIAN_POINT('Ctrl Pts',(17.4454069882982,6.36049820391623,-330.769301620633)) ;
#43866 = CARTESIAN_POINT('Ctrl Pts',(17.5813613865055,5.96650835964682,-330.774426246179)) ;
#43867 = CARTESIAN_POINT('Ctrl Pts',(17.6116041530699,5.87663929233429,-330.775589856258)) ;
#43868 = CARTESIAN_POINT('Ctrl Pts',(17.7504623036431,5.45330904603572,-330.781052110883)) ;
#43869 = CARTESIAN_POINT('Ctrl Pts',(17.850303590099,5.11704536422929,-330.785337317924)) ;
#43870 = CARTESIAN_POINT('Ctrl Pts',(18.0108946178227,4.51407365820172,-330.793020421365)) ;
#43871 = CARTESIAN_POINT('Ctrl Pts',(18.0753888958531,4.248470532261,-330.796404094652)) ;
#43872 = CARTESIAN_POINT('Ctrl Pts',(18.1801601453633,3.77128809313169,-330.802512228286)) ;
#43873 = CARTESIAN_POINT('Ctrl Pts',(18.2226635623305,3.56024848195099,-330.805223510444)) ;
#43874 = CARTESIAN_POINT('Ctrl Pts',(18.2854204969547,3.21799706598658,-330.809644639257)) ;
#43875 = CARTESIAN_POINT('Ctrl Pts',(18.3079534214318,3.0872235624646,-330.811339542366)) ;
#43876 = CARTESIAN_POINT('Ctrl Pts',(18.3492000632301,2.83148713834371,-330.814666222814)) ;
#43877 = CARTESIAN_POINT('Ctrl Pts',(18.3680438894766,2.70655241874825,-330.816297048297)) ;
#43878 = CARTESIAN_POINT('Ctrl Pts',(18.4114024266118,2.39774234540761,-330.82034251724)) ;
#43879 = CARTESIAN_POINT('Ctrl Pts',(18.4344394283744,2.21367352296865,-330.822766516354)) ;
#43880 = CARTESIAN_POINT('Ctrl Pts',(18.5072558371612,1.55146872798468,-330.831530158293)) ;
#43881 = CARTESIAN_POINT('Ctrl Pts',(18.5412200923983,1.07178776105259,-330.837963614467)) ;
#43882 = CARTESIAN_POINT('Ctrl Pts',(18.5722535928492,0.0979286306117823,
-330.851076039381)) ;
#43883 = CARTESIAN_POINT('Ctrl Pts',(18.568291445729,-0.395901093677352,-330.857751613595)) ;
#43884 = CARTESIAN_POINT('Ctrl Pts',(18.544654593739,-0.888979978073086,-330.86430516735)) ;
#43885 = CARTESIAN_POINT('Origin',(0.,0.,-315.477129595899)) ;
#43886 = CARTESIAN_POINT('',(18.5446545939399,-0.88897997388336,-332.65888667131)) ;
#43887 = CARTESIAN_POINT('',(18.5446545937435,-0.888979977979341,-332.362654732516)) ;
#43888 = CARTESIAN_POINT('',(18.544654593745,-0.888979977948782,-315.477129595899)) ;
#43889 = CARTESIAN_POINT('Ctrl Pts',(18.5446545941347,-0.888979969817794,
-332.65888667131)) ;
#43890 = CARTESIAN_POINT('Ctrl Pts',(18.549807122682,-0.781495138392689,-332.65744111959)) ;
#43891 = CARTESIAN_POINT('Ctrl Pts',(18.5540254542741,-0.673959749677189,
-332.655998027345)) ;
#43892 = CARTESIAN_POINT('Ctrl Pts',(18.5625531864199,-0.394553534468471,
-332.652260710908)) ;
#43893 = CARTESIAN_POINT('Ctrl Pts',(18.5654107839571,-0.222656339114593,
-332.649973388167)) ;
#43894 = CARTESIAN_POINT('Ctrl Pts',(18.5662305343021,0.0772676058847497,
-332.646015943345)) ;
#43895 = CARTESIAN_POINT('Ctrl Pts',(18.5652564444396,0.205279736459089,-332.644337495356)) ;
#43896 = CARTESIAN_POINT('Ctrl Pts',(18.5616731456678,0.404866537420916,-332.641742379208)) ;
#43897 = CARTESIAN_POINT('Ctrl Pts',(18.5599735727799,0.476453434465815,-332.640815953297)) ;
#43898 = CARTESIAN_POINT('Ctrl Pts',(18.5557735883991,0.618677214032688,-332.638985330595)) ;
#43899 = CARTESIAN_POINT('Ctrl Pts',(18.553283867115,0.689313221327153,-332.638081040308)) ;
#43900 = CARTESIAN_POINT('Ctrl Pts',(18.5453445207493,0.883117037619062,-332.635611442937)) ;
#43901 = CARTESIAN_POINT('Ctrl Pts',(18.5390713076382,1.00624759371806,-332.634055158421)) ;
#43902 = CARTESIAN_POINT('Ctrl Pts',(18.5186817551908,1.34083383255402,-332.629851165483)) ;
#43903 = CARTESIAN_POINT('Ctrl Pts',(18.5021706053315,1.55212514206539,-332.62722334177)) ;
#43904 = CARTESIAN_POINT('Ctrl Pts',(18.4258644882299,2.35202479411313,-332.617315128808)) ;
#43905 = CARTESIAN_POINT('Ctrl Pts',(18.3415651534932,2.9379401085981,-332.610129238686)) ;
#43906 = CARTESIAN_POINT('Ctrl Pts',(18.1989692959521,3.67666369827731,-332.60082916468)) ;
#43907 = CARTESIAN_POINT('Ctrl Pts',(18.1664539358332,3.83409581363103,-332.598833986268)) ;
#43908 = CARTESIAN_POINT('Ctrl Pts',(18.0824381810205,4.21578772559234,-332.59395653658)) ;
#43909 = CARTESIAN_POINT('Ctrl Pts',(18.0288054755193,4.43955060391422,-332.591063081894)) ;
#43910 = CARTESIAN_POINT('Ctrl Pts',(17.9370514416407,4.79322346820572,-332.586425045286)) ;
#43911 = CARTESIAN_POINT('Ctrl Pts',(17.9016443649152,4.9238130146975,-332.584698412051)) ;
#43912 = CARTESIAN_POINT('Ctrl Pts',(17.8303951398075,5.17566365698886,-332.581339738305)) ;
#43913 = CARTESIAN_POINT('Ctrl Pts',(17.7947353896132,5.29696870781754,-332.579709005057)) ;
#43914 = CARTESIAN_POINT('Ctrl Pts',(17.714149104945,5.56110025666202,-332.57612918988)) ;
#43915 = CARTESIAN_POINT('Ctrl Pts',(17.6687283038838,5.70376670393188,-332.574176898779)) ;
#43916 = CARTESIAN_POINT('Ctrl Pts',(17.3868838103935,6.55334922010558,-332.562439959055)) ;
#43917 = CARTESIAN_POINT('Ctrl Pts',(17.1097877719656,7.24605184294243,-332.552376386737)) ;
#43918 = CARTESIAN_POINT('Ctrl Pts',(16.6226325593421,8.27887961503089,-332.537010334729)) ;
#43919 = CARTESIAN_POINT('Ctrl Pts',(16.4420112256915,8.63203503321068,-332.531694544842)) ;
#43920 = CARTESIAN_POINT('Ctrl Pts',(16.2020137445322,9.06637661318281,-332.525183802754)) ;
#43921 = CARTESIAN_POINT('Ctrl Pts',(16.1531062217308,9.1532285944377,-332.523883429686)) ;
#43922 = CARTESIAN_POINT('Ctrl Pts',(16.0703500834186,9.29746121219674,-332.52172919014)) ;
#43923 = CARTESIAN_POINT('Ctrl Pts',(16.0368877934428,9.35506102245181,-332.520870366894)) ;
#43924 = CARTESIAN_POINT('Ctrl Pts',(15.9627790855007,9.48106079043604,-332.518995572742)) ;
#43925 = CARTESIAN_POINT('Ctrl Pts',(15.9220015809274,9.54938194464102,-332.517981299589)) ;
#43926 = CARTESIAN_POINT('Ctrl Pts',(15.7914525268394,9.76495093601675,-332.514785194037)) ;
#43927 = CARTESIAN_POINT('Ctrl Pts',(15.7000678159441,9.91121135106646,-332.512622816313)) ;
#43928 = CARTESIAN_POINT('Ctrl Pts',(15.1515977814083,10.7624079985534,-332.50001896546)) ;
#43929 = CARTESIAN_POINT('Ctrl Pts',(14.649123808177,11.4369368134646,-332.489904354698)) ;
#43930 = CARTESIAN_POINT('Ctrl Pts',(13.9354617321469,12.2704328666442,-332.476251252102)) ;
#43931 = CARTESIAN_POINT('Ctrl Pts',(13.7641860659879,12.4622549320057,-332.473025864191)) ;
#43932 = CARTESIAN_POINT('Ctrl Pts',(13.4936432589056,12.7528690346586,-332.467993299187)) ;
#43933 = CARTESIAN_POINT('Ctrl Pts',(13.3971500553403,12.8541995992538,-332.466210113709)) ;
#43934 = CARTESIAN_POINT('Ctrl Pts',(13.2123268252194,13.0439463078578,-332.462814949249)) ;
#43935 = CARTESIAN_POINT('Ctrl Pts',(13.1242314196923,13.1325802875496,-332.461205136951)) ;
#43936 = CARTESIAN_POINT('Ctrl Pts',(12.9187006471593,13.3352338531682,-332.457468131073)) ;
#43937 = CARTESIAN_POINT('Ctrl Pts',(12.8006389329762,13.4486033149329,-332.455335270008)) ;
#43938 = CARTESIAN_POINT('Ctrl Pts',(12.3502811365066,13.869758356576,-332.447251320563)) ;
#43939 = CARTESIAN_POINT('Ctrl Pts',(12.0082596987081,14.1669099653063,-332.441212524246)) ;
#43940 = CARTESIAN_POINT('Ctrl Pts',(11.6251546450346,14.4759048234444,-332.434600358558)) ;
#43941 = CARTESIAN_POINT('Ctrl Pts',(11.5945153010191,14.5004570932174,-332.434072595585)) ;
#43942 = CARTESIAN_POINT('Ctrl Pts',(11.1636381964721,14.8434936595125,-332.426666140075)) ;
#43943 = CARTESIAN_POINT('Ctrl Pts',(10.7504837829534,15.1454026115569,-332.419743338692)) ;
#43944 = CARTESIAN_POINT('Ctrl Pts',(10.1727890915306,15.5319856287705,-332.410502354599)) ;
#43945 = CARTESIAN_POINT('Ctrl Pts',(10.018679129557,15.6318355985427,-332.408078385857)) ;
#43946 = CARTESIAN_POINT('Ctrl Pts',(9.79422237962059,15.7725812536972,-332.404620432278)) ;
#43947 = CARTESIAN_POINT('Ctrl Pts',(9.72504838303429,15.8153262817544,-332.403564522606)) ;
#43948 = CARTESIAN_POINT('Ctrl Pts',(9.599006512591,15.8920723314215,-332.401659843577)) ;
#43949 = CARTESIAN_POINT('Ctrl Pts',(9.54223336082573,15.9262259025619,-332.400809109733)) ;
#43950 = CARTESIAN_POINT('Ctrl Pts',(9.40223221098179,16.0094303929321,-332.398728101208)) ;
#43951 = CARTESIAN_POINT('Ctrl Pts',(9.31880185771756,16.0581370037351,-332.397502348841)) ;
#43952 = CARTESIAN_POINT('Ctrl Pts',(8.99876857171655,16.2416382398168,-332.392848390569)) ;
#43953 = CARTESIAN_POINT('Ctrl Pts',(8.75959023009571,16.3718730787138,-332.389469108606)) ;
#43954 = CARTESIAN_POINT('Ctrl Pts',(7.99753636437719,16.7653370039253,-332.378898453835)) ;
#43955 = CARTESIAN_POINT('Ctrl Pts',(7.46503062565287,17.0091279008574,-332.371786955298)) ;
#43956 = CARTESIAN_POINT('Ctrl Pts',(6.70699416531564,17.3137046618252,-332.361687555079)) ;
#43957 = CARTESIAN_POINT('Ctrl Pts',(6.49049194098694,17.3960240854922,-332.358807284647)) ;
#43958 = CARTESIAN_POINT('Ctrl Pts',(6.09178352230214,17.539143141048,-332.353493805869)) ;
#43959 = CARTESIAN_POINT('Ctrl Pts',(5.91006512688105,17.6012073060264,-332.351068725161)) ;
#43960 = CARTESIAN_POINT('Ctrl Pts',(5.60501782098526,17.700136493211,-332.346986704977)) ;
#43961 = CARTESIAN_POINT('Ctrl Pts',(5.48220940392533,17.7385579077676,-332.345340404376)) ;
#43962 = CARTESIAN_POINT('Ctrl Pts',(5.2479779908468,17.8091739115513,-332.342193862824)) ;
#43963 = CARTESIAN_POINT('Ctrl Pts',(5.1366332503701,17.8416071925664,-332.340695324067)) ;
#43964 = CARTESIAN_POINT('Ctrl Pts',(4.8393466680386,17.9251893063669,-332.336686494892)) ;
#43965 = CARTESIAN_POINT('Ctrl Pts',(4.65289962161678,17.9744878305147,-332.334164148901)) ;
#43966 = CARTESIAN_POINT('Ctrl Pts',(4.12886536216532,18.104347778357,-332.327054360683)) ;
#43967 = CARTESIAN_POINT('Ctrl Pts',(3.78973842521158,18.1783612973032,-332.322428693141)) ;
#43968 = CARTESIAN_POINT('Ctrl Pts',(2.94666925870943,18.3377403420374,-332.310917710426)) ;
#43969 = CARTESIAN_POINT('Ctrl Pts',(2.44089739739492,18.4118874597571,-332.303998350793)) ;
#43970 = CARTESIAN_POINT('Ctrl Pts',(1.76315019111453,18.4828262822888,-332.294888972572)) ;
#43971 = CARTESIAN_POINT('Ctrl Pts',(1.59335062937464,18.4982377506453,-332.292620963726)) ;
#43972 = CARTESIAN_POINT('Ctrl Pts',(1.29647590031274,18.5210649023294,-332.288692707784)) ;
#43973 = CARTESIAN_POINT('Ctrl Pts',(1.16949187160357,18.5295165538559,-332.287024292567)) ;
#43974 = CARTESIAN_POINT('Ctrl Pts',(0.9710841898059,18.5406742419482,-332.284441039087)) ;
#43975 = CARTESIAN_POINT('Ctrl Pts',(0.899714873390939,18.5442745615462,-332.28351657957)) ;
#43976 = CARTESIAN_POINT('Ctrl Pts',(0.766343673871551,18.5502308963782,-332.28179904819)) ;
#43977 = CARTESIAN_POINT('Ctrl Pts',(0.704347327440994,18.552688316967,-332.281004737179)) ;
#43978 = CARTESIAN_POINT('Ctrl Pts',(0.529057906255504,18.5587565666582,-332.278769032386)) ;
#43979 = CARTESIAN_POINT('Ctrl Pts',(0.415742335773235,18.5616407124527,-332.277335726447)) ;
#43980 = CARTESIAN_POINT('Ctrl Pts',(0.0693115659325736,18.5672842219207,
-332.272981803393)) ;
#43981 = CARTESIAN_POINT('Ctrl Pts',(-0.163835487773185,18.5666907591766,
-332.270090173147)) ;
#43982 = CARTESIAN_POINT('Ctrl Pts',(-0.986102803364694,18.5491080095177,
-332.259950270748)) ;
#43983 = CARTESIAN_POINT('Ctrl Pts',(-1.57436197876308,18.5084627287234,-332.252791425826)) ;
#43984 = CARTESIAN_POINT('Ctrl Pts',(-2.31906779467445,18.4212424554523,-332.243522692214)) ;
#43985 = CARTESIAN_POINT('Ctrl Pts',(-2.47819651328581,18.4005106180862,-332.24153092838)) ;
#43986 = CARTESIAN_POINT('Ctrl Pts',(-2.86452019720768,18.345076665137,-332.23666016997)) ;
#43987 = CARTESIAN_POINT('Ctrl Pts',(-3.09137803399052,18.3082138774632,-332.233769998456)) ;
#43988 = CARTESIAN_POINT('Ctrl Pts',(-3.45056971924063,18.2429811602815,-332.229135871343)) ;
#43989 = CARTESIAN_POINT('Ctrl Pts',(-3.58337856930062,18.2173596046806,-332.227409808361)) ;
#43990 = CARTESIAN_POINT('Ctrl Pts',(-3.83979184654705,18.1649797373889,-332.224051428984)) ;
#43991 = CARTESIAN_POINT('Ctrl Pts',(-3.96342630264408,18.1384051717356,-332.222420410533)) ;
#43992 = CARTESIAN_POINT('Ctrl Pts',(-4.26037602091029,18.0713963451136,-332.218474134592)) ;
#43993 = CARTESIAN_POINT('Ctrl Pts',(-4.43340010096782,18.02972914661,-332.216150919435)) ;
#43994 = CARTESIAN_POINT('Ctrl Pts',(-5.00416456956719,17.8835661761346,-332.208409585335)) ;
#43995 = CARTESIAN_POINT('Ctrl Pts',(-5.39903066813865,17.7683445645606,-332.20292582453)) ;
#43996 = CARTESIAN_POINT('Ctrl Pts',(-6.25178648474601,17.4884575226222,-332.190872454635)) ;
#43997 = CARTESIAN_POINT('Ctrl Pts',(-6.70769267480531,17.3187135609337,-332.184290612481)) ;
#43998 = CARTESIAN_POINT('Ctrl Pts',(-7.3782482857547,17.0385959802947,-332.174580095819)) ;
#43999 = CARTESIAN_POINT('Ctrl Pts',(-7.59826845615552,16.9416238186769,-332.171390033838)) ;
#44000 = CARTESIAN_POINT('Ctrl Pts',(-7.89686119614982,16.8030343213242,-332.167083336066)) ;
#44001 = CARTESIAN_POINT('Ctrl Pts',(-7.97710997844837,16.7650856120041,-332.165928187547)) ;
#44002 = CARTESIAN_POINT('Ctrl Pts',(-8.11631926401209,16.698029345755,-332.16393035829)) ;
#44003 = CARTESIAN_POINT('Ctrl Pts',(-8.1754028196708,16.6691814789894,-332.163084472881)) ;
#44004 = CARTESIAN_POINT('Ctrl Pts',(-8.31123330013605,16.6019656179091,-332.161144487101)) ;
#44005 = CARTESIAN_POINT('Ctrl Pts',(-8.38786982435409,16.5633783143841,-332.160053154124)) ;
#44006 = CARTESIAN_POINT('Ctrl Pts',(-8.64060995370358,16.4339170254216,-332.156460633363)) ;
#44007 = CARTESIAN_POINT('Ctrl Pts',(-8.81552630842516,16.3407547356567,-332.153984876491)) ;
#44008 = CARTESIAN_POINT('Ctrl Pts',(-9.03816107448489,16.2175618127977,-332.150829232131)) ;
#44009 = CARTESIAN_POINT('Ctrl Pts',(-9.08728011015319,16.1900897762684,-332.150132740655)) ;
#44010 = CARTESIAN_POINT('Ctrl Pts',(-9.22120697819413,16.1143836382101,-332.148232133249)) ;
#44011 = CARTESIAN_POINT('Ctrl Pts',(-9.30576073844549,16.0657036966129,-332.147030463072)) ;
#44012 = CARTESIAN_POINT('Ctrl Pts',(-9.85890925570984,15.7414087704791,-332.139147988091)) ;
#44013 = CARTESIAN_POINT('Ctrl Pts',(-10.3155886990881,15.445992107346,-332.132531119088)) ;
#44014 = CARTESIAN_POINT('Ctrl Pts',(-10.9419331163267,15.000639239088,-332.123022636887)) ;
#44015 = CARTESIAN_POINT('Ctrl Pts',(-11.1228370586685,14.8669961139795,-332.12022354312)) ;
#44016 = CARTESIAN_POINT('Ctrl Pts',(-11.4504935675418,14.615610573834,-332.115040357684)) ;
#44017 = CARTESIAN_POINT('Ctrl Pts',(-11.5979703829345,14.4988605835497,-332.112663686875)) ;
#44018 = CARTESIAN_POINT('Ctrl Pts',(-11.8428089869817,14.298907853711,-332.108638495641)) ;
#44019 = CARTESIAN_POINT('Ctrl Pts',(-11.9411299575785,14.216902116562,-332.106999932647)) ;
#44020 = CARTESIAN_POINT('Ctrl Pts',(-12.139362567579,14.0480566872367,-332.103649814877)) ;
#44021 = CARTESIAN_POINT('Ctrl Pts',(-12.2392095031714,13.9611522056943,-332.101937762266)) ;
#44022 = CARTESIAN_POINT('Ctrl Pts',(-12.4975661940141,13.7313826984516,-332.097442367107)) ;
#44023 = CARTESIAN_POINT('Ctrl Pts',(-12.6545571176853,13.5868397888012,-332.094644894841)) ;
#44024 = CARTESIAN_POINT('Ctrl Pts',(-13.0736108157426,13.1874485506062,-332.087000375313)) ;
#44025 = CARTESIAN_POINT('Ctrl Pts',(-13.3306951254719,12.9275158326647,-332.082114429343)) ;
#44026 = CARTESIAN_POINT('Ctrl Pts',(-14.0278265935417,12.1797370741932,-332.06837410686)) ;
#44027 = CARTESIAN_POINT('Ctrl Pts',(-14.4499043209779,11.6758802185596,-332.059457614808)) ;
#44028 = CARTESIAN_POINT('Ctrl Pts',(-14.9095618170519,11.0639613116525,-332.049396399595)) ;
#44029 = CARTESIAN_POINT('Ctrl Pts',(-14.9739702815395,10.9766337072438,-332.047978287905)) ;
#44030 = CARTESIAN_POINT('Ctrl Pts',(-15.0770662924487,10.8342557420151,-332.045698096177)) ;
#44031 = CARTESIAN_POINT('Ctrl Pts',(-15.1162266290251,10.7795509187291,-332.044829539051)) ;
#44032 = CARTESIAN_POINT('Ctrl Pts',(-15.1986425315683,10.6630881759881,-332.042997316525)) ;
#44033 = CARTESIAN_POINT('Ctrl Pts',(-15.241820923789,10.6012772437411,-332.042034684985)) ;
#44034 = CARTESIAN_POINT('Ctrl Pts',(-15.3687001440728,10.4172689734459,-332.039195359237)) ;
#44035 = CARTESIAN_POINT('Ctrl Pts',(-15.4513166261285,10.2943310430235,-332.037332544137)) ;
#44036 = CARTESIAN_POINT('Ctrl Pts',(-15.6487065940519,9.99287336646802,-332.032832334635)) ;
#44037 = CARTESIAN_POINT('Ctrl Pts',(-15.7619073672448,9.81334869196136,-332.030208875802)) ;
#44038 = CARTESIAN_POINT('Ctrl Pts',(-16.1934971425816,9.10215161073052,-332.019971947279)) ;
#44039 = CARTESIAN_POINT('Ctrl Pts',(-16.4882631041592,8.55661701258747,-332.012442079409)) ;
#44040 = CARTESIAN_POINT('Ctrl Pts',(-16.8782807517906,7.73949515207647,-332.001206907818)) ;
#44041 = CARTESIAN_POINT('Ctrl Pts',(-16.9953944594917,7.47881762195041,-331.997631340447)) ;
#44042 = CARTESIAN_POINT('Ctrl Pts',(-17.1625964651567,7.08241884168303,-331.992185373938)) ;
#44043 = CARTESIAN_POINT('Ctrl Pts',(-17.2171920751507,6.94864526685041,-331.990346172324)) ;
#44044 = CARTESIAN_POINT('Ctrl Pts',(-17.3158209906011,6.69867739422563,-331.986905106338)) ;
#44045 = CARTESIAN_POINT('Ctrl Pts',(-17.3602600745358,6.58265185952819,-331.985306181384)) ;
#44046 = CARTESIAN_POINT('Ctrl Pts',(-17.4588547502433,6.31728759638807,-331.981644679739)) ;
#44047 = CARTESIAN_POINT('Ctrl Pts',(-17.5122650125048,6.16768236795628,-331.979577130581)) ;
#44048 = CARTESIAN_POINT('Ctrl Pts',(-17.6944191665561,5.63600684395028,-331.972218226346)) ;
#44049 = CARTESIAN_POINT('Ctrl Pts',(-17.812631024771,5.25044924461633,-331.966859117515)) ;
#44050 = CARTESIAN_POINT('Ctrl Pts',(-18.0880249195642,4.23538935364533,-331.952760877219)) ;
#44051 = CARTESIAN_POINT('Ctrl Pts',(-18.224934926767,3.60096010385872,-331.943949095296)) ;
#44052 = CARTESIAN_POINT('Ctrl Pts',(-18.354300904181,2.80010566932789,-331.933190710941)) ;
#44053 = CARTESIAN_POINT('Ctrl Pts',(-18.3781268292017,2.63920591150181,-331.931048473519)) ;
#44054 = CARTESIAN_POINT('Ctrl Pts',(-18.4102387373538,2.40076742977382,-331.927912089315)) ;
#44055 = CARTESIAN_POINT('Ctrl Pts',(-18.4201554109191,2.32345632151092,-331.926901083589)) ;
#44056 = CARTESIAN_POINT('Ctrl Pts',(-18.4376988707512,2.17950865988861,-331.925031166317)) ;
#44057 = CARTESIAN_POINT('Ctrl Pts',(-18.445451957283,2.11288895321875,-331.924170888186)) ;
#44058 = CARTESIAN_POINT('Ctrl Pts',(-18.4641932931997,1.94388000924365,-331.922000292302)) ;
#44059 = CARTESIAN_POINT('Ctrl Pts',(-18.4746909976233,1.84143858090557,-331.920695530287)) ;
#44060 = CARTESIAN_POINT('Ctrl Pts',(-18.4962502282,1.61226806216169,-331.917796287431)) ;
#44061 = CARTESIAN_POINT('Ctrl Pts',(-18.5068626495285,1.48550184971682,-331.916205942429)) ;
#44062 = CARTESIAN_POINT('Ctrl Pts',(-18.5370632018517,1.07391375680445,-331.911073602429)) ;
#44063 = CARTESIAN_POINT('Ctrl Pts',(-18.5513849105104,0.788746615629087,
-331.907565632499)) ;
#44064 = CARTESIAN_POINT('Ctrl Pts',(-18.5782190912367,-0.200637317172788,
-331.89543262566)) ;
#44065 = CARTESIAN_POINT('Ctrl Pts',(-18.5572405141425,-0.905154107683385,
-331.886837573715)) ;
#44066 = CARTESIAN_POINT('Ctrl Pts',(-18.482756003825,-1.76258047396206,-331.876009761189)) ;
#44067 = CARTESIAN_POINT('Ctrl Pts',(-18.4672525632684,-1.91821325567096,
-331.874030727184)) ;
#44068 = CARTESIAN_POINT('Ctrl Pts',(-18.4356442133644,-2.19944320287778,
-331.87042684652)) ;
#44069 = CARTESIAN_POINT('Ctrl Pts',(-18.4202173037977,-2.32510696351003,
-331.86880645419)) ;
#44070 = CARTESIAN_POINT('Ctrl Pts',(-18.3860454622188,-2.58173021350686,
-331.865475793732)) ;
#44071 = CARTESIAN_POINT('Ctrl Pts',(-18.3671836865879,-2.71266695255667,
-331.863764847945)) ;
#44072 = CARTESIAN_POINT('Ctrl Pts',(-18.314315537329,-3.05379766475358,-331.859276691535)) ;
#44073 = CARTESIAN_POINT('Ctrl Pts',(-18.2780898313619,-3.26362768249181,
-331.856485439161)) ;
#44074 = CARTESIAN_POINT('Ctrl Pts',(-18.1685694300383,-3.83880301681021,
-331.848754020709)) ;
#44075 = CARTESIAN_POINT('Ctrl Pts',(-18.0878735331925,-4.20263652678464,
-331.843772455376)) ;
#44076 = CARTESIAN_POINT('Ctrl Pts',(-17.8369727094456,-5.19200689056596,
-331.83005204173)) ;
#44077 = CARTESIAN_POINT('Ctrl Pts',(-17.6448752355142,-5.81144634958503,
-331.821256627717)) ;
#44078 = CARTESIAN_POINT('Ctrl Pts',(-17.3828153877897,-6.52259802301906,
-331.811290390954)) ;
#44079 = CARTESIAN_POINT('Ctrl Pts',(-17.343935905551,-6.62528815485775,-331.809855037285)) ;
#44080 = CARTESIAN_POINT('Ctrl Pts',(-17.2818738063739,-6.7849182387354,-331.80763302811)) ;
#44081 = CARTESIAN_POINT('Ctrl Pts',(-17.2593154769174,-6.84209814715091,
-331.80683896384)) ;
#44082 = CARTESIAN_POINT('Ctrl Pts',(-17.2095486636328,-6.96643266519715,
-331.805117228929)) ;
#44083 = CARTESIAN_POINT('Ctrl Pts',(-17.1822301862727,-7.03354214666233,
-331.804191000133)) ;
#44084 = CARTESIAN_POINT('Ctrl Pts',(-17.1038883530322,-7.22281309858469,
-331.801585299412)) ;
#44085 = CARTESIAN_POINT('Ctrl Pts',(-17.0519501789276,-7.34459127760275,
-331.799916534015)) ;
#44086 = CARTESIAN_POINT('Ctrl Pts',(-16.9262038767758,-7.63090009558715,
-331.796001182187)) ;
#44087 = CARTESIAN_POINT('Ctrl Pts',(-16.8512923805617,-7.7949316355332,-331.793764295144)) ;
#44088 = CARTESIAN_POINT('Ctrl Pts',(-16.522771143864,-8.48740750170448,-331.784304876384)) ;
#44089 = CARTESIAN_POINT('Ctrl Pts',(-16.2466022108365,-9.00477488440505,
-331.777186250456)) ;
#44090 = CARTESIAN_POINT('Ctrl Pts',(-15.7719329963083,-9.80085278874171,
-331.765741430216)) ;
#44091 = CARTESIAN_POINT('Ctrl Pts',(-15.5894200194946,-10.0886356137815,
-331.761498829468)) ;
#44092 = CARTESIAN_POINT('Ctrl Pts',(-15.3118355723882,-10.5007899538457,
-331.755226136013)) ;
#44093 = CARTESIAN_POINT('Ctrl Pts',(-15.2229476208506,-10.6292409835721,
-331.753242599147)) ;
#44094 = CARTESIAN_POINT('Ctrl Pts',(-15.060561513905,-10.8576876914856,-331.749660603606)) ;
#44095 = CARTESIAN_POINT('Ctrl Pts',(-14.9876616231509,-10.9580971951812,
-331.748066943469)) ;
#44096 = CARTESIAN_POINT('Ctrl Pts',(-14.8265571237866,-11.1753809992731,
-331.744575225948)) ;
#44097 = CARTESIAN_POINT('Ctrl Pts',(-14.7379653691483,-11.291957904565,-331.742674122081)) ;
#44098 = CARTESIAN_POINT('Ctrl Pts',(-14.4644798384884,-11.643132666103,-331.736862131884)) ;
#44099 = CARTESIAN_POINT('Ctrl Pts',(-14.2752958122166,-11.8743271014631,
-331.732917557379)) ;
#44100 = CARTESIAN_POINT('Ctrl Pts',(-13.7758045688742,-12.4555376226363,
-331.72271140743)) ;
#44101 = CARTESIAN_POINT('Ctrl Pts',(-13.4576999457132,-12.7985749121859,
-331.716402170961)) ;
#44102 = CARTESIAN_POINT('Ctrl Pts',(-13.0175413938636,-13.2386580457913,
-331.708021896245)) ;
#44103 = CARTESIAN_POINT('Ctrl Pts',(-12.9067345198133,-13.3467095145243,
-331.705940395454)) ;
#44104 = CARTESIAN_POINT('Ctrl Pts',(-12.585874295672,-13.6518581169642,-331.700005083862)) ;
#44105 = CARTESIAN_POINT('Ctrl Pts',(-12.3725675824531,-13.8454697949743,
-331.696168941875)) ;
#44106 = CARTESIAN_POINT('Ctrl Pts',(-12.0903131565385,-14.0899295538039,
-331.691276097674)) ;
#44107 = CARTESIAN_POINT('Ctrl Pts',(-12.0253987302987,-14.1453728285473,
-331.690163031979)) ;
#44108 = CARTESIAN_POINT('Ctrl Pts',(-11.9088513873796,-14.243533560263,-331.68818812439)) ;
#44109 = CARTESIAN_POINT('Ctrl Pts',(-11.8573652216639,-14.2864229143945,
-331.687323798843)) ;
#44110 = CARTESIAN_POINT('Ctrl Pts',(-11.7453469840887,-14.378714410044,-331.685461532607)) ;
#44111 = CARTESIAN_POINT('Ctrl Pts',(-11.6847330806349,-14.4280149957899,
-331.684465030554)) ;
#44112 = CARTESIAN_POINT('Ctrl Pts',(-11.496118967138,-14.5794569338287,-331.681395705522)) ;
#44113 = CARTESIAN_POINT('Ctrl Pts',(-11.367077125032,-14.6802886069379,-331.679340252255)) ;
#44114 = CARTESIAN_POINT('Ctrl Pts',(-10.8345928260364,-15.0851342673703,
-331.67100485757)) ;
#44115 = CARTESIAN_POINT('Ctrl Pts',(-10.4201564032763,-15.3743299149691,
-331.664849149507)) ;
#44116 = CARTESIAN_POINT('Ctrl Pts',(-9.55254222534979,-15.9285401780937,
-331.652227925905)) ;
#44117 = CARTESIAN_POINT('Ctrl Pts',(-9.09888186648572,-16.1919672162433,
-331.645764047552)) ;
#44118 = CARTESIAN_POINT('Ctrl Pts',(-8.50170607225066,-16.5056976929444,
-331.637266746582)) ;
#44119 = CARTESIAN_POINT('Ctrl Pts',(-8.36788715208434,-16.5739412028438,
-331.635363940735)) ;
#44120 = CARTESIAN_POINT('Ctrl Pts',(-8.11984223289753,-16.6966665136509,
-331.631836754783)) ;
#44121 = CARTESIAN_POINT('Ctrl Pts',(-8.00585889708348,-16.7516188418197,
-331.63021586359)) ;
#44122 = CARTESIAN_POINT('Ctrl Pts',(-7.76905820725154,-16.8628134880897,
-331.626847376093)) ;
#44123 = CARTESIAN_POINT('Ctrl Pts',(-7.64617082176527,-16.9188893211251,
-331.625098706403)) ;
#44124 = CARTESIAN_POINT('Ctrl Pts',(-7.31352357533365,-17.0663180829324,
-331.620363199763)) ;
#44125 = CARTESIAN_POINT('Ctrl Pts',(-7.1026693458332,-17.1551428982102,-331.617359216536)) ;
#44126 = CARTESIAN_POINT('Ctrl Pts',(-6.74222807817581,-17.2991983230211,
-331.6122239784)) ;
#44127 = CARTESIAN_POINT('Ctrl Pts',(-6.593472910062,-17.3564402162134,-331.610104690238)) ;
#44128 = CARTESIAN_POINT('Ctrl Pts',(-5.8994400066628,-17.6132980899344,-331.600225387217)) ;
#44129 = CARTESIAN_POINT('Ctrl Pts',(-5.3457271956127,-17.7891781870182,-331.592356568875)) ;
#44130 = CARTESIAN_POINT('Ctrl Pts',(-4.51125014092158,-18.0117519289392,
-331.580782584627)) ;
#44131 = CARTESIAN_POINT('Ctrl Pts',(-4.236182275916,-18.0784221014574,-331.5770145252)) ;
#44132 = CARTESIAN_POINT('Ctrl Pts',(-3.87623896552559,-18.1569977751432,
-331.572186867686)) ;
#44133 = CARTESIAN_POINT('Ctrl Pts',(-3.79265524224161,-18.1746406557301,
-331.571073047531)) ;
#44134 = CARTESIAN_POINT('Ctrl Pts',(-3.64328296360497,-18.2050949028238,
-331.569097235563)) ;
#44135 = CARTESIAN_POINT('Ctrl Pts',(-3.57754117068616,-18.2181280702942,
-331.568232752751)) ;
#44136 = CARTESIAN_POINT('Ctrl Pts',(-3.43504503767567,-18.2455765537329,
-331.566370786161)) ;
#44137 = CARTESIAN_POINT('Ctrl Pts',(-3.35826753299521,-18.2598641119797,
-331.565374734357)) ;
#44138 = CARTESIAN_POINT('Ctrl Pts',(-3.12043525453086,-18.3025716510351,
-331.562308562521)) ;
#44139 = CARTESIAN_POINT('Ctrl Pts',(-2.95909324587885,-18.3293483937127,
-331.560255761816)) ;
#44140 = CARTESIAN_POINT('Ctrl Pts',(-2.29837045352273,-18.4300522776387,
-331.551927054896)) ;
#44141 = CARTESIAN_POINT('Ctrl Pts',(-1.79642693013304,-18.4857292583713,
-331.545775359711)) ;
#44142 = CARTESIAN_POINT('Ctrl Pts',(-0.812797026515212,-18.5543909502474,
-331.533687473049)) ;
#44143 = CARTESIAN_POINT('Ctrl Pts',(-0.331634497858101,-18.5692239972279,
-331.527759330114)) ;
#44144 = CARTESIAN_POINT('Ctrl Pts',(0.335011049879787,-18.5638536358676,
-331.519388768985)) ;
#44145 = CARTESIAN_POINT('Ctrl Pts',(0.520430378490183,-18.5595809834996,
-331.517044472027)) ;
#44146 = CARTESIAN_POINT('Ctrl Pts',(0.832001976769622,-18.5477285307899,
-331.513073261548)) ;
#44147 = CARTESIAN_POINT('Ctrl Pts',(0.958197217835081,-18.5416374406286,
-331.511456020372)) ;
#44148 = CARTESIAN_POINT('Ctrl Pts',(1.2168000838953,-18.5265082493368,-331.50812288899)) ;
#44149 = CARTESIAN_POINT('Ctrl Pts',(1.34919279268154,-18.5173375273755,-331.506406227867)) ;
#44150 = CARTESIAN_POINT('Ctrl Pts',(1.69610351393776,-18.4895671278544,-331.50188069614)) ;
#44151 = CARTESIAN_POINT('Ctrl Pts',(1.91041589647847,-18.4686537288215,-331.499057329471)) ;
#44152 = CARTESIAN_POINT('Ctrl Pts',(2.39590829321267,-18.4127364592579,-331.492602293534)) ;
#44153 = CARTESIAN_POINT('Ctrl Pts',(2.66677643416566,-18.3754603618096,-331.48895856669)) ;
#44154 = CARTESIAN_POINT('Ctrl Pts',(3.28288049015549,-18.2767638210294,-331.480596404203)) ;
#44155 = CARTESIAN_POINT('Ctrl Pts',(3.62739871416073,-18.2115177380719,-331.475866068262)) ;
#44156 = CARTESIAN_POINT('Ctrl Pts',(4.06211988287781,-18.1163627901775,-331.469876197196)) ;
#44157 = CARTESIAN_POINT('Ctrl Pts',(4.15422219233511,-18.095465085836,-331.468606048662)) ;
#44158 = CARTESIAN_POINT('Ctrl Pts',(4.559525554593,-18.0002456461708,-331.463016086596)) ;
#44159 = CARTESIAN_POINT('Ctrl Pts',(4.87092308454382,-17.9184883751614,-331.458718829005)) ;
#44160 = CARTESIAN_POINT('Ctrl Pts',(5.2740535943237,-17.8013607134388,-331.453213303412)) ;
#44161 = CARTESIAN_POINT('Ctrl Pts',(5.36785214476087,-17.7733015491847,-331.451936506685)) ;
#44162 = CARTESIAN_POINT('Ctrl Pts',(5.52488445153144,-17.7249699538037,-331.449808603074)) ;
#44163 = CARTESIAN_POINT('Ctrl Pts',(5.58823923867938,-17.7050978622671,-331.448952823472)) ;
#44164 = CARTESIAN_POINT('Ctrl Pts',(5.72820564884005,-17.660369372822,-331.447068775207)) ;
#44165 = CARTESIAN_POINT('Ctrl Pts',(5.80476473127387,-17.6353534917356,-331.446042377354)) ;
#44166 = CARTESIAN_POINT('Ctrl Pts',(6.05057109729312,-17.5532615349998,-331.442756981622)) ;
#44167 = CARTESIAN_POINT('Ctrl Pts',(6.21915853939948,-17.4942410060972,-331.440518976821)) ;
#44168 = CARTESIAN_POINT('Ctrl Pts',(6.6527138797483,-17.3353989774364,-331.434776098598)) ;
#44169 = CARTESIAN_POINT('Ctrl Pts',(6.91629713058768,-17.231932395471,-331.431296590616)) ;
#44170 = CARTESIAN_POINT('Ctrl Pts',(7.8326643082319,-16.8478090348305,-331.419115265044)) ;
#44171 = CARTESIAN_POINT('Ctrl Pts',(8.47161110839537,-16.5357523040289,-331.410445819442)) ;
#44172 = CARTESIAN_POINT('Ctrl Pts',(9.22661848126712,-16.1117401110325,-331.399549676209)) ;
#44173 = CARTESIAN_POINT('Ctrl Pts',(9.36117863113241,-16.0339325353331,-331.397582551302)) ;
#44174 = CARTESIAN_POINT('Ctrl Pts',(9.60335744134876,-15.8898080428494,-331.393993254042)) ;
#44175 = CARTESIAN_POINT('Ctrl Pts',(9.71130616221606,-15.8240641541709,-331.392375409092)) ;
#44176 = CARTESIAN_POINT('Ctrl Pts',(9.93113454678339,-15.6870856100257,-331.389042781119)) ;
#44177 = CARTESIAN_POINT('Ctrl Pts',(10.0429391620492,-15.6157440183855,-331.387327245373)) ;
#44178 = CARTESIAN_POINT('Ctrl Pts',(10.3338336504723,-15.4257103199362,-331.382809072979)) ;
#44179 = CARTESIAN_POINT('Ctrl Pts',(10.5116442313536,-15.3050969318215,-331.379992030126)) ;
#44180 = CARTESIAN_POINT('Ctrl Pts',(10.9101489418954,-15.0245601684591,-331.373555269436)) ;
#44181 = CARTESIAN_POINT('Ctrl Pts',(11.1294957261104,-14.8628087071858,-331.369923603706)) ;
#44182 = CARTESIAN_POINT('Ctrl Pts',(11.6236155285815,-14.4813593904754,-331.361558434222)) ;
#44183 = CARTESIAN_POINT('Ctrl Pts',(11.895864919779,-14.2585625232433,-331.356812603603)) ;
#44184 = CARTESIAN_POINT('Ctrl Pts',(12.1713405341519,-14.0197408851476,-331.351905238972)) ;
#44185 = CARTESIAN_POINT('Ctrl Pts',(12.1810516282365,-14.0113042260604,-331.351732106986)) ;
#44186 = CARTESIAN_POINT('Ctrl Pts',(12.4691174520005,-13.7605168719309,-331.346592388863)) ;
#44187 = CARTESIAN_POINT('Ctrl Pts',(12.7401933053267,-13.5099293110937,-331.341642916547)) ;
#44188 = CARTESIAN_POINT('Ctrl Pts',(13.0860464946712,-13.1705437657862,-331.335263791768)) ;
#44189 = CARTESIAN_POINT('Ctrl Pts',(13.1677166864622,-13.0888912164082,-331.333752638941)) ;
#44190 = CARTESIAN_POINT('Ctrl Pts',(13.2923361147654,-12.9619517844708,-331.331443164222)) ;
#44191 = CARTESIAN_POINT('Ctrl Pts',(13.33582765902,-12.9172014814219,-331.330636478535)) ;
#44192 = CARTESIAN_POINT('Ctrl Pts',(13.4282651881927,-12.8211241103788,-331.328921334361)) ;
#44193 = CARTESIAN_POINT('Ctrl Pts',(13.4771443639001,-12.7697341095066,-331.328014043487)) ;
#44194 = CARTESIAN_POINT('Ctrl Pts',(13.6110335365427,-12.6273422848489,-331.32552585105)) ;
#44195 = CARTESIAN_POINT('Ctrl Pts',(13.6954243430963,-12.5357632097247,-331.323954196127)) ;
#44196 = CARTESIAN_POINT('Ctrl Pts',(13.8897140754676,-12.3206203347204,-331.320319419235)) ;
#44197 = CARTESIAN_POINT('Ctrl Pts',(13.9988963246096,-12.1964234243719,-331.318264232337)) ;
#44198 = CARTESIAN_POINT('Ctrl Pts',(14.416287535097,-11.7086432430554,-331.310327075914)) ;
#44199 = CARTESIAN_POINT('Ctrl Pts',(14.7121100633971,-11.3347029741908,-331.304522422716)) ;
#44200 = CARTESIAN_POINT('Ctrl Pts',(15.2590919205798,-10.5857376221815,-331.293132577096)) ;
#44201 = CARTESIAN_POINT('Ctrl Pts',(15.511620235248,-10.2121184692607,-331.287556523951)) ;
#44202 = CARTESIAN_POINT('Ctrl Pts',(15.8298309562162,-9.70224288055688,-331.279985662157)) ;
#44203 = CARTESIAN_POINT('Ctrl Pts',(15.9078139956106,-9.57384556028879,-331.278082751899)) ;
#44204 = CARTESIAN_POINT('Ctrl Pts',(16.0485996199982,-9.33557503486647,-331.274555440085)) ;
#44205 = CARTESIAN_POINT('Ctrl Pts',(16.1118535889376,-9.22597880279746,-331.272934528528)) ;
#44206 = CARTESIAN_POINT('Ctrl Pts',(16.2403002102788,-8.99807713892284,-331.269566072056)) ;
#44207 = CARTESIAN_POINT('Ctrl Pts',(16.3053321333934,-8.87968958196487,-331.267817454528)) ;
#44208 = CARTESIAN_POINT('Ctrl Pts',(16.4770092900949,-8.55891317545061,-331.263082291909)) ;
#44209 = CARTESIAN_POINT('Ctrl Pts',(16.581215168311,-8.35524584512619,-331.260078605022)) ;
#44210 = CARTESIAN_POINT('Ctrl Pts',(16.7515828989432,-8.00652016055762,-331.254943978081)) ;
#44211 = CARTESIAN_POINT('Ctrl Pts',(16.8196886150558,-7.8624404297601,-331.252825003968)) ;
#44212 = CARTESIAN_POINT('Ctrl Pts',(17.1272227276842,-7.1895543275475,-331.24294847965)) ;
#44213 = CARTESIAN_POINT('Ctrl Pts',(17.3436213189177,-6.65058246789319,-331.235082189139)) ;
#44214 = CARTESIAN_POINT('Ctrl Pts',(17.627519564387,-5.83483442152804,-331.223506895498)) ;
#44215 = CARTESIAN_POINT('Ctrl Pts',(17.7144902594939,-5.56521105949688,-331.219735182345)) ;
#44216 = CARTESIAN_POINT('Ctrl Pts',(17.8196119877708,-5.21183495058931,-331.214904127218)) ;
#44217 = CARTESIAN_POINT('Ctrl Pts',(17.8434008144712,-5.129799445204,-331.213790445708)) ;
#44218 = CARTESIAN_POINT('Ctrl Pts',(17.8848433319184,-4.98310845616582,-331.211814799966)) ;
#44219 = CARTESIAN_POINT('Ctrl Pts',(17.9027146294807,-4.91851601892527,-331.210950346085)) ;
#44220 = CARTESIAN_POINT('Ctrl Pts',(17.9406544522097,-4.77844295313092,-331.209088324576)) ;
#44221 = CARTESIAN_POINT('Ctrl Pts',(17.9605971858126,-4.70292972316742,-331.208092190145)) ;
#44222 = CARTESIAN_POINT('Ctrl Pts',(18.0208330490043,-4.46887394962515,-331.205025439859)) ;
#44223 = CARTESIAN_POINT('Ctrl Pts',(18.0595078288074,-4.30992288747495,-331.202972152571)) ;
#44224 = CARTESIAN_POINT('Ctrl Pts',(18.2089432480868,-3.65838523819651,-331.194642218824)) ;
#44225 = CARTESIAN_POINT('Ctrl Pts',(18.3016899892517,-3.16188907643606,-331.188489787503)) ;
#44226 = CARTESIAN_POINT('Ctrl Pts',(18.4430680056035,-2.18613150994227,-331.176402817181)) ;
#44227 = CARTESIAN_POINT('Ctrl Pts',(18.4935194747455,-1.70753173741242,-331.170476360176)) ;
#44228 = CARTESIAN_POINT('Ctrl Pts',(18.5327994065473,-1.1147295427976,-331.163016922969)) ;
#44229 = CARTESIAN_POINT('Ctrl Pts',(18.539242482585,-1.00187985714273,-331.161591898881)) ;
#44230 = CARTESIAN_POINT('Ctrl Pts',(18.5446545937584,-0.888979977668651,
-331.160160528407)) ;
#44231 = CARTESIAN_POINT('Ctrl Pts',(18.544654593739,-0.888979978073095,-330.86430516735)) ;
#44232 = CARTESIAN_POINT('Ctrl Pts',(18.5441097763335,-0.900345195346051,
-330.864456223428)) ;
#44233 = CARTESIAN_POINT('Ctrl Pts',(18.5435545061637,-0.911710013754673,
-330.864607211556)) ;
#44234 = CARTESIAN_POINT('Ctrl Pts',(18.5348507836707,-1.08655293568775,-330.866929103306)) ;
#44235 = CARTESIAN_POINT('Ctrl Pts',(18.5245512397169,-1.24991694824044,-330.869085215214)) ;
#44236 = CARTESIAN_POINT('Ctrl Pts',(18.5061469696207,-1.49101515632244,-330.872237563732)) ;
#44237 = CARTESIAN_POINT('Ctrl Pts',(18.4997095493716,-1.56886853138097,-330.873250895538)) ;
#44238 = CARTESIAN_POINT('Ctrl Pts',(18.4868372992938,-1.71342839907376,-330.875122446275)) ;
#44239 = CARTESIAN_POINT('Ctrl Pts',(18.4805322972729,-1.78014499661427,-330.875982063671)) ;
#44240 = CARTESIAN_POINT('Ctrl Pts',(18.4653723774058,-1.93179021210006,-330.877927551247)) ;
#44241 = CARTESIAN_POINT('Ctrl Pts',(18.4562924851722,-2.01669486741578,-330.879010892966)) ;
#44242 = CARTESIAN_POINT('Ctrl Pts',(18.4144730367111,-2.38377329764873,-330.883674247619)) ;
#44243 = CARTESIAN_POINT('Ctrl Pts',(18.3758455132984,-2.66523820544436,-330.887198317088)) ;
#44244 = CARTESIAN_POINT('Ctrl Pts',(18.2648938052935,-3.35567733726642,-330.89581417164)) ;
#44245 = CARTESIAN_POINT('Ctrl Pts',(18.1852774394334,-3.76332314152292,-330.900877732374)) ;
#44246 = CARTESIAN_POINT('Ctrl Pts',(18.0219310007999,-4.47236939637491,-330.909813241256)) ;
#44247 = CARTESIAN_POINT('Ctrl Pts',(17.9441300679829,-4.77496394854851,-330.913667590865)) ;
#44248 = CARTESIAN_POINT('Ctrl Pts',(17.7944207332213,-5.30173860754561,-330.920497826828)) ;
#44249 = CARTESIAN_POINT('Ctrl Pts',(17.7258147158665,-5.52678331913014,-330.923454754092)) ;
#44250 = CARTESIAN_POINT('Ctrl Pts',(17.6107652535368,-5.8799657432534,-330.928168356854)) ;
#44251 = CARTESIAN_POINT('Ctrl Pts',(17.5671559334044,-6.00900010839035,-330.929905985652)) ;
#44252 = CARTESIAN_POINT('Ctrl Pts',(17.4804553548932,-6.25652243519602,-330.933270674963)) ;
#44253 = CARTESIAN_POINT('Ctrl Pts',(17.4375691811663,-6.3750743834906,-330.934896251667)) ;
#44254 = CARTESIAN_POINT('Ctrl Pts',(17.3321846373426,-6.65737115925951,-330.938801366615)) ;
#44255 = CARTESIAN_POINT('Ctrl Pts',(17.2685685885039,-6.8206857293893,-330.941088429854)) ;
#44256 = CARTESIAN_POINT('Ctrl Pts',(16.9445284381231,-7.61895144320848,-330.952403088899)) ;
#44257 = CARTESIAN_POINT('Ctrl Pts',(16.6513495227622,-8.24002530095249,-330.961654295319)) ;
#44258 = CARTESIAN_POINT('Ctrl Pts',(16.1345251515381,-9.19405277906069,-330.97626331395)) ;
#44259 = CARTESIAN_POINT('Ctrl Pts',(15.9333390915501,-9.53845976463505,-330.981619257573)) ;
#44260 = CARTESIAN_POINT('Ctrl Pts',(15.6587906480133,-9.97549737373529,-330.988416315131)) ;
#44261 = CARTESIAN_POINT('Ctrl Pts',(15.5954211016994,-10.0742797825858,-330.989952483218)) ;
#44262 = CARTESIAN_POINT('Ctrl Pts',(15.4930181431378,-10.2306267590345,-330.99237947787)) ;
#44263 = CARTESIAN_POINT('Ctrl Pts',(15.4545905330348,-10.288584283351,-330.993278182759)) ;
#44264 = CARTESIAN_POINT('Ctrl Pts',(15.3804165740384,-10.3991021518454,-330.994988967119)) ;
#44265 = CARTESIAN_POINT('Ctrl Pts',(15.3447241745437,-10.4516974494597,-330.995801905428)) ;
#44266 = CARTESIAN_POINT('Ctrl Pts',(15.2396353103713,-10.6048547074545,-330.998167096647)) ;
#44267 = CARTESIAN_POINT('Ctrl Pts',(15.1695153439629,-10.704916256608,-330.999709709479)) ;
#44268 = CARTESIAN_POINT('Ctrl Pts',(14.9737474582542,-10.9784916136851,-331.003929616931)) ;
#44269 = CARTESIAN_POINT('Ctrl Pts',(14.8460760999724,-11.1505343256369,-331.006586092132)) ;
#44270 = CARTESIAN_POINT('Ctrl Pts',(14.3548839927377,-11.7890418912718,-331.016519408154)) ;
#44271 = CARTESIAN_POINT('Ctrl Pts',(13.9721238991995,-12.2402597394375,-331.023702298116)) ;
#44272 = CARTESIAN_POINT('Ctrl Pts',(13.4587842694715,-12.7898966129418,-331.032998896299)) ;
#44273 = CARTESIAN_POINT('Ctrl Pts',(13.3475642182002,-12.9059233977497,-331.034993696942)) ;
#44274 = CARTESIAN_POINT('Ctrl Pts',(13.0735143328098,-13.1844850527023,-331.039870406405)) ;
#44275 = CARTESIAN_POINT('Ctrl Pts',(12.9091429360226,-13.3454655780042,-331.042763497922)) ;
#44276 = CARTESIAN_POINT('Ctrl Pts',(12.6434200022662,-13.5962029582196,-331.047401101902)) ;
#44277 = CARTESIAN_POINT('Ctrl Pts',(12.5440053229398,-13.6879777406398,-331.049127671882)) ;
#44278 = CARTESIAN_POINT('Ctrl Pts',(12.3497617804306,-13.8634003642929,-331.052486312486)) ;
#44279 = CARTESIAN_POINT('Ctrl Pts',(12.2550639238409,-13.9471822911523,-331.054117076876)) ;
#44280 = CARTESIAN_POINT('Ctrl Pts',(12.0251287578649,-14.1464625951566,-331.05806146061)) ;
#44281 = CARTESIAN_POINT('Ctrl Pts',(11.8890734092209,-14.2609978235547,-331.060383017681)) ;
#44282 = CARTESIAN_POINT('Ctrl Pts',(11.2354921139579,-14.7953463681454,-331.0714750165)) ;
#44283 = CARTESIAN_POINT('Ctrl Pts',(10.6972576826663,-15.1890496338167,-331.080453013357)) ;
#44284 = CARTESIAN_POINT('Ctrl Pts',(9.79526015437213,-15.7770649091209,-331.094952856296)) ;
#44285 = CARTESIAN_POINT('Ctrl Pts',(9.44415561414358,-15.9897099508716,-331.100468227632)) ;
#44286 = CARTESIAN_POINT('Ctrl Pts',(8.98285514861447,-16.248596314188,-331.107436316812)) ;
#44287 = CARTESIAN_POINT('Ctrl Pts',(8.8788626047792,-16.3056544706181,-331.108989249766)) ;
#44288 = CARTESIAN_POINT('Ctrl Pts',(8.71283755442982,-16.3946890787099,-331.111435995875)) ;
#44289 = CARTESIAN_POINT('Ctrl Pts',(8.65115926415511,-16.4273190647436,-331.112337903359)) ;
#44290 = CARTESIAN_POINT('Ctrl Pts',(8.53315121297165,-16.4889005324727,-331.114049008568)) ;
#44291 = CARTESIAN_POINT('Ctrl Pts',(8.47685443375419,-16.5179129830148,-331.114859118253)) ;
#44292 = CARTESIAN_POINT('Ctrl Pts',(8.31268276261775,-16.6014582278814,-331.117205073238)) ;
#44293 = CARTESIAN_POINT('Ctrl Pts',(8.20442230960213,-16.655226346107,-331.118731513974)) ;
#44294 = CARTESIAN_POINT('Ctrl Pts',(7.90039294779327,-16.8025404115189,-331.122970471546)) ;
#44295 = CARTESIAN_POINT('Ctrl Pts',(7.7034977824425,-16.8937176250662,-331.125661039915)) ;
#44296 = CARTESIAN_POINT('Ctrl Pts',(6.96443610819583,-17.2203507106018,-331.135624246862)) ;
#44297 = CARTESIAN_POINT('Ctrl Pts',(6.4127212551024,-17.4333260332723,-331.142803587748)) ;
#44298 = CARTESIAN_POINT('Ctrl Pts',(5.69929878068553,-17.6702662954348,-331.152096073932)) ;
#44299 = CARTESIAN_POINT('Ctrl Pts',(5.54615768729234,-17.7189292107757,-331.154090427393)) ;
#44300 = CARTESIAN_POINT('Ctrl Pts',(5.1723034991462,-17.832405433101,-331.158966260683)) ;
#44301 = CARTESIAN_POINT('Ctrl Pts',(4.95098045828004,-17.8951166311051,-331.161858922365)) ;
#44302 = CARTESIAN_POINT('Ctrl Pts',(4.59772196794183,-17.9881559723658,-331.166496014513)) ;
#44303 = CARTESIAN_POINT('Ctrl Pts',(4.46652158474351,-18.021181632986,-331.168222509841)) ;
#44304 = CARTESIAN_POINT('Ctrl Pts',(4.21202743047192,-18.0822927554013,-331.171581111831)) ;
#44305 = CARTESIAN_POINT('Ctrl Pts',(4.08878450538391,-18.1105584558184,-331.173211913479)) ;
#44306 = CARTESIAN_POINT('Ctrl Pts',(3.79151063264642,-18.1755489379813,-331.177156575053)) ;
#44307 = CARTESIAN_POINT('Ctrl Pts',(3.61722204271559,-18.2110361215927,-331.179478375634)) ;
#44308 = CARTESIAN_POINT('Ctrl Pts',(2.78711546092656,-18.3676683775864,-331.190577515518)) ;
#44309 = CARTESIAN_POINT('Ctrl Pts',(2.12559543858863,-18.4559229449141,-331.199562777584)) ;
#44310 = CARTESIAN_POINT('Ctrl Pts',(1.15854057714928,-18.5322474007988,-331.212626014104)) ;
#44311 = CARTESIAN_POINT('Ctrl Pts',(0.855773602491591,-18.5486943440046,
-331.216702170191)) ;
#44312 = CARTESIAN_POINT('Ctrl Pts',(0.366577110325669,-18.5632650127573,
-331.223210402425)) ;
#44313 = CARTESIAN_POINT('Ctrl Pts',(0.180341342491163,-18.5660082890026,
-331.225669690197)) ;
#44314 = CARTESIAN_POINT('Ctrl Pts',(-0.0876156468409861,-18.5659230735206,
-331.22916757371)) ;
#44315 = CARTESIAN_POINT('Ctrl Pts',(-0.169326398501262,-18.5653576536056,
-331.2302287745)) ;
#44316 = CARTESIAN_POINT('Ctrl Pts',(-0.317213538112543,-18.5633578839317,
-331.232137936549)) ;
#44317 = CARTESIAN_POINT('Ctrl Pts',(-0.38339085125449,-18.5621090344773,
-331.232987929659)) ;
#44318 = CARTESIAN_POINT('Ctrl Pts',(-0.545502099660334,-18.5581824840665,
-331.235060209075)) ;
#44319 = CARTESIAN_POINT('Ctrl Pts',(-0.641424653954942,-18.5551147693579,
-331.236278075621)) ;
#44320 = CARTESIAN_POINT('Ctrl Pts',(-1.05959377305711,-18.5384946910379,
-331.241558517715)) ;
#44321 = CARTESIAN_POINT('Ctrl Pts',(-1.38148069268011,-18.5172902016032,
-331.245549481872)) ;
#44322 = CARTESIAN_POINT('Ctrl Pts',(-2.31060338030414,-18.4317213301951,
-331.257023430549)) ;
#44323 = CARTESIAN_POINT('Ctrl Pts',(-2.91542254265853,-18.3457774854192,
-331.264446047105)) ;
#44324 = CARTESIAN_POINT('Ctrl Pts',(-3.79144351382164,-18.1768746233684,
-331.275520600804)) ;
#44325 = CARTESIAN_POINT('Ctrl Pts',(-4.06673109238057,-18.1172711174393,
-331.279045922301)) ;
#44326 = CARTESIAN_POINT('Ctrl Pts',(-4.48041862951445,-18.0177978950799,
-331.2844327952)) ;
#44327 = CARTESIAN_POINT('Ctrl Pts',(-4.61988588248379,-17.9825428246323,
-331.286264236867)) ;
#44328 = CARTESIAN_POINT('Ctrl Pts',(-4.87794249438734,-17.9141099879679,
-331.289683369772)) ;
#44329 = CARTESIAN_POINT('Ctrl Pts',(-4.99663878565135,-17.8813662910714,
-331.291268074259)) ;
#44330 = CARTESIAN_POINT('Ctrl Pts',(-5.26793522173483,-17.8036139041292,
-331.29491844428)) ;
#44331 = CARTESIAN_POINT('Ctrl Pts',(-5.42030009698362,-17.7578195818207,
-331.296989266319)) ;
#44332 = CARTESIAN_POINT('Ctrl Pts',(-5.9591785416877,-17.5882741672656,-331.304386606565)) ;
#44333 = CARTESIAN_POINT('Ctrl Pts',(-6.34220099019749,-17.453815690401,-331.309781902109)) ;
#44334 = CARTESIAN_POINT('Ctrl Pts',(-7.10537514608677,-17.1574648868725,
-331.320757430125)) ;
#44335 = CARTESIAN_POINT('Ctrl Pts',(-7.48515017746701,-16.9952194358773,
-331.326336177218)) ;
#44336 = CARTESIAN_POINT('Ctrl Pts',(-8.17091560180506,-16.6748018809099,
-331.336507069752)) ;
#44337 = CARTESIAN_POINT('Ctrl Pts',(-8.47852385226896,-16.5205179601351,
-331.341106013271)) ;
#44338 = CARTESIAN_POINT('Ctrl Pts',(-8.86846276489182,-16.3111793646129,
-331.346911105294)) ;
#44339 = CARTESIAN_POINT('Ctrl Pts',(-8.95488619290344,-16.2638930576343,
-331.348196006464)) ;
#44340 = CARTESIAN_POINT('Ctrl Pts',(-9.0989852571619,-16.1835529131439,-331.350332932471)) ;
#44341 = CARTESIAN_POINT('Ctrl Pts',(-9.15686703757934,-16.1508731557966,
-331.351189727604)) ;
#44342 = CARTESIAN_POINT('Ctrl Pts',(-9.28419381412733,-16.0780806075834,
-331.35307044433)) ;
#44343 = CARTESIAN_POINT('Ctrl Pts',(-9.35355679167832,-16.0378273519455,
-331.354092555978)) ;
#44344 = CARTESIAN_POINT('Ctrl Pts',(-9.57466023518528,-15.9075925907088,
-331.357346113269)) ;
#44345 = CARTESIAN_POINT('Ctrl Pts',(-9.72538006394519,-15.8158971751446,
-331.359557121069)) ;
#44346 = CARTESIAN_POINT('Ctrl Pts',(-10.1098017594987,-15.5744482735364,
-331.365204760896)) ;
#44347 = CARTESIAN_POINT('Ctrl Pts',(-10.3414937842337,-15.421577005722,-331.368617015808)) ;
#44348 = CARTESIAN_POINT('Ctrl Pts',(-10.7804742594848,-15.117593091634,-331.375164255486)) ;
#44349 = CARTESIAN_POINT('Ctrl Pts',(-10.9882302316875,-14.9672656998948,
-331.378299816587)) ;
#44350 = CARTESIAN_POINT('Ctrl Pts',(-11.5704488233802,-14.5273278901423,
-331.387255314615)) ;
#44351 = CARTESIAN_POINT('Ctrl Pts',(-11.9370405010022,-14.2276352316939,
-331.393102684929)) ;
#44352 = CARTESIAN_POINT('Ctrl Pts',(-12.4053085549168,-13.8139699922844,
-331.400971149525)) ;
#44353 = CARTESIAN_POINT('Ctrl Pts',(-12.5176076779195,-13.712291756874,-331.402889671316)) ;
#44354 = CARTESIAN_POINT('Ctrl Pts',(-12.7206782089786,-13.5238532698427,
-331.406419877833)) ;
#44355 = CARTESIAN_POINT('Ctrl Pts',(-12.8118379976024,-13.4375246392885,
-331.40802774849)) ;
#44356 = CARTESIAN_POINT('Ctrl Pts',(-12.9985854536365,-13.2570462143434,
-331.411370867122)) ;
#44357 = CARTESIAN_POINT('Ctrl Pts',(-13.0940423455259,-13.1627714830096,
-331.413107192211)) ;
#44358 = CARTESIAN_POINT('Ctrl Pts',(-13.3458267635657,-12.9086556634847,
-331.417761492747)) ;
#44359 = CARTESIAN_POINT('Ctrl Pts',(-13.500302809021,-12.747011682148,-331.420695569395)) ;
#44360 = CARTESIAN_POINT('Ctrl Pts',(-13.7561735302441,-12.469398426364,-331.42568731787)) ;
#44361 = CARTESIAN_POINT('Ctrl Pts',(-13.8591128683516,-12.3548855816682,
-331.427733222945)) ;
#44362 = CARTESIAN_POINT('Ctrl Pts',(-14.3167461561979,-11.8328831840082,
-331.436993826502)) ;
#44363 = CARTESIAN_POINT('Ctrl Pts',(-14.6549763772027,-11.4113106375806,
-331.444303884208)) ;
#44364 = CARTESIAN_POINT('Ctrl Pts',(-15.1700617287894,-10.7085637566994,
-331.456006102515)) ;
#44365 = CARTESIAN_POINT('Ctrl Pts',(-15.3586058313691,-10.4363469801212,
-331.460427998719)) ;
#44366 = CARTESIAN_POINT('Ctrl Pts',(-15.5933070923309,-10.0773431855292,
-331.466052962013)) ;
#44367 = CARTESIAN_POINT('Ctrl Pts',(-15.6461958840107,-9.99503007270438,
-331.467328887012)) ;
#44368 = CARTESIAN_POINT('Ctrl Pts',(-15.7338771291969,-9.85616647304519,
-331.469455822043)) ;
#44369 = CARTESIAN_POINT('Ctrl Pts',(-15.7690212956443,-9.7998405330711,-331.4703114943)) ;
#44370 = CARTESIAN_POINT('Ctrl Pts',(-15.8461503563063,-9.67473572291543,
-331.472195910214)) ;
#44371 = CARTESIAN_POINT('Ctrl Pts',(-15.8879910467882,-9.60586971305204,
-331.473222776428)) ;
#44372 = CARTESIAN_POINT('Ctrl Pts',(-16.0212528030751,-9.38328013874559,
-331.476511670561)) ;
#44373 = CARTESIAN_POINT('Ctrl Pts',(-16.1109014472047,-9.22850704607624,
-331.478752643936)) ;
#44374 = CARTESIAN_POINT('Ctrl Pts',(-16.3369549921495,-8.82490294762817,
-331.484506056995)) ;
#44375 = CARTESIAN_POINT('Ctrl Pts',(-16.4699168260395,-8.57419679058869,
-331.487993020809)) ;
#44376 = CARTESIAN_POINT('Ctrl Pts',(-16.9147867202385,-7.68680969129279,
-331.500162302095)) ;
#44377 = CARTESIAN_POINT('Ctrl Pts',(-17.1959353729,-7.03540043254521,-331.508812879716)) ;
#44378 = CARTESIAN_POINT('Ctrl Pts',(-17.4925489170177,-6.22329999630359,
-331.519691540344)) ;
#44379 = CARTESIAN_POINT('Ctrl Pts',(-17.5441120608831,-6.07641854716277,
-331.521661534681)) ;
#44380 = CARTESIAN_POINT('Ctrl Pts',(-17.6342000371274,-5.80908562643832,
-331.525254342114)) ;
#44381 = CARTESIAN_POINT('Ctrl Pts',(-17.673353004309,-5.68885579852728,-331.526872797266)) ;
#44382 = CARTESIAN_POINT('Ctrl Pts',(-17.7510257764981,-5.44179659955389,
-331.530204930518)) ;
#44383 = CARTESIAN_POINT('Ctrl Pts',(-17.7894216919508,-5.31493576185626,
-331.531919343106)) ;
#44384 = CARTESIAN_POINT('Ctrl Pts',(-17.8863554478203,-4.9818413814567,-331.53643017183)) ;
#44385 = CARTESIAN_POINT('Ctrl Pts',(-17.9426854311605,-4.77498628527236,
-331.539240904705)) ;
#44386 = CARTESIAN_POINT('Ctrl Pts',(-18.1639374705924,-3.9032221108315,-331.551119309564)) ;
#44387 = CARTESIAN_POINT('Ctrl Pts',(-18.2955763650669,-3.23042511831326,
-331.560387604609)) ;
#44388 = CARTESIAN_POINT('Ctrl Pts',(-18.4381439038572,-2.20304207254931,
-331.574329804321)) ;
#44389 = CARTESIAN_POINT('Ctrl Pts',(-18.4766175319275,-1.85287626235518,
-331.57904062491)) ;
#44390 = CARTESIAN_POINT('Ctrl Pts',(-18.5132166667941,-1.40191192968094,
-331.584977635847)) ;
#44391 = CARTESIAN_POINT('Ctrl Pts',(-18.520516264185,-1.30193155020809,-331.586285614674)) ;
#44392 = CARTESIAN_POINT('Ctrl Pts',(-18.5313229321195,-1.13534887234126,
-331.588448405205)) ;
#44393 = CARTESIAN_POINT('Ctrl Pts',(-18.5352814976047,-1.06877804941513,
-331.58930826546)) ;
#44394 = CARTESIAN_POINT('Ctrl Pts',(-18.5431600794371,-0.923036708281147,
-331.591180345956)) ;
#44395 = CARTESIAN_POINT('Ctrl Pts',(-18.5469319141503,-0.843859639608341,
-331.592190921782)) ;
#44396 = CARTESIAN_POINT('Ctrl Pts',(-18.55722350396,-0.594192050500668,-331.595360264501)) ;
#44397 = CARTESIAN_POINT('Ctrl Pts',(-18.5619002946768,-0.423634270060247,
-331.597500026508)) ;
#44398 = CARTESIAN_POINT('Ctrl Pts',(-18.5678128423706,0.0101452110234948,
-331.602901064301)) ;
#44399 = CARTESIAN_POINT('Ctrl Pts',(-18.5658030798211,0.273373418284622,
-331.60614043762)) ;
#44400 = CARTESIAN_POINT('Ctrl Pts',(-18.5362661362121,1.2951500308187,-331.618681193349)) ;
#44401 = CARTESIAN_POINT('Ctrl Pts',(-18.4678316157956,2.05177281078287,-331.627926452439)) ;
#44402 = CARTESIAN_POINT('Ctrl Pts',(-18.3285550607503,2.96401847065086,-331.639553227547)) ;
#44403 = CARTESIAN_POINT('Ctrl Pts',(-18.3016883016166,3.12562654674809,-331.641629943042)) ;
#44404 = CARTESIAN_POINT('Ctrl Pts',(-18.2505600686712,3.40986463996013,-331.645315617827)) ;
#44405 = CARTESIAN_POINT('Ctrl Pts',(-18.2271923110643,3.53264491375653,-331.64691863487)) ;
#44406 = CARTESIAN_POINT('Ctrl Pts',(-18.1750547849223,3.79228681864865,-331.650332617048)) ;
#44407 = CARTESIAN_POINT('Ctrl Pts',(-18.14597474636,3.92907828651783,-331.652145540222)) ;
#44408 = CARTESIAN_POINT('Ctrl Pts',(-18.059146120464,4.31597295924445,-331.65731397514)) ;
#44409 = CARTESIAN_POINT('Ctrl Pts',(-17.9977526962845,4.56522492894707,-331.660692662125)) ;
#44410 = CARTESIAN_POINT('Ctrl Pts',(-17.8382533704448,5.15943702951864,-331.668856110161)) ;
#44411 = CARTESIAN_POINT('Ctrl Pts',(-17.7352822109154,5.5029844533492,-331.673665711063)) ;
#44412 = CARTESIAN_POINT('Ctrl Pts',(-17.4371298653266,6.40215753372959,-331.686416412542)) ;
#44413 = CARTESIAN_POINT('Ctrl Pts',(-17.2253557058779,6.95185158931128,-331.694385868993)) ;
#44414 = CARTESIAN_POINT('Ctrl Pts',(-16.9441938947519,7.58949843422687,-331.703546542479)) ;
#44415 = CARTESIAN_POINT('Ctrl Pts',(-16.8997012346149,7.68806161913078,-331.704959715081)) ;
#44416 = CARTESIAN_POINT('Ctrl Pts',(-16.8261613680886,7.84724861457569,-331.707234191653)) ;
#44417 = CARTESIAN_POINT('Ctrl Pts',(-16.7976415635973,7.90811324806361,-331.708101911654)) ;
#44418 = CARTESIAN_POINT('Ctrl Pts',(-16.7363726172915,8.03704149195143,-331.709934970161)) ;
#44419 = CARTESIAN_POINT('Ctrl Pts',(-16.7035374133237,8.1050627530071,-331.710899249294)) ;
#44420 = CARTESIAN_POINT('Ctrl Pts',(-16.6047632936052,8.30653306224311,-331.71374945145)) ;
#44421 = CARTESIAN_POINT('Ctrl Pts',(-16.5376335534004,8.43939169173527,-331.715621338628)) ;
#44422 = CARTESIAN_POINT('Ctrl Pts',(-16.370215984556,8.76106331629915,-331.720149750636)) ;
#44423 = CARTESIAN_POINT('Ctrl Pts',(-16.2682504626407,8.94897921107539,-331.722792116712)) ;
#44424 = CARTESIAN_POINT('Ctrl Pts',(-15.7588434336498,9.85029222155326,-331.735530399111)) ;
#44425 = CARTESIAN_POINT('Ctrl Pts',(-15.3076006685487,10.5378730508359,-331.745490731296)) ;
#44426 = CARTESIAN_POINT('Ctrl Pts',(-14.7075415985295,11.3319422662572,-331.758011912124)) ;
#44427 = CARTESIAN_POINT('Ctrl Pts',(-14.6008356007635,11.46910175331,-331.760212097871)) ;
#44428 = CARTESIAN_POINT('Ctrl Pts',(-14.413549669923,11.7029879271909,-331.764032896281)) ;
#44429 = CARTESIAN_POINT('Ctrl Pts',(-14.3338823905267,11.8004303342313,-331.765645936428)) ;
#44430 = CARTESIAN_POINT('Ctrl Pts',(-14.1655944190609,12.0020472255589,-331.769029003547)) ;
#44431 = CARTESIAN_POINT('Ctrl Pts',(-14.0768009770804,12.1060677775006,-331.770800431064)) ;
#44432 = CARTESIAN_POINT('Ctrl Pts',(-13.8300367499831,12.3887633853556,-331.775686959527)) ;
#44433 = CARTESIAN_POINT('Ctrl Pts',(-13.6697600891816,12.5653903039335,-331.778821220587)) ;
#44434 = CARTESIAN_POINT('Ctrl Pts',(-13.2872091435448,12.9709817724761,-331.786205178204)) ;
#44435 = CARTESIAN_POINT('Ctrl Pts',(-13.0623464112431,13.1974012823016,-331.790473241135)) ;
#44436 = CARTESIAN_POINT('Ctrl Pts',(-12.5310896485368,13.7054504773766,-331.800352556521)) ;
#44437 = CARTESIAN_POINT('Ctrl Pts',(-12.220838141711,13.9827999893821,-331.805976160708)) ;
#44438 = CARTESIAN_POINT('Ctrl Pts',(-11.7253475713879,14.3966461032938,-331.814622879287)) ;
#44439 = CARTESIAN_POINT('Ctrl Pts',(-11.5464485919751,14.5405199324681,-331.817680380057)) ;
#44440 = CARTESIAN_POINT('Ctrl Pts',(-11.2740033495633,14.7514260114405,-331.822215745074)) ;
#44441 = CARTESIAN_POINT('Ctrl Pts',(-11.1824270203272,14.8209664628872,-331.823720236991)) ;
#44442 = CARTESIAN_POINT('Ctrl Pts',(-11.040232292008,14.9268768961609,-331.826021999575)) ;
#44443 = CARTESIAN_POINT('Ctrl Pts',(-10.9900669219232,14.963850172938,-331.826827548958)) ;
#44444 = CARTESIAN_POINT('Ctrl Pts',(-10.8823156573827,15.0424317369025,-331.82854307448)) ;
#44445 = CARTESIAN_POINT('Ctrl Pts',(-10.8246751445475,15.0839634929808,-331.829451860772)) ;
#44446 = CARTESIAN_POINT('Ctrl Pts',(-10.6648438465556,15.197738874673,-331.83194929016)) ;
#44447 = CARTESIAN_POINT('Ctrl Pts',(-10.5621587225438,15.2692817241382,-331.833528574788)) ;
#44448 = CARTESIAN_POINT('Ctrl Pts',(-10.3211816787165,15.4335813705844,-331.837185126018)) ;
#44449 = CARTESIAN_POINT('Ctrl Pts',(-10.1823495050015,15.5255268461562,-331.839254326873)) ;
#44450 = CARTESIAN_POINT('Ctrl Pts',(-9.63513571133012,15.8774369437671,-331.847296862428)) ;
#44451 = CARTESIAN_POINT('Ctrl Pts',(-9.21788657678393,16.1232568767848,-331.853191078634)) ;
#44452 = CARTESIAN_POINT('Ctrl Pts',(-8.42548722669793,16.5492706422417,-331.8642430431)) ;
#44453 = CARTESIAN_POINT('Ctrl Pts',(-8.05296334221619,16.7337077234566,-331.869382937618)) ;
#44454 = CARTESIAN_POINT('Ctrl Pts',(-7.51311146723126,16.9787836771746,-331.876836955329)) ;
#44455 = CARTESIAN_POINT('Ctrl Pts',(-7.35061568420548,17.0497621098074,-331.879080823854)) ;
#44456 = CARTESIAN_POINT('Ctrl Pts',(-7.07061997982843,17.1673177713276,-331.882951686474)) ;
#44457 = CARTESIAN_POINT('Ctrl Pts',(-6.95361536788679,17.2150428295426,-331.884570531106)) ;
#44458 = CARTESIAN_POINT('Ctrl Pts',(-6.71017734321866,17.3114520607135,-331.887942293788)) ;
#44459 = CARTESIAN_POINT('Ctrl Pts',(-6.58367982288382,17.3599542727317,-331.889696364602)) ;
#44460 = CARTESIAN_POINT('Ctrl Pts',(-6.24001542907438,17.4874269292189,-331.894467540683)) ;
#44461 = CARTESIAN_POINT('Ctrl Pts',(-6.0218869607842,17.5637345198057,-331.897502259535)) ;
#44462 = CARTESIAN_POINT('Ctrl Pts',(-5.64870356937853,17.686515319265,-331.902701027425)) ;
#44463 = CARTESIAN_POINT('Ctrl Pts',(-5.49436144900012,17.7350688844233,-331.904853028325)) ;
#44464 = CARTESIAN_POINT('Ctrl Pts',(-4.76454484726649,17.9542160009468,-331.91502880749)) ;
#44465 = CARTESIAN_POINT('Ctrl Pts',(-4.18165407044763,18.0988542924827,-331.923168279854)) ;
#44466 = CARTESIAN_POINT('Ctrl Pts',(-3.45341113900785,18.242495213728,-331.933103108547)) ;
#44467 = CARTESIAN_POINT('Ctrl Pts',(-3.31372652463599,18.2683851696051,-331.934997497831)) ;
#44468 = CARTESIAN_POINT('Ctrl Pts',(-3.03179040997574,18.3173007821852,-331.938790579861)) ;
#44469 = CARTESIAN_POINT('Ctrl Pts',(-2.88954021443678,18.3402785826744,-331.940688819553)) ;
#44470 = CARTESIAN_POINT('Ctrl Pts',(-2.66534431492158,18.3738200199791,-331.943648910296)) ;
#44471 = CARTESIAN_POINT('Ctrl Pts',(-2.58357105750912,18.3854965410316,-331.944721963404)) ;
#44472 = CARTESIAN_POINT('Ctrl Pts',(-2.43626337686835,18.4055286341393,-331.946641408023)) ;
#44473 = CARTESIAN_POINT('Ctrl Pts',(-2.37075732425834,18.4140808419076,-331.94748998443)) ;
#44474 = CARTESIAN_POINT('Ctrl Pts',(-2.21132165961733,18.4340312566281,-331.949543845586)) ;
#44475 = CARTESIAN_POINT('Ctrl Pts',(-2.11734790080118,18.4450613920446,-331.950744928739)) ;
#44476 = CARTESIAN_POINT('Ctrl Pts',(-1.72167342631557,18.4884398566989,-331.955769106123)) ;
#44477 = CARTESIAN_POINT('Ctrl Pts',(-1.41928694166473,18.5141079477051,-331.959528927246)) ;
#44478 = CARTESIAN_POINT('Ctrl Pts',(-0.280721623934055,18.5826962338751,
-331.97356903952)) ;
#44479 = CARTESIAN_POINT('Ctrl Pts',(0.557410764232457,18.576455562283,-331.983713292041)) ;
#44480 = CARTESIAN_POINT('Ctrl Pts',(1.5460708546203,18.5021068267284,-331.99619191967)) ;
#44481 = CARTESIAN_POINT('Ctrl Pts',(1.69973510802066,18.4886233285991,-331.998144487635)) ;
#44482 = CARTESIAN_POINT('Ctrl Pts',(1.97871519221223,18.4606363602097,-332.001716011425)) ;
#44483 = CARTESIAN_POINT('Ctrl Pts',(2.10408538715813,18.4467675560337,-332.003330794352)) ;
#44484 = CARTESIAN_POINT('Ctrl Pts',(2.36139797415323,18.4156456030462,-332.00666613251)) ;
#44485 = CARTESIAN_POINT('Ctrl Pts',(2.49331584615126,18.3982493568772,-332.008387534452)) ;
#44486 = CARTESIAN_POINT('Ctrl Pts',(2.84015425265685,18.3487123095595,-332.012944074571)) ;
#44487 = CARTESIAN_POINT('Ctrl Pts',(3.05471698134277,18.3142137014464,-332.015794089639)) ;
#44488 = CARTESIAN_POINT('Ctrl Pts',(3.41391851047208,18.2499711086659,-332.020615073385)) ;
#44489 = CARTESIAN_POINT('Ctrl Pts',(3.55889755013297,18.2222537909799,-332.022574541392)) ;
#44490 = CARTESIAN_POINT('Ctrl Pts',(4.19104212886648,18.0935674224194,-332.031172393643)) ;
#44491 = CARTESIAN_POINT('Ctrl Pts',(4.67436711268179,17.9747686139255,-332.037892972326)) ;
#44492 = CARTESIAN_POINT('Ctrl Pts',(5.22665637259435,17.8152335712315,-332.045626956807)) ;
#44493 = CARTESIAN_POINT('Ctrl Pts',(5.30084326235868,17.7933005580051,-332.046666834219)) ;
#44494 = CARTESIAN_POINT('Ctrl Pts',(5.67741552285269,17.6794045647664,-332.051947576863)) ;
#44495 = CARTESIAN_POINT('Ctrl Pts',(5.9775549568405,17.5801942605611,-332.056165041427)) ;
#44496 = CARTESIAN_POINT('Ctrl Pts',(6.36632838708065,17.4405784202165,-332.061581276427)) ;
#44497 = CARTESIAN_POINT('Ctrl Pts',(6.45738288298993,17.4070709513657,-332.062846334359)) ;
#44498 = CARTESIAN_POINT('Ctrl Pts',(6.61020879545238,17.3494678478016,-332.064961230441)) ;
#44499 = CARTESIAN_POINT('Ctrl Pts',(6.67212127391179,17.3257522971288,-332.065815600062)) ;
#44500 = CARTESIAN_POINT('Ctrl Pts',(6.80944650943599,17.2723046659681,-332.067704770073)) ;
#44501 = CARTESIAN_POINT('Ctrl Pts',(6.88479410764785,17.242409354803,-332.06873760878)) ;
#44502 = CARTESIAN_POINT('Ctrl Pts',(7.12863509967626,17.143808528611,-332.072071437282)) ;
#44503 = CARTESIAN_POINT('Ctrl Pts',(7.29631500291615,17.0731191302671,-332.07435057508)) ;
#44504 = CARTESIAN_POINT('Ctrl Pts',(7.73010947118155,16.8826849081625,-332.080240549846)) ;
#44505 = CARTESIAN_POINT('Ctrl Pts',(7.99448821531071,16.7591109774453,-332.083824459769)) ;
#44506 = CARTESIAN_POINT('Ctrl Pts',(8.87348924595585,16.3227203352077,-332.095852635572)) ;
#44507 = CARTESIAN_POINT('Ctrl Pts',(9.47357100943901,15.981910468644,-332.104272765041)) ;
#44508 = CARTESIAN_POINT('Ctrl Pts',(10.2009303023555,15.5134250575098,-332.115153500138)) ;
#44509 = CARTESIAN_POINT('Ctrl Pts',(10.3472047410798,15.4162475966418,-332.117376298661)) ;
#44510 = CARTESIAN_POINT('Ctrl Pts',(10.5961247282556,15.2457385971344,-332.121222959738)) ;
#44511 = CARTESIAN_POINT('Ctrl Pts',(10.6994420508467,15.1734091217618,-332.122838952109)) ;
#44512 = CARTESIAN_POINT('Ctrl Pts',(10.9126864268451,15.0208618490027,-332.126215857696)) ;
#44513 = CARTESIAN_POINT('Ctrl Pts',(11.0224846925921,14.9404767953348,-332.127978040791)) ;
#44514 = CARTESIAN_POINT('Ctrl Pts',(11.3190867362795,14.7182803635872,-332.132802981054)) ;
#44515 = CARTESIAN_POINT('Ctrl Pts',(11.5041027549559,14.574125046996,-332.135884065854)) ;
#44516 = CARTESIAN_POINT('Ctrl Pts',(11.9279271975545,14.2308016947911,-332.143104590161)) ;
#44517 = CARTESIAN_POINT('Ctrl Pts',(12.1645621819109,14.0290623518186,-332.147261178875)) ;
#44518 = CARTESIAN_POINT('Ctrl Pts',(12.8918232658396,13.3768062620202,-332.160385108515)) ;
#44519 = CARTESIAN_POINT('Ctrl Pts',(13.3633411116242,12.9057803530218,-332.169430712286)) ;
#44520 = CARTESIAN_POINT('Ctrl Pts',(13.8835154218664,12.3270062604297,-332.17966858666)) ;
#44521 = CARTESIAN_POINT('Ctrl Pts',(13.9577448622368,12.2428935400364,-332.181135664912)) ;
#44522 = CARTESIAN_POINT('Ctrl Pts',(14.0717118413588,12.1113686636672,-332.183394194914)) ;
#44523 = CARTESIAN_POINT('Ctrl Pts',(14.1119823935993,12.0644219916771,-332.184193451988)) ;
#44524 = CARTESIAN_POINT('Ctrl Pts',(14.1984744379758,11.9625655436357,-332.185911817685)) ;
#44525 = CARTESIAN_POINT('Ctrl Pts',(14.2446136457105,11.9075871969891,-332.186829605341)) ;
#44526 = CARTESIAN_POINT('Ctrl Pts',(14.3726990777383,11.7531539064573,-332.189382675768)) ;
#44527 = CARTESIAN_POINT('Ctrl Pts',(14.4539304202055,11.6531112162949,-332.191007916671)) ;
#44528 = CARTESIAN_POINT('Ctrl Pts',(14.6420919725536,11.4163810613987,-332.194796582731)) ;
#44529 = CARTESIAN_POINT('Ctrl Pts',(14.7481603794183,11.2790238687871,-332.196951126732)) ;
#44530 = CARTESIAN_POINT('Ctrl Pts',(15.1719887096987,10.7139693471667,-332.205675302701)) ;
#44531 = CARTESIAN_POINT('Ctrl Pts',(15.4731939097454,10.2741740416133,-332.21215398903)) ;
#44532 = CARTESIAN_POINT('Ctrl Pts',(15.8754760600177,9.6288920249461,-332.221516070776)) ;
#44533 = CARTESIAN_POINT('Ctrl Pts',(15.9923231607515,9.43355190260966,-332.224331099906)) ;
#44534 = CARTESIAN_POINT('Ctrl Pts',(16.2258969649451,9.0262556394395,-332.230182629515)) ;
#44535 = CARTESIAN_POINT('Ctrl Pts',(16.3421313944118,8.81406627810662,-332.233221411081)) ;
#44536 = CARTESIAN_POINT('Ctrl Pts',(16.5178063467136,8.47793832322024,-332.238032400112)) ;
#44537 = CARTESIAN_POINT('Ctrl Pts',(16.580073918033,8.35550797528294,-332.239784105139)) ;
#44538 = CARTESIAN_POINT('Ctrl Pts',(16.6966971540801,8.11976565726892,-332.24315734619)) ;
#44539 = CARTESIAN_POINT('Ctrl Pts',(16.7512721435412,8.00657053325846,-332.244777180012)) ;
#44540 = CARTESIAN_POINT('Ctrl Pts',(16.87793405211,7.73689355733387,-332.248637180834)) ;
#44541 = CARTESIAN_POINT('Ctrl Pts',(16.9490002600113,7.57994523975932,-332.250884400886)) ;
#44542 = CARTESIAN_POINT('Ctrl Pts',(17.24932435737,6.89133627237522,-332.260745764029)) ;
#44543 = CARTESIAN_POINT('Ctrl Pts',(17.4558253886552,6.35010725633239,-332.268512042367)) ;
#44544 = CARTESIAN_POINT('Ctrl Pts',(17.8004348630631,5.30223669175835,-332.283369264019)) ;
#44545 = CARTESIAN_POINT('Ctrl Pts',(17.9430154746527,4.79764441870485,-332.290445425046)) ;
#44546 = CARTESIAN_POINT('Ctrl Pts',(18.089801287868,4.17923622088749,-332.29880618908)) ;
#44547 = CARTESIAN_POINT('Ctrl Pts',(18.11456839653,4.07054515869485,-332.300263857364)) ;
#44548 = CARTESIAN_POINT('Ctrl Pts',(18.1515286734727,3.90132255242415,-332.302511540022)) ;
#44549 = CARTESIAN_POINT('Ctrl Pts',(18.1644012889704,3.84094215962314,-332.303309241649)) ;
#44550 = CARTESIAN_POINT('Ctrl Pts',(18.1916272130505,3.71003750282837,-332.305028508422)) ;
#44551 = CARTESIAN_POINT('Ctrl Pts',(18.2058721028726,3.63949171214811,-332.305948717724)) ;
#44552 = CARTESIAN_POINT('Ctrl Pts',(18.2446711724638,3.44141537883529,-332.308516838372)) ;
#44553 = CARTESIAN_POINT('Ctrl Pts',(18.2682979473849,3.31370731835557,-332.310154519616)) ;
#44554 = CARTESIAN_POINT('Ctrl Pts',(18.3206904642593,3.01290338390637,-332.313979237911)) ;
#44555 = CARTESIAN_POINT('Ctrl Pts',(18.3483461492828,2.83962666834625,-332.316157164572)) ;
#44556 = CARTESIAN_POINT('Ctrl Pts',(18.4521236564401,2.12440841226223,-332.325081521149)) ;
#44557 = CARTESIAN_POINT('Ctrl Pts',(18.5067223202752,1.57962305695096,-332.331733489889)) ;
#44558 = CARTESIAN_POINT('Ctrl Pts',(18.5408754758118,0.966877152202078,-332.339294922937)) ;
#44559 = CARTESIAN_POINT('Ctrl Pts',(18.544217236243,0.900512036507376,-332.340114796803)) ;
#44560 = CARTESIAN_POINT('Ctrl Pts',(18.554037632943,0.68215183631762,-332.342816323201)) ;
#44561 = CARTESIAN_POINT('Ctrl Pts',(18.5590043576457,0.530095088599722,-332.344703822096)) ;
#44562 = CARTESIAN_POINT('Ctrl Pts',(18.5669195460512,0.141405603914571,-332.349551882388)) ;
#44563 = CARTESIAN_POINT('Ctrl Pts',(18.5672136693237,-0.0952535122605108,
-332.352525865488)) ;
#44564 = CARTESIAN_POINT('Ctrl Pts',(18.5605451549998,-0.468272513056562,
-332.357259767486)) ;
#44565 = CARTESIAN_POINT('Ctrl Pts',(18.5566026237942,-0.604660726114443,
-332.359000340067)) ;
#44566 = CARTESIAN_POINT('Ctrl Pts',(18.5491863659681,-0.790330730519442,
-332.361384090202)) ;
#44567 = CARTESIAN_POINT('Ctrl Pts',(18.5470188521273,-0.839660132558339,
-332.362018778973)) ;
#44568 = CARTESIAN_POINT('Ctrl Pts',(18.544654593742,-0.888979978009869,-332.362654732516)) ;
#44569 = CARTESIAN_POINT('Origin',(0.,0.,-315.477129595899)) ;
#44570 = CARTESIAN_POINT('',(18.5446545951453,-0.888979948736908,-334.159397110263)) ;
#44571 = CARTESIAN_POINT('',(18.5446545936727,-0.888979979456325,-333.864249094225)) ;
#44572 = CARTESIAN_POINT('',(18.544654593745,-0.888979977948782,-315.477129595899)) ;
#44573 = CARTESIAN_POINT('Ctrl Pts',(18.5446545951453,-0.888979948736927,
-334.159397110264)) ;
#44574 = CARTESIAN_POINT('Ctrl Pts',(18.5692830990318,-0.37521459506579,-334.153090696754)) ;
#44575 = CARTESIAN_POINT('Ctrl Pts',(18.5725507246078,0.139351443153365,-334.14674863002)) ;
#44576 = CARTESIAN_POINT('Ctrl Pts',(18.5498213412484,0.784805709244924,-334.138615311045)) ;
#44577 = CARTESIAN_POINT('Ctrl Pts',(18.5437973724742,0.916171788360239,-334.136951158575)) ;
#44578 = CARTESIAN_POINT('Ctrl Pts',(18.5298187220353,1.16354438066611,-334.133798953664)) ;
#44579 = CARTESIAN_POINT('Ctrl Pts',(18.5221688495189,1.27956182573606,-334.132312908977)) ;
#44580 = CARTESIAN_POINT('Ctrl Pts',(18.5039344669633,1.52146869963332,-334.129197490693)) ;
#44581 = CARTESIAN_POINT('Ctrl Pts',(18.4931537900458,1.64733742915553,-334.127566917763)) ;
#44582 = CARTESIAN_POINT('Ctrl Pts',(18.4633853879098,1.95761704116994,-334.123523240871)) ;
#44583 = CARTESIAN_POINT('Ctrl Pts',(18.4429186453917,2.14187211037741,-334.121100800655)) ;
#44584 = CARTESIAN_POINT('Ctrl Pts',(18.3594588929034,2.802853369882,-334.112336877021)) ;
#44585 = CARTESIAN_POINT('Ctrl Pts',(18.2807109584137,3.27739567166514,-334.105901468451)) ;
#44586 = CARTESIAN_POINT('Ctrl Pts',(18.0625214680297,4.33585721756017,-334.091357686981)) ;
#44587 = CARTESIAN_POINT('Ctrl Pts',(17.9130095474824,4.91715660980554,-334.083234044209)) ;
#44588 = CARTESIAN_POINT('Ctrl Pts',(17.7080335944691,5.57931436451973,-334.074123382003)) ;
#44589 = CARTESIAN_POINT('Ctrl Pts',(17.6797749559515,5.66822371659494,-334.072903407742)) ;
#44590 = CARTESIAN_POINT('Ctrl Pts',(17.6341251077477,5.80818727544336,-334.070990223011)) ;
#44591 = CARTESIAN_POINT('Ctrl Pts',(17.6171795104917,5.85938510809401,-334.070291949485)) ;
#44592 = CARTESIAN_POINT('Ctrl Pts',(17.5786718350788,5.97405130371369,-334.068732139851)) ;
#44593 = CARTESIAN_POINT('Ctrl Pts',(17.5569886692368,6.03747805985553,-334.067872322134)) ;
#44594 = CARTESIAN_POINT('Ctrl Pts',(17.5068765580993,6.18151097362589,-334.065925587167)) ;
#44595 = CARTESIAN_POINT('Ctrl Pts',(17.4782334987114,6.26204108329537,-334.064841209301)) ;
#44596 = CARTESIAN_POINT('Ctrl Pts',(17.3497200452353,6.61560537919624,-334.060092859409)) ;
#44597 = CARTESIAN_POINT('Ctrl Pts',(17.244000317387,6.88647035464091,-334.05648769146)) ;
#44598 = CARTESIAN_POINT('Ctrl Pts',(17.0806633808841,7.27757918171694,-334.051267392867)) ;
#44599 = CARTESIAN_POINT('Ctrl Pts',(17.0280434709812,7.39986188069287,-334.049633203596)) ;
#44600 = CARTESIAN_POINT('Ctrl Pts',(16.7795470644528,7.96065000708573,-334.042113015239)) ;
#44601 = CARTESIAN_POINT('Ctrl Pts',(16.5680172306455,8.39201722617697,-334.036250076017)) ;
#44602 = CARTESIAN_POINT('Ctrl Pts',(16.2388160084323,9.00226497050727,-334.027658724401)) ;
#44603 = CARTESIAN_POINT('Ctrl Pts',(16.1344088880154,9.18807757900674,-334.025002270858)) ;
#44604 = CARTESIAN_POINT('Ctrl Pts',(15.9412332871798,9.51842060476988,-334.020194004397)) ;
#44605 = CARTESIAN_POINT('Ctrl Pts',(15.8536394513711,9.66361037874798,-334.018050305824)) ;
#44606 = CARTESIAN_POINT('Ctrl Pts',(15.7070164604246,9.89928268928725,-334.01451689974)) ;
#44607 = CARTESIAN_POINT('Ctrl Pts',(15.6491646340442,9.99048597786419,-334.013136086918)) ;
#44608 = CARTESIAN_POINT('Ctrl Pts',(15.5219760540935,10.1871828227723,-334.010128137392)) ;
#44609 = CARTESIAN_POINT('Ctrl Pts',(15.4523524836459,10.2924844986942,-334.008498839566)) ;
#44610 = CARTESIAN_POINT('Ctrl Pts',(15.2950159774999,10.5252517325553,-334.004854276294)) ;
#44611 = CARTESIAN_POINT('Ctrl Pts',(15.2067725995651,10.6523473842412,-334.002835003797)) ;
#44612 = CARTESIAN_POINT('Ctrl Pts',(14.7012089519089,11.361416823867,-333.991404950764)) ;
#44613 = CARTESIAN_POINT('Ctrl Pts',(14.2520796862702,11.9199644773943,-333.981742644226)) ;
#44614 = CARTESIAN_POINT('Ctrl Pts',(13.5835439141688,12.6594093651944,-333.968325100605)) ;
#44615 = CARTESIAN_POINT('Ctrl Pts',(13.3905720599802,12.8633545765292,-333.964555456458)) ;
#44616 = CARTESIAN_POINT('Ctrl Pts',(13.0680413219491,13.1891001504586,-333.95846528223)) ;
#44617 = CARTESIAN_POINT('Ctrl Pts',(12.9412266317032,13.3135540044423,-333.956121271594)) ;
#44618 = CARTESIAN_POINT('Ctrl Pts',(12.7544635830763,13.4916500616955,-333.952754032292)) ;
#44619 = CARTESIAN_POINT('Ctrl Pts',(12.6959223057353,13.5467530984379,-333.951710373808)) ;
#44620 = CARTESIAN_POINT('Ctrl Pts',(12.5883596461338,13.6466887370341,-333.94981579123)) ;
#44621 = CARTESIAN_POINT('Ctrl Pts',(12.5394521574716,13.6916416711179,-333.948963062504)) ;
#44622 = CARTESIAN_POINT('Ctrl Pts',(12.4176786583323,13.8023690588317,-333.946860518498)) ;
#44623 = CARTESIAN_POINT('Ctrl Pts',(12.3445302483214,13.8678299631384,-333.945615476673)) ;
#44624 = CARTESIAN_POINT('Ctrl Pts',(12.0012220180292,14.1701896620871,-333.939846560031)) ;
#44625 = CARTESIAN_POINT('Ctrl Pts',(11.7247399425815,14.3997944263043,-333.935411730716)) ;
#44626 = CARTESIAN_POINT('Ctrl Pts',(10.9086096140476,15.0384529981051,-333.922687356617)) ;
#44627 = CARTESIAN_POINT('Ctrl Pts',(10.3530271884397,15.4262004709477,-333.914449845671)) ;
#44628 = CARTESIAN_POINT('Ctrl Pts',(9.59285037226465,15.8971352391819,-333.903272452604)) ;
#44629 = CARTESIAN_POINT('Ctrl Pts',(9.40619431640646,16.008285208616,-333.900536990305)) ;
#44630 = CARTESIAN_POINT('Ctrl Pts',(9.1021433642462,16.1821873071397,-333.8960870842)) ;
#44631 = CARTESIAN_POINT('Ctrl Pts',(8.98594903340544,16.2469972540788,-333.894387970544)) ;
#44632 = CARTESIAN_POINT('Ctrl Pts',(8.75825228644693,16.3708102256992,-333.891059844996)) ;
#44633 = CARTESIAN_POINT('Ctrl Pts',(8.64682519713828,16.4299368384491,-333.889431860268)) ;
#44634 = CARTESIAN_POINT('Ctrl Pts',(8.39778883853749,16.5588479544717,-333.885794395821)) ;
#44635 = CARTESIAN_POINT('Ctrl Pts',(8.25989474318021,16.6280618741974,-333.883780964798)) ;
#44636 = CARTESIAN_POINT('Ctrl Pts',(7.47187998009878,17.0113729819262,-333.872280354112)) ;
#44637 = CARTESIAN_POINT('Ctrl Pts',(6.80473730189455,17.2890526868623,-333.862536633007)) ;
#44638 = CARTESIAN_POINT('Ctrl Pts',(5.86093735137052,17.6187697192086,-333.849081427472)) ;
#44639 = CARTESIAN_POINT('Ctrl Pts',(5.5967244496135,17.704471435148,-333.845352811526)) ;
#44640 = CARTESIAN_POINT('Ctrl Pts',(5.16163428212565,17.8348865430217,-333.839319127925)) ;
#44641 = CARTESIAN_POINT('Ctrl Pts',(4.99186582908364,17.8831463170608,-333.836991066754)) ;
#44642 = CARTESIAN_POINT('Ctrl Pts',(4.74397920997699,17.9498076288454,-333.833641974073)) ;
#44643 = CARTESIAN_POINT('Ctrl Pts',(4.66638920507221,17.9701347927033,-333.832600805548)) ;
#44644 = CARTESIAN_POINT('Ctrl Pts',(4.52426470362131,18.0063862611952,-333.830708224011)) ;
#44645 = CARTESIAN_POINT('Ctrl Pts',(4.45977193103318,18.0224679667486,-333.829855039123)) ;
#44646 = CARTESIAN_POINT('Ctrl Pts',(4.29950209943545,18.0615193633396,-333.82774787789)) ;
#44647 = CARTESIAN_POINT('Ctrl Pts',(4.20362595769419,18.0840739011969,-333.826498728546)) ;
#44648 = CARTESIAN_POINT('Ctrl Pts',(3.77175816303019,18.1820492988108,-333.820914791877)) ;
#44649 = CARTESIAN_POINT('Ctrl Pts',(3.43388608153248,18.2488767828614,-333.816661098102)) ;
#44650 = CARTESIAN_POINT('Ctrl Pts',(2.68726277554283,18.3750802405742,-333.807359209547)) ;
#44651 = CARTESIAN_POINT('Ctrl Pts',(2.27799271379392,18.4302931196425,-333.802322862565)) ;
#44652 = CARTESIAN_POINT('Ctrl Pts',(1.46364213842278,18.5126117262138,-333.792248250432)) ;
#44653 = CARTESIAN_POINT('Ctrl Pts',(1.05883351414502,18.5401702184589,-333.787214228111)) ;
#44654 = CARTESIAN_POINT('Ctrl Pts',(0.494473051735657,18.5600458076499,-333.78009006683)) ;
#44655 = CARTESIAN_POINT('Ctrl Pts',(0.335432275881041,18.5636011880126,-333.778071112791)) ;
#44656 = CARTESIAN_POINT('Ctrl Pts',(0.0521132528771823,18.5662926741285,
-333.774451608744)) ;
#44657 = CARTESIAN_POINT('Ctrl Pts',(-0.0721477423311649,18.5662256289417,
-333.772856305163)) ;
#44658 = CARTESIAN_POINT('Ctrl Pts',(-0.34071551233004,18.5633844449062,-333.769390625146)) ;
#44659 = CARTESIAN_POINT('Ctrl Pts',(-0.485009577318701,18.560174965229,-333.767517538534)) ;
#44660 = CARTESIAN_POINT('Ctrl Pts',(-0.913808476523894,18.5456334302443,
-333.761918219622)) ;
#44661 = CARTESIAN_POINT('Ctrl Pts',(-1.19810533775556,18.5294389634879,-333.75816198962)) ;
#44662 = CARTESIAN_POINT('Ctrl Pts',(-2.10139076772849,18.4571087950124,-333.746107531459)) ;
#44663 = CARTESIAN_POINT('Ctrl Pts',(-2.71798323154306,18.3764325132396,-333.737686877406)) ;
#44664 = CARTESIAN_POINT('Ctrl Pts',(-3.53802108650753,18.2269550613262,-333.726503384322)) ;
#44665 = CARTESIAN_POINT('Ctrl Pts',(-3.74601189793647,18.1853479229615,-333.723669825537)) ;
#44666 = CARTESIAN_POINT('Ctrl Pts',(-4.09790431537208,18.1086609116143,-333.718902910338)) ;
#44667 = CARTESIAN_POINT('Ctrl Pts',(-4.24218232867045,18.075406191845,-333.716956297397)) ;
#44668 = CARTESIAN_POINT('Ctrl Pts',(-4.45930081313688,18.0226196465507,-333.714046435685)) ;
#44669 = CARTESIAN_POINT('Ctrl Pts',(-4.5324452648662,18.0043639878663,-333.713069512077)) ;
#44670 = CARTESIAN_POINT('Ctrl Pts',(-4.67065480223079,17.9689735342331,-333.711231325064)) ;
#44671 = CARTESIAN_POINT('Ctrl Pts',(-4.73574178028643,17.9519295881244,-333.710369064216)) ;
#44672 = CARTESIAN_POINT('Ctrl Pts',(-4.9055812912154,17.9064667671088,-333.708126543744)) ;
#44673 = CARTESIAN_POINT('Ctrl Pts',(-5.01017991395002,17.87748240578,-333.706752842434)) ;
#44674 = CARTESIAN_POINT('Ctrl Pts',(-5.34894532859809,17.7804036015817,-333.702319879708)) ;
#44675 = CARTESIAN_POINT('Ctrl Pts',(-5.58202630834632,17.7086123413543,-333.699294652362)) ;
#44676 = CARTESIAN_POINT('Ctrl Pts',(-6.37225276910644,17.448062459815,-333.689037002683)) ;
#44677 = CARTESIAN_POINT('Ctrl Pts',(-6.92181120246833,17.237430787031,-333.681891415801)) ;
#44678 = CARTESIAN_POINT('Ctrl Pts',(-7.60725702771698,16.9366420850312,-333.672638052061)) ;
#44679 = CARTESIAN_POINT('Ctrl Pts',(-7.75323090664983,16.8703175736685,-333.67064796991)) ;
#44680 = CARTESIAN_POINT('Ctrl Pts',(-8.10618869083638,16.7043993664949,-333.665780508128)) ;
#44681 = CARTESIAN_POINT('Ctrl Pts',(-8.31221868165109,16.6028393233701,-333.662891954769)) ;
#44682 = CARTESIAN_POINT('Ctrl Pts',(-8.63647546490246,16.435451874502,-333.658259754524)) ;
#44683 = CARTESIAN_POINT('Ctrl Pts',(-8.7559585196429,16.372109733101,-333.656533972646)) ;
#44684 = CARTESIAN_POINT('Ctrl Pts',(-8.98581988854134,16.2470161496915,-333.653175737703)) ;
#44685 = CARTESIAN_POINT('Ctrl Pts',(-9.09628033315285,16.1854310070601,-333.651544577984)) ;
#44686 = CARTESIAN_POINT('Ctrl Pts',(-9.33624777553899,16.0484091735632,-333.647962346435)) ;
#44687 = CARTESIAN_POINT('Ctrl Pts',(-9.46548800247803,15.9725231668492,-333.646008046625)) ;
#44688 = CARTESIAN_POINT('Ctrl Pts',(-9.99026865752007,15.6557812670232,-333.637970515521)) ;
#44689 = CARTESIAN_POINT('Ctrl Pts',(-10.3776488787435,15.4017322558545,-333.631792861434)) ;
#44690 = CARTESIAN_POINT('Ctrl Pts',(-11.1365818345413,14.862370214123,-333.61928034052)) ;
#44691 = CARTESIAN_POINT('Ctrl Pts',(-11.5076536681429,14.5769479049027,-333.612949141621)) ;
#44692 = CARTESIAN_POINT('Ctrl Pts',(-11.9936612400819,14.1729842911952,-333.60450731056)) ;
#44693 = CARTESIAN_POINT('Ctrl Pts',(-12.1183841170804,14.066490684263,-333.602327403826)) ;
#44694 = CARTESIAN_POINT('Ctrl Pts',(-12.3347543696887,13.8767308829797,-333.598532814423)) ;
#44695 = CARTESIAN_POINT('Ctrl Pts',(-12.4270102791998,13.7941741672047,-333.596910668063)) ;
#44696 = CARTESIAN_POINT('Ctrl Pts',(-12.5707030980533,13.6629767147845,-333.594382168563)) ;
#44697 = CARTESIAN_POINT('Ctrl Pts',(-12.6226992443621,13.6149540174045,-333.593466814658)) ;
#44698 = CARTESIAN_POINT('Ctrl Pts',(-12.7200937472086,13.5239647056672,-333.591752626714)) ;
#44699 = CARTESIAN_POINT('Ctrl Pts',(-12.7655521980344,13.4810638819443,-333.590952677344)) ;
#44700 = CARTESIAN_POINT('Ctrl Pts',(-12.8948185414723,13.3578303287826,-333.588676933265)) ;
#44701 = CARTESIAN_POINT('Ctrl Pts',(-12.9780908578955,13.2769399357469,-333.587209698565)) ;
#44702 = CARTESIAN_POINT('Ctrl Pts',(-13.331639652637,12.9269995596112,-333.580962157566)) ;
#44703 = CARTESIAN_POINT('Ctrl Pts',(-13.5943507165442,12.650437279709,-333.576271993925)) ;
#44704 = CARTESIAN_POINT('Ctrl Pts',(-14.1678844608095,12.0081509177686,-333.565714991819)) ;
#44705 = CARTESIAN_POINT('Ctrl Pts',(-14.4734218025395,11.6380711347027,-333.559858378116)) ;
#44706 = CARTESIAN_POINT('Ctrl Pts',(-14.8520357558492,11.1414757484322,-333.552120820938)) ;
#44707 = CARTESIAN_POINT('Ctrl Pts',(-14.9384405700915,11.0253544714751,-333.550320186945)) ;
#44708 = CARTESIAN_POINT('Ctrl Pts',(-15.1494712252881,10.7347103304112,-333.545829066294)) ;
#44709 = CARTESIAN_POINT('Ctrl Pts',(-15.2724477531899,10.5590162268466,-333.543127874812)) ;
#44710 = CARTESIAN_POINT('Ctrl Pts',(-15.4664702909421,10.2713371235415,-333.538718752159)) ;
#44711 = CARTESIAN_POINT('Ctrl Pts',(-15.5394085003944,10.1606521918083,-333.537025604286)) ;
#44712 = CARTESIAN_POINT('Ctrl Pts',(-15.6795898404427,9.94288425436778,-333.533699481161)) ;
#44713 = CARTESIAN_POINT('Ctrl Pts',(-15.7469367700883,9.83587653262878,-333.532067425934)) ;
#44714 = CARTESIAN_POINT('Ctrl Pts',(-15.9106771142496,9.5697163749156,-333.528013256429)) ;
#44715 = CARTESIAN_POINT('Ctrl Pts',(-16.0057810010364,9.40978703854107,-333.52558169223)) ;
#44716 = CARTESIAN_POINT('Ctrl Pts',(-16.4164959449692,8.6948698192667,-333.514734724878)) ;
#44717 = CARTESIAN_POINT('Ctrl Pts',(-16.7057598459684,8.125249703337,-333.506135488341)) ;
#44718 = CARTESIAN_POINT('Ctrl Pts',(-17.090972395195,7.25873065620679,-333.493364243733)) ;
#44719 = CARTESIAN_POINT('Ctrl Pts',(-17.2097332866985,6.97248798422702,-333.4891967115)) ;
#44720 = CARTESIAN_POINT('Ctrl Pts',(-17.3892050262139,6.50735408952412,-333.482565162445)) ;
#44721 = CARTESIAN_POINT('Ctrl Pts',(-17.4544472120541,6.33027498883063,-333.48007279)) ;
#44722 = CARTESIAN_POINT('Ctrl Pts',(-17.5441772127584,6.0747907152436,-333.476537569209)) ;
#44723 = CARTESIAN_POINT('Ctrl Pts',(-17.5708619455238,5.99716990116247,-333.475471481229)) ;
#44724 = CARTESIAN_POINT('Ctrl Pts',(-17.6181163218021,5.85669277619681,-333.473558119492)) ;
#44725 = CARTESIAN_POINT('Ctrl Pts',(-17.6388664331624,5.79389885605945,-333.472708749965)) ;
#44726 = CARTESIAN_POINT('Ctrl Pts',(-17.6887291968813,5.64025354774623,-333.470644250884)) ;
#44727 = CARTESIAN_POINT('Ctrl Pts',(-17.7174779456772,5.54928607709174,-333.469433449243)) ;
#44728 = CARTESIAN_POINT('Ctrl Pts',(-17.8342297195443,5.16969957900751,-333.464421803735)) ;
#44729 = CARTESIAN_POINT('Ctrl Pts',(-17.915891486114,4.87917784760495,-333.460683097522)) ;
#44730 = CARTESIAN_POINT('Ctrl Pts',(-18.1301344319383,4.03886902972851,-333.45000879692)) ;
#44731 = CARTESIAN_POINT('Ctrl Pts',(-18.2447273919423,3.48484733495916,-333.443132978278)) ;
#44732 = CARTESIAN_POINT('Ctrl Pts',(-18.36987529007,2.70081382021052,-333.433314142055)) ;
#44733 = CARTESIAN_POINT('Ctrl Pts',(-18.4017243567966,2.4745209508225,-333.430471384381)) ;
#44734 = CARTESIAN_POINT('Ctrl Pts',(-18.4524154644303,2.05889304739787,-333.425218042883)) ;
#44735 = CARTESIAN_POINT('Ctrl Pts',(-18.4725398633097,1.86974540628183,-333.422815256417)) ;
#44736 = CARTESIAN_POINT('Ctrl Pts',(-18.5013730181646,1.5524741441585,-333.418759437293)) ;
#44737 = CARTESIAN_POINT('Ctrl Pts',(-18.5116653282435,1.42450912418015,-333.417116728114)) ;
#44738 = CARTESIAN_POINT('Ctrl Pts',(-18.5298379766709,1.16490060248909,-333.41376909457)) ;
#44739 = CARTESIAN_POINT('Ctrl Pts',(-18.5376445174144,1.0332591834301,-333.412063787439)) ;
#44740 = CARTESIAN_POINT('Ctrl Pts',(-18.5542722681086,0.691240208612273,
-333.407612518334)) ;
#44741 = CARTESIAN_POINT('Ctrl Pts',(-18.560918255816,0.480776131755427,-333.404852958042)) ;
#44742 = CARTESIAN_POINT('Ctrl Pts',(-18.5683727225125,-0.0312949001774819,
-333.398092566935)) ;
#44743 = CARTESIAN_POINT('Ctrl Pts',(-18.5654147377214,-0.332896377994954,
-333.394071376608)) ;
#44744 = CARTESIAN_POINT('Ctrl Pts',(-18.53738235311,-1.15293620149796,-333.38306718218)) ;
#44745 = CARTESIAN_POINT('Ctrl Pts',(-18.4979153065857,-1.67060915684535,
-333.376038559188)) ;
#44746 = CARTESIAN_POINT('Ctrl Pts',(-18.4166079898426,-2.3563751073202,-333.36680614447)) ;
#44747 = CARTESIAN_POINT('Ctrl Pts',(-18.3940391067207,-2.52651518302799,
-333.364522764008)) ;
#44748 = CARTESIAN_POINT('Ctrl Pts',(-18.3505456388797,-2.82282166304914,
-333.360571273815)) ;
#44749 = CARTESIAN_POINT('Ctrl Pts',(-18.3306704145828,-2.9491303158564,-333.358894870481)) ;
#44750 = CARTESIAN_POINT('Ctrl Pts',(-18.2976362631068,-3.14581146565148,
-333.356302171456)) ;
#44751 = CARTESIAN_POINT('Ctrl Pts',(-18.2853723783848,-3.21633014411529,
-333.35537614589)) ;
#44752 = CARTESIAN_POINT('Ctrl Pts',(-18.2617300550024,-3.34776869689039,
-333.353657964594)) ;
#44753 = CARTESIAN_POINT('Ctrl Pts',(-18.2504537970105,-3.4087059216986,-333.352864548875)) ;
#44754 = CARTESIAN_POINT('Ctrl Pts',(-18.2177727128358,-3.58050342308387,
-333.350635298725)) ;
#44755 = CARTESIAN_POINT('Ctrl Pts',(-18.1956613899698,-3.69122662803234,
-333.349207476479)) ;
#44756 = CARTESIAN_POINT('Ctrl Pts',(-18.1047247376207,-4.12590903588858,
-333.34362636548)) ;
#44757 = CARTESIAN_POINT('Ctrl Pts',(-18.0282461089619,-4.44820484537856,
-333.33954052548)) ;
#44758 = CARTESIAN_POINT('Ctrl Pts',(-17.9267926501359,-4.82997719464514,
-333.334690492664)) ;
#44759 = CARTESIAN_POINT('Ctrl Pts',(-17.9100796345253,-4.89158684975666,
-333.333907524337)) ;
#44760 = CARTESIAN_POINT('Ctrl Pts',(-17.8849184428461,-4.98248136324957,
-333.3327514136)) ;
#44761 = CARTESIAN_POINT('Ctrl Pts',(-17.8767153708889,-5.01183357572234,
-333.332377924923)) ;
#44762 = CARTESIAN_POINT('Ctrl Pts',(-17.8622613012014,-5.06306610916138,
-333.331725690591)) ;
#44763 = CARTESIAN_POINT('Ctrl Pts',(-17.8560422817328,-5.0849553833973,-333.331446915185)) ;
#44764 = CARTESIAN_POINT('Ctrl Pts',(-17.7289416419351,-5.52920699078976,
-333.325786573104)) ;
#44765 = CARTESIAN_POINT('Ctrl Pts',(-17.5931466062252,-5.94715846502317,
-333.320411877526)) ;
#44766 = CARTESIAN_POINT('Ctrl Pts',(-17.3726313318442,-6.55194358233835,
-333.312426210817)) ;
#44767 = CARTESIAN_POINT('Ctrl Pts',(-17.2994413886565,-6.7428192594266,-333.309875342685)) ;
#44768 = CARTESIAN_POINT('Ctrl Pts',(-17.1574812137254,-7.09550804337873,
-333.305094131393)) ;
#44769 = CARTESIAN_POINT('Ctrl Pts',(-17.0895355599389,-7.25762841460121,
-333.30286922916)) ;
#44770 = CARTESIAN_POINT('Ctrl Pts',(-16.968893916478,-7.53439114756365,-333.299020155823)) ;
#44771 = CARTESIAN_POINT('Ctrl Pts',(-16.9173125995371,-7.64950619776049,
-333.297403882696)) ;
#44772 = CARTESIAN_POINT('Ctrl Pts',(-16.8076829591078,-7.88763542036514,
-333.294027515067)) ;
#44773 = CARTESIAN_POINT('Ctrl Pts',(-16.7494477877459,-8.01055539379359,
-333.29226616257)) ;
#44774 = CARTESIAN_POINT('Ctrl Pts',(-16.5872887736351,-8.34333184907166,
-333.287446739549)) ;
#44775 = CARTESIAN_POINT('Ctrl Pts',(-16.4807369767188,-8.55187953532895,
-333.284370415212)) ;
#44776 = CARTESIAN_POINT('Ctrl Pts',(-16.2545256582397,-8.97469180329129,
-333.2780226828)) ;
#44777 = CARTESIAN_POINT('Ctrl Pts',(-16.1345054089778,-9.18871222005039,
-333.274749568037)) ;
#44778 = CARTESIAN_POINT('Ctrl Pts',(-15.7422714225201,-9.85675279015021,
-333.264365137266)) ;
#44779 = CARTESIAN_POINT('Ctrl Pts',(-15.4548658599776,-10.3015438385861,
-333.257194560458)) ;
#44780 = CARTESIAN_POINT('Ctrl Pts',(-15.0487989196275,-10.8746540419668,
-333.247802727714)) ;
#44781 = CARTESIAN_POINT('Ctrl Pts',(-14.9467784414668,-11.0144570366248,
-333.245499818777)) ;
#44782 = CARTESIAN_POINT('Ctrl Pts',(-14.7655569543291,-11.2556372227482,
-333.241518848225)) ;
#44783 = CARTESIAN_POINT('Ctrl Pts',(-14.68722915737,-11.3576556218177,-333.239832332498)) ;
#44784 = CARTESIAN_POINT('Ctrl Pts',(-14.5635794938802,-11.5152853247837,
-333.237227681259)) ;
#44785 = CARTESIAN_POINT('Ctrl Pts',(-14.5189847332259,-11.5714617106029,
-333.236299677707)) ;
#44786 = CARTESIAN_POINT('Ctrl Pts',(-14.4353110320079,-11.6756209287948,
-333.23458064765)) ;
#44787 = CARTESIAN_POINT('Ctrl Pts',(-14.3963155664725,-11.723669510049,-333.233788334913)) ;
#44788 = CARTESIAN_POINT('Ctrl Pts',(-14.2858413079411,-11.8584089090477,
-333.231567079246)) ;
#44789 = CARTESIAN_POINT('Ctrl Pts',(-14.2138146635012,-11.9446471902443,
-333.230146054956)) ;
#44790 = CARTESIAN_POINT('Ctrl Pts',(-13.98853429261,-12.2094544990122,-333.22577622842)) ;
#44791 = CARTESIAN_POINT('Ctrl Pts',(-13.8326651170548,-12.3857679185673,
-333.222857415561)) ;
#44792 = CARTESIAN_POINT('Ctrl Pts',(-13.2749867479253,-12.9929312737018,
-333.212693575408)) ;
#44793 = CARTESIAN_POINT('Ctrl Pts',(-12.8560631429616,-13.4075791339206,
-333.205537449396)) ;
#44794 = CARTESIAN_POINT('Ctrl Pts',(-12.2988693475015,-13.9089198972071,
-333.196271867447)) ;
#44795 = CARTESIAN_POINT('Ctrl Pts',(-12.1782161773896,-14.0146812520494,
-333.194280448067)) ;
#44796 = CARTESIAN_POINT('Ctrl Pts',(-11.8814612471979,-14.2680825636807,
-333.189410364834)) ;
#44797 = CARTESIAN_POINT('Ctrl Pts',(-11.7039600957701,-14.4140424313026,
-333.186520524698)) ;
#44798 = CARTESIAN_POINT('Ctrl Pts',(-11.4177533764113,-14.6406181413896,
-333.181886792184)) ;
#44799 = CARTESIAN_POINT('Ctrl Pts',(-11.3107969897057,-14.7234052827344,
-333.180160786767)) ;
#44800 = CARTESIAN_POINT('Ctrl Pts',(-11.1021051831103,-14.8813222298902,
-333.176802437003)) ;
#44801 = CARTESIAN_POINT('Ctrl Pts',(-11.000487798258,-14.9565958343809,-333.175171389659)) ;
#44802 = CARTESIAN_POINT('Ctrl Pts',(-10.7768104118294,-15.1187732650137,
-333.171589794287)) ;
#44803 = CARTESIAN_POINT('Ctrl Pts',(-10.6544513640579,-15.2052495452927,
-333.16963602323)) ;
#44804 = CARTESIAN_POINT('Ctrl Pts',(-9.91982750880368,-15.7112173847607,
-333.157939549185)) ;
#44805 = CARTESIAN_POINT('Ctrl Pts',(-9.283904202491,-16.0951683027597,-333.1479207311)) ;
#44806 = CARTESIAN_POINT('Ctrl Pts',(-8.27316496431097,-16.625542304717,-333.132560644341)) ;
#44807 = CARTESIAN_POINT('Ctrl Pts',(-7.91372136979153,-16.7996110258989,
-333.127207769158)) ;
#44808 = CARTESIAN_POINT('Ctrl Pts',(-7.45779720944002,-17.002520805654,-333.120660130185)) ;
#44809 = CARTESIAN_POINT('Ctrl Pts',(-7.36632342917403,-17.0423511330805,
-333.1193585085)) ;
#44810 = CARTESIAN_POINT('Ctrl Pts',(-7.21323448595236,-17.1075476515262,
-333.117202866894)) ;
#44811 = CARTESIAN_POINT('Ctrl Pts',(-7.15179588484512,-17.1333229134784,
-333.116343875141)) ;
#44812 = CARTESIAN_POINT('Ctrl Pts',(-7.01673177460878,-17.1891331129643,
-333.11446953512)) ;
#44813 = CARTESIAN_POINT('Ctrl Pts',(-6.94304950495508,-17.2190268472688,
-333.113455875768)) ;
#44814 = CARTESIAN_POINT('Ctrl Pts',(-6.70924650779701,-17.3121386693541,
-333.110264227876)) ;
#44815 = CARTESIAN_POINT('Ctrl Pts',(-6.54843721916864,-17.3736036611754,
-333.108105618731)) ;
#44816 = CARTESIAN_POINT('Ctrl Pts',(-5.59749910868084,-17.7219951867835,
-333.095499404855)) ;
#44817 = CARTESIAN_POINT('Ctrl Pts',(-4.7894729398757,-17.9572288907603,-333.085379532532)) ;
#44818 = CARTESIAN_POINT('Ctrl Pts',(-3.71710613448742,-18.1918590541924,
-333.071720796045)) ;
#44819 = CARTESIAN_POINT('Ctrl Pts',(-3.46480671498847,-18.2415933491819,
-333.068495469153)) ;
#44820 = CARTESIAN_POINT('Ctrl Pts',(-3.07374632681347,-18.3102747194317,
-333.063462976479)) ;
#44821 = CARTESIAN_POINT('Ctrl Pts',(-2.93566733276767,-18.3329194080751,
-333.061679801131)) ;
#44822 = CARTESIAN_POINT('Ctrl Pts',(-2.67380805737983,-18.3728295571781,
-333.058284644254)) ;
#44823 = CARTESIAN_POINT('Ctrl Pts',(-2.55008357236757,-18.3904102506348,
-333.056674829264)) ;
#44824 = CARTESIAN_POINT('Ctrl Pts',(-2.26391990133328,-18.4281294636121,
-333.052937799777)) ;
#44825 = CARTESIAN_POINT('Ctrl Pts',(-2.10137310712073,-18.4473716230041,
-333.050804917556)) ;
#44826 = CARTESIAN_POINT('Ctrl Pts',(-1.48812799914729,-18.5117565419224,
-333.042720739618)) ;
#44827 = CARTESIAN_POINT('Ctrl Pts',(-1.03608411202386,-18.5425506028167,
-333.036681729249)) ;
#44828 = CARTESIAN_POINT('Ctrl Pts',(-0.544158216969694,-18.5580152554972,
-333.030069792708)) ;
#44829 = CARTESIAN_POINT('Ctrl Pts',(-0.504943872655379,-18.5591236343007,
-333.029542473251)) ;
#44830 = CARTESIAN_POINT('Ctrl Pts',(0.0372160390379098,-18.5727279808557,
-333.022249287284)) ;
#44831 = CARTESIAN_POINT('Ctrl Pts',(0.540463392778109,-18.5648999197735,
-333.015440918262)) ;
#44832 = CARTESIAN_POINT('Ctrl Pts',(1.23205076363308,-18.5259950052167,-333.006226404174)) ;
#44833 = CARTESIAN_POINT('Ctrl Pts',(1.42115774437797,-18.5124485389726,-333.003722245486)) ;
#44834 = CARTESIAN_POINT('Ctrl Pts',(1.69192281180645,-18.4888792196527,-333.000173742365)) ;
#44835 = CARTESIAN_POINT('Ctrl Pts',(1.7737732018656,-18.4812062986659,-332.999105928424)) ;
#44836 = CARTESIAN_POINT('Ctrl Pts',(1.92135361262873,-18.4663821807441,-332.997191069649)) ;
#44837 = CARTESIAN_POINT('Ctrl Pts',(1.98710131570599,-18.4594230383671,-332.996341906909)) ;
#44838 = CARTESIAN_POINT('Ctrl Pts',(2.1474303671283,-18.4415863182516,-332.994280091972)) ;
#44839 = CARTESIAN_POINT('Ctrl Pts',(2.24196789579737,-18.4303321485726,-332.9930717359)) ;
#44840 = CARTESIAN_POINT('Ctrl Pts',(2.6310336042233,-18.3809781729037,-332.98812232515)) ;
#44841 = CARTESIAN_POINT('Ctrl Pts',(2.92471402419203,-18.3365412509288,-332.984441352276)) ;
#44842 = CARTESIAN_POINT('Ctrl Pts',(3.35323236843257,-18.2611447917583,-332.979084366988)) ;
#44843 = CARTESIAN_POINT('Ctrl Pts',(3.48899117366929,-18.2356934894022,-332.977389420714)) ;
#44844 = CARTESIAN_POINT('Ctrl Pts',(3.6503414371363,-18.2035766689314,-332.975372888862)) ;
#44845 = CARTESIAN_POINT('Ctrl Pts',(3.67621850707237,-18.1983684333975,-332.975049418475)) ;
#44846 = CARTESIAN_POINT('Ctrl Pts',(4.14721753276944,-18.102525632827,-332.969160193723)) ;
#44847 = CARTESIAN_POINT('Ctrl Pts',(4.5888763651798,-17.9956400538634,-332.96360726497)) ;
#44848 = CARTESIAN_POINT('Ctrl Pts',(5.1613354044454,-17.8346525368428,-332.956233668114)) ;
#44849 = CARTESIAN_POINT('Ctrl Pts',(5.29606622703783,-17.7951087867409,-332.954485658933)) ;
#44850 = CARTESIAN_POINT('Ctrl Pts',(5.63121336889924,-17.6925990857405,-332.950100840433)) ;
#44851 = CARTESIAN_POINT('Ctrl Pts',(5.83103379149865,-17.6277528663971,-332.94745349345)) ;
#44852 = CARTESIAN_POINT('Ctrl Pts',(6.15434988998392,-17.5167303917779,-332.943108402183)) ;
#44853 = CARTESIAN_POINT('Ctrl Pts',(6.27852995990068,-17.4726050624739,-332.941424597006)) ;
#44854 = CARTESIAN_POINT('Ctrl Pts',(6.52138634063726,-17.3833867285,-332.938100962584)) ;
#44855 = CARTESIAN_POINT('Ctrl Pts',(6.64009087741226,-17.3383911318642,-332.936461879296)) ;
#44856 = CARTESIAN_POINT('Ctrl Pts',(6.9345918049107,-17.2232909747025,-332.932358509805)) ;
#44857 = CARTESIAN_POINT('Ctrl Pts',(7.10979519491607,-17.1517091746467,-332.929884237081)) ;
#44858 = CARTESIAN_POINT('Ctrl Pts',(7.61203546791065,-16.9374938158835,-332.922697475816)) ;
#44859 = CARTESIAN_POINT('Ctrl Pts',(7.93609426646273,-16.7880966034519,-332.917942614331)) ;
#44860 = CARTESIAN_POINT('Ctrl Pts',(8.33557230198092,-16.5897768638928,-332.911958661224)) ;
#44861 = CARTESIAN_POINT('Ctrl Pts',(8.41521118746939,-16.5495221277923,-332.910759603925)) ;
#44862 = CARTESIAN_POINT('Ctrl Pts',(8.70344943512226,-16.40120900095,-332.906399509063)) ;
#44863 = CARTESIAN_POINT('Ctrl Pts',(8.91028319052653,-16.2897680215416,-332.903231597078)) ;
#44864 = CARTESIAN_POINT('Ctrl Pts',(9.35693018908766,-16.0380643855839,-332.896331454507)) ;
#44865 = CARTESIAN_POINT('Ctrl Pts',(9.59582367187074,-15.8962832185917,-332.892602377735)) ;
#44866 = CARTESIAN_POINT('Ctrl Pts',(9.98116717012184,-15.6557322764152,-332.886568058921)) ;
#44867 = CARTESIAN_POINT('Ctrl Pts',(10.1295480204247,-15.5601384402183,-332.884239817908)) ;
#44868 = CARTESIAN_POINT('Ctrl Pts',(10.34334515574,-15.418046049537,-332.880890520515)) ;
#44869 = CARTESIAN_POINT('Ctrl Pts',(10.409858547089,-15.373216255875,-332.879849323828)) ;
#44870 = CARTESIAN_POINT('Ctrl Pts',(10.530954039724,-15.2904520616228,-332.87795671976)) ;
#44871 = CARTESIAN_POINT('Ctrl Pts',(10.5856267773618,-15.2526529810222,-332.877103540131)) ;
#44872 = CARTESIAN_POINT('Ctrl Pts',(10.7208050231096,-15.1581179217008,-332.874996431596)) ;
#44873 = CARTESIAN_POINT('Ctrl Pts',(10.8010643091807,-15.1010333785959,-332.87374732908)) ;
#44874 = CARTESIAN_POINT('Ctrl Pts',(11.1599329203825,-14.8414628188532,-332.868162609989)) ;
#44875 = CARTESIAN_POINT('Ctrl Pts',(11.4333301451273,-14.6318858762706,-332.863908122262)) ;
#44876 = CARTESIAN_POINT('Ctrl Pts',(12.0212907954074,-14.1546290028262,-332.854605456179)) ;
#44877 = CARTESIAN_POINT('Ctrl Pts',(12.3330734993834,-13.8838126197973,-332.849569113175)) ;
#44878 = CARTESIAN_POINT('Ctrl Pts',(12.8389638225102,-13.4138947703999,-332.841070371004)) ;
#44879 = CARTESIAN_POINT('Ctrl Pts',(13.0380963319374,-13.2204239209766,-332.837634644567)) ;
#44880 = CARTESIAN_POINT('Ctrl Pts',(13.3854128889989,-12.867499803572,-332.8314456633)) ;
#44881 = CARTESIAN_POINT('Ctrl Pts',(13.5352728976098,-12.7097685561562,-332.828706175293)) ;
#44882 = CARTESIAN_POINT('Ctrl Pts',(13.7722939630875,-12.4513506979463,-332.82425147736)) ;
#44883 = CARTESIAN_POINT('Ctrl Pts',(13.8612043676685,-12.3522964919465,-332.822551662309)) ;
#44884 = CARTESIAN_POINT('Ctrl Pts',(14.0322636603256,-12.1575482219666,-332.819223282005)) ;
#44885 = CARTESIAN_POINT('Ctrl Pts',(14.1145178856588,-12.0619561848061,-332.817595756327)) ;
#44886 = CARTESIAN_POINT('Ctrl Pts',(14.2951272822193,-11.8476829683592,-332.813960781191)) ;
#44887 = CARTESIAN_POINT('Ctrl Pts',(14.3929912802687,-11.7285999865457,-332.811949399969)) ;
#44888 = CARTESIAN_POINT('Ctrl Pts',(14.9427819225857,-11.0423576764162,-332.800409483092)) ;
#44889 = CARTESIAN_POINT('Ctrl Pts',(15.3626527370053,-10.4503247213044,-332.790621728403)) ;
#44890 = CARTESIAN_POINT('Ctrl Pts',(15.8930124970672,-9.60118825909509,-332.777148086387)) ;
#44891 = CARTESIAN_POINT('Ctrl Pts',(16.03397298161,-9.36388663691548,-332.773443414459)) ;
#44892 = CARTESIAN_POINT('Ctrl Pts',(16.2559757189144,-8.97043222789427,-332.767442758364)) ;
#44893 = CARTESIAN_POINT('Ctrl Pts',(16.3401816093379,-8.81611400160364,-332.765124063464)) ;
#44894 = CARTESIAN_POINT('Ctrl Pts',(16.459547058751,-8.58977447864423,-332.761785635381)) ;
#44895 = CARTESIAN_POINT('Ctrl Pts',(16.4964518984026,-8.51868474359152,-332.76074593629)) ;
#44896 = CARTESIAN_POINT('Ctrl Pts',(16.5631485078854,-8.38814830453622,-332.758854527169)) ;
#44897 = CARTESIAN_POINT('Ctrl Pts',(16.5930830832363,-8.3287762762166,-332.758001064639)) ;
#44898 = CARTESIAN_POINT('Ctrl Pts',(16.6666543092695,-8.18088462090552,-332.755891138458)) ;
#44899 = CARTESIAN_POINT('Ctrl Pts',(16.7099053305672,-8.09217541392718,-332.75463953383)) ;
#44900 = CARTESIAN_POINT('Ctrl Pts',(16.9002205556867,-7.69380033799361,-332.7490727928)) ;
#44901 = CARTESIAN_POINT('Ctrl Pts',(17.0393988278243,-7.38044085099692,-332.74483786168)) ;
#44902 = CARTESIAN_POINT('Ctrl Pts',(17.3716548903147,-6.57278856447777,-332.734109208009)) ;
#44903 = CARTESIAN_POINT('Ctrl Pts',(17.5523666019045,-6.0737443320153,-332.72764827758)) ;
#44904 = CARTESIAN_POINT('Ctrl Pts',(17.7782196889635,-5.35527436640358,-332.718327791977)) ;
#44905 = CARTESIAN_POINT('Ctrl Pts',(17.841154658909,-5.14171752177126,-332.715556268902)) ;
#44906 = CARTESIAN_POINT('Ctrl Pts',(17.9497913517044,-4.74703713211614,-332.710417468934)) ;
#44907 = CARTESIAN_POINT('Ctrl Pts',(17.9966295609324,-4.56625616796636,-332.708057379554)) ;
#44908 = CARTESIAN_POINT('Ctrl Pts',(18.0709180036974,-4.26060527506791,-332.704051595018)) ;
#44909 = CARTESIAN_POINT('Ctrl Pts',(18.0998201592889,-4.13610262839098,-332.702415626751)) ;
#44910 = CARTESIAN_POINT('Ctrl Pts',(18.1561050314027,-3.88174683897472,-332.699063668517)) ;
#44911 = CARTESIAN_POINT('Ctrl Pts',(18.1833857054804,-3.75187855035543,-332.697347105609)) ;
#44912 = CARTESIAN_POINT('Ctrl Pts',(18.2512659101287,-3.41059154049628,-332.692822216165)) ;
#44913 = CARTESIAN_POINT('Ctrl Pts',(18.2895845965861,-3.19873990971338,-332.689999401413)) ;
#44914 = CARTESIAN_POINT('Ctrl Pts',(18.3708577754708,-2.70003526168335,-332.683325378463)) ;
#44915 = CARTESIAN_POINT('Ctrl Pts',(18.41079185662,-2.41274709572377,-332.679457954179)) ;
#44916 = CARTESIAN_POINT('Ctrl Pts',(18.491288153212,-1.71396019208233,-332.670025252939)) ;
#44917 = CARTESIAN_POINT('Ctrl Pts',(18.5248630693649,-1.30184302996486,-332.664439221364)) ;
#44918 = CARTESIAN_POINT('Ctrl Pts',(18.5446545941347,-0.888979969817808,
-332.65888667131)) ;
#44919 = CARTESIAN_POINT('',(-0.00018199629320621,-18.565949999108,-332.726272944078)) ;
#44920 = CARTESIAN_POINT('Ctrl Pts',(18.544654593742,-0.888979978009869,-332.362654732516)) ;
#44921 = CARTESIAN_POINT('Ctrl Pts',(18.5409868706898,-0.965490876829128,
-332.363641300434)) ;
#44922 = CARTESIAN_POINT('Ctrl Pts',(18.5368456630169,-1.0419787767752,-332.364630914379)) ;
#44923 = CARTESIAN_POINT('Ctrl Pts',(18.5217124712218,-1.2927315997512,-332.367886299804)) ;
#44924 = CARTESIAN_POINT('Ctrl Pts',(18.5087355062214,-1.46686661895616,-332.370164677092)) ;
#44925 = CARTESIAN_POINT('Ctrl Pts',(18.4754067491204,-1.84251367258044,-332.375116982855)) ;
#44926 = CARTESIAN_POINT('Ctrl Pts',(18.4542100364302,-2.04392830592316,-332.37779565012)) ;
#44927 = CARTESIAN_POINT('Ctrl Pts',(18.3776161067625,-2.67271798459491,-332.386222756599)) ;
#44928 = CARTESIAN_POINT('Ctrl Pts',(18.3106326642475,-3.09853602029094,-332.392026252816)) ;
#44929 = CARTESIAN_POINT('Ctrl Pts',(18.1424767781622,-3.96895420045448,-332.403967813284)) ;
#44930 = CARTESIAN_POINT('Ctrl Pts',(18.0396235006283,-4.41294075369034,-332.410102143892)) ;
#44931 = CARTESIAN_POINT('Ctrl Pts',(17.8902346562831,-4.96461976450407,-332.417627154172)) ;
#44932 = CARTESIAN_POINT('Ctrl Pts',(17.8588782837582,-5.07625964389746,-332.419144621208)) ;
#44933 = CARTESIAN_POINT('Ctrl Pts',(17.8090195386367,-5.24759245222634,-332.421461410201)) ;
#44934 = CARTESIAN_POINT('Ctrl Pts',(17.791258235538,-5.30749789265439,-332.422269176853)) ;
#44935 = CARTESIAN_POINT('Ctrl Pts',(17.7527239993247,-5.43509927222149,-332.423983995539)) ;
#44936 = CARTESIAN_POINT('Ctrl Pts',(17.7318654957402,-5.50276835324022,-332.424889900873)) ;
#44937 = CARTESIAN_POINT('Ctrl Pts',(17.6734297404255,-5.68856272965468,-332.427369518159)) ;
#44938 = CARTESIAN_POINT('Ctrl Pts',(17.6350557814675,-5.80643370570242,-332.428934086973)) ;
#44939 = CARTESIAN_POINT('Ctrl Pts',(17.5430835655907,-6.07961426783794,-332.432548681069)) ;
#44940 = CARTESIAN_POINT('Ctrl Pts',(17.4885983982314,-6.2346144084199,-332.434590891464)) ;
#44941 = CARTESIAN_POINT('Ctrl Pts',(17.2703839569688,-6.83001348206777,-332.442431959297)) ;
#44942 = CARTESIAN_POINT('Ctrl Pts',(17.0920173096295,-7.26486005268108,-332.448155136249)) ;
#44943 = CARTESIAN_POINT('Ctrl Pts',(16.7063296984482,-8.11206469713462,-332.459584149927)) ;
#44944 = CARTESIAN_POINT('Ctrl Pts',(16.4997489320953,-8.52439613518244,-332.465284461519)) ;
#44945 = CARTESIAN_POINT('Ctrl Pts',(16.2060261536226,-9.05989162087997,-332.47297873807)) ;
#44946 = CARTESIAN_POINT('Ctrl Pts',(16.1324313039198,-9.19029814611917,-332.474875686368)) ;
#44947 = CARTESIAN_POINT('Ctrl Pts',(15.9937972000412,-9.42915357596829,-332.478395817969)) ;
#44948 = CARTESIAN_POINT('Ctrl Pts',(15.9292119177615,-9.53785582092768,-332.480015573261)) ;
#44949 = CARTESIAN_POINT('Ctrl Pts',(15.7932306403496,-9.76148909423286,-332.483385838611)) ;
#44950 = CARTESIAN_POINT('Ctrl Pts',(15.7216785042645,-9.87631653698226,-332.485137465665)) ;
#44951 = CARTESIAN_POINT('Ctrl Pts',(15.5250964041906,-10.1842425639224,-332.489892491676)) ;
#44952 = CARTESIAN_POINT('Ctrl Pts',(15.3977224475582,-10.3758160200987,-332.492913292005)) ;
#44953 = CARTESIAN_POINT('Ctrl Pts',(15.1753762556539,-10.6971154466316,-332.498083256662)) ;
#44954 = CARTESIAN_POINT('Ctrl Pts',(15.0822189537513,-10.8280651423035,-332.500220409201)) ;
#44955 = CARTESIAN_POINT('Ctrl Pts',(14.6384377756168,-11.4350410914577,-332.51025984871)) ;
#44956 = CARTESIAN_POINT('Ctrl Pts',(14.2669060409798,-11.8953526650251,-332.518274623767)) ;
#44957 = CARTESIAN_POINT('Ctrl Pts',(13.7307723517689,-12.4982750308487,-332.529079789098)) ;
#44958 = CARTESIAN_POINT('Ctrl Pts',(13.584700872033,-12.6568910316472,-332.531952136263)) ;
#44959 = CARTESIAN_POINT('Ctrl Pts',(13.35203643845,-12.9008677614489,-332.536395435434)) ;
#44960 = CARTESIAN_POINT('Ctrl Pts',(13.2673116211508,-12.9879832334004,-332.537987133545)) ;
#44961 = CARTESIAN_POINT('Ctrl Pts',(13.1370589384309,-13.1193066572941,-332.540390125203)) ;
#44962 = CARTESIAN_POINT('Ctrl Pts',(13.0921496439651,-13.164123306637,-332.541210833072)) ;
#44963 = CARTESIAN_POINT('Ctrl Pts',(13.01356401674,-13.2417469099432,-332.542632689696)) ;
#44964 = CARTESIAN_POINT('Ctrl Pts',(12.9799911976487,-13.2746577414469,-332.543235613906)) ;
#44965 = CARTESIAN_POINT('Ctrl Pts',(12.8997183716975,-13.3527520653254,-332.544666976938)) ;
#44966 = CARTESIAN_POINT('Ctrl Pts',(12.852905411894,-13.3978186385798,-332.545493540795)) ;
#44967 = CARTESIAN_POINT('Ctrl Pts',(12.8048044867707,-13.4436410086833,-332.54633508729)) ;
#44968 = CARTESIAN_POINT('Ctrl Pts',(12.8037520618402,-13.4446433442356,-332.546353496141)) ;
#44969 = CARTESIAN_POINT('Ctrl Pts',(12.8015299140816,-13.446759232976,-332.546392357637)) ;
#44970 = CARTESIAN_POINT('Ctrl Pts',(12.8003601636317,-13.4478727571338,-332.54641280988)) ;
#44971 = CARTESIAN_POINT('Ctrl Pts',(12.7978893088446,-13.4502242310845,-332.546456001175)) ;
#44972 = CARTESIAN_POINT('Ctrl Pts',(12.7965881701203,-13.4514621447718,-332.54647873973)) ;
#44973 = CARTESIAN_POINT('Ctrl Pts',(12.7938386573008,-13.4540772930743,-332.546526777789)) ;
#44974 = CARTESIAN_POINT('Ctrl Pts',(12.7923902403966,-13.4554544826427,-332.546552076675)) ;
#44975 = CARTESIAN_POINT('Ctrl Pts',(12.7893282179307,-13.4583649858114,-332.54660554475)) ;
#44976 = CARTESIAN_POINT('Ctrl Pts',(12.7877145589167,-13.4598982431868,-332.54663371317)) ;
#44977 = CARTESIAN_POINT('Ctrl Pts',(12.7843017506741,-13.463139838298,-332.546693269437)) ;
#44978 = CARTESIAN_POINT('Ctrl Pts',(12.7825025346857,-13.4648481056643,-332.546724656326)) ;
#44979 = CARTESIAN_POINT('Ctrl Pts',(12.7786956554764,-13.468461100137,-332.546791043452)) ;
#44980 = CARTESIAN_POINT('Ctrl Pts',(12.7766879086751,-13.4703657391146,-332.546826042496)) ;
#44981 = CARTESIAN_POINT('Ctrl Pts',(12.7724380161347,-13.4743955734633,-332.546900098139)) ;
#44982 = CARTESIAN_POINT('Ctrl Pts',(12.7701957656623,-13.476520658272,-332.546939153251)) ;
#44983 = CARTESIAN_POINT('Ctrl Pts',(12.7654475493937,-13.4810185140472,-332.547021821446)) ;
#44984 = CARTESIAN_POINT('Ctrl Pts',(12.7629414521835,-13.4833911461674,-332.547065432674)) ;
#44985 = CARTESIAN_POINT('Ctrl Pts',(12.75763246256,-13.4884145931151,-332.547157776002)) ;
#44986 = CARTESIAN_POINT('Ctrl Pts',(12.754829405148,-13.491065233372,-332.547206505789)) ;
#44987 = CARTESIAN_POINT('Ctrl Pts',(12.7488892289613,-13.4966789045023,-332.54730971815)) ;
#44988 = CARTESIAN_POINT('Ctrl Pts',(12.7457519028935,-13.4996417157439,-332.547364197842)) ;
#44989 = CARTESIAN_POINT('Ctrl Pts',(12.7391012973305,-13.5059179940145,-332.547479617562)) ;
#44990 = CARTESIAN_POINT('Ctrl Pts',(12.7355877573517,-13.5092311846192,-332.547540554)) ;
#44991 = CARTESIAN_POINT('Ctrl Pts',(12.7281377605599,-13.5162508775382,-332.547669676858)) ;
#44992 = CARTESIAN_POINT('Ctrl Pts',(12.7242009764884,-13.5199570319687,-332.547737858814)) ;
#44993 = CARTESIAN_POINT('Ctrl Pts',(12.7158520214465,-13.5278100014189,-332.547882350458)) ;
#44994 = CARTESIAN_POINT('Ctrl Pts',(12.7114394396194,-13.5319563788357,-332.547958654604)) ;
#44995 = CARTESIAN_POINT('Ctrl Pts',(12.7050382142322,-13.5379655340834,-332.548069257284)) ;
#44996 = CARTESIAN_POINT('Ctrl Pts',(12.7030511879628,-13.5398300337608,-332.548103577291)) ;
#44997 = CARTESIAN_POINT('Ctrl Pts',(12.6983451597256,-13.5442439249794,-332.548184830406)) ;
#44998 = CARTESIAN_POINT('Ctrl Pts',(12.6956258004738,-13.5467929352011,-332.548231758789)) ;
#44999 = CARTESIAN_POINT('Ctrl Pts',(12.6891931047241,-13.5528190289879,-332.548342713677)) ;
#45000 = CARTESIAN_POINT('Ctrl Pts',(12.6854791063044,-13.5562954056407,-332.548406731505)) ;
#45001 = CARTESIAN_POINT('Ctrl Pts',(12.676709544919,-13.5644971305199,-332.548557789804)) ;
#45002 = CARTESIAN_POINT('Ctrl Pts',(12.6716527677834,-13.5692211796721,-332.548644814534)) ;
#45003 = CARTESIAN_POINT('Ctrl Pts',(12.6597452500862,-13.5803327403396,-332.548849551092)) ;
#45004 = CARTESIAN_POINT('Ctrl Pts',(12.6528923143566,-13.5867178971502,-332.548967234885)) ;
#45005 = CARTESIAN_POINT('Ctrl Pts',(12.6368208738301,-13.6016696023582,-332.549242890204)) ;
#45006 = CARTESIAN_POINT('Ctrl Pts',(12.6275984849127,-13.6102319698409,-332.549400813138)) ;
#45007 = CARTESIAN_POINT('Ctrl Pts',(12.4983428206846,-13.7299926874607,-332.551610607558)) ;
#45008 = CARTESIAN_POINT('Ctrl Pts',(12.3768532024904,-13.8396090040588,-332.55364472926)) ;
#45009 = CARTESIAN_POINT('Ctrl Pts',(11.904103637039,-14.2549520122255,-332.561426604256)) ;
#45010 = CARTESIAN_POINT('Ctrl Pts',(11.5428373024626,-14.5490291213305,-332.567099681078)) ;
#45011 = CARTESIAN_POINT('Ctrl Pts',(10.7989595345716,-15.1093948371796,-332.578532570543)) ;
#45012 = CARTESIAN_POINT('Ctrl Pts',(10.4166128295706,-15.3754842252688,-332.584288652172)) ;
#45013 = CARTESIAN_POINT('Ctrl Pts',(9.8871001486967,-15.7151666607572,-332.592213475305)) ;
#45014 = CARTESIAN_POINT('Ctrl Pts',(9.74837264789605,-15.8015962210896,-332.594284999122)) ;
#45015 = CARTESIAN_POINT('Ctrl Pts',(9.51904113291167,-15.9403039899409,-332.597704701943)) ;
#45016 = CARTESIAN_POINT('Ctrl Pts',(9.4291044502902,-15.9936682664424,-332.599044607796)) ;
#45017 = CARTESIAN_POINT('Ctrl Pts',(9.22697557530512,-16.1113046610739,-332.602053913314)) ;
#45018 = CARTESIAN_POINT('Ctrl Pts',(9.11455317023766,-16.1751703730894,-332.603726262867)) ;
#45019 = CARTESIAN_POINT('Ctrl Pts',(8.88289600347169,-16.3035897687109,-332.607169767099)) ;
#45020 = CARTESIAN_POINT('Ctrl Pts',(8.76360270731259,-16.3680221248359,-332.608941672812)) ;
#45021 = CARTESIAN_POINT('Ctrl Pts',(8.14939385975142,-16.6911271470905,-332.618056551196)) ;
#45022 = CARTESIAN_POINT('Ctrl Pts',(7.64369650447566,-16.9286811569303,-332.625544074346)) ;
#45023 = CARTESIAN_POINT('Ctrl Pts',(6.63009557290528,-17.3501347971755,-332.64032768909)) ;
#45024 = CARTESIAN_POINT('Ctrl Pts',(6.12334035574825,-17.5353941693649,-332.647613201731)) ;
#45025 = CARTESIAN_POINT('Ctrl Pts',(5.50403285938207,-17.7316751127372,-332.656157204252)) ;
#45026 = CARTESIAN_POINT('Ctrl Pts',(5.39852924709108,-17.7640806698403,-332.657600083318)) ;
#45027 = CARTESIAN_POINT('Ctrl Pts',(5.23373904423387,-17.8130925005906,-332.659830742326)) ;
#45028 = CARTESIAN_POINT('Ctrl Pts',(5.17464822546492,-17.8303478536104,-332.66062602472)) ;
#45029 = CARTESIAN_POINT('Ctrl Pts',(5.05733082060934,-17.8639738736241,-332.662195094564)) ;
#45030 = CARTESIAN_POINT('Ctrl Pts',(4.99910790565926,-17.8803545195542,-332.66296904373)) ;
#45031 = CARTESIAN_POINT('Ctrl Pts',(4.86967388166753,-17.9160883316886,-332.664680029477)) ;
#45032 = CARTESIAN_POINT('Ctrl Pts',(4.79842530900951,-17.9353020435515,-332.665615460567)) ;
#45033 = CARTESIAN_POINT('Ctrl Pts',(4.45985225517868,-18.024443652093,-332.670033992866)) ;
#45034 = CARTESIAN_POINT('Ctrl Pts',(4.191102559177,-18.0888228212409,-332.673463197062)) ;
#45035 = CARTESIAN_POINT('Ctrl Pts',(3.31931893444489,-18.2771869378127,-332.684455730257)) ;
#45036 = CARTESIAN_POINT('Ctrl Pts',(2.71152845299985,-18.3771884593749,-332.69193046579)) ;
#45037 = CARTESIAN_POINT('Ctrl Pts',(1.79635042048582,-18.4813678616395,-332.703336185325)) ;
#45038 = CARTESIAN_POINT('Ctrl Pts',(1.49199948812602,-18.5084242934456,-332.707151221583)) ;
#45039 = CARTESIAN_POINT('Ctrl Pts',(1.04052901559977,-18.5373508354029,-332.712870389489)) ;
#45040 = CARTESIAN_POINT('Ctrl Pts',(0.893831572952765,-18.5450031454643,
-332.714737914278)) ;
#45041 = CARTESIAN_POINT('Ctrl Pts',(0.633226507880376,-18.5554979029746,
-332.718073822772)) ;
#45042 = CARTESIAN_POINT('Ctrl Pts',(0.519354396397132,-18.559034166926,-332.719537637324)) ;
#45043 = CARTESIAN_POINT('Ctrl Pts',(0.270264067520439,-18.5644752847932,
-332.722753767207)) ;
#45044 = CARTESIAN_POINT('Ctrl Pts',(0.135042993128688,-18.5659513246769,
-332.724508765686)) ;
#45045 = CARTESIAN_POINT('Ctrl Pts',(-0.000181996293217197,-18.565949999108,
-332.726272944078)) ;
#45046 = CARTESIAN_POINT('Ctrl Pts',(-0.000181996293162345,-18.565949999108,
-332.726272944078)) ;
#45047 = CARTESIAN_POINT('Ctrl Pts',(-0.176929924793901,-18.5659482665024,
-332.728578840921)) ;
#45048 = CARTESIAN_POINT('Ctrl Pts',(-0.353668593251895,-18.5634225729408,
-332.730900257364)) ;
#45049 = CARTESIAN_POINT('Ctrl Pts',(-1.23228127524413,-18.5383143938595,
-332.742513137644)) ;
#45050 = CARTESIAN_POINT('Ctrl Pts',(-1.93251401323006,-18.4784469184749,
-332.752022876382)) ;
#45051 = CARTESIAN_POINT('Ctrl Pts',(-2.85588299120307,-18.3464323542094,
-332.764551949736)) ;
#45052 = CARTESIAN_POINT('Ctrl Pts',(-3.08347441316332,-18.3095557992409,
-332.76763672847)) ;
#45053 = CARTESIAN_POINT('Ctrl Pts',(-3.42092087897222,-18.2484090793984,
-332.772181144825)) ;
#45054 = CARTESIAN_POINT('Ctrl Pts',(-3.53133749106253,-18.2273637469237,
-332.773663379807)) ;
#45055 = CARTESIAN_POINT('Ctrl Pts',(-3.71324816206135,-18.1909766879873,
-332.776093915746)) ;
#45056 = CARTESIAN_POINT('Ctrl Pts',(-3.78485478925804,-18.1762129998792,
-332.777047722042)) ;
#45057 = CARTESIAN_POINT('Ctrl Pts',(-3.91543010248418,-18.1484862066509,
-332.778780460323)) ;
#45058 = CARTESIAN_POINT('Ctrl Pts',(-3.97442633978652,-18.1356576875728,
-332.779560897449)) ;
#45059 = CARTESIAN_POINT('Ctrl Pts',(-4.09381883038044,-18.1090856544887,
-332.781134577953)) ;
#45060 = CARTESIAN_POINT('Ctrl Pts',(-4.15421098431024,-18.0953272134762,
-332.781927600122)) ;
#45061 = CARTESIAN_POINT('Ctrl Pts',(-4.3243022977065,-18.0556809048547,-332.784154003867)) ;
#45062 = CARTESIAN_POINT('Ctrl Pts',(-4.43383628045254,-18.0290959062432,
-332.78557940658)) ;
#45063 = CARTESIAN_POINT('Ctrl Pts',(-5.03576689168719,-17.8771840324648,
-332.793381650613)) ;
#45064 = CARTESIAN_POINT('Ctrl Pts',(-5.52310234356574,-17.7326817118893,
-332.799590249782)) ;
#45065 = CARTESIAN_POINT('Ctrl Pts',(-6.55537570103544,-17.379907846883,-332.812951873021)) ;
#45066 = CARTESIAN_POINT('Ctrl Pts',(-7.0976741910527,-17.1655808796899,-332.820105890676)) ;
#45067 = CARTESIAN_POINT('Ctrl Pts',(-7.75311857595609,-16.8701567734299,
-332.829146257708)) ;
#45068 = CARTESIAN_POINT('Ctrl Pts',(-7.87662706486075,-16.8128457803031,
-332.830866921865)) ;
#45069 = CARTESIAN_POINT('Ctrl Pts',(-8.1100755980492,-16.7013828533122,-332.834154145294)) ;
#45070 = CARTESIAN_POINT('Ctrl Pts',(-8.22013179967204,-16.6474907588765,
-332.835718824259)) ;
#45071 = CARTESIAN_POINT('Ctrl Pts',(-8.44020691714935,-16.537010334569,-332.838878912442)) ;
#45072 = CARTESIAN_POINT('Ctrl Pts',(-8.55020991456653,-16.4804039385023,
-332.840474393702)) ;
#45073 = CARTESIAN_POINT('Ctrl Pts',(-8.81054845943651,-16.3431282502931,
-332.844288980448)) ;
#45074 = CARTESIAN_POINT('Ctrl Pts',(-8.96035389264517,-16.2614778895082,
-332.84651508752)) ;
#45075 = CARTESIAN_POINT('Ctrl Pts',(-9.79018821526244,-15.7942336964093,
-332.859019194102)) ;
#45076 = CARTESIAN_POINT('Ctrl Pts',(-10.4464584434506,-15.3680544684858,
-332.869601025997)) ;
#45077 = CARTESIAN_POINT('Ctrl Pts',(-11.2642053296691,-14.7603655938016,
-332.883290971973)) ;
#45078 = CARTESIAN_POINT('Ctrl Pts',(-11.4517824153023,-14.6153136788311,
-332.886465129517)) ;
#45079 = CARTESIAN_POINT('Ctrl Pts',(-11.7255762648179,-14.3950831937948,
-332.891123080878)) ;
#45080 = CARTESIAN_POINT('Ctrl Pts',(-11.8139594273255,-14.3226366846006,
-332.892630609544)) ;
#45081 = CARTESIAN_POINT('Ctrl Pts',(-11.9583122307089,-14.2020672763326,
-332.8950955234)) ;
#45082 = CARTESIAN_POINT('Ctrl Pts',(-12.0146737414955,-14.1544184349344,
-332.896058623406)) ;
#45083 = CARTESIAN_POINT('Ctrl Pts',(-12.1067113572339,-14.0756626728235,
-332.897631423471)) ;
#45084 = CARTESIAN_POINT('Ctrl Pts',(-12.1425552574274,-14.044753162371,-332.898243964958)) ;
#45085 = CARTESIAN_POINT('Ctrl Pts',(-12.2288590228466,-13.9697529159751,
-332.89971843141)) ;
#45086 = CARTESIAN_POINT('Ctrl Pts',(-12.2791990428529,-13.9255254978142,
-332.900577988846)) ;
#45087 = CARTESIAN_POINT('Ctrl Pts',(-12.3931207798733,-13.8243388091023,
-332.90252310191)) ;
#45088 = CARTESIAN_POINT('Ctrl Pts',(-12.4565513528077,-13.7672115766006,
-332.90360613236)) ;
#45089 = CARTESIAN_POINT('Ctrl Pts',(-12.730181348142,-13.5173339745886,-332.908283453334)) ;
#45090 = CARTESIAN_POINT('Ctrl Pts',(-12.9363182381565,-13.3201916672341,
-332.911821302352)) ;
#45091 = CARTESIAN_POINT('Ctrl Pts',(-13.5470356076894,-12.7085686694285,
-332.922469851462)) ;
#45092 = CARTESIAN_POINT('Ctrl Pts',(-13.9368401105088,-12.2798363346107,
-332.92950785098)) ;
#45093 = CARTESIAN_POINT('Ctrl Pts',(-14.4074314911705,-11.7109247399394,
-332.938636336359)) ;
#45094 = CARTESIAN_POINT('Ctrl Pts',(-14.5073134754075,-11.5869623323296,
-332.940612580873)) ;
#45095 = CARTESIAN_POINT('Ctrl Pts',(-14.7467130345622,-11.281897454798,-332.945452887256)) ;
#45096 = CARTESIAN_POINT('Ctrl Pts',(-14.8845036534993,-11.0994732406175,
-332.948328095774)) ;
#45097 = CARTESIAN_POINT('Ctrl Pts',(-15.0982780968702,-10.8053104507544,
-332.952944404618)) ;
#45098 = CARTESIAN_POINT('Ctrl Pts',(-15.1764716033163,-10.6952066383531,
-332.954667866966)) ;
#45099 = CARTESIAN_POINT('Ctrl Pts',(-15.325601580407,-10.4802886616336,-332.958024926894)) ;
#45100 = CARTESIAN_POINT('Ctrl Pts',(-15.3966812991223,-10.3755828343112,
-332.95965726923)) ;
#45101 = CARTESIAN_POINT('Ctrl Pts',(-15.549816115602,-10.1449643941507,-332.963246173694)) ;
#45102 = CARTESIAN_POINT('Ctrl Pts',(-15.6314241046803,-10.0187656005502,
-332.965206015731)) ;
#45103 = CARTESIAN_POINT('Ctrl Pts',(-15.9520549379486,-9.50948566049929,
-332.973097945853)) ;
#45104 = CARTESIAN_POINT('Ctrl Pts',(-16.1785990612862,-9.11873371953784,
-332.979118948172)) ;
#45105 = CARTESIAN_POINT('Ctrl Pts',(-16.6142149381398,-8.29993282078138,
-332.991579490287)) ;
#45106 = CARTESIAN_POINT('Ctrl Pts',(-16.8215181447942,-7.87131182849796,
-332.998019712317)) ;
#45107 = CARTESIAN_POINT('Ctrl Pts',(-17.0783009664027,-7.28377947165542,
-333.006585977831)) ;
#45108 = CARTESIAN_POINT('Ctrl Pts',(-17.1424553603454,-7.13148172756422,
-333.008782922735)) ;
#45109 = CARTESIAN_POINT('Ctrl Pts',(-17.2513534187016,-6.86300212038146,
-333.012603428887)) ;
#45110 = CARTESIAN_POINT('Ctrl Pts',(-17.296977672553,-6.74718877406822,-333.014234588078)) ;
#45111 = CARTESIAN_POINT('Ctrl Pts',(-17.3667602501668,-6.56469087141144,
-333.016773751578)) ;
#45112 = CARTESIAN_POINT('Ctrl Pts',(-17.3917069630018,-6.4983118390143,-333.017690876499)) ;
#45113 = CARTESIAN_POINT('Ctrl Pts',(-17.4378935300134,-6.37324592913827,
-333.019405647015)) ;
#45114 = CARTESIAN_POINT('Ctrl Pts',(-17.4592189398208,-6.31459170973239,
-333.02020443272)) ;
#45115 = CARTESIAN_POINT('Ctrl Pts',(-17.5191764854918,-6.14705636966585,
-333.022471991032)) ;
#45116 = CARTESIAN_POINT('Ctrl Pts',(-17.557088652206,-6.03792057438868,-333.023932300637)) ;
#45117 = CARTESIAN_POINT('Ctrl Pts',(-17.7367135743688,-5.50484301195917,
-333.030997981614)) ;
#45118 = CARTESIAN_POINT('Ctrl Pts',(-17.8641034620573,-5.0762303525688,-333.036476400351)) ;
#45119 = CARTESIAN_POINT('Ctrl Pts',(-17.979978128308,-4.62765078362187,-333.042151636226)) ;
#45120 = CARTESIAN_POINT('Ctrl Pts',(-17.9840353998729,-4.61185819444987,
-333.042351358)) ;
#45121 = CARTESIAN_POINT('Ctrl Pts',(-18.0936516372944,-4.18284189887237,
-333.047774940359)) ;
#45122 = CARTESIAN_POINT('Ctrl Pts',(-18.1849614602823,-3.76610836205566,
-333.052996460066)) ;
#45123 = CARTESIAN_POINT('Ctrl Pts',(-18.3130614144305,-3.06708856862826,
-333.061816050813)) ;
#45124 = CARTESIAN_POINT('Ctrl Pts',(-18.3578598786626,-2.7864369451825,-333.065372402138)) ;
#45125 = CARTESIAN_POINT('Ctrl Pts',(-18.415659413607,-2.36194687002244,-333.070795778185)) ;
#45126 = CARTESIAN_POINT('Ctrl Pts',(-18.4334536911952,-2.21880363980699,
-333.072632023555)) ;
#45127 = CARTESIAN_POINT('Ctrl Pts',(-18.4634698061982,-1.95197961470612,
-333.076070496639)) ;
#45128 = CARTESIAN_POINT('Ctrl Pts',(-18.476121313219,-1.82835523589385,-333.077669824517)) ;
#45129 = CARTESIAN_POINT('Ctrl Pts',(-18.502147401213,-1.54608704770923,-333.08133637996)) ;
#45130 = CARTESIAN_POINT('Ctrl Pts',(-18.5147244500455,-1.3873795616715,-333.083408633878)) ;
#45131 = CARTESIAN_POINT('Ctrl Pts',(-18.5498716322094,-0.857387975054706,
-333.090363986786)) ;
#45132 = CARTESIAN_POINT('Ctrl Pts',(-18.5633254564996,-0.485590909472479,
-333.095302554508)) ;
#45133 = CARTESIAN_POINT('Ctrl Pts',(-18.5689934955609,0.440391615893321,
-333.107700349429)) ;
#45134 = CARTESIAN_POINT('Ctrl Pts',(-18.5475829596294,0.994298371991139,
-333.115208955269)) ;
#45135 = CARTESIAN_POINT('Ctrl Pts',(-18.4908309556074,1.67328353686872,-333.124322660921)) ;
#45136 = CARTESIAN_POINT('Ctrl Pts',(-18.4789222552042,1.80003876600416,-333.126019659971)) ;
#45137 = CARTESIAN_POINT('Ctrl Pts',(-18.4490094526925,2.08673217205175,-333.129841518427)) ;
#45138 = CARTESIAN_POINT('Ctrl Pts',(-18.4302274354707,2.24657912593199,-333.131960848237)) ;
#45139 = CARTESIAN_POINT('Ctrl Pts',(-18.3993055249026,2.48316042006527,-333.135070844765)) ;
#45140 = CARTESIAN_POINT('Ctrl Pts',(-18.3887585787039,2.56009519873291,-333.136077983377)) ;
#45141 = CARTESIAN_POINT('Ctrl Pts',(-18.3682984900442,2.70268732811283,-333.137935355076)) ;
#45142 = CARTESIAN_POINT('Ctrl Pts',(-18.3585152092227,2.76836188310839,-333.13878700645)) ;
#45143 = CARTESIAN_POINT('Ctrl Pts',(-18.3353135440008,2.9185790970442,-333.140727267773)) ;
#45144 = CARTESIAN_POINT('Ctrl Pts',(-18.3216623492075,3.00308432966621,-333.141813237655)) ;
#45145 = CARTESIAN_POINT('Ctrl Pts',(-18.2587679154238,3.37601977232114,-333.146586721839)) ;
#45146 = CARTESIAN_POINT('Ctrl Pts',(-18.2032944417357,3.66335740573778,-333.150214663096)) ;
#45147 = CARTESIAN_POINT('Ctrl Pts',(-18.019125931765,4.50934051785376,-333.160877124651)) ;
#45148 = CARTESIAN_POINT('Ctrl Pts',(-17.8713268841018,5.0634699376241,-333.167844748277)) ;
#45149 = CARTESIAN_POINT('Ctrl Pts',(-17.6502601443748,5.76089538616308,-333.176891397168)) ;
#45150 = CARTESIAN_POINT('Ctrl Pts',(-17.6004586124387,5.91129895829353,-333.178858404637)) ;
#45151 = CARTESIAN_POINT('Ctrl Pts',(-17.4743482121151,6.27643035666174,-333.183680555006)) ;
#45152 = CARTESIAN_POINT('Ctrl Pts',(-17.3959993431832,6.49042602919687,-333.186546825843)) ;
#45153 = CARTESIAN_POINT('Ctrl Pts',(-17.2650232031959,6.82873889115415,-333.191152491203)) ;
#45154 = CARTESIAN_POINT('Ctrl Pts',(-17.2149450666118,6.95401807158209,-333.192874399146)) ;
#45155 = CARTESIAN_POINT('Ctrl Pts',(-17.1152335539942,7.19578413442279,-333.196230689402)) ;
#45156 = CARTESIAN_POINT('Ctrl Pts',(-17.0657652073416,7.3123311433941,-333.197863842168)) ;
#45157 = CARTESIAN_POINT('Ctrl Pts',(-16.9548674376392,7.56634910408699,-333.201457295405)) ;
#45158 = CARTESIAN_POINT('Ctrl Pts',(-16.8929499640735,7.70359721267887,-333.203420911174)) ;
#45159 = CARTESIAN_POINT('Ctrl Pts',(-16.6372681660222,8.2524392288631,-333.211361418898)) ;
#45160 = CARTESIAN_POINT('Ctrl Pts',(-16.4300759095894,8.65760063636187,-333.21742869212)) ;
#45161 = CARTESIAN_POINT('Ctrl Pts',(-15.9776498207253,9.46745464102918,-333.229893271224)) ;
#45162 = CARTESIAN_POINT('Ctrl Pts',(-15.7314075543493,9.87121103609941,-333.236289759675)) ;
#45163 = CARTESIAN_POINT('Ctrl Pts',(-15.378933915341,10.4024051829712,-333.244806148928)) ;
#45164 = CARTESIAN_POINT('Ctrl Pts',(-15.2860201891735,10.5384642552784,-333.246996299036)) ;
#45165 = CARTESIAN_POINT('Ctrl Pts',(-15.1199049341371,10.7748967892186,-333.250806473477)) ;
#45166 = CARTESIAN_POINT('Ctrl Pts',(-15.0474839179221,10.8758058943466,-333.2524340421)) ;
#45167 = CARTESIAN_POINT('Ctrl Pts',(-14.932164897378,11.0331306448998,-333.254968956818)) ;
#45168 = CARTESIAN_POINT('Ctrl Pts',(-14.8899471862556,11.0900402686853,-333.255885375728)) ;
#45169 = CARTESIAN_POINT('Ctrl Pts',(-14.8099120409585,11.1966470185692,-333.257599909561)) ;
#45170 = CARTESIAN_POINT('Ctrl Pts',(-14.7721676515203,11.2463977346799,-333.258399154765)) ;
#45171 = CARTESIAN_POINT('Ctrl Pts',(-14.6637467701677,11.3878193072035,-333.260669949941)) ;
#45172 = CARTESIAN_POINT('Ctrl Pts',(-14.5924629520732,11.4790209934549,-333.262132998586)) ;
#45173 = CARTESIAN_POINT('Ctrl Pts',(-14.3783186347003,11.7477822063117,-333.266449164744)) ;
#45174 = CARTESIAN_POINT('Ctrl Pts',(-14.2330366047752,11.9233847062325,-333.269275648092)) ;
#45175 = CARTESIAN_POINT('Ctrl Pts',(-13.7002330261233,12.5437663859952,-333.279358226079)) ;
#45176 = CARTESIAN_POINT('Ctrl Pts',(-13.294798738075,12.9726939444986,-333.286523635674)) ;
#45177 = CARTESIAN_POINT('Ctrl Pts',(-12.753927095584,13.4928727350859,-333.295799978066)) ;
#45178 = CARTESIAN_POINT('Ctrl Pts',(-12.6367812814632,13.6026478957221,-333.297792572643)) ;
#45179 = CARTESIAN_POINT('Ctrl Pts',(-12.3484618773211,13.865887384913,-333.302664959189)) ;
#45180 = CARTESIAN_POINT('Ctrl Pts',(-12.1758333134102,14.0177183076487,-333.305555929677)) ;
#45181 = CARTESIAN_POINT('Ctrl Pts',(-11.8972193203939,14.2537352478201,-333.310191008007)) ;
#45182 = CARTESIAN_POINT('Ctrl Pts',(-11.7930561523791,14.3400356552821,-333.311917209591)) ;
#45183 = CARTESIAN_POINT('Ctrl Pts',(-11.5897113876162,14.5047950338148,-333.315275659948)) ;
#45184 = CARTESIAN_POINT('Ctrl Pts',(-11.4906528442039,14.583394192752,-333.316906608506)) ;
#45185 = CARTESIAN_POINT('Ctrl Pts',(-11.2502951582311,14.7701393510807,-333.320852365073)) ;
#45186 = CARTESIAN_POINT('Ctrl Pts',(-11.1082293152159,14.8772779409375,-333.323175125279)) ;
#45187 = CARTESIAN_POINT('Ctrl Pts',(-10.42546366122,15.3769511933369,-333.334291737183)) ;
#45188 = CARTESIAN_POINT('Ctrl Pts',(-9.86537549259348,15.7421498024099,-333.343294375837)) ;
#45189 = CARTESIAN_POINT('Ctrl Pts',(-9.02511469636042,16.2275430629978,-333.356361744373)) ;
#45190 = CARTESIAN_POINT('Ctrl Pts',(-8.75974936913429,16.3723132289215,-333.360425239304)) ;
#45191 = CARTESIAN_POINT('Ctrl Pts',(-8.32564814620522,16.5955608989263,-333.366916336885)) ;
#45192 = CARTESIAN_POINT('Ctrl Pts',(-8.15906000204271,16.6780933772944,-333.369370995283)) ;
#45193 = CARTESIAN_POINT('Ctrl Pts',(-7.91755207820026,16.7932586717237,-333.372863653351)) ;
#45194 = CARTESIAN_POINT('Ctrl Pts',(-7.84361264475933,16.8279205022621,-333.373924163669)) ;
#45195 = CARTESIAN_POINT('Ctrl Pts',(-7.70932501505491,16.8897954177682,-333.375832735668)) ;
#45196 = CARTESIAN_POINT('Ctrl Pts',(-7.649055555295,16.9171756079629,-333.376682821338)) ;
#45197 = CARTESIAN_POINT('Ctrl Pts',(-7.50097916736094,16.9834930700749,-333.378756219468)) ;
#45198 = CARTESIAN_POINT('Ctrl Pts',(-7.41301404435475,17.0220723810835,-333.379975098996)) ;
#45199 = CARTESIAN_POINT('Ctrl Pts',(-7.04182369300143,17.1814441864609,-333.385071949227)) ;
#45200 = CARTESIAN_POINT('Ctrl Pts',(-6.75591510037491,17.2958641657077,-333.388885258305)) ;
#45201 = CARTESIAN_POINT('Ctrl Pts',(-6.35051256678759,17.4465185807303,-333.39420697231)) ;
#45202 = CARTESIAN_POINT('Ctrl Pts',(-6.23329813465139,17.4887396581955,-333.395735679651)) ;
#45203 = CARTESIAN_POINT('Ctrl Pts',(-5.66970197980063,17.685363186401,-333.403052330168)) ;
#45204 = CARTESIAN_POINT('Ctrl Pts',(-5.21796143599458,17.8238735920603,-333.408820737122)) ;
#45205 = CARTESIAN_POINT('Ctrl Pts',(-4.62272552435464,17.9818103159411,-333.416452869909)) ;
#45206 = CARTESIAN_POINT('Ctrl Pts',(-4.48359671517524,18.0170045776417,-333.41823855001)) ;
#45207 = CARTESIAN_POINT('Ctrl Pts',(-4.13678870436674,18.1004677943033,-333.422699542089)) ;
#45208 = CARTESIAN_POINT('Ctrl Pts',(-3.92865980879362,18.146778971393,-333.42538551301)) ;
#45209 = CARTESIAN_POINT('Ctrl Pts',(-3.59012837434456,18.2160091717535,-333.429776528879)) ;
#45210 = CARTESIAN_POINT('Ctrl Pts',(-3.46019727490057,18.2411361117591,-333.431467031026)) ;
#45211 = CARTESIAN_POINT('Ctrl Pts',(-3.20548983433008,18.2875737776433,-333.43479236479)) ;
#45212 = CARTESIAN_POINT('Ctrl Pts',(-3.08074211150248,18.3090018225732,-333.43642632485)) ;
#45213 = CARTESIAN_POINT('Ctrl Pts',(-2.80152664549176,18.354028504838,-333.440095851601)) ;
#45214 = CARTESIAN_POINT('Ctrl Pts',(-2.64696042991937,18.3769560669108,-333.442135621647)) ;
#45215 = CARTESIAN_POINT('Ctrl Pts',(-1.79334964999277,18.4925833918664,-333.45344505984)) ;
#45216 = CARTESIAN_POINT('Ctrl Pts',(-1.08975279150549,18.547349525349,-333.462956628382)) ;
#45217 = CARTESIAN_POINT('Ctrl Pts',(-0.0996556950809554,18.5678723710647,
-333.476287607101)) ;
#45218 = CARTESIAN_POINT('Ctrl Pts',(0.18554171743911,18.5672127750281,-333.480117712307)) ;
#45219 = CARTESIAN_POINT('Ctrl Pts',(0.649956807699827,18.5554369731698,-333.486290900692)) ;
#45220 = CARTESIAN_POINT('Ctrl Pts',(0.829227908166867,18.5482901203723,-333.488658187769)) ;
#45221 = CARTESIAN_POINT('Ctrl Pts',(1.08891360215054,18.5341650324675,-333.492051879007)) ;
#45222 = CARTESIAN_POINT('Ctrl Pts',(1.16943045096206,18.5292589902646,-333.493099143531)) ;
#45223 = CARTESIAN_POINT('Ctrl Pts',(1.31613560772452,18.5193599211075,-333.494996655237)) ;
#45224 = CARTESIAN_POINT('Ctrl Pts',(1.38233380571354,18.5145363989898,-333.495848754326)) ;
#45225 = CARTESIAN_POINT('Ctrl Pts',(1.54589729654637,18.5017362520058,-333.497944758691)) ;
#45226 = CARTESIAN_POINT('Ctrl Pts',(1.64322822103561,18.4933459342484,-333.499183966519)) ;
#45227 = CARTESIAN_POINT('Ctrl Pts',(2.06733839139269,18.4534113225673,-333.504556464405)) ;
#45228 = CARTESIAN_POINT('Ctrl Pts',(2.39331533652417,18.4139707869471,-333.508616222852)) ;
#45229 = CARTESIAN_POINT('Ctrl Pts',(2.77327452358049,18.3577384641806,-333.513337736712)) ;
#45230 = CARTESIAN_POINT('Ctrl Pts',(2.82843672518767,18.3493203905691,-333.514022911433)) ;
#45231 = CARTESIAN_POINT('Ctrl Pts',(2.89902717831782,18.3382219957264,-333.514899683102)) ;
#45232 = CARTESIAN_POINT('Ctrl Pts',(2.91449113222997,18.3357706678868,-333.515091751334)) ;
#45233 = CARTESIAN_POINT('Ctrl Pts',(3.41593761832023,18.2556315693196,-333.521320011182)) ;
#45234 = CARTESIAN_POINT('Ctrl Pts',(3.89864304961073,18.1586699990293,-333.527324615667)) ;
#45235 = CARTESIAN_POINT('Ctrl Pts',(4.58633430475311,17.991844554022,-333.536089917377)) ;
#45236 = CARTESIAN_POINT('Ctrl Pts',(4.79484418843973,17.937402315364,-333.538775009016)) ;
#45237 = CARTESIAN_POINT('Ctrl Pts',(5.17809607999879,17.8301744667059,-333.543774234244)) ;
#45238 = CARTESIAN_POINT('Ctrl Pts',(5.35309862543383,17.7784176878733,-333.546081889967)) ;
#45239 = CARTESIAN_POINT('Ctrl Pts',(5.64868210456148,17.686239109797,-333.550026540283)) ;
#45240 = CARTESIAN_POINT('Ctrl Pts',(5.76966260925521,17.6471430177341,-333.551654527742)) ;
#45241 = CARTESIAN_POINT('Ctrl Pts',(6.00180500329098,17.5694814350065,-333.554805330464)) ;
#45242 = CARTESIAN_POINT('Ctrl Pts',(6.11302070434476,17.5310957734354,-333.556326854624)) ;
#45243 = CARTESIAN_POINT('Ctrl Pts',(6.4157881906657,17.4233653402193,-333.560502253498)) ;
#45244 = CARTESIAN_POINT('Ctrl Pts',(6.60657519515343,17.3519209847571,-333.563170138087)) ;
#45245 = CARTESIAN_POINT('Ctrl Pts',(7.09273641182047,17.1606866200038,-333.570060297574)) ;
#45246 = CARTESIAN_POINT('Ctrl Pts',(7.38627148474827,17.0364041972363,-333.574309370653)) ;
#45247 = CARTESIAN_POINT('Ctrl Pts',(8.14620853083603,16.6913136563169,-333.585504218126)) ;
#45248 = CARTESIAN_POINT('Ctrl Pts',(8.60685984457301,16.4585123238381,-333.592491315004)) ;
#45249 = CARTESIAN_POINT('Ctrl Pts',(9.20665712865618,16.1233145266273,-333.601677003311)) ;
#45250 = CARTESIAN_POINT('Ctrl Pts',(9.35493598143648,16.0377361159052,-333.603954576904)) ;
#45251 = CARTESIAN_POINT('Ctrl Pts',(9.61166097353728,15.8847966016328,-333.607897292968)) ;
#45252 = CARTESIAN_POINT('Ctrl Pts',(9.72063542347296,15.8183449447465,-333.609570681551)) ;
#45253 = CARTESIAN_POINT('Ctrl Pts',(9.88960188788093,15.7129052302107,-333.612159816118)) ;
#45254 = CARTESIAN_POINT('Ctrl Pts',(9.9500683670251,15.6746851892984,-333.61308525093)) ;
#45255 = CARTESIAN_POINT('Ctrl Pts',(10.0625274449029,15.6026883796109,-333.614803184514)) ;
#45256 = CARTESIAN_POINT('Ctrl Pts',(10.114574648318,15.568998777777,-333.61559693542)) ;
#45257 = CARTESIAN_POINT('Ctrl Pts',(10.2610659579705,15.4731318847202,-333.617828606163)) ;
#45258 = CARTESIAN_POINT('Ctrl Pts',(10.3551122665437,15.4103515508876,-333.619258485455)) ;
#45259 = CARTESIAN_POINT('Ctrl Pts',(10.7253450185761,15.1582841852052,-333.624887190084)) ;
#45260 = CARTESIAN_POINT('Ctrl Pts',(10.9969634426094,14.9623995799628,-333.629016977603)) ;
#45261 = CARTESIAN_POINT('Ctrl Pts',(11.740756916482,14.3947940503471,-333.640503094221)) ;
#45262 = CARTESIAN_POINT('Ctrl Pts',(12.2004042197325,14.0073411442073,-333.647819213943)) ;
#45263 = CARTESIAN_POINT('Ctrl Pts',(12.8294321369826,13.4226205212189,-333.658504264199)) ;
#45264 = CARTESIAN_POINT('Ctrl Pts',(13.0147269504874,13.2430341176597,-333.661740457688)) ;
#45265 = CARTESIAN_POINT('Ctrl Pts',(13.2947435777149,12.9600891630984,-333.666785829568)) ;
#45266 = CARTESIAN_POINT('Ctrl Pts',(13.3921388852559,12.8594219900997,-333.668570806938)) ;
#45267 = CARTESIAN_POINT('Ctrl Pts',(13.5742329689178,12.6668980673108,-333.671967317222)) ;
#45268 = CARTESIAN_POINT('Ctrl Pts',(13.6591618763326,12.5752695448711,-333.673576657815)) ;
#45269 = CARTESIAN_POINT('Ctrl Pts',(13.8530178108667,12.3618402697478,-333.677309511865)) ;
#45270 = CARTESIAN_POINT('Ctrl Pts',(13.9612745899325,12.2394448008588,-333.679438650682)) ;
#45271 = CARTESIAN_POINT('Ctrl Pts',(14.3617278444615,11.7744641154123,-333.687483559095)) ;
#45272 = CARTESIAN_POINT('Ctrl Pts',(14.6430450139477,11.4227169523423,-333.693485899691)) ;
#45273 = CARTESIAN_POINT('Ctrl Pts',(15.1972894421022,10.6755482321547,-333.70598251633)) ;
#45274 = CARTESIAN_POINT('Ctrl Pts',(15.4682228352271,10.279057275902,-333.71247876251)) ;
#45275 = CARTESIAN_POINT('Ctrl Pts',(15.8505502133089,9.67014254485675,-333.722085091886)) ;
#45276 = CARTESIAN_POINT('Ctrl Pts',(15.9736968933091,9.4653371232579,-333.725255353887)) ;
#45277 = CARTESIAN_POINT('Ctrl Pts',(16.1370398842255,9.18141023135086,-333.729540547771)) ;
#45278 = CARTESIAN_POINT('Ctrl Pts',(16.180673367045,9.10429346415845,-333.730693512643)) ;
#45279 = CARTESIAN_POINT('Ctrl Pts',(16.2557201555781,8.96941382747543,-333.732689129548)) ;
#45280 = CARTESIAN_POINT('Ctrl Pts',(16.2873816434602,8.91179114438341,-333.733534959612)) ;
#45281 = CARTESIAN_POINT('Ctrl Pts',(16.3597272152027,8.77845161932615,-333.735476796217)) ;
#45282 = CARTESIAN_POINT('Ctrl Pts',(16.4001928227195,8.70261815746615,-333.736570010765)) ;
#45283 = CARTESIAN_POINT('Ctrl Pts',(16.5382760413192,8.43946340826532,-333.74032952922)) ;
#45284 = CARTESIAN_POINT('Ctrl Pts',(16.6332226873881,8.25075877571256,-333.742966198425)) ;
#45285 = CARTESIAN_POINT('Ctrl Pts',(16.7425142792203,8.02398627156324,-333.746085120462)) ;
#45286 = CARTESIAN_POINT('Ctrl Pts',(16.7599803184982,7.98744012816727,-333.746586233416)) ;
#45287 = CARTESIAN_POINT('Ctrl Pts',(17.0420250203897,7.3922881940109,-333.754723873783)) ;
#45288 = CARTESIAN_POINT('Ctrl Pts',(17.2786657371352,6.82086902301961,-333.762223247522)) ;
#45289 = CARTESIAN_POINT('Ctrl Pts',(17.5657830324307,6.01611366258911,-333.772780686972)) ;
#45290 = CARTESIAN_POINT('Ctrl Pts',(17.6409432985255,5.79201833904203,-333.775718272788)) ;
#45291 = CARTESIAN_POINT('Ctrl Pts',(17.7701980291416,5.38075198599374,-333.781123390985)) ;
#45292 = CARTESIAN_POINT('Ctrl Pts',(17.8256641395329,5.19404733675151,-333.783582278872)) ;
#45293 = CARTESIAN_POINT('Ctrl Pts',(17.9130052370937,4.88215308761592,-333.787704115441)) ;
#45294 = CARTESIAN_POINT('Ctrl Pts',(17.9465296318657,4.75744148791338,-333.789355941754)) ;
#45295 = CARTESIAN_POINT('Ctrl Pts',(18.0075871354738,4.52047147742886,-333.792502684003)) ;
#45296 = CARTESIAN_POINT('Ctrl Pts',(18.0353783713527,4.40828580979545,-333.793995787677)) ;
#45297 = CARTESIAN_POINT('Ctrl Pts',(18.1061322251825,4.11079749109798,-333.797964428802)) ;
#45298 = CARTESIAN_POINT('Ctrl Pts',(18.1472976861948,3.92508174182237,-333.800451563522)) ;
#45299 = CARTESIAN_POINT('Ctrl Pts',(18.2569187187187,3.39187795202367,-333.807617486295)) ;
#45300 = CARTESIAN_POINT('Ctrl Pts',(18.3182952743577,3.04302061328379,-333.812337517632)) ;
#45301 = CARTESIAN_POINT('Ctrl Pts',(18.3826886844754,2.60371476109412,-333.818294559685)) ;
#45302 = CARTESIAN_POINT('Ctrl Pts',(18.3950751401083,2.51471358404458,-333.819502000797)) ;
#45303 = CARTESIAN_POINT('Ctrl Pts',(18.4374616456409,2.19306442715255,-333.823865764763)) ;
#45304 = CARTESIAN_POINT('Ctrl Pts',(18.4636980920934,1.95994291975142,-333.827028918595)) ;
#45305 = CARTESIAN_POINT('Ctrl Pts',(18.5113566890086,1.44963241527223,-333.833926997681)) ;
#45306 = CARTESIAN_POINT('Ctrl Pts',(18.5309848337237,1.17233186742342,-333.837658748359)) ;
#45307 = CARTESIAN_POINT('Ctrl Pts',(18.5528889688586,0.718324094432647,-333.843696752568)) ;
#45308 = CARTESIAN_POINT('Ctrl Pts',(18.5588816463034,0.541840218410327,-333.846026036718)) ;
#45309 = CARTESIAN_POINT('Ctrl Pts',(18.5639343351448,0.285091147960057,-333.84937652137)) ;
#45310 = CARTESIAN_POINT('Ctrl Pts',(18.5649928927966,0.204875270651735,-333.850417881275)) ;
#45311 = CARTESIAN_POINT('Ctrl Pts',(18.5659777694683,0.0581923424251096,
-333.852310615797)) ;
#45312 = CARTESIAN_POINT('Ctrl Pts',(18.5660671239561,-0.00827208619058709,
-333.853163764812)) ;
#45313 = CARTESIAN_POINT('Ctrl Pts',(18.5654032119382,-0.173200850197427,
-333.855270567403)) ;
#45314 = CARTESIAN_POINT('Ctrl Pts',(18.5642235240493,-0.271661455251548,
-333.85651939813)) ;
#45315 = CARTESIAN_POINT('Ctrl Pts',(18.5588104403247,-0.543147194567071,
-333.859943352131)) ;
#45316 = CARTESIAN_POINT('Ctrl Pts',(18.5529409609457,-0.71612139748226,-333.862103148148)) ;
#45317 = CARTESIAN_POINT('Ctrl Pts',(18.5446545936004,-0.888979980963969,
-333.864249094225)) ;
#45318 = CARTESIAN_POINT('Origin',(0.,0.,-315.477129595899)) ;
#45319 = CARTESIAN_POINT('',(18.5446545937806,-0.888979977205187,-335.659885874007)) ;
#45320 = CARTESIAN_POINT('',(18.5446545935791,-0.888979981409804,-335.363183819487)) ;
#45321 = CARTESIAN_POINT('',(18.544654593745,-0.888979977948782,-315.477129595899)) ;
#45322 = CARTESIAN_POINT('Ctrl Pts',(18.5446545938163,-0.888979976461604,
-335.659885874007)) ;
#45323 = CARTESIAN_POINT('Ctrl Pts',(18.5558655382488,-0.65511296294481,-335.656771309662)) ;
#45324 = CARTESIAN_POINT('Ctrl Pts',(18.5626518543671,-0.421047992405619,
-335.653636281598)) ;
#45325 = CARTESIAN_POINT('Ctrl Pts',(18.5691905708464,0.22841400672865,-335.644909722255)) ;
#45326 = CARTESIAN_POINT('Ctrl Pts',(18.559433775498,0.643761729554131,-335.639295316782)) ;
#45327 = CARTESIAN_POINT('Ctrl Pts',(18.5196860659661,1.33984239217039,-335.629952200477)) ;
#45328 = CARTESIAN_POINT('Ctrl Pts',(18.4972103671677,1.62085126235232,-335.626199321161)) ;
#45329 = CARTESIAN_POINT('Ctrl Pts',(18.4595924780413,1.98626558838669,-335.621385673521)) ;
#45330 = CARTESIAN_POINT('Ctrl Pts',(18.4502523234525,2.07123023127707,-335.62027117357)) ;
#45331 = CARTESIAN_POINT('Ctrl Pts',(18.4325412217626,2.2227048070847,-335.618294546381)) ;
#45332 = CARTESIAN_POINT('Ctrl Pts',(18.424396177365,2.28923963158799,-335.617429921525)) ;
#45333 = CARTESIAN_POINT('Ctrl Pts',(18.4059860957794,2.43316027776215,-335.615568223306)) ;
#45334 = CARTESIAN_POINT('Ctrl Pts',(18.3955929734265,2.51052828573006,-335.61457257593)) ;
#45335 = CARTESIAN_POINT('Ctrl Pts',(18.3619438296115,2.74958192623614,-335.611509233963)) ;
#45336 = CARTESIAN_POINT('Ctrl Pts',(18.3370416815569,2.91102808233788,-335.609458813545)) ;
#45337 = CARTESIAN_POINT('Ctrl Pts',(18.2265312578581,3.56967555917701,-335.601136108231)) ;
#45338 = CARTESIAN_POINT('Ctrl Pts',(18.1228043386915,4.06361789820827,-335.594988014203)) ;
#45339 = CARTESIAN_POINT('Ctrl Pts',(17.8809329799853,5.01985117940733,-335.582896268257)) ;
#45340 = CARTESIAN_POINT('Ctrl Pts',(17.7446363797407,5.48220289712154,-335.576960508905)) ;
#45341 = CARTESIAN_POINT('Ctrl Pts',(17.5311915306416,6.1144265329805,-335.568582205502)) ;
#45342 = CARTESIAN_POINT('Ctrl Pts',(17.4692446813531,6.28922717182213,-335.566238104824)) ;
#45343 = CARTESIAN_POINT('Ctrl Pts',(17.3607101571914,6.58150462643401,-335.56226712302)) ;
#45344 = CARTESIAN_POINT('Ctrl Pts',(17.3155229509453,6.69948693496976,-335.560649911528)) ;
#45345 = CARTESIAN_POINT('Ctrl Pts',(17.2204068538475,6.94043941225237,-335.557316755067)) ;
#45346 = CARTESIAN_POINT('Ctrl Pts',(17.1703565000958,7.06335395152022,-335.555600038281)) ;
#45347 = CARTESIAN_POINT('Ctrl Pts',(17.0356488639269,7.38427637217871,-335.551074142481)) ;
#45348 = CARTESIAN_POINT('Ctrl Pts',(16.9488570667261,7.5813662116102,-335.54825046295)) ;
#45349 = CARTESIAN_POINT('Ctrl Pts',(16.7441215859397,8.02518888920079,-335.54179452227)) ;
#45350 = CARTESIAN_POINT('Ctrl Pts',(16.6241156399017,8.27091549792316,-335.538150198102)) ;
#45351 = CARTESIAN_POINT('Ctrl Pts',(16.3379890561044,8.82538800520952,-335.529788190633)) ;
#45352 = CARTESIAN_POINT('Ctrl Pts',(16.1684627333268,9.13225998066787,-335.525058628138)) ;
#45353 = CARTESIAN_POINT('Ctrl Pts',(15.9424352510938,9.51536387211735,-335.519071482091)) ;
#45354 = CARTESIAN_POINT('Ctrl Pts',(15.8939008025664,9.5962132448198,-335.517803280702)) ;
#45355 = CARTESIAN_POINT('Ctrl Pts',(15.6768002161025,9.95169691647751,-335.512210655861)) ;
#45356 = CARTESIAN_POINT('Ctrl Pts',(15.5017163214388,10.2222858679354,-335.507908830672)) ;
#45357 = CARTESIAN_POINT('Ctrl Pts',(15.2644308799062,10.5688795005813,-335.50240034878)) ;
#45358 = CARTESIAN_POINT('Ctrl Pts',(15.20854611416,10.649140299531,-335.501124952734)) ;
#45359 = CARTESIAN_POINT('Ctrl Pts',(15.1136665873926,10.7831344580485,-335.498998605056)) ;
#45360 = CARTESIAN_POINT('Ctrl Pts',(15.0750131059346,10.8371069177214,-335.498142997565)) ;
#45361 = CARTESIAN_POINT('Ctrl Pts',(14.9887891621417,10.9561487569534,-335.496258356927)) ;
#45362 = CARTESIAN_POINT('Ctrl Pts',(14.9410828507015,11.0211178835974,-335.495231205263)) ;
#45363 = CARTESIAN_POINT('Ctrl Pts',(14.7860737756539,11.2293616290605,-335.491940178135)) ;
#45364 = CARTESIAN_POINT('Ctrl Pts',(14.6771214687123,11.3713959515619,-335.489697394733)) ;
#45365 = CARTESIAN_POINT('Ctrl Pts',(14.3899618382606,11.7347442781482,-335.483937552399)) ;
#45366 = CARTESIAN_POINT('Ctrl Pts',(14.2086974671388,11.9535827967356,-335.480446036835)) ;
#45367 = CARTESIAN_POINT('Ctrl Pts',(13.558506340965,12.7028564887664,-335.468284339736)) ;
#45368 = CARTESIAN_POINT('Ctrl Pts',(13.0643282980803,13.2105633057365,-335.459645514416)) ;
#45369 = CARTESIAN_POINT('Ctrl Pts',(12.4274883152737,13.7940679745472,-335.448777684871)) ;
#45370 = CARTESIAN_POINT('Ctrl Pts',(12.3112858280405,13.8978781934371,-335.446805845125)) ;
#45371 = CARTESIAN_POINT('Ctrl Pts',(12.0984187997336,14.0832793655732,-335.443210778725)) ;
#45372 = CARTESIAN_POINT('Ctrl Pts',(12.0022008632722,14.1653686689334,-335.441591929667)) ;
#45373 = CARTESIAN_POINT('Ctrl Pts',(11.8034882620262,14.3314241162502,-335.438260106764)) ;
#45374 = CARTESIAN_POINT('Ctrl Pts',(11.7009183955691,14.4152891400008,-335.436546410105)) ;
#45375 = CARTESIAN_POINT('Ctrl Pts',(11.4302922572453,14.6317717677516,-335.432040264131)) ;
#45376 = CARTESIAN_POINT('Ctrl Pts',(11.260824703532,14.7625930275574,-335.42923355503)) ;
#45377 = CARTESIAN_POINT('Ctrl Pts',(10.9733449157868,14.9766833149813,-335.424499816349)) ;
#45378 = CARTESIAN_POINT('Ctrl Pts',(10.8565550136431,15.0615588479245,-335.42258414024)) ;
#45379 = CARTESIAN_POINT('Ctrl Pts',(10.3492663821095,15.4212578778579,-335.414300041746)) ;
#45380 = CARTESIAN_POINT('Ctrl Pts',(9.94923571986067,15.6823217775779,-335.407855243476)) ;
#45381 = CARTESIAN_POINT('Ctrl Pts',(9.35949150821033,16.0355382770163,-335.398601761999)) ;
#45382 = CARTESIAN_POINT('Ctrl Pts',(9.17757834366956,16.1403415386339,-335.395780765775)) ;
#45383 = CARTESIAN_POINT('Ctrl Pts',(8.79300287415107,16.3532978103023,-335.389909769287)) ;
#45384 = CARTESIAN_POINT('Ctrl Pts',(8.59003108939005,16.4608206069525,-335.386863655496)) ;
#45385 = CARTESIAN_POINT('Ctrl Pts',(8.31295942105643,16.6010766490952,-335.382799862364)) ;
#45386 = CARTESIAN_POINT('Ctrl Pts',(8.24056431016954,16.6371313668731,-335.381746648795)) ;
#45387 = CARTESIAN_POINT('Ctrl Pts',(8.10845978946807,16.7018491679338,-335.379841947244)) ;
#45388 = CARTESIAN_POINT('Ctrl Pts',(8.04882822793687,16.7306679476897,-335.378988565922)) ;
#45389 = CARTESIAN_POINT('Ctrl Pts',(7.91551299361442,16.7942189105125,-335.377095389019)) ;
#45390 = CARTESIAN_POINT('Ctrl Pts',(7.84175251613057,16.8287864169338,-335.376057624167)) ;
#45391 = CARTESIAN_POINT('Ctrl Pts',(7.60013399321661,16.9400863705023,-335.372686260311)) ;
#45392 = CARTESIAN_POINT('Ctrl Pts',(7.43135868727245,17.0148015337243,-335.370375190869)) ;
#45393 = CARTESIAN_POINT('Ctrl Pts',(6.98662777341595,17.2037998721767,-335.364369308555)) ;
#45394 = CARTESIAN_POINT('Ctrl Pts',(6.7089792487783,17.3139624459942,-335.360702682872)) ;
#45395 = CARTESIAN_POINT('Ctrl Pts',(5.79613710197483,17.6508945495868,-335.348778546037)) ;
#45396 = CARTESIAN_POINT('Ctrl Pts',(5.1512265327555,17.8497660523533,-335.340539495933)) ;
#45397 = CARTESIAN_POINT('Ctrl Pts',(4.32462111604155,18.0561261845534,-335.329828447429)) ;
#45398 = CARTESIAN_POINT('Ctrl Pts',(4.15170295482127,18.0966682852616,-335.327581051997)) ;
#45399 = CARTESIAN_POINT('Ctrl Pts',(3.85476386808479,18.1618080706447,-335.323706129004)) ;
#45400 = CARTESIAN_POINT('Ctrl Pts',(3.73102448906178,18.1876313213735,-335.322086797838)) ;
#45401 = CARTESIAN_POINT('Ctrl Pts',(3.47423462310636,18.2384900652559,-335.318715842315)) ;
#45402 = CARTESIAN_POINT('Ctrl Pts',(3.34115451005407,18.2633379356204,-335.316963084381)) ;
#45403 = CARTESIAN_POINT('Ctrl Pts',(2.98076800916878,18.3265560850992,-335.312200588201)) ;
#45404 = CARTESIAN_POINT('Ctrl Pts',(2.75299966168767,18.3621520639727,-335.309173350557)) ;
#45405 = CARTESIAN_POINT('Ctrl Pts',(2.36492155502531,18.4154183256899,-335.303990071552)) ;
#45406 = CARTESIAN_POINT('Ctrl Pts',(2.20493652800374,18.435258091332,-335.3018460589)) ;
#45407 = CARTESIAN_POINT('Ctrl Pts',(1.4529934456604,18.5185782699569,-335.291744006921)) ;
#45408 = CARTESIAN_POINT('Ctrl Pts',(0.858463657234613,18.5556452041077,-335.283672015171)) ;
#45409 = CARTESIAN_POINT('Ctrl Pts',(0.0836350694795375,18.5666299792394,
-335.273297028593)) ;
#45410 = CARTESIAN_POINT('Ctrl Pts',(-0.0959413081253097,18.5665704699472,
-335.27090368709)) ;
#45411 = CARTESIAN_POINT('Ctrl Pts',(-0.414857152040541,18.5618377539163,
-335.266687483408)) ;
#45412 = CARTESIAN_POINT('Ctrl Pts',(-0.554198145662138,18.5582001222467,
-335.264856968614)) ;
#45413 = CARTESIAN_POINT('Ctrl Pts',(-0.767221322165178,18.5502376123155,
-335.262082794278)) ;
#45414 = CARTESIAN_POINT('Ctrl Pts',(-0.840940534724422,18.5470418953215,
-335.261127219382)) ;
#45415 = CARTESIAN_POINT('Ctrl Pts',(-0.983553431257418,18.5400076276155,
-335.259288563337)) ;
#45416 = CARTESIAN_POINT('Ctrl Pts',(-1.05244855549534,18.5362243247583,-335.258404918397)) ;
#45417 = CARTESIAN_POINT('Ctrl Pts',(-1.23556842475216,18.5251442729891,-335.256066790827)) ;
#45418 = CARTESIAN_POINT('Ctrl Pts',(-1.34974964382732,18.5171751524668,-335.254619781902)) ;
#45419 = CARTESIAN_POINT('Ctrl Pts',(-1.5414543799913,18.5020128071182,-335.252203800741)) ;
#45420 = CARTESIAN_POINT('Ctrl Pts',(-1.61901946611997,18.495386870883,-335.251229994438)) ;
#45421 = CARTESIAN_POINT('Ctrl Pts',(-1.82368492970421,18.4766061406513,-335.248668034141)) ;
#45422 = CARTESIAN_POINT('Ctrl Pts',(-1.95070560465792,18.4636277283922,-335.247085699949)) ;
#45423 = CARTESIAN_POINT('Ctrl Pts',(-2.63157552302649,18.3869548869227,-335.238626109414)) ;
#45424 = CARTESIAN_POINT('Ctrl Pts',(-3.18247789605013,18.299648514517,-335.23185117434)) ;
#45425 = CARTESIAN_POINT('Ctrl Pts',(-4.08843821929149,18.1139196799848,-335.220450284611)) ;
#45426 = CARTESIAN_POINT('Ctrl Pts',(-4.44599185360067,18.0294916404773,-335.21588451051)) ;
#45427 = CARTESIAN_POINT('Ctrl Pts',(-4.95471813663165,17.8933131202418,-335.209241017136)) ;
#45428 = CARTESIAN_POINT('Ctrl Pts',(-5.10809469044629,17.8501331861639,-335.207218878031)) ;
#45429 = CARTESIAN_POINT('Ctrl Pts',(-5.38007940568743,17.7697689839347,-335.203595962243)) ;
#45430 = CARTESIAN_POINT('Ctrl Pts',(-5.4989058594434,17.7333577884122,-335.20200047228)) ;
#45431 = CARTESIAN_POINT('Ctrl Pts',(-5.75475111258785,17.6521420286851,-335.198536927407)) ;
#45432 = CARTESIAN_POINT('Ctrl Pts',(-5.89163180330693,17.6069291241693,-335.19666619085)) ;
#45433 = CARTESIAN_POINT('Ctrl Pts',(-6.29618725340927,17.4680549051085,-335.191084321221)) ;
#45434 = CARTESIAN_POINT('Ctrl Pts',(-6.5622573393476,17.3698501478164,-335.187343483541)) ;
#45435 = CARTESIAN_POINT('Ctrl Pts',(-7.22112320227258,17.109366688551,-335.177919699912)) ;
#45436 = CARTESIAN_POINT('Ctrl Pts',(-7.6107932800005,16.9396243556441,-335.172198915819)) ;
#45437 = CARTESIAN_POINT('Ctrl Pts',(-8.02955406953755,16.7398413084959,-335.165948881032)) ;
#45438 = CARTESIAN_POINT('Ctrl Pts',(-8.0647602298304,16.7229084798281,-335.165422651895)) ;
#45439 = CARTESIAN_POINT('Ctrl Pts',(-8.48364630451576,16.5198097059098,-335.159153009936)) ;
#45440 = CARTESIAN_POINT('Ctrl Pts',(-8.86085608479542,16.3205881570122,-335.153418610567)) ;
#45441 = CARTESIAN_POINT('Ctrl Pts',(-9.33122703995194,16.0510460713502,-335.146281354338)) ;
#45442 = CARTESIAN_POINT('Ctrl Pts',(-9.43104407875029,15.9926009674279,-335.144767770698)) ;
#45443 = CARTESIAN_POINT('Ctrl Pts',(-9.58388844362059,15.9011785601962,-335.142455480551)) ;
#45444 = CARTESIAN_POINT('Ctrl Pts',(-9.6373063933843,15.8688601605454,-335.141648379132)) ;
#45445 = CARTESIAN_POINT('Ctrl Pts',(-9.75101834568968,15.7992773400052,-335.139933364301)) ;
#45446 = CARTESIAN_POINT('Ctrl Pts',(-9.8112640393381,15.7619358331698,-335.139026610432)) ;
#45447 = CARTESIAN_POINT('Ctrl Pts',(-9.97657591044811,15.6581571388878,-335.136541739612)) ;
#45448 = CARTESIAN_POINT('Ctrl Pts',(-10.0811910610357,15.5910082659753,-335.134972829174)) ;
#45449 = CARTESIAN_POINT('Ctrl Pts',(-10.3230319520279,15.4323270170347,-335.131345873768)) ;
#45450 = CARTESIAN_POINT('Ctrl Pts',(-10.4597280422189,15.3400063640323,-335.12929571719)) ;
#45451 = CARTESIAN_POINT('Ctrl Pts',(-10.9843970389093,14.9753857842908,-335.121395976615)) ;
#45452 = CARTESIAN_POINT('Ctrl Pts',(-11.3631175357686,14.6900891316423,-335.115623071099)) ;
#45453 = CARTESIAN_POINT('Ctrl Pts',(-12.0820925289846,14.1040168304179,-335.104232612596)) ;
#45454 = CARTESIAN_POINT('Ctrl Pts',(-12.4230581271686,13.8046324143305,-335.098622990248)) ;
#45455 = CARTESIAN_POINT('Ctrl Pts',(-12.8620620501793,13.3897160660976,-335.091014365331)) ;
#45456 = CARTESIAN_POINT('Ctrl Pts',(-12.9701478705579,13.2850442469859,-335.08910852522)) ;
#45457 = CARTESIAN_POINT('Ctrl Pts',(-13.1668064692589,13.0899095015855,-335.085577679936)) ;
#45458 = CARTESIAN_POINT('Ctrl Pts',(-13.2557492799914,12.9998320885681,-335.083956195253)) ;
#45459 = CARTESIAN_POINT('Ctrl Pts',(-13.4376021828007,12.8118523866817,-335.08058859985)) ;
#45460 = CARTESIAN_POINT('Ctrl Pts',(-13.5303799442115,12.7138323294396,-335.078841438118)) ;
#45461 = CARTESIAN_POINT('Ctrl Pts',(-13.7770941940885,12.4474183657497,-335.074115873475)) ;
#45462 = CARTESIAN_POINT('Ctrl Pts',(-13.9290089261635,12.2771844671933,-335.071120453631)) ;
#45463 = CARTESIAN_POINT('Ctrl Pts',(-14.1812223124025,11.9838484358036,-335.066002867069)) ;
#45464 = CARTESIAN_POINT('Ctrl Pts',(-14.283149556353,11.8621805868552,-335.063892643693)) ;
#45465 = CARTESIAN_POINT('Ctrl Pts',(-14.7473399079588,11.2934304211647,-335.054093063119)) ;
#45466 = CARTESIAN_POINT('Ctrl Pts',(-15.0902541599651,10.8309663600002,-335.04629668586)) ;
#45467 = CARTESIAN_POINT('Ctrl Pts',(-15.572861369413,10.1125958711499,-335.034695197299)) ;
#45468 = CARTESIAN_POINT('Ctrl Pts',(-15.7289246302337,9.86810706586958,-335.03083221794)) ;
#45469 = CARTESIAN_POINT('Ctrl Pts',(-15.9234651211404,9.54699203720604,-335.025912460148)) ;
#45470 = CARTESIAN_POINT('Ctrl Pts',(-15.9672285833637,9.47361651199007,-335.02479850755)) ;
#45471 = CARTESIAN_POINT('Ctrl Pts',(-16.0444176408969,9.34214397268195,-335.02282253678)) ;
#45472 = CARTESIAN_POINT('Ctrl Pts',(-16.0780380431757,9.28416308365611,-335.021958026319)) ;
#45473 = CARTESIAN_POINT('Ctrl Pts',(-16.1501484068445,9.15823692815331,-335.020096112132)) ;
#45474 = CARTESIAN_POINT('Ctrl Pts',(-16.188525083951,9.09022842527761,-335.019100139213)) ;
#45475 = CARTESIAN_POINT('Ctrl Pts',(-16.3059249618025,8.87907900695379,-335.01603451953)) ;
#45476 = CARTESIAN_POINT('Ctrl Pts',(-16.3834872810126,8.73513466074679,-335.013982183281)) ;
#45477 = CARTESIAN_POINT('Ctrl Pts',(-16.6926791096162,8.14271070656478,-335.005654647406)) ;
#45478 = CARTESIAN_POINT('Ctrl Pts',(-16.9078751841561,7.68589828810875,-334.999503654886)) ;
#45479 = CARTESIAN_POINT('Ctrl Pts',(-17.291398207944,6.77744314014036,-334.987414932742)) ;
#45480 = CARTESIAN_POINT('Ctrl Pts',(-17.4612904415509,6.32688883870352,-334.98148522021)) ;
#45481 = CARTESIAN_POINT('Ctrl Pts',(-17.6721185750458,5.69430566333641,-334.973113098637)) ;
#45482 = CARTESIAN_POINT('Ctrl Pts',(-17.7281159708373,5.51749906089888,-334.970768878094)) ;
#45483 = CARTESIAN_POINT('Ctrl Pts',(-17.8177920233857,5.21888379894125,-334.966797756639)) ;
#45484 = CARTESIAN_POINT('Ctrl Pts',(-17.85289293483,5.09751650313552,-334.965180527014)) ;
#45485 = CARTESIAN_POINT('Ctrl Pts',(-17.9223189315593,4.84794749321801,-334.961847385857)) ;
#45486 = CARTESIAN_POINT('Ctrl Pts',(-17.9565136593231,4.7197169323728,-334.960130703055)) ;
#45487 = CARTESIAN_POINT('Ctrl Pts',(-18.0425774792356,4.38249489724143,-334.955605029565)) ;
#45488 = CARTESIAN_POINT('Ctrl Pts',(-18.0921906532526,4.172948685534,-334.952781541077)) ;
#45489 = CARTESIAN_POINT('Ctrl Pts',(-18.196501377866,3.69548202369461,-334.946326152874)) ;
#45490 = CARTESIAN_POINT('Ctrl Pts',(-18.2489477107355,3.42712077750293,-334.942682193463)) ;
#45491 = CARTESIAN_POINT('Ctrl Pts',(-18.3550699083316,2.81225764761921,-334.934320091271)) ;
#45492 = CARTESIAN_POINT('Ctrl Pts',(-18.4048958466047,2.46519633404073,-334.92959005641)) ;
#45493 = CARTESIAN_POINT('Ctrl Pts',(-18.4556281785574,2.02316491890919,-334.923601266693)) ;
#45494 = CARTESIAN_POINT('Ctrl Pts',(-18.4656748793322,1.92931568512083,-334.922331896669)) ;
#45495 = CARTESIAN_POINT('Ctrl Pts',(-18.5068379991275,1.51496928309236,-334.916741283838)) ;
#45496 = CARTESIAN_POINT('Ctrl Pts',(-18.5303291502361,1.19377007003294,-334.91244260925)) ;
#45497 = CARTESIAN_POINT('Ctrl Pts',(-18.5500526863247,0.774354243649999,
-334.90693609709)) ;
#45498 = CARTESIAN_POINT('Ctrl Pts',(-18.5538771632842,0.676551114338569,
-334.905659668122)) ;
#45499 = CARTESIAN_POINT('Ctrl Pts',(-18.558997681759,0.512359922785138,-334.90353217313)) ;
#45500 = CARTESIAN_POINT('Ctrl Pts',(-18.5607112821091,0.445986972133665,
-334.902676438815)) ;
#45501 = CARTESIAN_POINT('Ctrl Pts',(-18.5637159208321,0.299065403920491,
-334.9007922355)) ;
#45502 = CARTESIAN_POINT('Ctrl Pts',(-18.5648388140045,0.218514848972907,
-334.899765640107)) ;
#45503 = CARTESIAN_POINT('Ctrl Pts',(-18.5667653923379,-0.040748022389909,
-334.896478769565)) ;
#45504 = CARTESIAN_POINT('Ctrl Pts',(-18.5655129890358,-0.219465687027397,
-334.894239513396)) ;
#45505 = CARTESIAN_POINT('Ctrl Pts',(-18.555603492766,-0.681459016635274,
-334.888492195916)) ;
#45506 = CARTESIAN_POINT('Ctrl Pts',(-18.5430403599362,-0.964604577339727,
-334.885009546554)) ;
#45507 = CARTESIAN_POINT('Ctrl Pts',(-18.4763110929399,-1.95557857740714,
-334.872833236993)) ;
#45508 = CARTESIAN_POINT('Ctrl Pts',(-18.3880439379573,-2.66048846941545,
-334.864171681887)) ;
#45509 = CARTESIAN_POINT('Ctrl Pts',(-18.2314995654853,-3.5115682418143,-334.853282864372)) ;
#45510 = CARTESIAN_POINT('Ctrl Pts',(-18.2014436970678,-3.66416909718802,
-334.851314554047)) ;
#45511 = CARTESIAN_POINT('Ctrl Pts',(-18.1434893136446,-3.94008561693026,
-334.847723806858)) ;
#45512 = CARTESIAN_POINT('Ctrl Pts',(-18.1162417789462,-4.06352838017884,
-334.84610571001)) ;
#45513 = CARTESIAN_POINT('Ctrl Pts',(-18.0578364914556,-4.31585686373898,
-334.842773287736)) ;
#45514 = CARTESIAN_POINT('Ctrl Pts',(-18.0265543993462,-4.44470647463516,
-334.841058217131)) ;
#45515 = CARTESIAN_POINT('Ctrl Pts',(-17.9410222858601,-4.78124381212508,
-334.83654308645)) ;
#45516 = CARTESIAN_POINT('Ctrl Pts',(-17.8845460617282,-4.98834491270067,
-334.833728657251)) ;
#45517 = CARTESIAN_POINT('Ctrl Pts',(-17.7483517476163,-5.45569150749847,
-334.827299443169)) ;
#45518 = CARTESIAN_POINT('Ctrl Pts',(-17.66647659598,-5.71525711241862,-334.823672755528)) ;
#45519 = CARTESIAN_POINT('Ctrl Pts',(-17.4656206151431,-6.30639633022794,
-334.815306417608)) ;
#45520 = CARTESIAN_POINT('Ctrl Pts',(-17.3428499747142,-6.63657235056142,
-334.810554264224)) ;
#45521 = CARTESIAN_POINT('Ctrl Pts',(-17.1719479848504,-7.05899516766195,
-334.804420666509)) ;
#45522 = CARTESIAN_POINT('Ctrl Pts',(-17.1323316724229,-7.15460843429407,
-334.803028856265)) ;
#45523 = CARTESIAN_POINT('Ctrl Pts',(-16.9686325099822,-7.54053627696221,
-334.797402016748)) ;
#45524 = CARTESIAN_POINT('Ctrl Pts',(-16.8379529937919,-7.82799567563168,
-334.793189220597)) ;
#45525 = CARTESIAN_POINT('Ctrl Pts',(-16.6576324496975,-8.19921863509387,
-334.787778046712)) ;
#45526 = CARTESIAN_POINT('Ctrl Pts',(-16.6145750401886,-8.28612100615992,
-334.786513517972)) ;
#45527 = CARTESIAN_POINT('Ctrl Pts',(-16.5409418945252,-8.43185244127477,
-334.784399206381)) ;
#45528 = CARTESIAN_POINT('Ctrl Pts',(-16.5107284164295,-8.49086223785387,
-334.783544898425)) ;
#45529 = CARTESIAN_POINT('Ctrl Pts',(-16.4428595308351,-8.62168455555351,
-334.781655488455)) ;
#45530 = CARTESIAN_POINT('Ctrl Pts',(-16.4050484981966,-8.69341462961981,
-334.780622352302)) ;
#45531 = CARTESIAN_POINT('Ctrl Pts',(-16.2807921051508,-8.92543973732067,
-334.777286270285)) ;
#45532 = CARTESIAN_POINT('Ctrl Pts',(-16.1924577370712,-9.08471126219075,
-334.7750052168)) ;
#45533 = CARTESIAN_POINT('Ctrl Pts',(-16.0251053456448,-9.37625877157221,
-334.77082590501)) ;
#45534 = CARTESIAN_POINT('Ctrl Pts',(-15.9467564671573,-9.50890046969323,
-334.768923016434)) ;
#45535 = CARTESIAN_POINT('Ctrl Pts',(-15.431169504156,-10.3574719845986,-334.756700645397)) ;
#45536 = CARTESIAN_POINT('Ctrl Pts',(-14.9474851005102,-11.0440441628066,
-334.74653650393)) ;
#45537 = CARTESIAN_POINT('Ctrl Pts',(-14.3221177228642,-11.8150375761764,
-334.734040774378)) ;
#45538 = CARTESIAN_POINT('Ctrl Pts',(-14.2237196057069,-11.9333134326557,
-334.732093130011)) ;
#45539 = CARTESIAN_POINT('Ctrl Pts',(-14.0420522173019,-12.1462404230145,
-334.728527603671)) ;
#45540 = CARTESIAN_POINT('Ctrl Pts',(-13.9592672232226,-12.2412926370082,
-334.72691384249)) ;
#45541 = CARTESIAN_POINT('Ctrl Pts',(-13.7870155784079,-12.4350490611055,
-334.723577507064)) ;
#45542 = CARTESIAN_POINT('Ctrl Pts',(-13.6974415680007,-12.533648237426,-334.721854053729)) ;
#45543 = CARTESIAN_POINT('Ctrl Pts',(-13.4583883598942,-12.7911640198104,
-334.717284092982)) ;
#45544 = CARTESIAN_POINT('Ctrl Pts',(-13.3071559617381,-12.9484243896679,
-334.714422542752)) ;
#45545 = CARTESIAN_POINT('Ctrl Pts',(-12.9564530151125,-13.3004710736074,
-334.707856672908)) ;
#45546 = CARTESIAN_POINT('Ctrl Pts',(-12.7552959823839,-13.4935032324896,
-334.704139618936)) ;
#45547 = CARTESIAN_POINT('Ctrl Pts',(-12.2455972803217,-13.9610287176639,
-334.694866640363)) ;
#45548 = CARTESIAN_POINT('Ctrl Pts',(-11.9320996672972,-14.2298971425154,
-334.689287473819)) ;
#45549 = CARTESIAN_POINT('Ctrl Pts',(-11.3448073337259,-14.7005185735621,
-334.679175474132)) ;
#45550 = CARTESIAN_POINT('Ctrl Pts',(-11.0739338404125,-14.9056328240651,
-334.674635099578)) ;
#45551 = CARTESIAN_POINT('Ctrl Pts',(-10.7165473698945,-15.1611356961604,
-334.668871130383)) ;
#45552 = CARTESIAN_POINT('Ctrl Pts',(-10.6350442105427,-15.2184183741542,
-334.667571502045)) ;
#45553 = CARTESIAN_POINT('Ctrl Pts',(-10.4982836472523,-15.3129022822457,
-334.665418098418)) ;
#45554 = CARTESIAN_POINT('Ctrl Pts',(-10.4432800152174,-15.3504670419113,
-334.664559375342)) ;
#45555 = CARTESIAN_POINT('Ctrl Pts',(-10.3221067933255,-15.4322696291284,
-334.662684308674)) ;
#45556 = CARTESIAN_POINT('Ctrl Pts',(-10.2558525896091,-15.4763794940035,
-334.661669668119)) ;
#45557 = CARTESIAN_POINT('Ctrl Pts',(-10.0450017396543,-15.61480845753,-334.658470891547)) ;
#45558 = CARTESIAN_POINT('Ctrl Pts',(-9.8993720055007,-15.7075375916401,-334.65630625538)) ;
#45559 = CARTESIAN_POINT('Ctrl Pts',(-9.52429504265865,-15.9390780008328,
-334.650819882003)) ;
#45560 = CARTESIAN_POINT('Ctrl Pts',(-9.29309489686995,-16.074974064613,-334.647520889701)) ;
#45561 = CARTESIAN_POINT('Ctrl Pts',(-8.40423521688958,-16.5718456359355,
-334.635030408914)) ;
#45562 = CARTESIAN_POINT('Ctrl Pts',(-7.72785449681234,-16.8978549643495,
-334.625888748716)) ;
#45563 = CARTESIAN_POINT('Ctrl Pts',(-6.88167301169118,-17.2442462894622,
-334.614369620857)) ;
#45564 = CARTESIAN_POINT('Ctrl Pts',(-6.72891546106093,-17.3044257384822,
-334.61228849112)) ;
#45565 = CARTESIAN_POINT('Ctrl Pts',(-6.45846015792787,-17.4068498773485,
-334.608597874609)) ;
#45566 = CARTESIAN_POINT('Ctrl Pts',(-6.34109611966826,-17.4499464243691,
-334.606994385402)) ;
#45567 = CARTESIAN_POINT('Ctrl Pts',(-6.09172608314385,-17.5386680652489,
-334.603582379403)) ;
#45568 = CARTESIAN_POINT('Ctrl Pts',(-5.95962241660026,-17.5839956993332,
-334.601771936799)) ;
#45569 = CARTESIAN_POINT('Ctrl Pts',(-5.58436872933906,-17.7080388145836,
-334.596620649977)) ;
#45570 = CARTESIAN_POINT('Ctrl Pts',(-5.34008756417781,-17.783230222862,-334.593256884592)) ;
#45571 = CARTESIAN_POINT('Ctrl Pts',(-4.91263407461246,-17.9052011509568,
-334.587359444321)) ;
#45572 = CARTESIAN_POINT('Ctrl Pts',(-4.73015483795835,-17.9542707145394,
-334.584838398952)) ;
#45573 = CARTESIAN_POINT('Ctrl Pts',(-4.20009954116143,-18.0881632902019,
-334.577515640882)) ;
#45574 = CARTESIAN_POINT('Ctrl Pts',(-3.8507806160192,-18.1657363087151,-334.572688826933)) ;
#45575 = CARTESIAN_POINT('Ctrl Pts',(-3.45144829283486,-18.2423790138929,
-334.567215090276)) ;
#45576 = CARTESIAN_POINT('Ctrl Pts',(-3.40342083171717,-18.2514003311451,
-334.566557519119)) ;
#45577 = CARTESIAN_POINT('Ctrl Pts',(-3.01805138687179,-18.3222128254613,
-334.561288281021)) ;
#45578 = CARTESIAN_POINT('Ctrl Pts',(-2.67909121276421,-18.3748357275041,
-334.556695716192)) ;
#45579 = CARTESIAN_POINT('Ctrl Pts',(-2.22616288534428,-18.4323521430718,
-334.55068732171)) ;
#45580 = CARTESIAN_POINT('Ctrl Pts',(-2.11332848287763,-18.445629550162,-334.549201166485)) ;
#45581 = CARTESIAN_POINT('Ctrl Pts',(-1.93865279246789,-18.4645600991707,
-334.546920611706)) ;
#45582 = CARTESIAN_POINT('Ctrl Pts',(-1.87689313665326,-18.4709400538601,
-334.546118166271)) ;
#45583 = CARTESIAN_POINT('Ctrl Pts',(-1.74405316600134,-18.4839896854498,
-334.544401391305)) ;
#45584 = CARTESIAN_POINT('Ctrl Pts',(-1.67296401224935,-18.4905594174153,
-334.543488314414)) ;
#45585 = CARTESIAN_POINT('Ctrl Pts',(-1.47539718496243,-18.5076689483902,
-334.540964417224)) ;
#45586 = CARTESIAN_POINT('Ctrl Pts',(-1.3488465631758,-18.5173221548281,-334.539363278067)) ;
#45587 = CARTESIAN_POINT('Ctrl Pts',(-1.05274130264155,-18.5368573038878,
-334.535644106933)) ;
#45588 = CARTESIAN_POINT('Ctrl Pts',(-0.883130162201162,-18.5457117469981,
-334.533534522364)) ;
#45589 = CARTESIAN_POINT('Ctrl Pts',(-0.207385116840132,-18.5716973408216,
-334.525178411999)) ;
#45590 = CARTESIAN_POINT('Ctrl Pts',(0.299235767185004,-18.5704445275094,
-334.519016412708)) ;
#45591 = CARTESIAN_POINT('Ctrl Pts',(1.17806417954462,-18.532295477931,-334.508199821747)) ;
#45592 = CARTESIAN_POINT('Ctrl Pts',(1.55038398504384,-18.5048674568597,-334.503578921506)) ;
#45593 = CARTESIAN_POINT('Ctrl Pts',(2.10397535003999,-18.4472599496149,-334.496588216107)) ;
#45594 = CARTESIAN_POINT('Ctrl Pts',(2.28603653196849,-18.4255840815446,-334.494270066832)) ;
#45595 = CARTESIAN_POINT('Ctrl Pts',(2.59263787521039,-18.3844664490713,-334.490329271862)) ;
#45596 = CARTESIAN_POINT('Ctrl Pts',(2.71735532290006,-18.3664465198158,-334.488715938975)) ;
#45597 = CARTESIAN_POINT('Ctrl Pts',(2.97358133457003,-18.3267584413797,-334.485379171281)) ;
#45598 = CARTESIAN_POINT('Ctrl Pts',(3.10505952347914,-18.3049410328061,-334.483654843658)) ;
#45599 = CARTESIAN_POINT('Ctrl Pts',(3.45147480144925,-18.243617406876,-334.479079161555)) ;
#45600 = CARTESIAN_POINT('Ctrl Pts',(3.66596865724095,-18.2017287072936,-334.476212693314)) ;
#45601 = CARTESIAN_POINT('Ctrl Pts',(4.55125348137117,-18.0125568991946,-334.464250697676)) ;
#45602 = CARTESIAN_POINT('Ctrl Pts',(5.21435352797801,-17.8318990944563,-334.454955756248)) ;
#45603 = CARTESIAN_POINT('Ctrl Pts',(6.19458890065182,-17.5054727110899,-334.441072156181)) ;
#45604 = CARTESIAN_POINT('Ctrl Pts',(6.52013711864472,-17.3868432815609,-334.436441152158)) ;
#45605 = CARTESIAN_POINT('Ctrl Pts',(6.93375071595263,-17.2228715481268,-334.430605207607)) ;
#45606 = CARTESIAN_POINT('Ctrl Pts',(7.02503548756114,-17.1858395137953,-334.429320355292)) ;
#45607 = CARTESIAN_POINT('Ctrl Pts',(7.17741420547475,-17.122606193807,-334.427183483661)) ;
#45608 = CARTESIAN_POINT('Ctrl Pts',(7.23866988640693,-17.0968001642626,-334.426326694641)) ;
#45609 = CARTESIAN_POINT('Ctrl Pts',(7.37352489145439,-17.0391332470442,-334.424445957889)) ;
#45610 = CARTESIAN_POINT('Ctrl Pts',(7.44705888295391,-17.007123365019,-334.423423820469)) ;
#45611 = CARTESIAN_POINT('Ctrl Pts',(7.68168683400369,-16.9031746325087,-334.420170073241)) ;
#45612 = CARTESIAN_POINT('Ctrl Pts',(7.84196389482282,-16.8294155494729,-334.417958904565)) ;
#45613 = CARTESIAN_POINT('Ctrl Pts',(8.25164397890684,-16.6337584629967,-334.412310700348)) ;
#45614 = CARTESIAN_POINT('Ctrl Pts',(8.4994085598984,-16.5085312333746,-334.408898047725)) ;
#45615 = CARTESIAN_POINT('Ctrl Pts',(9.38142646674977,-16.0376128787603,-334.396638044146)) ;
#45616 = CARTESIAN_POINT('Ctrl Pts',(9.99818703630216,-15.6605378311281,-334.387828880518)) ;
#45617 = CARTESIAN_POINT('Ctrl Pts',(10.7181128048373,-15.1604867009398,-334.376796449642)) ;
#45618 = CARTESIAN_POINT('Ctrl Pts',(10.8437163370719,-15.0709029263927,-334.374843602471)) ;
#45619 = CARTESIAN_POINT('Ctrl Pts',(11.0699608966569,-14.9052465804426,-334.371271738166)) ;
#45620 = CARTESIAN_POINT('Ctrl Pts',(11.1709710003382,-14.8296937505098,-334.369656896886)) ;
#45621 = CARTESIAN_POINT('Ctrl Pts',(11.3769274072928,-14.6723455480637,-334.366321613404)) ;
#45622 = CARTESIAN_POINT('Ctrl Pts',(11.4817801608207,-14.5904395200544,-334.364600326314)) ;
#45623 = CARTESIAN_POINT('Ctrl Pts',(11.7555052887966,-14.3718403150183,-334.360044538547)) ;
#45624 = CARTESIAN_POINT('Ctrl Pts',(11.9228741949506,-14.2332979069273,-334.357195170265)) ;
#45625 = CARTESIAN_POINT('Ctrl Pts',(12.2980492562701,-13.9114785004873,-334.350664752019)) ;
#45626 = CARTESIAN_POINT('Ctrl Pts',(12.5042617611538,-13.7264229486378,-334.346971186346)) ;
#45627 = CARTESIAN_POINT('Ctrl Pts',(12.9582890673179,-13.3002530034025,-334.338623546852)) ;
#45628 = CARTESIAN_POINT('Ctrl Pts',(13.2036664901206,-13.0566908680963,-334.333959319758)) ;
#45629 = CARTESIAN_POINT('Ctrl Pts',(13.5285869382446,-12.7156421603863,-334.327619265712)) ;
#45630 = CARTESIAN_POINT('Ctrl Pts',(13.6141512864416,-12.6239892612005,-334.325933570971)) ;
#45631 = CARTESIAN_POINT('Ctrl Pts',(13.8974877698098,-12.314260053083,-334.320304848645)) ;
#45632 = CARTESIAN_POINT('Ctrl Pts',(14.0910006784114,-12.0923474755302,-334.316382160305)) ;
#45633 = CARTESIAN_POINT('Ctrl Pts',(14.3400293973394,-11.7926726491013,-334.311275575564)) ;
#45634 = CARTESIAN_POINT('Ctrl Pts',(14.4003391777056,-11.7189505899678,-334.310034167337)) ;
#45635 = CARTESIAN_POINT('Ctrl Pts',(14.501549326356,-11.5932712467783,-334.307945235598)) ;
#45636 = CARTESIAN_POINT('Ctrl Pts',(14.5427442106202,-11.5415537048316,-334.307093465033)) ;
#45637 = CARTESIAN_POINT('Ctrl Pts',(14.5870205934659,-11.4853541112165,-334.306176508206)) ;
#45638 = CARTESIAN_POINT('Ctrl Pts',(14.5903772125746,-11.4810897413541,-334.306106982867)) ;
#45639 = CARTESIAN_POINT('Ctrl Pts',(14.5964088578749,-11.4734200048863,-334.305982030865)) ;
#45640 = CARTESIAN_POINT('Ctrl Pts',(14.5990845632339,-11.4700151730643,-334.305926593993)) ;
#45641 = CARTESIAN_POINT('Ctrl Pts',(14.6032861400707,-11.4646648196558,-334.30583953231)) ;
#45642 = CARTESIAN_POINT('Ctrl Pts',(14.6048128144616,-11.462719928986,-334.305807895535)) ;
#45643 = CARTESIAN_POINT('Ctrl Pts',(14.6072011058389,-11.4596761387939,-334.305758400167)) ;
#45644 = CARTESIAN_POINT('Ctrl Pts',(14.6080629873956,-11.4585774469935,-334.305740537652)) ;
#45645 = CARTESIAN_POINT('Ctrl Pts',(14.6107766949918,-11.4551173183529,-334.305684293679)) ;
#45646 = CARTESIAN_POINT('Ctrl Pts',(14.6126280725162,-11.4527555296731,-334.305645918852)) ;
#45647 = CARTESIAN_POINT('Ctrl Pts',(14.6161587865224,-11.4482491739567,-334.305572728619)) ;
#45648 = CARTESIAN_POINT('Ctrl Pts',(14.6178382238301,-11.4461046860393,-334.305537911733)) ;
#45649 = CARTESIAN_POINT('Ctrl Pts',(14.621041680062,-11.4420123103101,-334.305471494467)) ;
#45650 = CARTESIAN_POINT('Ctrl Pts',(14.6225657817803,-11.4400644874453,-334.305439892879)) ;
#45651 = CARTESIAN_POINT('Ctrl Pts',(14.6254735138087,-11.4363468356861,-334.305379597708)) ;
#45652 = CARTESIAN_POINT('Ctrl Pts',(14.6268572122201,-11.4345770600644,-334.305350903136)) ;
#45653 = CARTESIAN_POINT('Ctrl Pts',(14.684340900627,-11.3610268618028,-334.304158746142)) ;
#45654 = CARTESIAN_POINT('Ctrl Pts',(14.7399121766279,-11.2888346651964,-334.303002929337)) ;
#45655 = CARTESIAN_POINT('Ctrl Pts',(14.9705546641567,-10.9846021267888,-334.298185627773)) ;
#45656 = CARTESIAN_POINT('Ctrl Pts',(15.1406958325475,-10.7488753480212,-334.294581831229)) ;
#45657 = CARTESIAN_POINT('Ctrl Pts',(15.7798840102583,-9.81798848822343,-334.280675628014)) ;
#45658 = CARTESIAN_POINT('Ctrl Pts',(16.2071584254526,-9.09536462014561,-334.270520559468)) ;
#45659 = CARTESIAN_POINT('Ctrl Pts',(16.6627203593302,-8.1901658754324,-334.257774378502)) ;
#45660 = CARTESIAN_POINT('Ctrl Pts',(16.7391077518726,-8.03289103494846,-334.255561053074)) ;
#45661 = CARTESIAN_POINT('Ctrl Pts',(16.8667074425404,-7.76044828213136,-334.251725240976)) ;
#45662 = CARTESIAN_POINT('Ctrl Pts',(16.9189894217914,-7.6457945554539,-334.250110499529)) ;
#45663 = CARTESIAN_POINT('Ctrl Pts',(17.0202127641094,-7.41768972438955,-334.246896087154)) ;
#45664 = CARTESIAN_POINT('Ctrl Pts',(17.0691968927181,-7.30426456053074,-334.245296819076)) ;
#45665 = CARTESIAN_POINT('Ctrl Pts',(17.1382553962219,-7.13986699418179,-334.242977395412)) ;
#45666 = CARTESIAN_POINT('Ctrl Pts',(17.1592420671434,-7.08928137385079,-334.24226350844)) ;
#45667 = CARTESIAN_POINT('Ctrl Pts',(17.212711257848,-6.95877239973039,-334.240421235097)) ;
#45668 = CARTESIAN_POINT('Ctrl Pts',(17.2448610666167,-6.87871419192239,-334.239290670346)) ;
#45669 = CARTESIAN_POINT('Ctrl Pts',(17.4618110502084,-6.32739230861528,-334.231502560684)) ;
#45670 = CARTESIAN_POINT('Ctrl Pts',(17.6278278810132,-5.84896743316346,-334.224724982449)) ;
#45671 = CARTESIAN_POINT('Ctrl Pts',(17.9441733164718,-4.80079921556183,-334.209987094631)) ;
#45672 = CARTESIAN_POINT('Ctrl Pts',(18.0873610074677,-4.22946824820636,-334.202019905579)) ;
#45673 = CARTESIAN_POINT('Ctrl Pts',(18.2239350176425,-3.54878010385512,-334.192898809154)) ;
#45674 = CARTESIAN_POINT('Ctrl Pts',(18.2438224347482,-3.44508211391819,-334.191519659579)) ;
#45675 = CARTESIAN_POINT('Ctrl Pts',(18.2748465935001,-3.27550670364407,-334.189284396455)) ;
#45676 = CARTESIAN_POINT('Ctrl Pts',(18.2865142331733,-3.20972887036489,-334.188422285293)) ;
#45677 = CARTESIAN_POINT('Ctrl Pts',(18.3082225652916,-3.08338367843785,-334.18677659065)) ;
#45678 = CARTESIAN_POINT('Ctrl Pts',(18.3183183308969,-3.0228268140341,-334.185992195983)) ;
#45679 = CARTESIAN_POINT('Ctrl Pts',(18.3405660872816,-2.88517354228373,-334.184218065884)) ;
#45680 = CARTESIAN_POINT('Ctrl Pts',(18.3525326713659,-2.80804831456253,-334.183230369278)) ;
#45681 = CARTESIAN_POINT('Ctrl Pts',(18.3825217873611,-2.60638197280485,-334.180661863784)) ;
#45682 = CARTESIAN_POINT('Ctrl Pts',(18.3997650965196,-2.48172897547759,-334.179088250415)) ;
#45683 = CARTESIAN_POINT('Ctrl Pts',(18.4781203008743,-1.86949986221311,-334.171410388187)) ;
#45684 = CARTESIAN_POINT('Ctrl Pts',(18.5211258234318,-1.37980423008815,-334.16542192462)) ;
#45685 = CARTESIAN_POINT('Ctrl Pts',(18.5446545951453,-0.888979948736885,
-334.159397110264)) ;
#45686 = CARTESIAN_POINT('Ctrl Pts',(18.5446545936004,-0.888979980963982,
-333.864249094225)) ;
#45687 = CARTESIAN_POINT('Ctrl Pts',(18.5364060801737,-1.06104890904447,-333.866385237156)) ;
#45688 = CARTESIAN_POINT('Ctrl Pts',(18.5257627102001,-1.23300327160291,-333.868507658875)) ;
#45689 = CARTESIAN_POINT('Ctrl Pts',(18.4814882950303,-1.81646298999327,-333.875695449156)) ;
#45690 = CARTESIAN_POINT('Ctrl Pts',(18.4365268932318,-2.2269763609594,-333.880731733973)) ;
#45691 = CARTESIAN_POINT('Ctrl Pts',(18.3385715194033,-2.91000203681898,-333.889225167194)) ;
#45692 = CARTESIAN_POINT('Ctrl Pts',(18.2930869448647,-3.18343947944684,-333.892655512125)) ;
#45693 = CARTESIAN_POINT('Ctrl Pts',(18.2010477239368,-3.66927628575645,-333.898836146372)) ;
#45694 = CARTESIAN_POINT('Ctrl Pts',(18.1568515815253,-3.88206995265725,-333.901572730302)) ;
#45695 = CARTESIAN_POINT('Ctrl Pts',(18.0795887957112,-4.22382209790757,-333.906023971289)) ;
#45696 = CARTESIAN_POINT('Ctrl Pts',(18.0488531584613,-4.35328654460257,-333.907723280171)) ;
#45697 = CARTESIAN_POINT('Ctrl Pts',(17.9862766986735,-4.60480821919209,-333.911051475793)) ;
#45698 = CARTESIAN_POINT('Ctrl Pts',(17.9545784001488,-4.72689355032367,-333.912679331906)) ;
#45699 = CARTESIAN_POINT('Ctrl Pts',(17.8813572375459,-4.99753470145266,-333.916316100126)) ;
#45700 = CARTESIAN_POINT('Ctrl Pts',(17.839222135693,-5.14591520012333,-333.918328958077)) ;
#45701 = CARTESIAN_POINT('Ctrl Pts',(17.5891077884254,-5.98668834988175,-333.92984116475)) ;
#45702 = CARTESIAN_POINT('Ctrl Pts',(17.3426753624236,-6.66698978674249,-333.939597839374)) ;
#45703 = CARTESIAN_POINT('Ctrl Pts',(16.9477440001816,-7.58586302227325,-333.953058411041)) ;
#45704 = CARTESIAN_POINT('Ctrl Pts',(16.8325912294537,-7.83806208814005,-333.956779925646)) ;
#45705 = CARTESIAN_POINT('Ctrl Pts',(16.6350450904975,-8.2462626987908,-333.962803818454)) ;
#45706 = CARTESIAN_POINT('Ctrl Pts',(16.555999424233,-8.40383584517819,-333.965129106194)) ;
#45707 = CARTESIAN_POINT('Ctrl Pts',(16.4377552092092,-8.63140377377534,-333.968475041525)) ;
#45708 = CARTESIAN_POINT('Ctrl Pts',(16.4003282117755,-8.70230785445617,-333.969515775402)) ;
#45709 = CARTESIAN_POINT('Ctrl Pts',(16.3310320130392,-8.83155205022018,-333.971408009307)) ;
#45710 = CARTESIAN_POINT('Ctrl Pts',(16.2993065982752,-8.88996752724849,-333.972261275484)) ;
#45711 = CARTESIAN_POINT('Ctrl Pts',(16.21977006569,-9.03455978564466,-333.974369250694)) ;
#45712 = CARTESIAN_POINT('Ctrl Pts',(16.1715852078454,-9.12052868042802,-333.975619123293)) ;
#45713 = CARTESIAN_POINT('Ctrl Pts',(15.9505704565034,-9.50759320205602,-333.981239269331)) ;
#45714 = CARTESIAN_POINT('Ctrl Pts',(15.7699999203731,-9.80418941231599,-333.985527043904)) ;
#45715 = CARTESIAN_POINT('Ctrl Pts',(15.3567328172156,-10.4420156282245,-333.994862288099)) ;
#45716 = CARTESIAN_POINT('Ctrl Pts',(15.1207524438782,-10.7808987995435,-333.999898473163)) ;
#45717 = CARTESIAN_POINT('Ctrl Pts',(14.7083882915456,-11.3328760861695,-334.008380103941)) ;
#45718 = CARTESIAN_POINT('Ctrl Pts',(14.5381892058658,-11.5504034908375,-334.01179845341)) ;
#45719 = CARTESIAN_POINT('Ctrl Pts',(14.2258347592792,-11.9317694944369,-334.017960472686)) ;
#45720 = CARTESIAN_POINT('Ctrl Pts',(14.0855411589775,-12.0970669125876,-334.020690573568)) ;
#45721 = CARTESIAN_POINT('Ctrl Pts',(13.8545820268105,-12.359722339258,-334.025134098081)) ;
#45722 = CARTESIAN_POINT('Ctrl Pts',(13.7657087651635,-12.4586292011734,-334.0268322776)) ;
#45723 = CARTESIAN_POINT('Ctrl Pts',(13.5904397072279,-12.6495205586803,-334.030160069561)) ;
#45724 = CARTESIAN_POINT('Ctrl Pts',(13.5041533341459,-12.74159583704,-334.03178867142)) ;
#45725 = CARTESIAN_POINT('Ctrl Pts',(13.3101520215797,-12.9444281275674,-334.035429476969)) ;
#45726 = CARTESIAN_POINT('Ctrl Pts',(13.2019797081778,-13.054734699573,-334.0374456582)) ;
#45727 = CARTESIAN_POINT('Ctrl Pts',(12.5791377785212,-13.6742061411934,-334.048975013189)) ;
#45728 = CARTESIAN_POINT('Ctrl Pts',(12.0364116004989,-14.1542717207302,-334.058746182979)) ;
#45729 = CARTESIAN_POINT('Ctrl Pts',(11.2498704771485,-14.7719724234797,-334.072205681112)) ;
#45730 = CARTESIAN_POINT('Ctrl Pts',(11.0289150869606,-14.9376633829717,-334.075912648649)) ;
#45731 = CARTESIAN_POINT('Ctrl Pts',(10.661335665571,-15.2007021647557,-334.081916473074)) ;
#45732 = CARTESIAN_POINT('Ctrl Pts',(10.516878082963,-15.3010032367193,-334.084236067762)) ;
#45733 = CARTESIAN_POINT('Ctrl Pts',(10.3045730284832,-15.4439856051886,-334.087575520522)) ;
#45734 = CARTESIAN_POINT('Ctrl Pts',(10.237839822277,-15.4883037311974,-334.088615360916)) ;
#45735 = CARTESIAN_POINT('Ctrl Pts',(10.1151976016924,-15.5686125792083,-334.090506882322)) ;
#45736 = CARTESIAN_POINT('Ctrl Pts',(10.0593782291162,-15.6047374152743,-334.091360317701)) ;
#45737 = CARTESIAN_POINT('Ctrl Pts',(9.9202427214049,-15.6937254854263,-334.093469975944)) ;
#45738 = CARTESIAN_POINT('Ctrl Pts',(9.8366969140021,-15.746225869286,-334.094721342886)) ;
#45739 = CARTESIAN_POINT('Ctrl Pts',(9.45586571684599,-15.9813273203421,-334.100364446704)) ;
#45740 = CARTESIAN_POINT('Ctrl Pts',(9.15388723672968,-16.1561928988392,-334.104672873246)) ;
#45741 = CARTESIAN_POINT('Ctrl Pts',(8.38452932051349,-16.573203516772,-334.115421141634)) ;
#45742 = CARTESIAN_POINT('Ctrl Pts',(7.91144540126423,-16.8041792044361,-334.121831058525)) ;
#45743 = CARTESIAN_POINT('Ctrl Pts',(7.28992739324099,-17.0755541635573,-334.130224751194)) ;
#45744 = CARTESIAN_POINT('Ctrl Pts',(7.14992216220353,-17.1346492348249,-334.132113200787)) ;
#45745 = CARTESIAN_POINT('Ctrl Pts',(6.80400139234613,-17.275681561107,-334.136779996954)) ;
#45746 = CARTESIAN_POINT('Ctrl Pts',(6.59731426680543,-17.3556634145908,-334.139569291856)) ;
#45747 = CARTESIAN_POINT('Ctrl Pts',(6.26360490354329,-17.4779764032883,-334.144083288628)) ;
#45748 = CARTESIAN_POINT('Ctrl Pts',(6.13747047776568,-17.5226670804847,-334.145791786265)) ;
#45749 = CARTESIAN_POINT('Ctrl Pts',(5.89191572122929,-17.6066928738069,-334.149123630426)) ;
#45750 = CARTESIAN_POINT('Ctrl Pts',(5.77255712211019,-17.6461862462551,-334.150745786696)) ;
#45751 = CARTESIAN_POINT('Ctrl Pts',(5.47998667982631,-17.7397058542262,-334.154728930388)) ;
#45752 = CARTESIAN_POINT('Ctrl Pts',(5.3063663907609,-17.7924111176026,-334.157098603147)) ;
#45753 = CARTESIAN_POINT('Ctrl Pts',(4.53173775694455,-18.015215177998,-334.167695090417)) ;
#45754 = CARTESIAN_POINT('Ctrl Pts',(3.92314529884862,-18.1574654275551,-334.176098800478)) ;
#45755 = CARTESIAN_POINT('Ctrl Pts',(2.84082238948169,-18.3534783872777,-334.19091474368)) ;
#45756 = CARTESIAN_POINT('Ctrl Pts',(2.37001671250625,-18.4201917146807,-334.19731311006)) ;
#45757 = CARTESIAN_POINT('Ctrl Pts',(1.79531814421084,-18.4792265956159,-334.204897777105)) ;
#45758 = CARTESIAN_POINT('Ctrl Pts',(1.69338066734606,-18.4888464965266,-334.206234318073)) ;
#45759 = CARTESIAN_POINT('Ctrl Pts',(1.5246318301483,-18.5033641256042,-334.208429432628)) ;
#45760 = CARTESIAN_POINT('Ctrl Pts',(1.45786426468749,-18.5087443660465,-334.209293400324)) ;
#45761 = CARTESIAN_POINT('Ctrl Pts',(1.3130742312624,-18.5196234563505,-334.211156358076)) ;
#45762 = CARTESIAN_POINT('Ctrl Pts',(1.23504331076919,-18.5249908217135,-334.212153894217)) ;
#45763 = CARTESIAN_POINT('Ctrl Pts',(0.99304677073675,-18.5401007719236,-334.215230472338)) ;
#45764 = CARTESIAN_POINT('Ctrl Pts',(0.828983915114168,-18.5481606729392,
-334.217292028442)) ;
#45765 = CARTESIAN_POINT('Ctrl Pts',(0.362822641533809,-18.5648643423225,
-334.223104286098)) ;
#45766 = CARTESIAN_POINT('Ctrl Pts',(0.0605900320434588,-18.568310577315,
-334.226819147546)) ;
#45767 = CARTESIAN_POINT('Ctrl Pts',(-0.721153041578525,-18.5581371757636,
-334.236404149761)) ;
#45768 = CARTESIAN_POINT('Ctrl Pts',(-1.20029231359165,-18.5333163615334,
-334.242259255512)) ;
#45769 = CARTESIAN_POINT('Ctrl Pts',(-1.82205415582555,-18.4768926112265,
-334.249995012317)) ;
#45770 = CARTESIAN_POINT('Ctrl Pts',(-1.96601924831227,-18.4621290801129,
-334.251795392878)) ;
#45771 = CARTESIAN_POINT('Ctrl Pts',(-2.32282785022268,-18.4213177075875,
-334.256286003353)) ;
#45772 = CARTESIAN_POINT('Ctrl Pts',(-2.53542039264459,-18.3932628564735,
-334.258986937321)) ;
#45773 = CARTESIAN_POINT('Ctrl Pts',(-2.8785683235496,-18.3419168298212,-334.263395753412)) ;
#45774 = CARTESIAN_POINT('Ctrl Pts',(-3.00944375969563,-18.320898361752,-334.265088856315)) ;
#45775 = CARTESIAN_POINT('Ctrl Pts',(-3.26469715371016,-18.2770959927701,
-334.268414965052)) ;
#45776 = CARTESIAN_POINT('Ctrl Pts',(-3.38908972751508,-18.2544393559275,
-334.270047051673)) ;
#45777 = CARTESIAN_POINT('Ctrl Pts',(-3.66606851802552,-18.2010621850121,
-334.273706590879)) ;
#45778 = CARTESIAN_POINT('Ctrl Pts',(-3.81851942844445,-18.1696899345628,
-334.275738168226)) ;
#45779 = CARTESIAN_POINT('Ctrl Pts',(-4.66322470512088,-17.9847607222305,
-334.287089683705)) ;
#45780 = CARTESIAN_POINT('Ctrl Pts',(-5.34663356926141,-17.7935601915349,
-334.296654972771)) ;
#45781 = CARTESIAN_POINT('Ctrl Pts',(-6.28579369319399,-17.4717993665789,
-334.31001829902)) ;
#45782 = CARTESIAN_POINT('Ctrl Pts',(-6.55202096753423,-17.3737156939757,
-334.313828228738)) ;
#45783 = CARTESIAN_POINT('Ctrl Pts',(-6.98223753741354,-17.2039192596352,
-334.319973746453)) ;
#45784 = CARTESIAN_POINT('Ctrl Pts',(-7.1476219923382,-17.1358682000654,-334.322333296239)) ;
#45785 = CARTESIAN_POINT('Ctrl Pts',(-7.3860610225564,-17.0337046583356,-334.325718198654)) ;
#45786 = CARTESIAN_POINT('Ctrl Pts',(-7.45991707887951,-17.0014890235164,
-334.326764268105)) ;
#45787 = CARTESIAN_POINT('Ctrl Pts',(-7.59424086944535,-16.9418538772457,
-334.328660804968)) ;
#45788 = CARTESIAN_POINT('Ctrl Pts',(-7.65477553867067,-16.9145889287314,
-334.329513108642)) ;
#45789 = CARTESIAN_POINT('Ctrl Pts',(-7.80415937277042,-16.8463399441307,
-334.331611260977)) ;
#45790 = CARTESIAN_POINT('Ctrl Pts',(-7.8928332868889,-16.8049771131737,-334.332852387202)) ;
#45791 = CARTESIAN_POINT('Ctrl Pts',(-8.28021454280187,-16.6205367575039,
-334.338263290012)) ;
#45792 = CARTESIAN_POINT('Ctrl Pts',(-8.57539026262081,-16.4701814752492,
-334.342358192938)) ;
#45793 = CARTESIAN_POINT('Ctrl Pts',(-9.3409387196988,-16.0540679539547,-334.353067645324)) ;
#45794 = CARTESIAN_POINT('Ctrl Pts',(-9.80400883300223,-15.775539463952,-334.359642782408)) ;
#45795 = CARTESIAN_POINT('Ctrl Pts',(-10.3826217124048,-15.3921853306752,
-334.368230764424)) ;
#45796 = CARTESIAN_POINT('Ctrl Pts',(-10.5099047488373,-15.3055579767557,
-334.370143498812)) ;
#45797 = CARTESIAN_POINT('Ctrl Pts',(-10.8193306280354,-15.0892863163607,
-334.374858500856)) ;
#45798 = CARTESIAN_POINT('Ctrl Pts',(-11.0002373504479,-14.9579161232912,
-334.377671776257)) ;
#45799 = CARTESIAN_POINT('Ctrl Pts',(-11.2858399385413,-14.742534190098,-334.382214329645)) ;
#45800 = CARTESIAN_POINT('Ctrl Pts',(-11.3920738375009,-14.6605985922271,
-334.383927008033)) ;
#45801 = CARTESIAN_POINT('Ctrl Pts',(-11.5959872731738,-14.4997703713686,
-334.387260711737)) ;
#45802 = CARTESIAN_POINT('Ctrl Pts',(-11.6937730282488,-14.4210240265024,
-334.388880476053)) ;
#45803 = CARTESIAN_POINT('Ctrl Pts',(-11.9077721896485,-14.2450837319193,
-334.392472689701)) ;
#45804 = CARTESIAN_POINT('Ctrl Pts',(-12.0236098740814,-14.1474469271071,
-334.394448735454)) ;
#45805 = CARTESIAN_POINT('Ctrl Pts',(-12.4968342514946,-13.7385669542848,
-334.402652056966)) ;
#45806 = CARTESIAN_POINT('Ctrl Pts',(-12.8434332773064,-13.4151148923754,
-334.408978375996)) ;
#45807 = CARTESIAN_POINT('Ctrl Pts',(-13.498746496785,-12.7548654431428,-334.421484800521)) ;
#45808 = CARTESIAN_POINT('Ctrl Pts',(-13.8081664109825,-12.4192306423428,
-334.427656766833)) ;
#45809 = CARTESIAN_POINT('Ctrl Pts',(-14.2565399962579,-11.8953750017877,
-334.436865522598)) ;
#45810 = CARTESIAN_POINT('Ctrl Pts',(-14.4048241148071,-11.7153711717295,
-334.439957907253)) ;
#45811 = CARTESIAN_POINT('Ctrl Pts',(-14.6043070908721,-11.4637013278624,
-334.444158313241)) ;
#45812 = CARTESIAN_POINT('Ctrl Pts',(-14.6584456478166,-11.3943935757637,
-334.445302506692)) ;
#45813 = CARTESIAN_POINT('Ctrl Pts',(-14.7482570584799,-11.2777182465074,
-334.447205892481)) ;
#45814 = CARTESIAN_POINT('Ctrl Pts',(-14.7841990102298,-11.2305598592307,
-334.447968969192)) ;
#45815 = CARTESIAN_POINT('Ctrl Pts',(-14.8704460065605,-11.1162661242848,
-334.449803283974)) ;
#45816 = CARTESIAN_POINT('Ctrl Pts',(-14.9205230524449,-11.048960532472,-334.450871234164)) ;
#45817 = CARTESIAN_POINT('Ctrl Pts',(-15.0826689722672,-10.8279171632307,
-334.454342553687)) ;
#45818 = CARTESIAN_POINT('Ctrl Pts',(-15.1928313830656,-10.6727957076851,
-334.456722311533)) ;
#45819 = CARTESIAN_POINT('Ctrl Pts',(-15.449534817977,-10.2992971383052,-334.462349586075)) ;
#45820 = CARTESIAN_POINT('Ctrl Pts',(-15.5938585115071,-10.0794456526334,
-334.465580725262)) ;
#45821 = CARTESIAN_POINT('Ctrl Pts',(-15.9223120742536,-9.55515626982791,
-334.473165346432)) ;
#45822 = CARTESIAN_POINT('Ctrl Pts',(-16.1024580766535,-9.24834455357784,
-334.477511918964)) ;
#45823 = CARTESIAN_POINT('Ctrl Pts',(-16.4031146215664,-8.70084141298767,
-334.485205579039)) ;
#45824 = CARTESIAN_POINT('Ctrl Pts',(-16.5274143295523,-8.4623510826058,-334.488536427741)) ;
#45825 = CARTESIAN_POINT('Ctrl Pts',(-16.7407702828393,-8.03034504475609,
-334.494562262328)) ;
#45826 = CARTESIAN_POINT('Ctrl Pts',(-16.8317598321595,-7.83783719699524,
-334.497244654576)) ;
#45827 = CARTESIAN_POINT('Ctrl Pts',(-16.9738807287608,-7.52325536951615,
-334.50163141387)) ;
#45828 = CARTESIAN_POINT('Ctrl Pts',(-17.0270533269511,-7.40212491718791,
-334.50332129445)) ;
#45829 = CARTESIAN_POINT('Ctrl Pts',(-17.1285734497884,-7.16397234138079,
-334.506646452178)) ;
#45830 = CARTESIAN_POINT('Ctrl Pts',(-17.177027451193,-7.0470033361435,-334.508280869247)) ;
#45831 = CARTESIAN_POINT('Ctrl Pts',(-17.2826559256686,-6.78445020123704,
-334.511952824053)) ;
#45832 = CARTESIAN_POINT('Ctrl Pts',(-17.3391947607239,-6.63862073991387,
-334.513994584264)) ;
#45833 = CARTESIAN_POINT('Ctrl Pts',(-17.6452034078317,-5.81874989867252,
-334.525484348613)) ;
#45834 = CARTESIAN_POINT('Ctrl Pts',(-17.8572104796468,-5.13138179749463,
-334.535184913434)) ;
#45835 = CARTESIAN_POINT('Ctrl Pts',(-18.0948060746764,-4.16519082095492,
-334.54857548798)) ;
#45836 = CARTESIAN_POINT('Ctrl Pts',(-18.1547807037349,-3.89547934922758,
-334.552284097521)) ;
#45837 = CARTESIAN_POINT('Ctrl Pts',(-18.2430550491769,-3.45201155716157,
-334.558290187986)) ;
#45838 = CARTESIAN_POINT('Ctrl Pts',(-18.2749422013507,-3.27901342508881,
-334.560610426075)) ;
#45839 = CARTESIAN_POINT('Ctrl Pts',(-18.3177673711693,-3.02660146436936,
-334.563950611575)) ;
#45840 = CARTESIAN_POINT('Ctrl Pts',(-18.3306571591814,-2.94752879965032,
-334.564990553045)) ;
#45841 = CARTESIAN_POINT('Ctrl Pts',(-18.353306776474,-2.80268626697792,-334.566882154935)) ;
#45842 = CARTESIAN_POINT('Ctrl Pts',(-18.3632258551222,-2.73694284368088,
-334.567735571055)) ;
#45843 = CARTESIAN_POINT('Ctrl Pts',(-18.3869856787266,-2.57351709098916,
-334.569845038344)) ;
#45844 = CARTESIAN_POINT('Ctrl Pts',(-18.4004013739677,-2.47577500698039,
-334.5710962358)) ;
#45845 = CARTESIAN_POINT('Ctrl Pts',(-18.4569666177143,-2.03777317124503,
-334.576664774228)) ;
#45846 = CARTESIAN_POINT('Ctrl Pts',(-18.4914615690006,-1.69646289845218,
-334.580901805232)) ;
#45847 = CARTESIAN_POINT('Ctrl Pts',(-18.546601632436,-0.942619601587035,
-334.590187354682)) ;
#45848 = CARTESIAN_POINT('Ctrl Pts',(-18.5629768743386,-0.529956224781748,
-334.595223777141)) ;
#45849 = CARTESIAN_POINT('Ctrl Pts',(-18.5673349395481,0.161046040277517,
-334.603728896662)) ;
#45850 = CARTESIAN_POINT('Ctrl Pts',(-18.5628386078489,0.439186823947205,
-334.607171077334)) ;
#45851 = CARTESIAN_POINT('Ctrl Pts',(-18.5436811086748,0.934795978556484,
-334.613370065815)) ;
#45852 = CARTESIAN_POINT('Ctrl Pts',(-18.5314366423763,1.15230564973967,-334.616113032938)) ;
#45853 = CARTESIAN_POINT('Ctrl Pts',(-18.5055454482277,1.50233689082579,-334.620571872066)) ;
#45854 = CARTESIAN_POINT('Ctrl Pts',(-18.4942951810996,1.63501503434382,-334.622272293172)) ;
#45855 = CARTESIAN_POINT('Ctrl Pts',(-18.4696155105787,1.89306574802085,-334.625600896314)) ;
#45856 = CARTESIAN_POINT('Ctrl Pts',(-18.4563342380763,2.01844531107866,-334.627228028078)) ;
#45857 = CARTESIAN_POINT('Ctrl Pts',(-18.4205569663601,2.32623217401537,-334.631247166166)) ;
#45858 = CARTESIAN_POINT('Ctrl Pts',(-18.3966276075011,2.50845920609918,-334.633648243915)) ;
#45859 = CARTESIAN_POINT('Ctrl Pts',(-18.277206622158,3.32389338748949,-334.644486639968)) ;
#45860 = CARTESIAN_POINT('Ctrl Pts',(-18.1516993285938,3.95225948531527,-334.653110232385)) ;
#45861 = CARTESIAN_POINT('Ctrl Pts',(-17.9171599939278,4.87515640878925,-334.665934987984)) ;
#45862 = CARTESIAN_POINT('Ctrl Pts',(-17.8327363118529,5.17545053380942,-334.670130313629)) ;
#45863 = CARTESIAN_POINT('Ctrl Pts',(-17.6849378879217,5.65449911082292,-334.676799255836)) ;
#45864 = CARTESIAN_POINT('Ctrl Pts',(-17.6263199943303,5.83465782853139,-334.679301578091)) ;
#45865 = CARTESIAN_POINT('Ctrl Pts',(-17.5383327709844,6.0916449256034,-334.682848012174)) ;
#45866 = CARTESIAN_POINT('Ctrl Pts',(-17.5111943223633,6.16922423934497,-334.68391555763)) ;
#45867 = CARTESIAN_POINT('Ctrl Pts',(-17.4612960013028,6.30888364768524,-334.685830182909)) ;
#45868 = CARTESIAN_POINT('Ctrl Pts',(-17.4387180028674,6.37102702394005,-334.6866793772)) ;
#45869 = CARTESIAN_POINT('Ctrl Pts',(-17.3828101705274,6.52238296149466,-334.688741606875)) ;
#45870 = CARTESIAN_POINT('Ctrl Pts',(-17.3491249463938,6.61146220988443,-334.689950341215)) ;
#45871 = CARTESIAN_POINT('Ctrl Pts',(-17.2083728990571,6.97519147283076,-334.694872318711)) ;
#45872 = CARTESIAN_POINT('Ctrl Pts',(-17.0954574713869,7.24753257978813,-334.698526475989)) ;
#45873 = CARTESIAN_POINT('Ctrl Pts',(-16.7449739859308,8.03904372989135,-334.709185342693)) ;
#45874 = CARTESIAN_POINT('Ctrl Pts',(-16.4898913497585,8.55007966398541,-334.716125255647)) ;
#45875 = CARTESIAN_POINT('Ctrl Pts',(-16.1346040966126,9.18662362269907,-334.725139648184)) ;
#45876 = CARTESIAN_POINT('Ctrl Pts',(-16.0557774060232,9.32370713590794,-334.727102977928)) ;
#45877 = CARTESIAN_POINT('Ctrl Pts',(-15.8592529973868,9.65558831335999,-334.731917893013)) ;
#45878 = CARTESIAN_POINT('Ctrl Pts',(-15.7397061963683,9.84926088056226,-334.7347805987)) ;
#45879 = CARTESIAN_POINT('Ctrl Pts',(-15.5436941048321,10.1541253151516,-334.739382018417)) ;
#45880 = CARTESIAN_POINT('Ctrl Pts',(-15.4695249852774,10.2667659954944,-334.741103306113)) ;
#45881 = CARTESIAN_POINT('Ctrl Pts',(-15.3233469350836,10.4835859113985,-334.744459293243)) ;
#45882 = CARTESIAN_POINT('Ctrl Pts',(-15.2514862958781,10.5878562781614,-334.746092773423)) ;
#45883 = CARTESIAN_POINT('Ctrl Pts',(-15.0753970175753,10.8378503561383,-334.750057271545)) ;
#45884 = CARTESIAN_POINT('Ctrl Pts',(-14.9701149257459,10.9828163300826,-334.752396439518)) ;
#45885 = CARTESIAN_POINT('Ctrl Pts',(-14.3655955815914,11.7903509726719,-334.765652954175)) ;
#45886 = CARTESIAN_POINT('Ctrl Pts',(-13.8244871909281,12.4203966440916,-334.776914533803)) ;
#45887 = CARTESIAN_POINT('Ctrl Pts',(-13.1014090935313,13.1563077242409,-334.790746377223)) ;
#45888 = CARTESIAN_POINT('Ctrl Pts',(-12.95740392087,13.2981591578323,-334.793444219881)) ;
#45889 = CARTESIAN_POINT('Ctrl Pts',(-12.7074064393077,13.5365006882383,-334.798012809579)) ;
#45890 = CARTESIAN_POINT('Ctrl Pts',(-12.602560414978,13.6341666556337,-334.799895507527)) ;
#45891 = CARTESIAN_POINT('Ctrl Pts',(-12.4414866794291,13.7807641648348,-334.802730783084)) ;
#45892 = CARTESIAN_POINT('Ctrl Pts',(-12.3860775970797,13.8305868834271,-334.803696054865)) ;
#45893 = CARTESIAN_POINT('Ctrl Pts',(-12.2791137743815,13.9256082389218,-334.805538909772)) ;
#45894 = CARTESIAN_POINT('Ctrl Pts',(-12.2276057249237,13.9708574588943,-334.80641720435)) ;
#45895 = CARTESIAN_POINT('Ctrl Pts',(-12.0912680675626,14.0892969497332,-334.808719627033)) ;
#45896 = CARTESIAN_POINT('Ctrl Pts',(-12.0060244345187,14.1620065440826,-334.810136693374)) ;
#45897 = CARTESIAN_POINT('Ctrl Pts',(-11.8106733596294,14.3256021300721,-334.813339530063)) ;
#45898 = CARTESIAN_POINT('Ctrl Pts',(-11.7001651441998,14.4159986571247,-334.81511974059)) ;
#45899 = CARTESIAN_POINT('Ctrl Pts',(-11.3129673514627,14.7253440942672,-334.821266630856)) ;
#45900 = CARTESIAN_POINT('Ctrl Pts',(-11.031087114766,14.9376740724118,-334.825584898947)) ;
#45901 = CARTESIAN_POINT('Ctrl Pts',(-10.6331662647779,15.2200039204554,-334.831560752741)) ;
#45902 = CARTESIAN_POINT('Ctrl Pts',(-10.5221549149392,15.2969604853562,-334.833215232113)) ;
#45903 = CARTESIAN_POINT('Ctrl Pts',(-10.0114837144603,15.6427844347577,-334.840782520056)) ;
#45904 = CARTESIAN_POINT('Ctrl Pts',(-9.60229484780592,15.8972464049429,-334.846730793534)) ;
#45905 = CARTESIAN_POINT('Ctrl Pts',(-9.05209245154869,16.2103992740447,-334.854703446733)) ;
#45906 = CARTESIAN_POINT('Ctrl Pts',(-8.91959807017974,16.2836787169063,-334.856620955008)) ;
#45907 = CARTESIAN_POINT('Ctrl Pts',(-8.67563934037428,16.4147354267462,-334.860149937448)) ;
#45908 = CARTESIAN_POINT('Ctrl Pts',(-8.5644567821932,16.4730184564934,-334.861757608175)) ;
#45909 = CARTESIAN_POINT('Ctrl Pts',(-8.33321214612718,16.5912652568681,-334.865100991801)) ;
#45910 = CARTESIAN_POINT('Ctrl Pts',(-8.21307371371956,16.6510638580455,-334.866837788918)) ;
#45911 = CARTESIAN_POINT('Ctrl Pts',(-7.89090322448729,16.8070883332038,-334.871495187783)) ;
#45912 = CARTESIAN_POINT('Ctrl Pts',(-7.68776226443511,16.9009728424642,-334.874431930134)) ;
#45913 = CARTESIAN_POINT('Ctrl Pts',(-7.34187373136741,17.0533035043484,-334.879429125121)) ;
#45914 = CARTESIAN_POINT('Ctrl Pts',(-7.20000472379042,17.1136846470925,-334.881477803015)) ;
#45915 = CARTESIAN_POINT('Ctrl Pts',(-6.55638293432096,17.3781977745533,-334.890760756644)) ;
#45916 = CARTESIAN_POINT('Ctrl Pts',(-6.04659468888901,17.562078631726,-334.89809085744)) ;
#45917 = CARTESIAN_POINT('Ctrl Pts',(-5.21517692005276,17.8214714518222,-334.909787442976)) ;
#45918 = CARTESIAN_POINT('Ctrl Pts',(-4.89830028389441,17.911157699109,-334.914184676779)) ;
#45919 = CARTESIAN_POINT('Ctrl Pts',(-4.48448268482471,18.0164776857446,-334.919784517542)) ;
#45920 = CARTESIAN_POINT('Ctrl Pts',(-4.38957009510065,18.0398372379562,-334.921059175655)) ;
#45921 = CARTESIAN_POINT('Ctrl Pts',(-4.22989830484183,18.0778003623423,-334.923184703913)) ;
#45922 = CARTESIAN_POINT('Ctrl Pts',(-4.1652373305955,18.0928080635579,-334.924040221036)) ;
#45923 = CARTESIAN_POINT('Ctrl Pts',(-4.02185386386184,18.1252777304896,-334.925925175342)) ;
#45924 = CARTESIAN_POINT('Ctrl Pts',(-3.94309544245242,18.1425742292935,-334.926952725404)) ;
#45925 = CARTESIAN_POINT('Ctrl Pts',(-3.68894562083752,18.1966561299096,-334.930246733325)) ;
#45926 = CARTESIAN_POINT('Ctrl Pts',(-3.51313330886312,18.2314154320961,-334.932492046634)) ;
#45927 = CARTESIAN_POINT('Ctrl Pts',(-3.05682923452235,18.3147842117468,-334.938260883452)) ;
#45928 = CARTESIAN_POINT('Ctrl Pts',(-2.7756733597146,18.3594979099268,-334.941758769023)) ;
#45929 = CARTESIAN_POINT('Ctrl Pts',(-1.79347841549302,18.492623135642,-334.95390957906)) ;
#45930 = CARTESIAN_POINT('Ctrl Pts',(-1.08850959084819,18.5474748060651,-334.962531681146)) ;
#45931 = CARTESIAN_POINT('Ctrl Pts',(-0.226137140071919,18.5652284470579,
-334.973384166821)) ;
#45932 = CARTESIAN_POINT('Ctrl Pts',(-0.0701043697563229,18.5664732941174,
-334.975358700397)) ;
#45933 = CARTESIAN_POINT('Ctrl Pts',(0.21244671517656,18.5651656009107,-334.978957065454)) ;
#45934 = CARTESIAN_POINT('Ctrl Pts',(0.338958649907062,18.5632867342027,-334.980576490627)) ;
#45935 = CARTESIAN_POINT('Ctrl Pts',(0.5978107187438,18.5567953701525,-334.983907868395)) ;
#45936 = CARTESIAN_POINT('Ctrl Pts',(0.730140633484629,18.5520599033789,-334.985620526827)) ;
#45937 = CARTESIAN_POINT('Ctrl Pts',(1.07581454084149,18.5359856258674,-334.990119884488)) ;
#45938 = CARTESIAN_POINT('Ctrl Pts',(1.28903312566806,18.5223792586798,-334.992920761094)) ;
#45939 = CARTESIAN_POINT('Ctrl Pts',(1.64543360628384,18.4934519580819,-334.997642786405)) ;
#45940 = CARTESIAN_POINT('Ctrl Pts',(1.78875779975869,18.4801396788161,-334.999552601963)) ;
#45941 = CARTESIAN_POINT('Ctrl Pts',(2.40423387420777,18.4157456621252,-335.007795697354)) ;
#45942 = CARTESIAN_POINT('Ctrl Pts',(2.87448468528685,18.3482251235911,-335.014204611253)) ;
#45943 = CARTESIAN_POINT('Ctrl Pts',(3.39848912335852,18.2523454008388,-335.021375768667)) ;
#45944 = CARTESIAN_POINT('Ctrl Pts',(3.45530234345666,18.2416755444744,-335.022153590786)) ;
#45945 = CARTESIAN_POINT('Ctrl Pts',(3.84219285405449,18.1671429414192,-335.027451132733)) ;
#45946 = CARTESIAN_POINT('Ctrl Pts',(4.17053313509686,18.0945898729303,-335.031951522119)) ;
#45947 = CARTESIAN_POINT('Ctrl Pts',(4.60649799103957,17.9857576252338,-335.037864328576)) ;
#45948 = CARTESIAN_POINT('Ctrl Pts',(4.71602109080528,17.9573507574365,-335.039344269852)) ;
#45949 = CARTESIAN_POINT('Ctrl Pts',(4.88515740810982,17.911827986345,-335.041617645744)) ;
#45950 = CARTESIAN_POINT('Ctrl Pts',(4.94495597873575,17.8954115654784,-335.042419047708)) ;
#45951 = CARTESIAN_POINT('Ctrl Pts',(5.07353742131262,17.8594185684256,-335.044136307057)) ;
#45952 = CARTESIAN_POINT('Ctrl Pts',(5.14229171559571,17.8397435378726,-335.045050889888)) ;
#45953 = CARTESIAN_POINT('Ctrl Pts',(5.33334117923825,17.7838757573816,-335.047584099105)) ;
#45954 = CARTESIAN_POINT('Ctrl Pts',(5.45537976069907,17.7468193442043,-335.049192929798)) ;
#45955 = CARTESIAN_POINT('Ctrl Pts',(5.74013998785896,17.6571384165459,-335.052934228669)) ;
#45956 = CARTESIAN_POINT('Ctrl Pts',(5.9025356937898,17.6035171672623,-335.055058112492)) ;
#45957 = CARTESIAN_POINT('Ctrl Pts',(6.55056128187799,17.37957074211,-335.063529007624)) ;
#45958 = CARTESIAN_POINT('Ctrl Pts',(7.02975633091527,17.1913309416564,-335.069789497846)) ;
#45959 = CARTESIAN_POINT('Ctrl Pts',(7.79878571541552,16.8516990447861,-335.080130829806)) ;
#45960 = CARTESIAN_POINT('Ctrl Pts',(8.09353731585515,16.7121354863115,-335.084166417869)) ;
#45961 = CARTESIAN_POINT('Ctrl Pts',(8.56364763437041,16.4741850441395,-335.090766887485)) ;
#45962 = CARTESIAN_POINT('Ctrl Pts',(8.74135166370509,16.3805862096651,-335.093300613804)) ;
#45963 = CARTESIAN_POINT('Ctrl Pts',(9.02029785367972,16.2278298594257,-335.097345867512)) ;
#45964 = CARTESIAN_POINT('Ctrl Pts',(9.12255836368312,16.1705647450697,-335.098843554123)) ;
#45965 = CARTESIAN_POINT('Ctrl Pts',(9.3349146132372,16.0489913487388,-335.101985472813)) ;
#45966 = CARTESIAN_POINT('Ctrl Pts',(9.44490399068585,15.984509460715,-335.103630943268)) ;
#45967 = CARTESIAN_POINT('Ctrl Pts',(9.71263952343891,15.8238196955139,-335.107681537368)) ;
#45968 = CARTESIAN_POINT('Ctrl Pts',(9.86963032907834,15.7263801706782,-335.110095728314)) ;
#45969 = CARTESIAN_POINT('Ctrl Pts',(10.608794353554,15.2521748694022,-335.121646920329)) ;
#45970 = CARTESIAN_POINT('Ctrl Pts',(11.171010492361,14.8453316983266,-335.131007608716)) ;
#45971 = CARTESIAN_POINT('Ctrl Pts',(11.7775881036003,14.3523759763163,-335.141526842396)) ;
#45972 = CARTESIAN_POINT('Ctrl Pts',(11.8456338819633,14.2962664932035,-335.142712793918)) ;
#45973 = CARTESIAN_POINT('Ctrl Pts',(12.159573251382,14.0336167525546,-335.148208226059)) ;
#45974 = CARTESIAN_POINT('Ctrl Pts',(12.400482178262,13.8212033954704,-335.152494796295)) ;
#45975 = CARTESIAN_POINT('Ctrl Pts',(12.7072422536448,13.5362480902016,-335.157985287618)) ;
#45976 = CARTESIAN_POINT('Ctrl Pts',(12.7781993768155,13.4692850136443,-335.159257552131)) ;
#45977 = CARTESIAN_POINT('Ctrl Pts',(12.8965263157421,13.3558418634424,-335.161380424814)) ;
#45978 = CARTESIAN_POINT('Ctrl Pts',(12.9441806394015,13.3096615472793,-335.162235651157)) ;
#45979 = CARTESIAN_POINT('Ctrl Pts',(13.0492654056539,13.2067289895713,-335.164121633935)) ;
#45980 = CARTESIAN_POINT('Ctrl Pts',(13.1065751819114,13.1498557123733,-335.165150484866)) ;
#45981 = CARTESIAN_POINT('Ctrl Pts',(13.290362555739,12.96507305494,-335.16845424268)) ;
#45982 = CARTESIAN_POINT('Ctrl Pts',(13.4153529347383,12.8356987352135,-335.170707832878)) ;
#45983 = CARTESIAN_POINT('Ctrl Pts',(13.7344153334279,12.4956933315431,-335.176506159499)) ;
#45984 = CARTESIAN_POINT('Ctrl Pts',(13.9255290044252,12.2823515155602,-335.180024946812)) ;
#45985 = CARTESIAN_POINT('Ctrl Pts',(14.5676699450911,11.5312615220473,-335.192138305371)) ;
#45986 = CARTESIAN_POINT('Ctrl Pts',(14.9930981765787,10.9724202655962,-335.200703778461)) ;
#45987 = CARTESIAN_POINT('Ctrl Pts',(15.4832365987254,10.2466653948714,-335.21172074007)) ;
#45988 = CARTESIAN_POINT('Ctrl Pts',(15.5785749733478,10.1011271131525,-335.213923475159)) ;
#45989 = CARTESIAN_POINT('Ctrl Pts',(15.7393503430648,9.84800479290957,-335.217747183199)) ;
#45990 = CARTESIAN_POINT('Ctrl Pts',(15.8057643995335,9.74105534921626,-335.219360550176)) ;
#45991 = CARTESIAN_POINT('Ctrl Pts',(15.9420061327822,9.51659716334298,-335.222742887616)) ;
#45992 = CARTESIAN_POINT('Ctrl Pts',(16.0116342319869,9.39897602189123,-335.224513243621)) ;
#45993 = CARTESIAN_POINT('Ctrl Pts',(16.1989391232153,9.0744435962426,-335.229392614435)) ;
#45994 = CARTESIAN_POINT('Ctrl Pts',(16.3139454326785,8.86602162089748,-335.232520691805)) ;
#45995 = CARTESIAN_POINT('Ctrl Pts',(16.7484870171236,8.04141858283041,-335.244864565451)) ;
#45996 = CARTESIAN_POINT('Ctrl Pts',(17.0373744834704,7.40972974153398,-335.254273306065)) ;
#45997 = CARTESIAN_POINT('Ctrl Pts',(17.4028773753953,6.47533833914841,-335.267736308515)) ;
#45998 = CARTESIAN_POINT('Ctrl Pts',(17.5083268686601,6.1845483665394,-335.271861169753)) ;
#45999 = CARTESIAN_POINT('Ctrl Pts',(17.6369936157038,5.80001833959915,-335.27717671423)) ;
#46000 = CARTESIAN_POINT('Ctrl Pts',(17.6668141086649,5.7085406040964,-335.278431005129)) ;
#46001 = CARTESIAN_POINT('Ctrl Pts',(17.7159539974586,5.55372465704394,-335.280534038441)) ;
#46002 = CARTESIAN_POINT('Ctrl Pts',(17.7356480328786,5.49050748954687,-335.281387182829)) ;
#46003 = CARTESIAN_POINT('Ctrl Pts',(17.7788443887502,5.34919089565252,-335.28328137853)) ;
#46004 = CARTESIAN_POINT('Ctrl Pts',(17.8021710712351,5.27103938638333,-335.284320381813)) ;
#46005 = CARTESIAN_POINT('Ctrl Pts',(17.8767873112735,5.01490601589579,-335.287701252093)) ;
#46006 = CARTESIAN_POINT('Ctrl Pts',(17.9259285651468,4.83630977255176,-335.290020416263)) ;
#46007 = CARTESIAN_POINT('Ctrl Pts',(18.1401181458702,4.00970639251432,-335.300632559098)) ;
#46008 = CARTESIAN_POINT('Ctrl Pts',(18.272754612018,3.35381502164704,-335.308728569246)) ;
#46009 = CARTESIAN_POINT('Ctrl Pts',(18.4216534090388,2.33783205182358,-335.321397904403)) ;
#46010 = CARTESIAN_POINT('Ctrl Pts',(18.4633231901178,1.98203657134443,-335.32585448747)) ;
#46011 = CARTESIAN_POINT('Ctrl Pts',(18.50833031021,1.46987710301421,-335.332344842534)) ;
#46012 = CARTESIAN_POINT('Ctrl Pts',(18.5200261629321,1.3143288773807,-335.334325667501)) ;
#46013 = CARTESIAN_POINT('Ctrl Pts',(18.5375033057871,1.03482537456268,-335.33790482575)) ;
#46014 = CARTESIAN_POINT('Ctrl Pts',(18.5440046642734,0.910924436206806,-335.339498394796)) ;
#46015 = CARTESIAN_POINT('Ctrl Pts',(18.5554770703173,0.640513505423163,-335.342992291914)) ;
#46016 = CARTESIAN_POINT('Ctrl Pts',(18.559955810908,0.493990962892338,-335.344895693779)) ;
#46017 = CARTESIAN_POINT('Ctrl Pts',(18.5683104299641,0.0476165308628815,
-335.350725534762)) ;
#46018 = CARTESIAN_POINT('Ctrl Pts',(18.5666574562054,-0.252289148872367,
-335.354685981898)) ;
#46019 = CARTESIAN_POINT('Ctrl Pts',(18.5543991293277,-0.664386315309379,
-335.360177154725)) ;
#46020 = CARTESIAN_POINT('Ctrl Pts',(18.5500365024344,-0.776710141285842,
-335.361678784497)) ;
#46021 = CARTESIAN_POINT('Ctrl Pts',(18.5446545934131,-0.888979984870959,
-335.363183819487)) ;
#46022 = CARTESIAN_POINT('Origin',(0.,0.,-315.477129595899)) ;
#46023 = CARTESIAN_POINT('',(18.5446545937554,-0.888979977731322,-337.158465839576)) ;
#46024 = CARTESIAN_POINT('',(18.544654593745,-0.888979977948828,-336.86323988221)) ;
#46025 = CARTESIAN_POINT('',(18.544654593745,-0.888979977948782,-315.477129595899)) ;
#46026 = CARTESIAN_POINT('Ctrl Pts',(18.5446545937658,-0.888979977513935,
-337.158465839576)) ;
#46027 = CARTESIAN_POINT('Ctrl Pts',(18.5567562697993,-0.636531769767257,
-337.155292643735)) ;
#46028 = CARTESIAN_POINT('Ctrl Pts',(18.5637020684296,-0.383857592640776,
-337.152163036735)) ;
#46029 = CARTESIAN_POINT('Ctrl Pts',(18.5663697796789,-0.0061192947651607,
-337.147512304642)) ;
#46030 = CARTESIAN_POINT('Ctrl Pts',(18.5659901745631,0.118882716158257,-337.145977908322)) ;
#46031 = CARTESIAN_POINT('Ctrl Pts',(18.5597324315834,0.595244166917408,-337.14013704646)) ;
#46032 = CARTESIAN_POINT('Ctrl Pts',(18.5451417327675,0.946415148907194,-337.135843235536)) ;
#46033 = CARTESIAN_POINT('Ctrl Pts',(18.5015418685101,1.5690214974659,-337.128158002302)) ;
#46034 = CARTESIAN_POINT('Ctrl Pts',(18.4764975206981,1.84063005911752,-337.124781065078)) ;
#46035 = CARTESIAN_POINT('Ctrl Pts',(18.4210302448419,2.32515666672852,-337.118683393839)) ;
#46036 = CARTESIAN_POINT('Ctrl Pts',(18.3928741750221,2.53828449067063,-337.115975760661)) ;
#46037 = CARTESIAN_POINT('Ctrl Pts',(18.341368806701,2.88206284969703,-337.111558877197)) ;
#46038 = CARTESIAN_POINT('Ctrl Pts',(18.3203086444005,3.01303619058971,-337.109864509858)) ;
#46039 = CARTESIAN_POINT('Ctrl Pts',(18.2764450857783,3.26833732425785,-337.106537758219)) ;
#46040 = CARTESIAN_POINT('Ctrl Pts',(18.2537720555308,3.3926802869411,-337.104906313498)) ;
#46041 = CARTESIAN_POINT('Ctrl Pts',(18.2003958829717,3.66936466357962,-337.101250644211)) ;
#46042 = CARTESIAN_POINT('Ctrl Pts',(18.1690461305778,3.82157165818196,-337.099222327372)) ;
#46043 = CARTESIAN_POINT('Ctrl Pts',(17.9836530903229,4.66776813269176,-337.087850924263)) ;
#46044 = CARTESIAN_POINT('Ctrl Pts',(17.7917609371563,5.35285647313084,-337.078260924487)) ;
#46045 = CARTESIAN_POINT('Ctrl Pts',(17.4692148511989,6.29294280349286,-337.064882584481)) ;
#46046 = CARTESIAN_POINT('Ctrl Pts',(17.3712584096113,6.55850426742939,-337.06108178205)) ;
#46047 = CARTESIAN_POINT('Ctrl Pts',(17.2016573048195,6.98780170118767,-337.05494875179)) ;
#46048 = CARTESIAN_POINT('Ctrl Pts',(17.1336522304962,7.15292584092232,-337.052592671772)) ;
#46049 = CARTESIAN_POINT('Ctrl Pts',(17.0315351592198,7.39106188012024,-337.04921168884)) ;
#46050 = CARTESIAN_POINT('Ctrl Pts',(16.9993133661875,7.46487312000773,-337.048166133859)) ;
#46051 = CARTESIAN_POINT('Ctrl Pts',(16.9396529773855,7.59914895596636,-337.046270050309)) ;
#46052 = CARTESIAN_POINT('Ctrl Pts',(16.9123684159812,7.65968030700843,-337.045417691896)) ;
#46053 = CARTESIAN_POINT('Ctrl Pts',(16.8440486129559,7.80910438499991,-337.043318719734)) ;
#46054 = CARTESIAN_POINT('Ctrl Pts',(16.802633799864,7.89782137043411,-337.04207683876)) ;
#46055 = CARTESIAN_POINT('Ctrl Pts',(16.6220771512405,8.27675260561849,-337.03678330221)) ;
#46056 = CARTESIAN_POINT('Ctrl Pts',(16.4761032282204,8.56365026456009,-337.032801961933)) ;
#46057 = CARTESIAN_POINT('Ctrl Pts',(16.2777037036849,8.92971426445733,-337.027682521909)) ;
#46058 = CARTESIAN_POINT('Ctrl Pts',(16.2320280035139,9.01247477726652,-337.026522515515)) ;
#46059 = CARTESIAN_POINT('Ctrl Pts',(16.0139482573076,9.40058073245432,-337.021064478593)) ;
#46060 = CARTESIAN_POINT('Ctrl Pts',(15.8335481805643,9.70135087926533,-337.016779893667)) ;
#46061 = CARTESIAN_POINT('Ctrl Pts',(15.4975674229055,10.2271506263078,-337.009096999331)) ;
#46062 = CARTESIAN_POINT('Ctrl Pts',(15.3453276903723,10.4541916813073,-337.005712895873)) ;
#46063 = CARTESIAN_POINT('Ctrl Pts',(15.0643199055576,10.8538983379358,-336.999604145336)) ;
#46064 = CARTESIAN_POINT('Ctrl Pts',(14.9374550057992,11.0278411787421,-336.996892683186)) ;
#46065 = CARTESIAN_POINT('Ctrl Pts',(14.7275511370488,11.3053679161451,-336.992471453234)) ;
#46066 = CARTESIAN_POINT('Ctrl Pts',(14.6463759817764,11.4103363996441,-336.990776634408)) ;
#46067 = CARTESIAN_POINT('Ctrl Pts',(14.4857356215429,11.613523216645,-336.987450264637)) ;
#46068 = CARTESIAN_POINT('Ctrl Pts',(14.4063792906671,11.7118185471072,-336.985819667026)) ;
#46069 = CARTESIAN_POINT('Ctrl Pts',(14.208070037954,11.9523903358009,-336.981775088934)) ;
#46070 = CARTESIAN_POINT('Ctrl Pts',(14.087976904432,12.0937089231611,-336.979351759017)) ;
#46071 = CARTESIAN_POINT('Ctrl Pts',(13.6481913655868,12.5957810650133,-336.97057167981)) ;
#46072 = CARTESIAN_POINT('Ctrl Pts',(13.3165973381164,12.9458511187139,-336.964120467453)) ;
#46073 = CARTESIAN_POINT('Ctrl Pts',(12.6108566173104,13.6350749963717,-336.950844779163)) ;
#46074 = CARTESIAN_POINT('Ctrl Pts',(12.2357395372514,13.9726752301543,-336.944022257355)) ;
#46075 = CARTESIAN_POINT('Ctrl Pts',(11.7216064221612,14.3987885259726,-336.935165816693)) ;
#46076 = CARTESIAN_POINT('Ctrl Pts',(11.5945019994838,14.5013341341481,-336.93301473412)) ;
#46077 = CARTESIAN_POINT('Ctrl Pts',(11.4046746967651,14.6503920162474,-336.929868240186)) ;
#46078 = CARTESIAN_POINT('Ctrl Pts',(11.342984852882,14.6982068912601,-336.928855816822)) ;
#46079 = CARTESIAN_POINT('Ctrl Pts',(11.2277571357391,14.7863606840983,-336.92698495313)) ;
#46080 = CARTESIAN_POINT('Ctrl Pts',(11.1742988899914,14.8268013032702,-336.926125126086)) ;
#46081 = CARTESIAN_POINT('Ctrl Pts',(11.0521730600659,14.9181525989152,-336.924178265233)) ;
#46082 = CARTESIAN_POINT('Ctrl Pts',(10.9833704833917,14.9688803577792,-336.923093772265)) ;
#46083 = CARTESIAN_POINT('Ctrl Pts',(10.6789273384906,15.1901154886566,-336.918343633572)) ;
#46084 = CARTESIAN_POINT('Ctrl Pts',(10.4396486137258,15.3555473752115,-336.914736844778)) ;
#46085 = CARTESIAN_POINT('Ctrl Pts',(10.0746492802615,15.5954233763319,-336.909357438523)) ;
#46086 = CARTESIAN_POINT('Ctrl Pts',(9.95177606831765,15.6741169297108,-336.907566836997)) ;
#46087 = CARTESIAN_POINT('Ctrl Pts',(9.42794367936804,16.0009598449627,-336.89999874063)) ;
#46088 = CARTESIAN_POINT('Ctrl Pts',(9.01853544827729,16.2352350196351,-336.894239840264)) ;
#46089 = CARTESIAN_POINT('Ctrl Pts',(8.33480329127769,16.5926351629743,-336.884678171299)) ;
#46090 = CARTESIAN_POINT('Ctrl Pts',(8.06562385307727,16.7251367367903,-336.88092859648)) ;
#46091 = CARTESIAN_POINT('Ctrl Pts',(7.6602864556012,16.9125989963316,-336.875278541703)) ;
#46092 = CARTESIAN_POINT('Ctrl Pts',(7.52649588348654,16.9725617697364,-336.87341316603)) ;
#46093 = CARTESIAN_POINT('Ctrl Pts',(7.27819199945763,17.0803341717333,-336.869948370651)) ;
#46094 = CARTESIAN_POINT('Ctrl Pts',(7.16388245636576,17.1285925370263,-336.868352235365)) ;
#46095 = CARTESIAN_POINT('Ctrl Pts',(6.90480067224838,17.2349225675018,-336.864731485817)) ;
#46096 = CARTESIAN_POINT('Ctrl Pts',(6.75976307380804,17.2923229011406,-336.862702340124)) ;
#46097 = CARTESIAN_POINT('Ctrl Pts',(6.28507108121731,17.4733029719652,-336.856054341685)) ;
#46098 = CARTESIAN_POINT('Ctrl Pts',(5.95262280313957,17.5893352915917,-336.851386464728)) ;
#46099 = CARTESIAN_POINT('Ctrl Pts',(4.97366137958809,17.9000806887025,-336.837652218947)) ;
#46100 = CARTESIAN_POINT('Ctrl Pts',(4.31958675082728,18.0690720154357,-336.828474708222)) ;
#46101 = CARTESIAN_POINT('Ctrl Pts',(3.4763905016348,18.2385151308603,-336.81703926607)) ;
#46102 = CARTESIAN_POINT('Ctrl Pts',(3.29447959314486,18.2722502588086,-336.814596710105)) ;
#46103 = CARTESIAN_POINT('Ctrl Pts',(3.03172002294195,18.3169271429608,-336.811117675029)) ;
#46104 = CARTESIAN_POINT('Ctrl Pts',(2.95125608790527,18.330063660189,-336.810058919755)) ;
#46105 = CARTESIAN_POINT('Ctrl Pts',(2.80528283975242,18.352909112998,-336.808151796256)) ;
#46106 = CARTESIAN_POINT('Ctrl Pts',(2.73980333612965,18.3627983269661,-336.807301427291)) ;
#46107 = CARTESIAN_POINT('Ctrl Pts',(2.57900092377559,18.3862046808985,-336.80522493634)) ;
#46108 = CARTESIAN_POINT('Ctrl Pts',(2.48362310448242,18.399331092353,-336.804003282988)) ;
#46109 = CARTESIAN_POINT('Ctrl Pts',(2.08093738961163,18.4515626660339,-336.798880220109)) ;
#46110 = CARTESIAN_POINT('Ctrl Pts',(1.77277739324593,18.4837151674474,-336.795044236238)) ;
#46111 = CARTESIAN_POINT('Ctrl Pts',(0.907565020169588,18.5521517373054,-336.784365830641)) ;
#46112 = CARTESIAN_POINT('Ctrl Pts',(0.349471609057681,18.5710494802052,-336.7775769169)) ;
#46113 = CARTESIAN_POINT('Ctrl Pts',(-0.43592428748611,18.5622235053451,-336.767862016259)) ;
#46114 = CARTESIAN_POINT('Ctrl Pts',(-0.663158423480988,18.555494930888,-336.765033651854)) ;
#46115 = CARTESIAN_POINT('Ctrl Pts',(-1.07949910790506,18.5355089896144,-336.759803437191)) ;
#46116 = CARTESIAN_POINT('Ctrl Pts',(-1.26863640305428,18.5235248627216,-336.757409259633)) ;
#46117 = CARTESIAN_POINT('Ctrl Pts',(-1.58541793185425,18.4985783031037,-336.753363582959)) ;
#46118 = CARTESIAN_POINT('Ctrl Pts',(-1.71317115918243,18.487184582256,-336.751722286901)) ;
#46119 = CARTESIAN_POINT('Ctrl Pts',(-1.97216889210278,18.4613780488473,-336.748374004994)) ;
#46120 = CARTESIAN_POINT('Ctrl Pts',(-2.10339834486485,18.4468871342256,-336.74666659927)) ;
#46121 = CARTESIAN_POINT('Ctrl Pts',(-2.44437362391138,18.4055493676765,-336.7422014074)) ;
#46122 = CARTESIAN_POINT('Ctrl Pts',(-2.65383490751731,18.376516807677,-336.739429854847)) ;
#46123 = CARTESIAN_POINT('Ctrl Pts',(-3.15857874535579,18.2977463968594,-336.732685478952)) ;
#46124 = CARTESIAN_POINT('Ctrl Pts',(-3.45324271576011,18.244430851697,-336.728693087521)) ;
#46125 = CARTESIAN_POINT('Ctrl Pts',(-4.25515248535949,18.0792118150392,-336.717712723824)) ;
#46126 = CARTESIAN_POINT('Ctrl Pts',(-4.75919515028514,17.9531134708476,-336.710678590039)) ;
#46127 = CARTESIAN_POINT('Ctrl Pts',(-5.42193805271025,17.7574367696726,-336.701439981366)) ;
#46128 = CARTESIAN_POINT('Ctrl Pts',(-5.58590769350217,17.7065413971175,-336.699155829618)) ;
#46129 = CARTESIAN_POINT('Ctrl Pts',(-5.87075010631022,17.6137772209458,-336.695203185153)) ;
#46130 = CARTESIAN_POINT('Ctrl Pts',(-5.99193998127609,17.5729197956022,-336.693526391886)) ;
#46131 = CARTESIAN_POINT('Ctrl Pts',(-6.18028721615459,17.5072463003436,-336.690933260321)) ;
#46132 = CARTESIAN_POINT('Ctrl Pts',(-6.24773948238433,17.4832884341897,-336.690007186094)) ;
#46133 = CARTESIAN_POINT('Ctrl Pts',(-6.37332284432578,17.4378638346729,-336.688289022035)) ;
#46134 = CARTESIAN_POINT('Ctrl Pts',(-6.43148827095938,17.4164949924739,-336.687495671126)) ;
#46135 = CARTESIAN_POINT('Ctrl Pts',(-6.5953026184196,17.3553802612759,-336.685266860367)) ;
#46136 = CARTESIAN_POINT('Ctrl Pts',(-6.70069769891658,17.3149614798411,-336.683839407664)) ;
#46137 = CARTESIAN_POINT('Ctrl Pts',(-7.02358678683696,17.1877445697093,-336.679477887345)) ;
#46138 = CARTESIAN_POINT('Ctrl Pts',(-7.23981271987873,17.0977907015879,-336.67657328316)) ;
#46139 = CARTESIAN_POINT('Ctrl Pts',(-7.99392065307223,16.7671974887354,-336.666421941636)) ;
#46140 = CARTESIAN_POINT('Ctrl Pts',(-8.5219940652943,16.5050688491558,-336.659264380148)) ;
#46141 = CARTESIAN_POINT('Ctrl Pts',(-9.1768721728353,16.1401754037574,-336.649997126615)) ;
#46142 = CARTESIAN_POINT('Ctrl Pts',(-9.31601836366531,16.0602629715205,-336.648005517679)) ;
#46143 = CARTESIAN_POINT('Ctrl Pts',(-9.65188776211912,15.861537479519,-336.643135053198)) ;
#46144 = CARTESIAN_POINT('Ctrl Pts',(-9.84747445905211,15.740856237419,-336.640245020884)) ;
#46145 = CARTESIAN_POINT('Ctrl Pts',(-10.1545368813124,15.5434286267316,-336.635611046358)) ;
#46146 = CARTESIAN_POINT('Ctrl Pts',(-10.2675007687193,15.4690407151842,-336.63388499411)) ;
#46147 = CARTESIAN_POINT('Ctrl Pts',(-10.4844904167196,15.3227266391031,-336.630526590696)) ;
#46148 = CARTESIAN_POINT('Ctrl Pts',(-10.5886140457514,15.2509587728463,-336.628895536981)) ;
#46149 = CARTESIAN_POINT('Ctrl Pts',(-10.8144819938412,15.0918496596646,-336.625313969049)) ;
#46150 = CARTESIAN_POINT('Ctrl Pts',(-10.9359186805812,15.0040870921575,-336.623360232306)) ;
#46151 = CARTESIAN_POINT('Ctrl Pts',(-11.6525467406019,14.4728559637148,-336.611663134489)) ;
#46152 = CARTESIAN_POINT('Ctrl Pts',(-12.2217695931637,13.9954901206591,-336.601643618155)) ;
#46153 = CARTESIAN_POINT('Ctrl Pts',(-12.9589093723638,13.2979508370078,-336.587986986086)) ;
#46154 = CARTESIAN_POINT('Ctrl Pts',(-13.1527849684153,13.1062228143882,-336.584327958292)) ;
#46155 = CARTESIAN_POINT('Ctrl Pts',(-13.463676746494,12.784926317954,-336.578390382288)) ;
#46156 = CARTESIAN_POINT('Ctrl Pts',(-13.5832126386779,12.657853968376,-336.576089660141)) ;
#46157 = CARTESIAN_POINT('Ctrl Pts',(-13.7548502106752,12.4701634617688,-336.572771700365)) ;
#46158 = CARTESIAN_POINT('Ctrl Pts',(-13.8083793848541,12.4108637841577,-336.571734823991)) ;
#46159 = CARTESIAN_POINT('Ctrl Pts',(-13.9057904337165,12.3015413394571,-336.569845635621)) ;
#46160 = CARTESIAN_POINT('Ctrl Pts',(-13.9497891796328,12.2516247391718,-336.568991608613)) ;
#46161 = CARTESIAN_POINT('Ctrl Pts',(-14.0586333753049,12.1267944558571,-336.566876218597)) ;
#46162 = CARTESIAN_POINT('Ctrl Pts',(-14.1231493066189,12.0515961540475,-336.56561977761)) ;
#46163 = CARTESIAN_POINT('Ctrl Pts',(-14.4138022021324,11.7072783723535,-336.559938952931)) ;
#46164 = CARTESIAN_POINT('Ctrl Pts',(-14.6328706427724,11.4322858053713,-336.555599003202)) ;
#46165 = CARTESIAN_POINT('Ctrl Pts',(-15.2569942737539,10.6014820992475,-336.542837805108)) ;
#46166 = CARTESIAN_POINT('Ctrl Pts',(-15.6391277067598,10.0292064663032,-336.534474030605)) ;
#46167 = CARTESIAN_POINT('Ctrl Pts',(-16.097757337041,9.25217787662991,-336.52319229753)) ;
#46168 = CARTESIAN_POINT('Ctrl Pts',(-16.2036637890586,9.06542146414458,-336.520488169062)) ;
#46169 = CARTESIAN_POINT('Ctrl Pts',(-16.3697043533782,8.76041437548144,-336.516075554971)) ;
#46170 = CARTESIAN_POINT('Ctrl Pts',(-16.4318517381587,8.64328230715969,-336.514381899269)) ;
#46171 = CARTESIAN_POINT('Ctrl Pts',(-16.5507852195466,8.41320312227444,-336.511055624868)) ;
#46172 = CARTESIAN_POINT('Ctrl Pts',(-16.6076830542664,8.30032178143017,-336.509423935506)) ;
#46173 = CARTESIAN_POINT('Ctrl Pts',(-16.7319975258299,8.0472940513436,-336.505766510194)) ;
#46174 = CARTESIAN_POINT('Ctrl Pts',(-16.7988150144228,7.90686390211875,-336.503736666043)) ;
#46175 = CARTESIAN_POINT('Ctrl Pts',(-17.1608143969122,7.12074327833533,-336.492375538771)) ;
#46176 = CARTESIAN_POINT('Ctrl Pts',(-17.4205338990276,6.4593750599135,-336.482798126859)) ;
#46177 = CARTESIAN_POINT('Ctrl Pts',(-17.730023271277,5.51552875132217,-336.46942760497)) ;
#46178 = CARTESIAN_POINT('Ctrl Pts',(-17.8121321647762,5.2443045931346,-336.465622319275)) ;
#46179 = CARTESIAN_POINT('Ctrl Pts',(-17.93584988548,4.79913745501913,-336.459483175267)) ;
#46180 = CARTESIAN_POINT('Ctrl Pts',(-17.9812101117979,4.62628517669532,-336.457125410538)) ;
#46181 = CARTESIAN_POINT('Ctrl Pts',(-18.0433879899686,4.37460149887323,-336.453742539951)) ;
#46182 = CARTESIAN_POINT('Ctrl Pts',(-18.062198801569,4.29627314160134,-336.452696750144)) ;
#46183 = CARTESIAN_POINT('Ctrl Pts',(-18.095582908199,4.15316588925237,-336.450800445282)) ;
#46184 = CARTESIAN_POINT('Ctrl Pts',(-18.1103195698457,4.08842668559268,-336.44994809757)) ;
#46185 = CARTESIAN_POINT('Ctrl Pts',(-18.1459211819759,3.92805605074874,-336.447849461296)) ;
#46186 = CARTESIAN_POINT('Ctrl Pts',(-18.1663777533453,3.83233600343261,-336.446607900867)) ;
#46187 = CARTESIAN_POINT('Ctrl Pts',(-18.2508778676688,3.42105738117352,-336.441312804342)) ;
#46188 = CARTESIAN_POINT('Ctrl Pts',(-18.3074634740286,3.10402297325208,-336.437329661554)) ;
#46189 = CARTESIAN_POINT('Ctrl Pts',(-18.3699386717705,2.69235262795825,-336.432210067408)) ;
#46190 = CARTESIAN_POINT('Ctrl Pts',(-18.3833897152854,2.59892132656995,-336.43105169549)) ;
#46191 = CARTESIAN_POINT('Ctrl Pts',(-18.4434339071094,2.15803988468078,-336.425596431966)) ;
#46192 = CARTESIAN_POINT('Ctrl Pts',(-18.4808927472196,1.80941804718231,-336.421312987516)) ;
#46193 = CARTESIAN_POINT('Ctrl Pts',(-18.5299579981378,1.18739330582407,-336.413630369156)) ;
#46194 = CARTESIAN_POINT('Ctrl Pts',(-18.5454339069767,0.914399885724085,
-336.41024536525)) ;
#46195 = CARTESIAN_POINT('Ctrl Pts',(-18.5623115221588,0.425973134568299,
-336.404135161628)) ;
#46196 = CARTESIAN_POINT('Ctrl Pts',(-18.5660033562227,0.210668697880257,
-336.401423155009)) ;
#46197 = CARTESIAN_POINT('Ctrl Pts',(-18.5659161735629,-0.137358097947155,
-336.397001164568)) ;
#46198 = CARTESIAN_POINT('Ctrl Pts',(-18.5644600674199,-0.270061020512011,
-336.395306135838)) ;
#46199 = CARTESIAN_POINT('Ctrl Pts',(-18.5588407984291,-0.529045351700046,
-336.391979415567)) ;
#46200 = CARTESIAN_POINT('Ctrl Pts',(-18.5548110498324,-0.655322528790837,
-336.390348678161)) ;
#46201 = CARTESIAN_POINT('Ctrl Pts',(-18.5416858984054,-0.966838532375095,
-336.386303830494)) ;
#46202 = CARTESIAN_POINT('Ctrl Pts',(-18.531103222829,-1.15200081721432,-336.383880371292)) ;
#46203 = CARTESIAN_POINT('Ctrl Pts',(-18.483089750188,-1.81701145684823,-336.375109608542)) ;
#46204 = CARTESIAN_POINT('Ctrl Pts',(-18.4297782597219,-2.29551918311458,
-336.368668198411)) ;
#46205 = CARTESIAN_POINT('Ctrl Pts',(-18.2825850409861,-3.27053240538154,
-336.355398101143)) ;
#46206 = CARTESIAN_POINT('Ctrl Pts',(-18.1869112130232,-3.76637210749894,
-336.348571176284)) ;
#46207 = CARTESIAN_POINT('Ctrl Pts',(-18.0336523692484,-4.41685634927133,
-336.339707462039)) ;
#46208 = CARTESIAN_POINT('Ctrl Pts',(-17.9940517843836,-4.57551508804472,
-336.33755352673)) ;
#46209 = CARTESIAN_POINT('Ctrl Pts',(-17.9324501406615,-4.80914020858552,
-336.334403681478)) ;
#46210 = CARTESIAN_POINT('Ctrl Pts',(-17.9120636184851,-4.88452398323032,
-336.333390713508)) ;
#46211 = CARTESIAN_POINT('Ctrl Pts',(-17.8732975390369,-5.02436328813107,
-336.331519418475)) ;
#46212 = CARTESIAN_POINT('Ctrl Pts',(-17.8550434264498,-5.08885209058303,
-336.330659697937)) ;
#46213 = CARTESIAN_POINT('Ctrl Pts',(-17.812728065778,-5.2353143774279,-336.328713570545)) ;
#46214 = CARTESIAN_POINT('Ctrl Pts',(-17.7884493942864,-5.31722351885506,
-336.327629697744)) ;
#46215 = CARTESIAN_POINT('Ctrl Pts',(-17.6813555249235,-5.66958259143766,
-336.322981278002)) ;
#46216 = CARTESIAN_POINT('Ctrl Pts',(-17.5929312022217,-5.93828867028473,
-336.319472130966)) ;
#46217 = CARTESIAN_POINT('Ctrl Pts',(-17.3043095538492,-6.75223285826448,
-336.30883132113)) ;
#46218 = CARTESIAN_POINT('Ctrl Pts',(-17.084640688499,-7.29018734870015,-336.301774043995)) ;
#46219 = CARTESIAN_POINT('Ctrl Pts',(-16.7730086680608,-7.96153794060978,
-336.292623162396)) ;
#46220 = CARTESIAN_POINT('Ctrl Pts',(-16.7040383798498,-8.10524570202314,
-336.29064441308)) ;
#46221 = CARTESIAN_POINT('Ctrl Pts',(-16.5315834185869,-8.45302284840997,
-336.285799186626)) ;
#46222 = CARTESIAN_POINT('Ctrl Pts',(-16.4261605342635,-8.65610163002536,
-336.282921557853)) ;
#46223 = CARTESIAN_POINT('Ctrl Pts',(-16.2525716896902,-8.97589317218265,
-336.278302365516)) ;
#46224 = CARTESIAN_POINT('Ctrl Pts',(-16.1868382803381,-9.09389966894386,
-336.276578480985)) ;
#46225 = CARTESIAN_POINT('Ctrl Pts',(-16.0570451834132,-9.32104126853999,
-336.273221206447)) ;
#46226 = CARTESIAN_POINT('Ctrl Pts',(-15.9931458759472,-9.43025955573592,
-336.271589078608)) ;
#46227 = CARTESIAN_POINT('Ctrl Pts',(-15.8509624496447,-9.66768072320648,
-336.268001387954)) ;
#46228 = CARTESIAN_POINT('Ctrl Pts',(-15.7722288425241,-9.79560403429044,
-336.266042554703)) ;
#46229 = CARTESIAN_POINT('Ctrl Pts',(-15.4510962710633,-10.3034566413096,
-336.258163064071)) ;
#46230 = CARTESIAN_POINT('Ctrl Pts',(-15.1964527699241,-10.6754585813738,
-336.25215386373)) ;
#46231 = CARTESIAN_POINT('Ctrl Pts',(-14.6450789876428,-11.4211850932865,
-336.239694244621)) ;
#46232 = CARTESIAN_POINT('Ctrl Pts',(-14.3469692556618,-11.7934846595732,
-336.233242751879)) ;
#46233 = CARTESIAN_POINT('Ctrl Pts',(-13.9265978178705,-12.2789137548389,
-336.224663640599)) ;
#46234 = CARTESIAN_POINT('Ctrl Pts',(-13.8166691038514,-12.4024797833195,
-336.22246495281)) ;
#46235 = CARTESIAN_POINT('Ctrl Pts',(-13.6210884603511,-12.6164955196736,
-336.218641797016)) ;
#46236 = CARTESIAN_POINT('Ctrl Pts',(-13.5361497673482,-12.7075827597181,
-336.217009717293)) ;
#46237 = CARTESIAN_POINT('Ctrl Pts',(-13.4014112342618,-12.849190895936,-336.214469463719)) ;
#46238 = CARTESIAN_POINT('Ctrl Pts',(-13.3522274458185,-12.9002927100518,
-336.213552157006)) ;
#46239 = CARTESIAN_POINT('Ctrl Pts',(-13.2592229408114,-12.9958224154869,
-336.211837323868)) ;
#46240 = CARTESIAN_POINT('Ctrl Pts',(-13.2154687116982,-13.0403136461891,
-336.211038654821)) ;
#46241 = CARTESIAN_POINT('Ctrl Pts',(-13.0901089262946,-13.1665060684571,
-336.208771918995)) ;
#46242 = CARTESIAN_POINT('Ctrl Pts',(-13.0079642387823,-13.2476677259745,
-336.20731230549)) ;
#46243 = CARTESIAN_POINT('Ctrl Pts',(-12.6602195939087,-13.5848978849575,
-336.201227786037)) ;
#46244 = CARTESIAN_POINT('Ctrl Pts',(-12.3877740321692,-13.8337871335208,
-336.196687072756)) ;
#46245 = CARTESIAN_POINT('Ctrl Pts',(-11.7374178303764,-14.3932836272165,
-336.186166061244)) ;
#46246 = CARTESIAN_POINT('Ctrl Pts',(-11.3542883848001,-14.6974054206845,
-336.180199361344)) ;
#46247 = CARTESIAN_POINT('Ctrl Pts',(-10.712914175235,-15.1664554625799,-336.170356233692)) ;
#46248 = CARTESIAN_POINT('Ctrl Pts',(-10.4618096435821,-15.340744435252,-336.166537845105)) ;
#46249 = CARTESIAN_POINT('Ctrl Pts',(-10.0833784872978,-15.5897950106231,
-336.160807458966)) ;
#46250 = CARTESIAN_POINT('Ctrl Pts',(-9.95927826892772,-15.6693652223449,
-336.158932175915)) ;
#46251 = CARTESIAN_POINT('Ctrl Pts',(-9.72904969648478,-15.8131424081075,
-336.155458276502)) ;
#46252 = CARTESIAN_POINT('Ctrl Pts',(-9.62320013510729,-15.877780069158,-336.153863075395)) ;
#46253 = CARTESIAN_POINT('Ctrl Pts',(-9.38366580608846,-16.0207779117035,
-336.150256844704)) ;
#46254 = CARTESIAN_POINT('Ctrl Pts',(-9.24963168175542,-16.0985347938967,
-336.148241439955)) ;
#46255 = CARTESIAN_POINT('Ctrl Pts',(-8.88244010399662,-16.3054529315315,
-336.142727129234)) ;
#46256 = CARTESIAN_POINT('Ctrl Pts',(-8.64744983524044,-16.4312856588522,
-336.13920531375)) ;
#46257 = CARTESIAN_POINT('Ctrl Pts',(-7.82969122251205,-16.846776631901,-336.12699341413)) ;
#46258 = CARTESIAN_POINT('Ctrl Pts',(-7.23445637700788,-17.1108323764909,
-336.118164196097)) ;
#46259 = CARTESIAN_POINT('Ctrl Pts',(-6.37277447255356,-17.440070897112,-336.105812533271)) ;
#46260 = CARTESIAN_POINT('Ctrl Pts',(-6.11685910743164,-17.5314677811533,
-336.102198629731)) ;
#46261 = CARTESIAN_POINT('Ctrl Pts',(-5.77177263480566,-17.6462346130356,
-336.097436552554)) ;
#46262 = CARTESIAN_POINT('Ctrl Pts',(-5.68430087336002,-17.674605483054,-336.09623895615)) ;
#46263 = CARTESIAN_POINT('Ctrl Pts',(-5.53975546378756,-17.7203037732492,
-336.094277652373)) ;
#46264 = CARTESIAN_POINT('Ctrl Pts',(-5.48280277303901,-17.7380080671276,
-336.093509447661)) ;
#46265 = CARTESIAN_POINT('Ctrl Pts',(-5.34844881763035,-17.7790643946202,
-336.091708281867)) ;
#46266 = CARTESIAN_POINT('Ctrl Pts',(-5.27097849655186,-17.8021858550007,
-336.090678104859)) ;
#46267 = CARTESIAN_POINT('Ctrl Pts',(-5.01999843318225,-17.8753103596158,
-336.087364379375)) ;
#46268 = CARTESIAN_POINT('Ctrl Pts',(-4.84590935068426,-17.9232884117445,
-336.08510232428)) ;
#46269 = CARTESIAN_POINT('Ctrl Pts',(-4.57238560123841,-17.9943936403405,
-336.081588115083)) ;
#46270 = CARTESIAN_POINT('Ctrl Pts',(-4.47341320665446,-18.0192532274795,
-336.080324649826)) ;
#46271 = CARTESIAN_POINT('Ctrl Pts',(-3.8211484267994,-18.1773819480632,-336.072039446597)) ;
#46272 = CARTESIAN_POINT('Ctrl Pts',(-3.26218292272399,-18.2859660395737,
-336.065125083936)) ;
#46273 = CARTESIAN_POINT('Ctrl Pts',(-2.34258864956133,-18.4210920620614,
-336.053659245367)) ;
#46274 = CARTESIAN_POINT('Ctrl Pts',(-1.98461423367481,-18.4630891196864,
-336.049176280948)) ;
#46275 = CARTESIAN_POINT('Ctrl Pts',(-1.46960006791021,-18.50835793268,-336.042650674601)) ;
#46276 = CARTESIAN_POINT('Ctrl Pts',(-1.31338743287277,-18.5200985709464,
-336.040661642094)) ;
#46277 = CARTESIAN_POINT('Ctrl Pts',(-1.03318318949492,-18.5375951378299,
-336.037073880576)) ;
#46278 = CARTESIAN_POINT('Ctrl Pts',(-0.909246943366904,-18.5440872232164,
-336.035480019602)) ;
#46279 = CARTESIAN_POINT('Ctrl Pts',(-0.639313325296582,-18.5555144102518,
-336.031992632679)) ;
#46280 = CARTESIAN_POINT('Ctrl Pts',(-0.493303939459485,-18.5599700349355,
-336.030096114867)) ;
#46281 = CARTESIAN_POINT('Ctrl Pts',(-0.0509525005324996,-18.5682452195222,
-336.024319556377)) ;
#46282 = CARTESIAN_POINT('Ctrl Pts',(0.24544195023237,-18.5666928749577,-336.020406457729)) ;
#46283 = CARTESIAN_POINT('Ctrl Pts',(1.00222184847998,-18.5446040173945,-336.010325388514)) ;
#46284 = CARTESIAN_POINT('Ctrl Pts',(1.46211167608331,-18.5140221158868,-336.004111424955)) ;
#46285 = CARTESIAN_POINT('Ctrl Pts',(2.04506559064242,-18.4533985866081,-335.996219226975)) ;
#46286 = CARTESIAN_POINT('Ctrl Pts',(2.16961129492292,-18.4391702500714,-335.994532517905)) ;
#46287 = CARTESIAN_POINT('Ctrl Pts',(2.61270404909148,-18.3839990697948,-335.988537713386)) ;
#46288 = CARTESIAN_POINT('Ctrl Pts',(2.93032208277452,-18.336053486963,-335.984250645725)) ;
#46289 = CARTESIAN_POINT('Ctrl Pts',(3.34260043567125,-18.2628322302956,-335.978759624777)) ;
#46290 = CARTESIAN_POINT('Ctrl Pts',(3.43852840371608,-18.2450141463756,-335.977487313044)) ;
#46291 = CARTESIAN_POINT('Ctrl Pts',(3.59945729527878,-18.213808227023,-335.97536438761)) ;
#46292 = CARTESIAN_POINT('Ctrl Pts',(3.66453486222498,-18.2008265534706,-335.974509155172)) ;
#46293 = CARTESIAN_POINT('Ctrl Pts',(3.80863316193467,-18.1712776475879,-335.972623191489)) ;
#46294 = CARTESIAN_POINT('Ctrl Pts',(3.8876180935596,-18.1545433291696,-335.97159436539)) ;
#46295 = CARTESIAN_POINT('Ctrl Pts',(4.14220557159471,-18.0988669405723,-335.96829079451)) ;
#46296 = CARTESIAN_POINT('Ctrl Pts',(4.31735232574465,-18.0578880444827,-335.966037363104)) ;
#46297 = CARTESIAN_POINT('Ctrl Pts',(4.76972153831358,-17.9450899613946,-335.960239603275)) ;
#46298 = CARTESIAN_POINT('Ctrl Pts',(5.04592731089906,-17.8693904559283,-335.956721217965)) ;
#46299 = CARTESIAN_POINT('Ctrl Pts',(5.99271267098134,-17.5862026731802,-335.944607124163)) ;
#46300 = CARTESIAN_POINT('Ctrl Pts',(6.65320780109245,-17.3471022097047,-335.936040546542)) ;
#46301 = CARTESIAN_POINT('Ctrl Pts',(7.45852865400606,-17.0027971710733,-335.925022604997)) ;
#46302 = CARTESIAN_POINT('Ctrl Pts',(7.61751325109287,-16.9321662247471,-335.922820081268)) ;
#46303 = CARTESIAN_POINT('Ctrl Pts',(7.88979697982699,-16.8065895008203,-335.918996614525)) ;
#46304 = CARTESIAN_POINT('Ctrl Pts',(8.0035731088039,-16.7527061835142,-335.917383274711)) ;
#46305 = CARTESIAN_POINT('Ctrl Pts',(8.23972513215248,-16.6379119077236,-335.914000877156)) ;
#46306 = CARTESIAN_POINT('Ctrl Pts',(8.36199413672027,-16.576798149584,-335.912230432631)) ;
#46307 = CARTESIAN_POINT('Ctrl Pts',(8.6953331183131,-16.405558672651,-335.907350470768)) ;
#46308 = CARTESIAN_POINT('Ctrl Pts',(8.90497699432193,-16.2927148687468,-335.904221882818)) ;
#46309 = CARTESIAN_POINT('Ctrl Pts',(9.71993570488659,-15.8336222114342,-335.891834506938)) ;
#46310 = CARTESIAN_POINT('Ctrl Pts',(10.307714166003,-15.4574177974468,-335.882380570414)) ;
#46311 = CARTESIAN_POINT('Ctrl Pts',(11.1214919922946,-14.8694636076743,-335.868911013355)) ;
#46312 = CARTESIAN_POINT('Ctrl Pts',(11.3655652125875,-14.6837481655826,-335.864821910574)) ;
#46313 = CARTESIAN_POINT('Ctrl Pts',(11.6797860764473,-14.4321271478439,-335.8595452399)) ;
#46314 = CARTESIAN_POINT('Ctrl Pts',(11.7541798796942,-14.3716022835743,-335.858295089916)) ;
#46315 = CARTESIAN_POINT('Ctrl Pts',(11.8791140339333,-14.2683401004377,-335.856196600657)) ;
#46316 = CARTESIAN_POINT('Ctrl Pts',(11.9299007895305,-14.225904070989,-335.855343909202)) ;
#46317 = CARTESIAN_POINT('Ctrl Pts',(12.0429146983721,-14.130441915041,-335.853447692923)) ;
#46318 = CARTESIAN_POINT('Ctrl Pts',(12.1050205720342,-14.0772745985223,-335.85240625014)) ;
#46319 = CARTESIAN_POINT('Ctrl Pts',(12.3076670394367,-13.9014612364561,-335.84900657256)) ;
#46320 = CARTESIAN_POINT('Ctrl Pts',(12.446710883384,-13.7771071299423,-335.846671385337)) ;
#46321 = CARTESIAN_POINT('Ctrl Pts',(12.807325210481,-13.4446753640954,-335.840576928652)) ;
#46322 = CARTESIAN_POINT('Ctrl Pts',(13.0257010845447,-13.2332152714803,-335.836846826742)) ;
#46323 = CARTESIAN_POINT('Ctrl Pts',(13.7055778663635,-12.5417274434548,-335.824964477589)) ;
#46324 = CARTESIAN_POINT('Ctrl Pts',(14.1464919548063,-12.0421989850211,-335.816826809427)) ;
#46325 = CARTESIAN_POINT('Ctrl Pts',(14.6699574299694,-11.380618175491,-335.806221125627)) ;
#46326 = CARTESIAN_POINT('Ctrl Pts',(14.7782873830265,-11.2395882015158,-335.803970938718)) ;
#46327 = CARTESIAN_POINT('Ctrl Pts',(14.9601458050896,-10.9956592670613,-335.800092800337)) ;
#46328 = CARTESIAN_POINT('Ctrl Pts',(15.0346796097078,-10.8935253341977,-335.79847308245)) ;
#46329 = CARTESIAN_POINT('Ctrl Pts',(15.1868012449538,-10.6805371285541,-335.795102755632)) ;
#46330 = CARTESIAN_POINT('Ctrl Pts',(15.2642322371292,-10.5695799137498,-335.793351028236)) ;
#46331 = CARTESIAN_POINT('Ctrl Pts',(15.4700402476174,-10.2676817847379,-335.788595340753)) ;
#46332 = CARTESIAN_POINT('Ctrl Pts',(15.5960919032851,-10.0751849379759,-335.785573970629)) ;
#46333 = CARTESIAN_POINT('Ctrl Pts',(15.8040771356618,-9.74430519000732,-335.780402828035)) ;
#46334 = CARTESIAN_POINT('Ctrl Pts',(15.8878500417749,-9.60710980012188,-335.778265068858)) ;
#46335 = CARTESIAN_POINT('Ctrl Pts',(16.2715385199525,-8.9599938442345,-335.768220117827)) ;
#46336 = CARTESIAN_POINT('Ctrl Pts',(16.5487527548252,-8.43701579263089,-335.760200309543)) ;
#46337 = CARTESIAN_POINT('Ctrl Pts',(16.8908789576445,-7.70958993684472,-335.749434943328)) ;
#46338 = CARTESIAN_POINT('Ctrl Pts',(16.9779308737153,-7.51594521258067,-335.746606649694)) ;
#46339 = CARTESIAN_POINT('Ctrl Pts',(17.1101854561587,-7.20771865244227,-335.742184867733)) ;
#46340 = CARTESIAN_POINT('Ctrl Pts',(17.1576018031395,-7.09410705839913,-335.740571962958)) ;
#46341 = CARTESIAN_POINT('Ctrl Pts',(17.2278428871278,-6.9209818517865,-335.738144291973)) ;
#46342 = CARTESIAN_POINT('Ctrl Pts',(17.2514968684681,-6.86180851861114,-335.737319828005)) ;
#46343 = CARTESIAN_POINT('Ctrl Pts',(17.300265986958,-6.73796034533484,-335.735606211945)) ;
#46344 = CARTESIAN_POINT('Ctrl Pts',(17.3253241798233,-6.67326418608659,-335.734717908428)) ;
#46345 = CARTESIAN_POINT('Ctrl Pts',(17.3914889007665,-6.49955283060892,-335.732349387754)) ;
#46346 = CARTESIAN_POINT('Ctrl Pts',(17.4319329461844,-6.39028849167808,-335.730876997474)) ;
#46347 = CARTESIAN_POINT('Ctrl Pts',(17.6036438507278,-5.91262769005917,-335.724502665087)) ;
#46348 = CARTESIAN_POINT('Ctrl Pts',(17.7242808599766,-5.54051553966805,-335.719695670775)) ;
#46349 = CARTESIAN_POINT('Ctrl Pts',(18.026714909058,-4.49628245723896,-335.70636980271)) ;
#46350 = CARTESIAN_POINT('Ctrl Pts',(18.182600991019,-3.81733244457233,-335.697872688997)) ;
#46351 = CARTESIAN_POINT('Ctrl Pts',(18.3295148688494,-2.95871905123448,-335.686916465868)) ;
#46352 = CARTESIAN_POINT('Ctrl Pts',(18.3565928806566,-2.78579098872454,-335.684700782015)) ;
#46353 = CARTESIAN_POINT('Ctrl Pts',(18.3989566947429,-2.48772521732273,-335.680862270824)) ;
#46354 = CARTESIAN_POINT('Ctrl Pts',(18.4154206037213,-2.36276705304418,-335.679247219785)) ;
#46355 = CARTESIAN_POINT('Ctrl Pts',(18.4470366554315,-2.10235864654082,-335.675868449205)) ;
#46356 = CARTESIAN_POINT('Ctrl Pts',(18.4619722249938,-1.9668896109491,-335.674103419246)) ;
#46357 = CARTESIAN_POINT('Ctrl Pts',(18.498667463784,-1.59667642803706,-335.669259552181)) ;
#46358 = CARTESIAN_POINT('Ctrl Pts',(18.5174497915935,-1.3616631154694,-335.666162133276)) ;
#46359 = CARTESIAN_POINT('Ctrl Pts',(18.5365593472123,-1.04725680702123,-335.661991743979)) ;
#46360 = CARTESIAN_POINT('Ctrl Pts',(18.5408603713437,-0.968129729065171,
-335.660939964508)) ;
#46361 = CARTESIAN_POINT('Ctrl Pts',(18.5446545938163,-0.888979976461629,
-335.659885874007)) ;
#46362 = CARTESIAN_POINT('Ctrl Pts',(18.5446545934131,-0.888979984870909,
-335.363183819487)) ;
#46363 = CARTESIAN_POINT('Ctrl Pts',(18.5274773631996,-1.24730728875046,-335.367987381273)) ;
#46364 = CARTESIAN_POINT('Ctrl Pts',(18.4999170091639,-1.6050846689973,-335.372827203657)) ;
#46365 = CARTESIAN_POINT('Ctrl Pts',(18.4457968108924,-2.11438034440564,-335.379722413713)) ;
#46366 = CARTESIAN_POINT('Ctrl Pts',(18.4276999900379,-2.26669304111968,-335.381785006543)) ;
#46367 = CARTESIAN_POINT('Ctrl Pts',(18.3707061504084,-2.70043792830454,-335.387647964213)) ;
#46368 = CARTESIAN_POINT('Ctrl Pts',(18.3272339112023,-2.9812257895604,-335.391430876734)) ;
#46369 = CARTESIAN_POINT('Ctrl Pts',(18.2623382693532,-3.34496505956417,-335.396272411271)) ;
#46370 = CARTESIAN_POINT('Ctrl Pts',(18.2467612735903,-3.42892014569708,-335.397385731343)) ;
#46371 = CARTESIAN_POINT('Ctrl Pts',(18.2179264561967,-3.57856756232574,-335.399360943711)) ;
#46372 = CARTESIAN_POINT('Ctrl Pts',(18.204891069443,-3.64430121574535,-335.400225322137)) ;
#46373 = CARTESIAN_POINT('Ctrl Pts',(18.1758898581029,-3.78650628010723,-335.402087486718)) ;
#46374 = CARTESIAN_POINT('Ctrl Pts',(18.1597967253699,-3.86295027907294,-335.403083836486)) ;
#46375 = CARTESIAN_POINT('Ctrl Pts',(18.1084913710847,-4.09924775802851,-335.406152095274)) ;
#46376 = CARTESIAN_POINT('Ctrl Pts',(18.0716472468421,-4.25873899896801,-335.408206651624)) ;
#46377 = CARTESIAN_POINT('Ctrl Pts',(17.9125266788189,-4.90825317797366,-335.416539785052)) ;
#46378 = CARTESIAN_POINT('Ctrl Pts',(17.7723889353657,-5.39367732076572,-335.422694136307)) ;
#46379 = CARTESIAN_POINT('Ctrl Pts',(17.4605826181039,-6.32879280746731,-335.43477852423)) ;
#46380 = CARTESIAN_POINT('Ctrl Pts',(17.2908779858376,-6.77872414270108,-335.440700389258)) ;
#46381 = CARTESIAN_POINT('Ctrl Pts',(17.0317533885978,-7.39244777852428,-335.449064846342)) ;
#46382 = CARTESIAN_POINT('Ctrl Pts',(16.9570450434212,-7.56224377337838,-335.451409589574)) ;
#46383 = CARTESIAN_POINT('Ctrl Pts',(16.8271948528679,-7.84576164285713,-335.455381319778)) ;
#46384 = CARTESIAN_POINT('Ctrl Pts',(16.7734135892526,-7.96009163788595,-335.456998628237)) ;
#46385 = CARTESIAN_POINT('Ctrl Pts',(16.6607630390207,-8.19335601743633,-335.460331702028)) ;
#46386 = CARTESIAN_POINT('Ctrl Pts',(16.6017771400517,-8.31222615191562,-335.462048236235)) ;
#46387 = CARTESIAN_POINT('Ctrl Pts',(16.4437758770691,-8.62224284836822,-335.466572938997)) ;
#46388 = CARTESIAN_POINT('Ctrl Pts',(16.342701735866,-8.812317320173,-335.469395593491)) ;
#46389 = CARTESIAN_POINT('Ctrl Pts',(16.1058578282291,-9.23961739762066,-335.475848570329)) ;
#46390 = CARTESIAN_POINT('Ctrl Pts',(15.9681089109282,-9.47568907453852,-335.479490937868)) ;
#46391 = CARTESIAN_POINT('Ctrl Pts',(15.6418076838945,-10.0075643369964,-335.487853451055)) ;
#46392 = CARTESIAN_POINT('Ctrl Pts',(15.4499828815418,-10.3012387707321,-335.492585545034)) ;
#46393 = CARTESIAN_POINT('Ctrl Pts',(15.1958746987544,-10.6671871760292,-335.498582258604)) ;
#46394 = CARTESIAN_POINT('Ctrl Pts',(15.1411975319602,-10.7446557606444,-335.499857480419)) ;
#46395 = CARTESIAN_POINT('Ctrl Pts',(14.8982625584874,-11.0833178125441,-335.505453372739)) ;
#46396 = CARTESIAN_POINT('Ctrl Pts',(14.7038218711425,-11.3400081181365,-335.509751453207)) ;
#46397 = CARTESIAN_POINT('Ctrl Pts',(14.4417884144324,-11.6678531738936,-335.515255348585)) ;
#46398 = CARTESIAN_POINT('Ctrl Pts',(14.3801703610754,-11.7437111136783,-335.51652981205)) ;
#46399 = CARTESIAN_POINT('Ctrl Pts',(14.2757002239312,-11.8702690999123,-335.518655124242)) ;
#46400 = CARTESIAN_POINT('Ctrl Pts',(14.2331700339669,-11.9212321597634,-335.519510617606)) ;
#46401 = CARTESIAN_POINT('Ctrl Pts',(14.1383659690171,-12.0336033840814,-335.521395654992)) ;
#46402 = CARTESIAN_POINT('Ctrl Pts',(14.085963553445,-12.0949011353684,-335.522423310406)) ;
#46403 = CARTESIAN_POINT('Ctrl Pts',(13.9157946651901,-12.2913503115116,-335.525718106856)) ;
#46404 = CARTESIAN_POINT('Ctrl Pts',(13.7964695249517,-12.4251383288522,-335.527964089446)) ;
#46405 = CARTESIAN_POINT('Ctrl Pts',(13.4826055391519,-12.7669476885797,-335.533735307216)) ;
#46406 = CARTESIAN_POINT('Ctrl Pts',(13.2851841418668,-12.9722584054192,-335.537234879398)) ;
#46407 = CARTESIAN_POINT('Ctrl Pts',(12.582090180083,-13.6705578557767,-335.54938275708)) ;
#46408 = CARTESIAN_POINT('Ctrl Pts',(12.053080119611,-14.1391797697511,-335.558000380931)) ;
#46409 = CARTESIAN_POINT('Ctrl Pts',(11.3761172157347,-14.6732007749142,-335.568848770328)) ;
#46410 = CARTESIAN_POINT('Ctrl Pts',(11.2523524476432,-14.768325165274,-335.570824037677)) ;
#46411 = CARTESIAN_POINT('Ctrl Pts',(11.0261121421737,-14.9377160827822,-335.574423301638)) ;
#46412 = CARTESIAN_POINT('Ctrl Pts',(10.9240486928393,-15.0125171388613,-335.576042884117)) ;
#46413 = CARTESIAN_POINT('Ctrl Pts',(10.7136513598514,-15.1634330253873,-335.579374142734)) ;
#46414 = CARTESIAN_POINT('Ctrl Pts',(10.6052518880291,-15.2394441796742,-335.581086520098)) ;
#46415 = CARTESIAN_POINT('Ctrl Pts',(10.3199258518366,-15.434999842403,-335.585584039716)) ;
#46416 = CARTESIAN_POINT('Ctrl Pts',(10.1417339144932,-15.5526628807797,-335.588383337061)) ;
#46417 = CARTESIAN_POINT('Ctrl Pts',(9.64470771898151,-15.8686826094302,-335.596161233655)) ;
#46418 = CARTESIAN_POINT('Ctrl Pts',(9.32182533424749,-16.0604808817661,-335.60118204392)) ;
#46419 = CARTESIAN_POINT('Ctrl Pts',(8.43138312839876,-16.553516424503,-335.614865367491)) ;
#46420 = CARTESIAN_POINT('Ctrl Pts',(7.85364586991162,-16.8353014189392,-335.623581211539)) ;
#46421 = CARTESIAN_POINT('Ctrl Pts',(7.16059530128688,-17.1298752943899,-335.633485576558)) ;
#46422 = CARTESIAN_POINT('Ctrl Pts',(7.05833585889369,-17.1722639051843,-335.634932838381)) ;
#46423 = CARTESIAN_POINT('Ctrl Pts',(6.8985797834561,-17.236817927763,-335.637168539028)) ;
#46424 = CARTESIAN_POINT('Ctrl Pts',(6.84134158923589,-17.2596158874615,-335.637964534974)) ;
#46425 = CARTESIAN_POINT('Ctrl Pts',(6.71679082019853,-17.308507508772,-335.639684892952)) ;
#46426 = CARTESIAN_POINT('Ctrl Pts',(6.64943739023208,-17.334494325333,-335.640607859626)) ;
#46427 = CARTESIAN_POINT('Ctrl Pts',(6.45942240965936,-17.4065369380194,-335.643193163933)) ;
#46428 = CARTESIAN_POINT('Ctrl Pts',(6.33642233361407,-17.45168811715,-335.644845054755)) ;
#46429 = CARTESIAN_POINT('Ctrl Pts',(6.04552526660874,-17.5549904965224,-335.648711106168)) ;
#46430 = CARTESIAN_POINT('Ctrl Pts',(5.8772509338337,-17.6120410142795,-335.650915890014)) ;
#46431 = CARTESIAN_POINT('Ctrl Pts',(5.17102826160835,-17.8402248897353,-335.660078304486)) ;
#46432 = CARTESIAN_POINT('Ctrl Pts',(4.62623668279112,-17.9891937885443,-335.666937277826)) ;
#46433 = CARTESIAN_POINT('Ctrl Pts',(3.72117205385357,-18.1928361365434,-335.678378221337)) ;
#46434 = CARTESIAN_POINT('Ctrl Pts',(3.36457578229734,-18.2621476583946,-335.682895061056)) ;
#46435 = CARTESIAN_POINT('Ctrl Pts',(2.85058591928489,-18.3464852148715,-335.68946799442)) ;
#46436 = CARTESIAN_POINT('Ctrl Pts',(2.69467594077538,-18.3700321528772,-335.691469659938)) ;
#46437 = CARTESIAN_POINT('Ctrl Pts',(2.4154879284857,-18.4085668640108,-335.695070752324)) ;
#46438 = CARTESIAN_POINT('Ctrl Pts',(2.29232363194527,-18.4243091657438,-335.696665151404)) ;
#46439 = CARTESIAN_POINT('Ctrl Pts',(2.02469447952201,-18.4557911525432,-335.700142995389)) ;
#46440 = CARTESIAN_POINT('Ctrl Pts',(1.88018397643718,-18.4710725983935,-335.702029310084)) ;
#46441 = CARTESIAN_POINT('Ctrl Pts',(1.44555132452498,-18.5118799003401,-335.70772793962)) ;
#46442 = CARTESIAN_POINT('Ctrl Pts',(1.15499370184704,-18.5322773837841,-335.71157194813)) ;
#46443 = CARTESIAN_POINT('Ctrl Pts',(0.418580504240088,-18.5665879464058,
-335.721384087056)) ;
#46444 = CARTESIAN_POINT('Ctrl Pts',(-0.0275189157587249,-18.5712853371342,
-335.727394752062)) ;
#46445 = CARTESIAN_POINT('Ctrl Pts',(-0.547625919799585,-18.5580205132199,
-335.734402122302)) ;
#46446 = CARTESIAN_POINT('Ctrl Pts',(-0.621887209276719,-18.5556804191639,
-335.735402516399)) ;
#46447 = CARTESIAN_POINT('Ctrl Pts',(-0.796446928902621,-18.5491306764911,
-335.737752723704)) ;
#46448 = CARTESIAN_POINT('Ctrl Pts',(-0.896729258491385,-18.5445531952714,
-335.739101856017)) ;
#46449 = CARTESIAN_POINT('Ctrl Pts',(-1.29584885458761,-18.5230899776942,
-335.744462456376)) ;
#46450 = CARTESIAN_POINT('Ctrl Pts',(-1.59429641616559,-18.4997920571509,
-335.74845173471)) ;
#46451 = CARTESIAN_POINT('Ctrl Pts',(-1.98680889456779,-18.4595818814092,
-335.753622882504)) ;
#46452 = CARTESIAN_POINT('Ctrl Pts',(-2.08149144948029,-18.4491454057727,
-335.754864395207)) ;
#46453 = CARTESIAN_POINT('Ctrl Pts',(-2.24175311720873,-18.4302309839971,
-335.756953440762)) ;
#46454 = CARTESIAN_POINT('Ctrl Pts',(-2.30737476773423,-18.4221305194097,
-335.757805221927)) ;
#46455 = CARTESIAN_POINT('Ctrl Pts',(-2.45445262988278,-18.4031767462576,
-335.759705817049)) ;
#46456 = CARTESIAN_POINT('Ctrl Pts',(-2.53588271326722,-18.3921328550058,
-335.760752476517)) ;
#46457 = CARTESIAN_POINT('Ctrl Pts',(-2.8046982342454,-18.3538557665272,-335.764192751267)) ;
#46458 = CARTESIAN_POINT('Ctrl Pts',(-2.991740622067,-18.3242964930456,-335.766562565817)) ;
#46459 = CARTESIAN_POINT('Ctrl Pts',(-3.48533201525628,-18.2385327238313,
-335.77278579663)) ;
#46460 = CARTESIAN_POINT('Ctrl Pts',(-3.79097429135877,-18.1774621329308,
-335.776608593526)) ;
#46461 = CARTESIAN_POINT('Ctrl Pts',(-4.71916399508871,-17.9675701867732,
-335.788267426841)) ;
#46462 = CARTESIAN_POINT('Ctrl Pts',(-5.33567720882668,-17.794230384558,-335.79609392181)) ;
#46463 = CARTESIAN_POINT('Ctrl Pts',(-6.11643702438022,-17.5304762243907,
-335.806443482945)) ;
#46464 = CARTESIAN_POINT('Ctrl Pts',(-6.28998338880483,-17.4689583931982,
-335.808771247093)) ;
#46465 = CARTESIAN_POINT('Ctrl Pts',(-6.58082767941278,-17.3609652722419,
-335.812723215026)) ;
#46466 = CARTESIAN_POINT('Ctrl Pts',(-6.69861897412264,-17.3158572388618,
-335.814337974192)) ;
#46467 = CARTESIAN_POINT('Ctrl Pts',(-6.93970998732344,-17.2207035160282,
-335.817673334951)) ;
#46468 = CARTESIAN_POINT('Ctrl Pts',(-7.06294976816604,-17.1705254667594,
-335.819394784002)) ;
#46469 = CARTESIAN_POINT('Ctrl Pts',(-7.38602440691943,-17.0349162500238,
-335.823951632333)) ;
#46470 = CARTESIAN_POINT('Ctrl Pts',(-7.58491684124977,-16.9472937201395,
-335.826801912308)) ;
#46471 = CARTESIAN_POINT('Ctrl Pts',(-7.91181944834641,-16.7963682684946,
-335.831558958492)) ;
#46472 = CARTESIAN_POINT('Ctrl Pts',(-8.04071964325235,-16.7350441155975,
-335.833453609637)) ;
#46473 = CARTESIAN_POINT('Ctrl Pts',(-8.60617386456888,-16.4579884277976,
-335.841843707323)) ;
#46474 = CARTESIAN_POINT('Ctrl Pts',(-9.03484927405166,-16.2266172929978,
-335.84841857797)) ;
#46475 = CARTESIAN_POINT('Ctrl Pts',(-9.55214617044281,-15.9205535669559,
-335.856507433423)) ;
#46476 = CARTESIAN_POINT('Ctrl Pts',(-9.6498233279977,-15.8615393986178,-335.858041525314)) ;
#46477 = CARTESIAN_POINT('Ctrl Pts',(-10.0011107363825,-15.6448540810405,
-335.863576908721)) ;
#46478 = CARTESIAN_POINT('Ctrl Pts',(-10.2514523652854,-15.4819701660421,
-335.86755685313)) ;
#46479 = CARTESIAN_POINT('Ctrl Pts',(-10.5763018442078,-15.2592728362574,
-335.872718632993)) ;
#46480 = CARTESIAN_POINT('Ctrl Pts',(-10.654431945796,-15.2048231867766,-335.873959822097)) ;
#46481 = CARTESIAN_POINT('Ctrl Pts',(-10.7860910685688,-15.1115555229098,
-335.876048514775)) ;
#46482 = CARTESIAN_POINT('Ctrl Pts',(-10.8398378396984,-15.0730483480079,
-335.876900262769)) ;
#46483 = CARTESIAN_POINT('Ctrl Pts',(-10.9599339440802,-14.9860302496266,
-335.8788010264)) ;
#46484 = CARTESIAN_POINT('Ctrl Pts',(-11.0261690136788,-14.9373642791632,
-335.879847884793)) ;
#46485 = CARTESIAN_POINT('Ctrl Pts',(-11.2440096604312,-14.7750682412346,
-335.883289717874)) ;
#46486 = CARTESIAN_POINT('Ctrl Pts',(-11.394199259038,-14.6595572325294,-335.885660862677)) ;
#46487 = CARTESIAN_POINT('Ctrl Pts',(-11.7869160745852,-14.347836459618,-335.891889079029)) ;
#46488 = CARTESIAN_POINT('Ctrl Pts',(-12.0263114861197,-14.1477784177621,
-335.895715474379)) ;
#46489 = CARTESIAN_POINT('Ctrl Pts',(-12.741458630008,-13.5188704277034,-335.907383067258)) ;
#46490 = CARTESIAN_POINT('Ctrl Pts',(-13.2001604398673,-13.0713575821924,
-335.915214904207)) ;
#46491 = CARTESIAN_POINT('Ctrl Pts',(-13.7595132417925,-12.466116006806,-335.925565434011)) ;
#46492 = CARTESIAN_POINT('Ctrl Pts',(-13.8821984303031,-12.3293478958293,
-335.927888319434)) ;
#46493 = CARTESIAN_POINT('Ctrl Pts',(-14.0856125680081,-12.095698048235,-335.931834616302)) ;
#46494 = CARTESIAN_POINT('Ctrl Pts',(-14.1674210769188,-11.9997738589716,
-335.933448650069)) ;
#46495 = CARTESIAN_POINT('Ctrl Pts',(-14.3336223336374,-11.80082639626,-335.936784714158)) ;
#46496 = CARTESIAN_POINT('Ctrl Pts',(-14.417896388251,-11.6977133027227,-335.938507614875)) ;
#46497 = CARTESIAN_POINT('Ctrl Pts',(-14.6371428266436,-11.4234864662596,
-335.943073960606)) ;
#46498 = CARTESIAN_POINT('Ctrl Pts',(-14.7702241001134,-11.2508876513431,
-335.945932403682)) ;
#46499 = CARTESIAN_POINT('Ctrl Pts',(-15.0662739311693,-10.8526195284953,
-335.952489223089)) ;
#46500 = CARTESIAN_POINT('Ctrl Pts',(-15.227268150274,-10.6255477530029,-335.956200277765)) ;
#46501 = CARTESIAN_POINT('Ctrl Pts',(-15.614263666664,-10.0528472290745,-335.965466934884)) ;
#46502 = CARTESIAN_POINT('Ctrl Pts',(-15.8339549721789,-9.70313540812938,
-335.971045912676)) ;
#46503 = CARTESIAN_POINT('Ctrl Pts',(-16.2141427265182,-9.05059507603661,
-335.981193433851)) ;
#46504 = CARTESIAN_POINT('Ctrl Pts',(-16.378267773699,-8.75008806551203,-335.985769092919)) ;
#46505 = CARTESIAN_POINT('Ctrl Pts',(-16.5789288923932,-8.35723495954348,
-335.991555631055)) ;
#46506 = CARTESIAN_POINT('Ctrl Pts',(-16.623164444904,-8.26889734288747,-335.992844266301)) ;
#46507 = CARTESIAN_POINT('Ctrl Pts',(-16.6959944930646,-8.12051045233272,
-335.994985360415)) ;
#46508 = CARTESIAN_POINT('Ctrl Pts',(-16.7249751591501,-8.06065308030398,
-335.995842634557)) ;
#46509 = CARTESIAN_POINT('Ctrl Pts',(-16.7881255011991,-7.928413964869,-335.997721870492)) ;
#46510 = CARTESIAN_POINT('Ctrl Pts',(-16.8221499134748,-7.85596449549852,
-335.998742049887)) ;
#46511 = CARTESIAN_POINT('Ctrl Pts',(-16.9292489038866,-7.62402822017504,
-336.001981353258)) ;
#46512 = CARTESIAN_POINT('Ctrl Pts',(-17.0005320599442,-7.46372458089711,
-336.004180285562)) ;
#46513 = CARTESIAN_POINT('Ctrl Pts',(-17.1777265373408,-7.04953026332026,
-336.009785651805)) ;
#46514 = CARTESIAN_POINT('Ctrl Pts',(-17.2802865345593,-6.79425224676871,
-336.013168141533)) ;
#46515 = CARTESIAN_POINT('Ctrl Pts',(-17.6330566245216,-5.85646254593097,
-336.02545477956)) ;
#46516 = CARTESIAN_POINT('Ctrl Pts',(-17.8488030819397,-5.16169234639476,
-336.034318009026)) ;
#46517 = CARTESIAN_POINT('Ctrl Pts',(-18.0602310403077,-4.30653922511104,
-336.045405715722)) ;
#46518 = CARTESIAN_POINT('Ctrl Pts',(-18.0953384416368,-4.15655529482406,
-336.047355614413)) ;
#46519 = CARTESIAN_POINT('Ctrl Pts',(-18.1557819366841,-3.88303735394985,
-336.050923885749)) ;
#46520 = CARTESIAN_POINT('Ctrl Pts',(-18.1817336200057,-3.75964883237853,
-336.052538113747)) ;
#46521 = CARTESIAN_POINT('Ctrl Pts',(-18.2325005158333,-3.50544577534052,
-336.055873987054)) ;
#46522 = CARTESIAN_POINT('Ctrl Pts',(-18.2571694661401,-3.37460933522918,
-336.05759649659)) ;
#46523 = CARTESIAN_POINT('Ctrl Pts',(-18.3184733648802,-3.02910139661202,
-336.062160282979)) ;
#46524 = CARTESIAN_POINT('Ctrl Pts',(-18.3527422708443,-2.81403137325167,
-336.065016526234)) ;
#46525 = CARTESIAN_POINT('Ctrl Pts',(-18.4221286336303,-2.32313678465176,
-336.071566941386)) ;
#46526 = CARTESIAN_POINT('Ctrl Pts',(-18.4548495404508,-2.04702611783494,
-336.075273752073)) ;
#46527 = CARTESIAN_POINT('Ctrl Pts',(-18.5207255910791,-1.359295863721,-336.084535941677)) ;
#46528 = CARTESIAN_POINT('Ctrl Pts',(-18.5463729221208,-0.94710751380241,
-336.090114790525)) ;
#46529 = CARTESIAN_POINT('Ctrl Pts',(-18.5681415683955,-0.191153551558178,
-336.100276631728)) ;
#46530 = CARTESIAN_POINT('Ctrl Pts',(-18.5685008398542,0.152310163944746,
-336.104866549654)) ;
#46531 = CARTESIAN_POINT('Ctrl Pts',(-18.5567027574909,0.594139617409694,
-336.110664000756)) ;
#46532 = CARTESIAN_POINT('Ctrl Pts',(-18.5532861372631,0.692670675679252,
-336.111949918189)) ;
#46533 = CARTESIAN_POINT('Ctrl Pts',(-18.5462519442838,0.857588271429485,
-336.114087977898)) ;
#46534 = CARTESIAN_POINT('Ctrl Pts',(-18.5430623035918,0.923990944389028,
-336.11494490271)) ;
#46535 = CARTESIAN_POINT('Ctrl Pts',(-18.535240397903,1.07041457494002,-336.116825213065)) ;
#46536 = CARTESIAN_POINT('Ctrl Pts',(-18.5304464430942,1.15042540549828,-336.117846796191)) ;
#46537 = CARTESIAN_POINT('Ctrl Pts',(-18.5134611721284,1.40615827878428,-336.121096448638)) ;
#46538 = CARTESIAN_POINT('Ctrl Pts',(-18.4992872112119,1.58173908876808,-336.123304147702)) ;
#46539 = CARTESIAN_POINT('Ctrl Pts',(-18.4564140903844,2.03271579750189,-336.128940184567)) ;
#46540 = CARTESIAN_POINT('Ctrl Pts',(-18.4240491012346,2.30771958733761,-336.132344264429)) ;
#46541 = CARTESIAN_POINT('Ctrl Pts',(-18.2849234231809,3.29842597660611,-336.1446115221)) ;
#46542 = CARTESIAN_POINT('Ctrl Pts',(-18.1424992023407,4.00846117673017,-336.153435746986)) ;
#46543 = CARTESIAN_POINT('Ctrl Pts',(-17.9198941579576,4.8575378789742,-336.164483661252)) ;
#46544 = CARTESIAN_POINT('Ctrl Pts',(-17.8789285313958,5.00621567220246,-336.166435780378)) ;
#46545 = CARTESIAN_POINT('Ctrl Pts',(-17.8011003243769,5.27553162138632,-336.170006757127)) ;
#46546 = CARTESIAN_POINT('Ctrl Pts',(-17.7648514804252,5.39633750540368,-336.171621446599)) ;
#46547 = CARTESIAN_POINT('Ctrl Pts',(-17.6878335820268,5.64382407506593,-336.174956873903)) ;
#46548 = CARTESIAN_POINT('Ctrl Pts',(-17.6469277639348,5.77045470022852,-336.176678461387)) ;
#46549 = CARTESIAN_POINT('Ctrl Pts',(-17.5356232918261,6.10275914538369,-336.181236215306)) ;
#46550 = CARTESIAN_POINT('Ctrl Pts',(-17.4629677138333,6.30765501476063,-336.184087273612)) ;
#46551 = CARTESIAN_POINT('Ctrl Pts',(-17.1448779018516,7.15704049088048,-336.196070358147)) ;
#46552 = CARTESIAN_POINT('Ctrl Pts',(-16.8672308176833,7.7888757224233,-336.205404486304)) ;
#46553 = CARTESIAN_POINT('Ctrl Pts',(-16.3985788646021,8.71209822607914,-336.219317387319)) ;
#46554 = CARTESIAN_POINT('Ctrl Pts',(-16.2334933985647,9.0159712295388,-336.223939282063)) ;
#46555 = CARTESIAN_POINT('Ctrl Pts',(-16.010611222847,9.40024069076365,-336.229765982323)) ;
#46556 = CARTESIAN_POINT('Ctrl Pts',(-15.9605264372088,9.4850299241349,-336.23105038965)) ;
#46557 = CARTESIAN_POINT('Ctrl Pts',(-15.8755114120268,9.62637285886781,-336.233186764962)) ;
#46558 = CARTESIAN_POINT('Ctrl Pts',(-15.8409478042327,9.68314461891534,-336.234043497295)) ;
#46559 = CARTESIAN_POINT('Ctrl Pts',(-15.763998094957,9.80802213478902,-336.235924412564)) ;
#46560 = CARTESIAN_POINT('Ctrl Pts',(-15.7214740329294,9.8760411294199,-336.236946781887)) ;
#46561 = CARTESIAN_POINT('Ctrl Pts',(-15.5839550353451,10.0928693889064,-336.240202244278)) ;
#46562 = CARTESIAN_POINT('Ctrl Pts',(-15.4872777640754,10.24060030934,-336.242414866493)) ;
#46563 = CARTESIAN_POINT('Ctrl Pts',(-15.2330470546021,10.6172497446688,-336.248068173139)) ;
#46564 = CARTESIAN_POINT('Ctrl Pts',(-15.072434542249,10.8440505379828,-336.251484422158)) ;
#46565 = CARTESIAN_POINT('Ctrl Pts',(-14.7678052807181,11.2543676073785,-336.257750556726)) ;
#46566 = CARTESIAN_POINT('Ctrl Pts',(-14.6253043346455,11.4389394693402,-336.260602454362)) ;
#46567 = CARTESIAN_POINT('Ctrl Pts',(-14.4083345819757,11.7092814509909,-336.264854180674)) ;
#46568 = CARTESIAN_POINT('Ctrl Pts',(-14.3364942413808,11.7971314470239,-336.26624782126)) ;
#46569 = CARTESIAN_POINT('Ctrl Pts',(-14.0994474180707,12.0816409379055,-336.270805883876)) ;
#46570 = CARTESIAN_POINT('Ctrl Pts',(-13.930965093299,12.2755316200063,-336.273983147639)) ;
#46571 = CARTESIAN_POINT('Ctrl Pts',(-13.6046076231195,12.635730802631,-336.280049652995)) ;
#46572 = CARTESIAN_POINT('Ctrl Pts',(-13.4475680449257,12.8027323215245,-336.282932536417)) ;
#46573 = CARTESIAN_POINT('Ctrl Pts',(-13.193085597127,13.0635086168393,-336.287557984781)) ;
#46574 = CARTESIAN_POINT('Ctrl Pts',(-13.0976411462376,13.1592006328394,-336.289282781318)) ;
#46575 = CARTESIAN_POINT('Ctrl Pts',(-12.910854236077,13.3424264939033,-336.292640513232)) ;
#46576 = CARTESIAN_POINT('Ctrl Pts',(-12.8196450589781,13.43008571671,-336.294272171413)) ;
#46577 = CARTESIAN_POINT('Ctrl Pts',(-12.5977567893812,13.6390177276984,-336.298223205011)) ;
#46578 = CARTESIAN_POINT('Ctrl Pts',(-12.4662130066133,13.7593536849493,-336.30055058827)) ;
#46579 = CARTESIAN_POINT('Ctrl Pts',(-12.1770991684383,14.0162845057729,-336.305632819249)) ;
#46580 = CARTESIAN_POINT('Ctrl Pts',(-12.0189195114307,14.1521570467785,-336.308392910177)) ;
#46581 = CARTESIAN_POINT('Ctrl Pts',(-11.5060443348556,14.5779028983082,-336.317267704812)) ;
#46582 = CARTESIAN_POINT('Ctrl Pts',(-11.1428976606122,14.8573261240034,-336.323444534676)) ;
#46583 = CARTESIAN_POINT('Ctrl Pts',(-10.4187841022637,15.3729999290968,-336.335415600943)) ;
#46584 = CARTESIAN_POINT('Ctrl Pts',(-10.0591804804814,15.6106719318834,-336.341206478574)) ;
#46585 = CARTESIAN_POINT('Ctrl Pts',(-9.60028067702208,15.8915254620212,-336.348277332331)) ;
#46586 = CARTESIAN_POINT('Ctrl Pts',(-9.50844566604864,15.9466432723273,-336.349676715036)) ;
#46587 = CARTESIAN_POINT('Ctrl Pts',(-9.35835608112252,16.0349669767516,-336.351935263997)) ;
#46588 = CARTESIAN_POINT('Ctrl Pts',(-9.30038951846853,16.0686573593127,-336.35280067625)) ;
#46589 = CARTESIAN_POINT('Ctrl Pts',(-9.1764029695416,16.1398231325885,-336.354636234313)) ;
#46590 = CARTESIAN_POINT('Ctrl Pts',(-9.11033314604264,16.1772090361517,-336.355605247957)) ;
#46591 = CARTESIAN_POINT('Ctrl Pts',(-8.91218267164981,16.2877344546401,-336.358486869147)) ;
#46592 = CARTESIAN_POINT('Ctrl Pts',(-8.77943710279873,16.3596692485729,-336.360384983473)) ;
#46593 = CARTESIAN_POINT('Ctrl Pts',(-8.54340766658229,16.4838733234786,-336.363714561511)) ;
#46594 = CARTESIAN_POINT('Ctrl Pts',(-8.44048473989926,16.5368108079078,-336.36515144791)) ;
#46595 = CARTESIAN_POINT('Ctrl Pts',(-7.92799232610451,16.7943756369697,-336.372245535503)) ;
#46596 = CARTESIAN_POINT('Ctrl Pts',(-7.51144580523368,16.9847666551633,-336.377824732685)) ;
#46597 = CARTESIAN_POINT('Ctrl Pts',(-6.65203920224582,17.3397710790753,-336.389236300615)) ;
#46598 = CARTESIAN_POINT('Ctrl Pts',(-6.20907781673635,17.5032750621506,-336.395067643566)) ;
#46599 = CARTESIAN_POINT('Ctrl Pts',(-5.61637812750229,17.696715459099,-336.402919173305)) ;
#46600 = CARTESIAN_POINT('Ctrl Pts',(-5.47181755365528,17.7419461695852,-336.404837451913)) ;
#46601 = CARTESIAN_POINT('Ctrl Pts',(-5.20645536693862,17.8214220208331,-336.408367364496)) ;
#46602 = CARTESIAN_POINT('Ctrl Pts',(-5.08582873106328,17.8562203839036,-336.409975186948)) ;
#46603 = CARTESIAN_POINT('Ctrl Pts',(-4.83557718357955,17.9256713587492,-336.413318368301)) ;
#46604 = CARTESIAN_POINT('Ctrl Pts',(-4.70591082589835,17.9601476495753,-336.415054806015)) ;
#46605 = CARTESIAN_POINT('Ctrl Pts',(-4.359162905314,18.0483296469286,-336.419709846822)) ;
#46606 = CARTESIAN_POINT('Ctrl Pts',(-4.14146582230994,18.0995238843538,-336.422644560534)) ;
#46607 = CARTESIAN_POINT('Ctrl Pts',(-3.77235242304641,18.1793173565713,-336.427637610606)) ;
#46608 = CARTESIAN_POINT('Ctrl Pts',(-3.62140831640021,18.2099869325782,-336.429684178304)) ;
#46609 = CARTESIAN_POINT('Ctrl Pts',(-2.93905272368347,18.3398115688181,-336.438950116827)) ;
#46610 = CARTESIAN_POINT('Ctrl Pts',(-2.40384617198713,18.4176068208539,-336.446264957943)) ;
#46611 = CARTESIAN_POINT('Ctrl Pts',(-1.53704327125577,18.5051701383092,-336.457965816601)) ;
#46612 = CARTESIAN_POINT('Ctrl Pts',(-1.20724530034186,18.5296082914501,-336.462381810492)) ;
#46613 = CARTESIAN_POINT('Ctrl Pts',(-0.779263766545773,18.5498467749549,
-336.468000768131)) ;
#46614 = CARTESIAN_POINT('Ctrl Pts',(-0.681521750322263,18.553694929485,-336.469276396151)) ;
#46615 = CARTESIAN_POINT('Ctrl Pts',(-0.517398984326241,18.5588578585254,
-336.471403001518)) ;
#46616 = CARTESIAN_POINT('Ctrl Pts',(-0.451033429609828,18.5605893118278,
-336.472258637513)) ;
#46617 = CARTESIAN_POINT('Ctrl Pts',(-0.304084826244664,18.5636345291202,
-336.47414318028)) ;
#46618 = CARTESIAN_POINT('Ctrl Pts',(-0.223499784666542,18.5647796211695,
-336.475170207338)) ;
#46619 = CARTESIAN_POINT('Ctrl Pts',(0.036020094517566,18.566777311963,-336.478460301196)) ;
#46620 = CARTESIAN_POINT('Ctrl Pts',(0.214960839268421,18.5655678403829,-336.480702292379)) ;
#46621 = CARTESIAN_POINT('Ctrl Pts',(0.677749457253094,18.555748076693,-336.486459320058)) ;
#46622 = CARTESIAN_POINT('Ctrl Pts',(0.961467449650487,18.5432120131931,-336.489948842773)) ;
#46623 = CARTESIAN_POINT('Ctrl Pts',(1.95154972364018,18.476680525379,-336.50211387363)) ;
#46624 = CARTESIAN_POINT('Ctrl Pts',(2.6550166336632,18.3887779855933,-336.510757857971)) ;
#46625 = CARTESIAN_POINT('Ctrl Pts',(3.50492264461624,18.2327801975812,-336.521630436128)) ;
#46626 = CARTESIAN_POINT('Ctrl Pts',(3.65775039657228,18.2027365640732,-336.523601459922)) ;
#46627 = CARTESIAN_POINT('Ctrl Pts',(3.93394980712235,18.1448210340557,-336.527195527761)) ;
#46628 = CARTESIAN_POINT('Ctrl Pts',(4.05744924656672,18.1176046154292,-336.52881420291)) ;
#46629 = CARTESIAN_POINT('Ctrl Pts',(4.30976856864022,18.0592899481375,-336.532146163601)) ;
#46630 = CARTESIAN_POINT('Ctrl Pts',(4.43855298618197,18.0280699430895,-336.533860177119)) ;
#46631 = CARTESIAN_POINT('Ctrl Pts',(4.77461467731618,17.9427823278538,-336.538368393595)) ;
#46632 = CARTESIAN_POINT('Ctrl Pts',(4.98130956522554,17.8865015513902,-336.541176881499)) ;
#46633 = CARTESIAN_POINT('Ctrl Pts',(5.53186207879498,17.7263084730677,-336.548749409958)) ;
#46634 = CARTESIAN_POINT('Ctrl Pts',(5.87375485722929,17.6159732378403,-336.553550047724)) ;
#46635 = CARTESIAN_POINT('Ctrl Pts',(6.78764964243154,17.2914765934202,-336.566582584134)) ;
#46636 = CARTESIAN_POINT('Ctrl Pts',(7.35263823070325,17.0588997643321,-336.574864915176)) ;
#46637 = CARTESIAN_POINT('Ctrl Pts',(8.02910400955891,16.7405722441362,-336.58474407851)) ;
#46638 = CARTESIAN_POINT('Ctrl Pts',(8.15242160551762,16.6808660543016,-336.586542788729)) ;
#46639 = CARTESIAN_POINT('Ctrl Pts',(8.34071868836916,16.5871121598808,-336.589279634255)) ;
#46640 = CARTESIAN_POINT('Ctrl Pts',(8.4061760203606,16.5540352414931,-336.590229219872)) ;
#46641 = CARTESIAN_POINT('Ctrl Pts',(8.53309748956789,16.4889523188703,-336.59206562258)) ;
#46642 = CARTESIAN_POINT('Ctrl Pts',(8.5945817621173,16.4569883536608,-336.592952910309)) ;
#46643 = CARTESIAN_POINT('Ctrl Pts',(8.75856320618787,16.3705693459544,-336.595314854343)) ;
#46644 = CARTESIAN_POINT('Ctrl Pts',(8.86073123510505,16.3154960755063,-336.596781760389)) ;
#46645 = CARTESIAN_POINT('Ctrl Pts',(9.33009219305828,16.0567797758318,-336.603512783883)) ;
#46646 = CARTESIAN_POINT('Ctrl Pts',(9.69082746740933,15.8416748433257,-336.608666026154)) ;
#46647 = CARTESIAN_POINT('Ctrl Pts',(10.6006441670877,15.2564401155219,-336.621920671892)) ;
#46648 = CARTESIAN_POINT('Ctrl Pts',(11.1377812130958,14.8688415977146,-336.630012512024)) ;
#46649 = CARTESIAN_POINT('Ctrl Pts',(11.7913923492662,14.341866570518,-336.640567700127)) ;
#46650 = CARTESIAN_POINT('Ctrl Pts',(11.9281074994823,14.2283632791518,-336.642816125266)) ;
#46651 = CARTESIAN_POINT('Ctrl Pts',(12.1592659193274,14.0307780337073,-336.646692232955)) ;
#46652 = CARTESIAN_POINT('Ctrl Pts',(12.2545181618922,13.9476616138505,-336.648311705373)) ;
#46653 = CARTESIAN_POINT('Ctrl Pts',(12.4499808924639,13.7735541584542,-336.651682424056)) ;
#46654 = CARTESIAN_POINT('Ctrl Pts',(12.5500601956619,13.6824269556898,-336.653434798297)) ;
#46655 = CARTESIAN_POINT('Ctrl Pts',(12.8177502724778,13.4332735769396,-336.658194765053)) ;
#46656 = CARTESIAN_POINT('Ctrl Pts',(12.9834308579745,13.2732092536153,-336.661219823784)) ;
#46657 = CARTESIAN_POINT('Ctrl Pts',(13.3596863137221,12.8959210111008,-336.668270300761)) ;
#46658 = CARTESIAN_POINT('Ctrl Pts',(13.5680161862333,12.6765505313175,-336.672311651406)) ;
#46659 = CARTESIAN_POINT('Ctrl Pts',(14.2302096695341,11.9442298308755,-336.685569231387)) ;
#46660 = CARTESIAN_POINT('Ctrl Pts',(14.6610688071018,11.4112468122039,-336.694877026294)) ;
#46661 = CARTESIAN_POINT('Ctrl Pts',(15.1261539172385,10.7659739666095,-336.705338237633)) ;
#46662 = CARTESIAN_POINT('Ctrl Pts',(15.1900095341653,10.6756891199396,-336.706783999225)) ;
#46663 = CARTESIAN_POINT('Ctrl Pts',(15.288170164031,10.5342368548669,-336.709017973716)) ;
#46664 = CARTESIAN_POINT('Ctrl Pts',(15.3230335492272,10.4834601133414,-336.709813725017)) ;
#46665 = CARTESIAN_POINT('Ctrl Pts',(15.385586565875,10.3913761498993,-336.711245000505)) ;
#46666 = CARTESIAN_POINT('Ctrl Pts',(15.4133641151279,10.35012941587,-336.711881879415)) ;
#46667 = CARTESIAN_POINT('Ctrl Pts',(15.441858489285,10.3074491668673,-336.712536798886)) ;
#46668 = CARTESIAN_POINT('Ctrl Pts',(15.4427411789722,10.3061266637827,-336.712557088373)) ;
#46669 = CARTESIAN_POINT('Ctrl Pts',(15.4444221621669,10.3036074046309,-336.712595730481)) ;
#46670 = CARTESIAN_POINT('Ctrl Pts',(15.4452204864739,10.3024106691689,-336.712614083518)) ;
#46671 = CARTESIAN_POINT('Ctrl Pts',(15.4994420847522,10.2211088117034,-336.713860698078)) ;
#46672 = CARTESIAN_POINT('Ctrl Pts',(15.5522415945285,10.1405893172973,-336.715080549578)) ;
#46673 = CARTESIAN_POINT('Ctrl Pts',(15.6724090207215,9.95418723447399,-336.717874633862)) ;
#46674 = CARTESIAN_POINT('Ctrl Pts',(15.7393345548186,9.84802497187523,-336.719444054811)) ;
#46675 = CARTESIAN_POINT('Ctrl Pts',(15.9514215635742,9.50391174913691,-336.724472639074)) ;
#46676 = CARTESIAN_POINT('Ctrl Pts',(16.0923027449555,9.2633677026108,-336.727899145572)) ;
#46677 = CARTESIAN_POINT('Ctrl Pts',(16.5758995830656,8.39331280436065,-336.740104247365)) ;
#46678 = CARTESIAN_POINT('Ctrl Pts',(16.8875197914619,7.74724608133012,-336.748846084691)) ;
#46679 = CARTESIAN_POINT('Ctrl Pts',(17.2204232560578,6.94087623535054,-336.759822984308)) ;
#46680 = CARTESIAN_POINT('Ctrl Pts',(17.2780235925646,6.79622252973804,-336.76179335756)) ;
#46681 = CARTESIAN_POINT('Ctrl Pts',(17.3790949499431,6.53280546375797,-336.765386629941)) ;
#46682 = CARTESIAN_POINT('Ctrl Pts',(17.4231849996114,6.41428974418798,-336.767005167114)) ;
#46683 = CARTESIAN_POINT('Ctrl Pts',(17.5069715585861,6.18182846812967,-336.770184421531)) ;
#46684 = CARTESIAN_POINT('Ctrl Pts',(17.5467748201958,6.0679279597706,-336.771744310635)) ;
#46685 = CARTESIAN_POINT('Ctrl Pts',(17.6174090954213,5.85929341465668,-336.774605731026)) ;
#46686 = CARTESIAN_POINT('Ctrl Pts',(17.6485932820567,5.7646836594305,-336.775904834849)) ;
#46687 = CARTESIAN_POINT('Ctrl Pts',(17.7324738574679,5.50313674499995,-336.779500214258)) ;
#46688 = CARTESIAN_POINT('Ctrl Pts',(17.7835729263924,5.33569835938262,-336.781806494656)) ;
#46689 = CARTESIAN_POINT('Ctrl Pts',(17.9228055462893,4.85523251205596,-336.788433577623)) ;
#46690 = CARTESIAN_POINT('Ctrl Pts',(18.0050932671665,4.54057895175931,-336.792785514256)) ;
#46691 = CARTESIAN_POINT('Ctrl Pts',(18.2253194808984,3.59797609250834,-336.805798716501)) ;
#46692 = CARTESIAN_POINT('Ctrl Pts',(18.3389572516868,2.96485225607021,-336.814520758419)) ;
#46693 = CARTESIAN_POINT('Ctrl Pts',(18.4333941711011,2.2173667532049,-336.824429859012)) ;
#46694 = CARTESIAN_POINT('Ctrl Pts',(18.4462784148842,2.10749820449643,-336.825876115381)) ;
#46695 = CARTESIAN_POINT('Ctrl Pts',(18.4648074636674,1.93627971815218,-336.828110659655)) ;
#46696 = CARTESIAN_POINT('Ctrl Pts',(18.4711301000094,1.87500577749903,-336.828906492121)) ;
#46697 = CARTESIAN_POINT('Ctrl Pts',(18.483054996078,1.75352047544371,-336.830475967602)) ;
#46698 = CARTESIAN_POINT('Ctrl Pts',(18.4886682591311,1.6933109756913,-336.831249776767)) ;
#46699 = CARTESIAN_POINT('Ctrl Pts',(18.5004714635441,1.55964393623653,-336.832959678667)) ;
#46700 = CARTESIAN_POINT('Ctrl Pts',(18.5065182621756,1.48617475751466,-336.833894173919)) ;
#46701 = CARTESIAN_POINT('Ctrl Pts',(18.5208048449971,1.29895851735991,-336.836263861446)) ;
#46702 = CARTESIAN_POINT('Ctrl Pts',(18.5284344295844,1.18516791004337,-336.837693260093)) ;
#46703 = CARTESIAN_POINT('Ctrl Pts',(18.5727468430842,0.418510199645596,-336.847268754458)) ;
#46704 = CARTESIAN_POINT('Ctrl Pts',(18.5759646867155,-0.235832692476801,
-336.855190346612)) ;
#46705 = CARTESIAN_POINT('Ctrl Pts',(18.544654593745,-0.888979977948838,-336.86323988221)) ;
#46706 = CARTESIAN_POINT('Origin',(0.,0.,-315.477129595899)) ;
#46707 = CARTESIAN_POINT('',(1.74714810520642,18.4835595300519,-338.)) ;
#46708 = CARTESIAN_POINT('Ctrl Pts',(18.544654593745,-0.88897997794884,-336.86323988221)) ;
#46709 = CARTESIAN_POINT('Ctrl Pts',(18.5265686305932,-1.26626399779565,-336.867889616222)) ;
#46710 = CARTESIAN_POINT('Ctrl Pts',(18.4969733686538,-1.64290749982776,-336.872575171038)) ;
#46711 = CARTESIAN_POINT('Ctrl Pts',(18.4415834579998,-2.14938732150166,-336.878990748352)) ;
#46712 = CARTESIAN_POINT('Ctrl Pts',(18.4258623126442,-2.28023338170186,-336.880658333735)) ;
#46713 = CARTESIAN_POINT('Ctrl Pts',(18.393655079212,-2.52615593426246,-336.883813539215)) ;
#46714 = CARTESIAN_POINT('Ctrl Pts',(18.3774786508234,-2.64126662313804,-336.885299110609)) ;
#46715 = CARTESIAN_POINT('Ctrl Pts',(18.3414912639957,-2.88099239673001,-336.888411946457)) ;
#46716 = CARTESIAN_POINT('Ctrl Pts',(18.3214887815987,-3.00557278223992,-336.890040393454)) ;
#46717 = CARTESIAN_POINT('Ctrl Pts',(18.2691318471016,-3.31169477659058,-336.894068946227)) ;
#46718 = CARTESIAN_POINT('Ctrl Pts',(18.2353397246696,-3.49297662515185,-336.896478224894)) ;
#46719 = CARTESIAN_POINT('Ctrl Pts',(18.1060003392576,-4.13369649534109,-336.905075295906)) ;
#46720 = CARTESIAN_POINT('Ctrl Pts',(17.9957429284565,-4.58998140408656,-336.911351892757)) ;
#46721 = CARTESIAN_POINT('Ctrl Pts',(17.7119139045931,-5.5959221044881,-336.925414311519)) ;
#46722 = CARTESIAN_POINT('Ctrl Pts',(17.5297990794366,-6.14266904028077,-336.93321430086)) ;
#46723 = CARTESIAN_POINT('Ctrl Pts',(17.2810249938321,-6.7877834091317,-336.942337520284)) ;
#46724 = CARTESIAN_POINT('Ctrl Pts',(17.2384814132826,-6.8951132746513,-336.943852235716)) ;
#46725 = CARTESIAN_POINT('Ctrl Pts',(17.171257265604,-7.06019591400926,-336.946173375537)) ;
#46726 = CARTESIAN_POINT('Ctrl Pts',(17.1472801556599,-7.11823192237263,-336.946987727237)) ;
#46727 = CARTESIAN_POINT('Ctrl Pts',(17.0974213867107,-7.23719999332893,-336.94865279573)) ;
#46728 = CARTESIAN_POINT('Ctrl Pts',(17.0715074014463,-7.29811735020341,-336.949502912958)) ;
#46729 = CARTESIAN_POINT('Ctrl Pts',(17.0071843443249,-7.44710762215979,-336.951576730206)) ;
#46730 = CARTESIAN_POINT('Ctrl Pts',(16.9684163292498,-7.53502346202996,-336.952795992257)) ;
#46731 = CARTESIAN_POINT('Ctrl Pts',(16.8024443076704,-7.90362764754281,-336.95789645455)) ;
#46732 = CARTESIAN_POINT('Ctrl Pts',(16.6689442964888,-8.18142784433175,-336.961712887694)) ;
#46733 = CARTESIAN_POINT('Ctrl Pts',(16.4869757416514,-8.53712360864424,-336.966629076275)) ;
#46734 = CARTESIAN_POINT('Ctrl Pts',(16.4447598828384,-8.61816227620197,-336.967751106731)) ;
#46735 = CARTESIAN_POINT('Ctrl Pts',(16.1701554218104,-9.13593523586149,-336.974940055253)) ;
#46736 = CARTESIAN_POINT('Ctrl Pts',(15.9209872872141,-9.56354551294087,-336.980975123815)) ;
#46737 = CARTESIAN_POINT('Ctrl Pts',(15.5389315482835,-10.1628123343842,-336.98977773544)) ;
#46738 = CARTESIAN_POINT('Ctrl Pts',(15.4196541204778,-10.3428919946753,-336.99246887544)) ;
#46739 = CARTESIAN_POINT('Ctrl Pts',(15.200159035679,-10.6620367470411,-336.99733432259)) ;
#46740 = CARTESIAN_POINT('Ctrl Pts',(15.1011060513966,-10.8018729027347,-336.999500238586)) ;
#46741 = CARTESIAN_POINT('Ctrl Pts',(14.9358094690646,-11.0285089633956,-337.003070634853)) ;
#46742 = CARTESIAN_POINT('Ctrl Pts',(14.8707108383856,-11.116131232529,-337.004466034893)) ;
#46743 = CARTESIAN_POINT('Ctrl Pts',(14.728750532445,-11.3037298578851,-337.007486879867)) ;
#46744 = CARTESIAN_POINT('Ctrl Pts',(14.6516353065675,-11.4035075190406,-337.009114336854)) ;
#46745 = CARTESIAN_POINT('Ctrl Pts',(14.4780317605986,-11.6234609876665,-337.012748953348)) ;
#46746 = CARTESIAN_POINT('Ctrl Pts',(14.381051499472,-11.7432366350648,-337.014760041866)) ;
#46747 = CARTESIAN_POINT('Ctrl Pts',(13.771784871978,-12.4768447721432,-337.027275009489)) ;
#46748 = CARTESIAN_POINT('Ctrl Pts',(13.2217835308721,-13.0582595354045,-337.038103053513)) ;
#46749 = CARTESIAN_POINT('Ctrl Pts',(12.4671662859456,-13.7592653897275,-337.051937970139)) ;
#46750 = CARTESIAN_POINT('Ctrl Pts',(12.2953997165666,-13.912971117315,-337.055021905454)) ;
#46751 = CARTESIAN_POINT('Ctrl Pts',(12.0356866446258,-14.1368092786094,-337.059565249018)) ;
#46752 = CARTESIAN_POINT('Ctrl Pts',(11.9498927894016,-14.2094050529352,-337.06104724391)) ;
#46753 = CARTESIAN_POINT('Ctrl Pts',(11.8622583982412,-14.2822031730269,-337.062539867073)) ;
#46754 = CARTESIAN_POINT('Ctrl Pts',(11.8610716462739,-14.2831887610653,-337.062560076389)) ;
#46755 = CARTESIAN_POINT('Ctrl Pts',(11.8588167939988,-14.2850609230665,-337.062598467058)) ;
#46756 = CARTESIAN_POINT('Ctrl Pts',(11.857748717066,-14.2859475251827,-337.062616648757)) ;
#46757 = CARTESIAN_POINT('Ctrl Pts',(11.8557184002759,-14.2876324903445,-337.06265120448)) ;
#46758 = CARTESIAN_POINT('Ctrl Pts',(11.8547561791747,-14.2884308759957,-337.062667578783)) ;
#46759 = CARTESIAN_POINT('Ctrl Pts',(11.8529262878602,-14.2899488833151,-337.062698713501)) ;
#46760 = CARTESIAN_POINT('Ctrl Pts',(11.8520586327732,-14.2906685231487,-337.06271347414)) ;
#46761 = CARTESIAN_POINT('Ctrl Pts',(11.8504079135291,-14.2920373887053,-337.062741552363)) ;
#46762 = CARTESIAN_POINT('Ctrl Pts',(11.8496248615414,-14.2926866291094,-337.062754870128)) ;
#46763 = CARTESIAN_POINT('Ctrl Pts',(11.8481345415857,-14.2939220695666,-337.062780213511)) ;
#46764 = CARTESIAN_POINT('Ctrl Pts',(11.8474272834421,-14.2945082815013,-337.062792239277)) ;
#46765 = CARTESIAN_POINT('Ctrl Pts',(11.8460807488733,-14.2956241900424,-337.062815132237)) ;
#46766 = CARTESIAN_POINT('Ctrl Pts',(11.8454414803834,-14.2961538962955,-337.062825999552)) ;
#46767 = CARTESIAN_POINT('Ctrl Pts',(11.8427935936528,-14.2983476704235,-337.062871007874)) ;
#46768 = CARTESIAN_POINT('Ctrl Pts',(11.8407846602433,-14.3000113578946,-337.062905144134)) ;
#46769 = CARTESIAN_POINT('Ctrl Pts',(11.8368450296075,-14.3032725425738,-337.062972065145)) ;
#46770 = CARTESIAN_POINT('Ctrl Pts',(11.8349143594196,-14.3048700723667,-337.063004850307)) ;
#46771 = CARTESIAN_POINT('Ctrl Pts',(11.8311267191055,-14.3080028572933,-337.063069148663)) ;
#46772 = CARTESIAN_POINT('Ctrl Pts',(11.8292697734438,-14.3095381419155,-337.06310066223)) ;
#46773 = CARTESIAN_POINT('Ctrl Pts',(11.8256253309633,-14.3125500980742,-337.063162491824)) ;
#46774 = CARTESIAN_POINT('Ctrl Pts',(11.8238378562684,-14.3140267963588,-337.06319280819)) ;
#46775 = CARTESIAN_POINT('Ctrl Pts',(11.8203283695737,-14.3169250058793,-337.063252313057)) ;
#46776 = CARTESIAN_POINT('Ctrl Pts',(11.8186063776903,-14.3183465413342,-337.063281501867)) ;
#46777 = CARTESIAN_POINT('Ctrl Pts',(11.8152241172785,-14.3211376326448,-337.06333881689)) ;
#46778 = CARTESIAN_POINT('Ctrl Pts',(11.8135638669432,-14.3225072105525,-337.063366943385)) ;
#46779 = CARTESIAN_POINT('Ctrl Pts',(11.8103015799519,-14.3251973914358,-337.063422194947)) ;
#46780 = CARTESIAN_POINT('Ctrl Pts',(11.8086995598674,-14.3265180144305,-337.063449320272)) ;
#46781 = CARTESIAN_POINT('Ctrl Pts',(11.8055504375172,-14.3291131019168,-337.063502626861)) ;
#46782 = CARTESIAN_POINT('Ctrl Pts',(11.8040033503379,-14.3303875846223,-337.06352880836)) ;
#46783 = CARTESIAN_POINT('Ctrl Pts',(11.8009609970708,-14.3328930331323,-337.063580281127)) ;
#46784 = CARTESIAN_POINT('Ctrl Pts',(11.7994657446899,-14.3341240155611,-337.06360557261)) ;
#46785 = CARTESIAN_POINT('Ctrl Pts',(11.7965241496713,-14.3365449427886,-337.063655315887)) ;
#46786 = CARTESIAN_POINT('Ctrl Pts',(11.795077819522,-14.3377349027591,-337.063679767879)) ;
#46787 = CARTESIAN_POINT('Ctrl Pts',(11.7922313302171,-14.3400761135696,-337.063727879664)) ;
#46788 = CARTESIAN_POINT('Ctrl Pts',(11.790831182477,-14.3412273782494,-337.063751539637)) ;
#46789 = CARTESIAN_POINT('Ctrl Pts',(11.788074480017,-14.3434933868624,-337.063798112034)) ;
#46790 = CARTESIAN_POINT('Ctrl Pts',(11.7867179357019,-14.3446081434663,-337.063821024624)) ;
#46791 = CARTESIAN_POINT('Ctrl Pts',(11.7840460118055,-14.3468031941408,-337.063866144261)) ;
#46792 = CARTESIAN_POINT('Ctrl Pts',(11.7827306417714,-14.3478834997786,-337.063888351462)) ;
#46793 = CARTESIAN_POINT('Ctrl Pts',(11.7801387775574,-14.3500115857538,-337.063932099874)) ;
#46794 = CARTESIAN_POINT('Ctrl Pts',(11.7788622921383,-14.3510593766671,-337.063953641226)) ;
#46795 = CARTESIAN_POINT('Ctrl Pts',(11.7763460381555,-14.3531242579314,-337.063996095212)) ;
#46796 = CARTESIAN_POINT('Ctrl Pts',(11.7751062775822,-14.3541413580069,-337.064017007974)) ;
#46797 = CARTESIAN_POINT('Ctrl Pts',(11.7726614351801,-14.3561465778156,-337.064058239928)) ;
#46798 = CARTESIAN_POINT('Ctrl Pts',(11.7714563606991,-14.3571347064538,-337.064078559237)) ;
#46799 = CARTESIAN_POINT('Ctrl Pts',(11.7690789649703,-14.3590836064218,-337.064118637456)) ;
#46800 = CARTESIAN_POINT('Ctrl Pts',(11.7679066504242,-14.3600443859628,-337.064138396474)) ;
#46801 = CARTESIAN_POINT('Ctrl Pts',(11.7655929538511,-14.3619401204602,-337.064177385446)) ;
#46802 = CARTESIAN_POINT('Ctrl Pts',(11.7644515779945,-14.3628750829497,-337.064196615501)) ;
#46803 = CARTESIAN_POINT('Ctrl Pts',(11.7621980356222,-14.3647206321386,-337.064234576172)) ;
#46804 = CARTESIAN_POINT('Ctrl Pts',(11.7610858748104,-14.3656312257386,-337.064253306882)) ;
#46805 = CARTESIAN_POINT('Ctrl Pts',(11.7588891301807,-14.3674294078918,-337.064290296904)) ;
#46806 = CARTESIAN_POINT('Ctrl Pts',(11.7578045515846,-14.3683170028146,-337.064308556302)) ;
#46807 = CARTESIAN_POINT('Ctrl Pts',(11.7556614235258,-14.3700704858472,-337.064344630265)) ;
#46808 = CARTESIAN_POINT('Ctrl Pts',(11.7546028788573,-14.370936379831,-337.06436244491)) ;
#46809 = CARTESIAN_POINT('Ctrl Pts',(11.7525103493197,-14.3726476919004,-337.064397654559)) ;
#46810 = CARTESIAN_POINT('Ctrl Pts',(11.7514763688978,-14.3734931153702,-337.064415049637)) ;
#46811 = CARTESIAN_POINT('Ctrl Pts',(11.6920605738015,-14.4220631330692,-337.065414450741)) ;
#46812 = CARTESIAN_POINT('Ctrl Pts',(11.6333885845426,-14.4694317627552,-337.066391622801)) ;
#46813 = CARTESIAN_POINT('Ctrl Pts',(11.5218290913369,-14.5583817636873,-337.068229968658)) ;
#46814 = CARTESIAN_POINT('Ctrl Pts',(11.4690010690042,-14.6000356046604,-337.069092143294)) ;
#46815 = CARTESIAN_POINT('Ctrl Pts',(11.3303910663484,-14.7081102701367,-337.071333973471)) ;
#46816 = CARTESIAN_POINT('Ctrl Pts',(11.2442511345906,-14.774068021703,-337.07270707896)) ;
#46817 = CARTESIAN_POINT('Ctrl Pts',(10.9625272986188,-14.9858941441139,-337.077141026413)) ;
#46818 = CARTESIAN_POINT('Ctrl Pts',(10.7646448538793,-15.1286631809299,-337.080167777639)) ;
#46819 = CARTESIAN_POINT('Ctrl Pts',(10.0803296811316,-15.6021600812877,-337.090426481884)) ;
#46820 = CARTESIAN_POINT('Ctrl Pts',(9.58102302231907,-15.9136559291941,-337.097571645627)) ;
#46821 = CARTESIAN_POINT('Ctrl Pts',(8.92787418422019,-16.2792280331928,-337.106824502396)) ;
#46822 = CARTESIAN_POINT('Ctrl Pts',(8.78696583365569,-16.3557156422516,-337.108814518315)) ;
#46823 = CARTESIAN_POINT('Ctrl Pts',(8.44182682730863,-16.537315702751,-337.113681850263)) ;
#46824 = CARTESIAN_POINT('Ctrl Pts',(8.23660228988048,-16.640481762122,-337.116570339585)) ;
#46825 = CARTESIAN_POINT('Ctrl Pts',(7.9075873222291,-16.7982990067202,-337.121202475483)) ;
#46826 = CARTESIAN_POINT('Ctrl Pts',(7.78502249357073,-16.8554504979229,-337.12292825858)) ;
#46827 = CARTESIAN_POINT('Ctrl Pts',(7.54664839825791,-16.9634486868319,-337.126286523949)) ;
#46828 = CARTESIAN_POINT('Ctrl Pts',(7.43092229329707,-17.0144611203132,-337.127917713177)) ;
#46829 = CARTESIAN_POINT('Ctrl Pts',(7.17693372168415,-17.123334474387,-337.131500046504)) ;
#46830 = CARTESIAN_POINT('Ctrl Pts',(7.03847352728636,-17.1807116117197,-337.133454419095)) ;
#46831 = CARTESIAN_POINT('Ctrl Pts',(6.4693413726946,-17.4085220274516,-337.141492907344)) ;
#46832 = CARTESIAN_POINT('Ctrl Pts',(6.03306002502255,-17.564486941311,-337.147671475266)) ;
#46833 = CARTESIAN_POINT('Ctrl Pts',(5.5451686283761,-17.7185765615315,-337.154547432412)) ;
#46834 = CARTESIAN_POINT('Ctrl Pts',(5.49887484141452,-17.7329982225645,-337.15519947808)) ;
#46835 = CARTESIAN_POINT('Ctrl Pts',(5.04014202546078,-17.8739357667677,-337.161656023324)) ;
#46836 = CARTESIAN_POINT('Ctrl Pts',(4.6234682830375,-17.9862211861031,-337.167486666762)) ;
#46837 = CARTESIAN_POINT('Ctrl Pts',(3.98240262974287,-18.135224923981,-337.176271801821)) ;
#46838 = CARTESIAN_POINT('Ctrl Pts',(3.76062041774433,-18.1825094024561,-337.179277074822)) ;
#46839 = CARTESIAN_POINT('Ctrl Pts',(3.45244364155189,-18.2423335387018,-337.183382237448)) ;
#46840 = CARTESIAN_POINT('Ctrl Pts',(3.36674362992775,-18.2583443224037,-337.18451626699)) ;
#46841 = CARTESIAN_POINT('Ctrl Pts',(3.22261795783564,-18.2842211560227,-337.186408893294)) ;
#46842 = CARTESIAN_POINT('Ctrl Pts',(3.16425228019977,-18.294412188025,-337.18717125781)) ;
#46843 = CARTESIAN_POINT('Ctrl Pts',(3.02247713089083,-18.3184682929686,-337.189013191714)) ;
#46844 = CARTESIAN_POINT('Ctrl Pts',(2.93901992079468,-18.3320432723602,-337.19008936472)) ;
#46845 = CARTESIAN_POINT('Ctrl Pts',(2.6731990927211,-18.3734192428039,-337.193495147808)) ;
#46846 = CARTESIAN_POINT('Ctrl Pts',(2.49051232565694,-18.3990727110932,-337.195803066356)) ;
#46847 = CARTESIAN_POINT('Ctrl Pts',(2.02627700329742,-18.457221158992,-337.201614160078)) ;
#46848 = CARTESIAN_POINT('Ctrl Pts',(1.74431061402484,-18.4859998991031,-337.205094199303)) ;
#46849 = CARTESIAN_POINT('Ctrl Pts',(0.996331021764724,-18.5450757085032,
-337.214289850893)) ;
#46850 = CARTESIAN_POINT('Ctrl Pts',(0.529644850950633,-18.56426633708,-337.219993725895)) ;
#46851 = CARTESIAN_POINT('Ctrl Pts',(-0.235706945328343,-18.5668524318551,
-337.229480335364)) ;
#46852 = CARTESIAN_POINT('Ctrl Pts',(-0.534127537944787,-18.5606647030296,
-337.233211113626)) ;
#46853 = CARTESIAN_POINT('Ctrl Pts',(-0.978497295567214,-18.5407245906999,
-337.238839077589)) ;
#46854 = CARTESIAN_POINT('Ctrl Pts',(-1.12464317494191,-18.5324338108651,
-337.240701587462)) ;
#46855 = CARTESIAN_POINT('Ctrl Pts',(-1.39446233738143,-18.5139236649315,
-337.244163571441)) ;
#46856 = CARTESIAN_POINT('Ctrl Pts',(-1.51816075258351,-18.5041909458274,
-337.245759796679)) ;
#46857 = CARTESIAN_POINT('Ctrl Pts',(-1.79737939195762,-18.4794030593261,
-337.249384109079)) ;
#46858 = CARTESIAN_POINT('Ctrl Pts',(-1.95282580772015,-18.4636231918855,
-337.25141676978)) ;
#46859 = CARTESIAN_POINT('Ctrl Pts',(-2.45317658527703,-18.4064415098261,
-337.258007388268)) ;
#46860 = CARTESIAN_POINT('Ctrl Pts',(-2.79712308874901,-18.357321859942,-337.262612671676)) ;
#46861 = CARTESIAN_POINT('Ctrl Pts',(-3.80889548323213,-18.1837320594787,
-337.276337332927)) ;
#46862 = CARTESIAN_POINT('Ctrl Pts',(-4.47149450999833,-18.0322358609752,
-337.28557207522)) ;
#46863 = CARTESIAN_POINT('Ctrl Pts',(-5.30201063540625,-17.7937452062654,
-337.297060982794)) ;
#46864 = CARTESIAN_POINT('Ctrl Pts',(-5.47895084124401,-17.7400615312942,
-337.299502097368)) ;
#46865 = CARTESIAN_POINT('Ctrl Pts',(-5.73269425455235,-17.6589172785579,
-337.30297944206)) ;
#46866 = CARTESIAN_POINT('Ctrl Pts',(-5.81016442807697,-17.6335796765932,
-337.304037923689)) ;
#46867 = CARTESIAN_POINT('Ctrl Pts',(-5.95027316648523,-17.5867317746885,
-337.305944827105)) ;
#46868 = CARTESIAN_POINT('Ctrl Pts',(-6.01296807900864,-17.5653949613401,
-337.306795246113)) ;
#46869 = CARTESIAN_POINT('Ctrl Pts',(-6.16655045187865,-17.5122080175102,
-337.308872168392)) ;
#46870 = CARTESIAN_POINT('Ctrl Pts',(-6.25730681961934,-17.4799852839671,
-337.310094198476)) ;
#46871 = CARTESIAN_POINT('Ctrl Pts',(-6.63915278250707,-17.3410572739465,
-337.315220708546)) ;
#46872 = CARTESIAN_POINT('Ctrl Pts',(-6.92779702139999,-17.227775431521,-337.319059669787)) ;
#46873 = CARTESIAN_POINT('Ctrl Pts',(-7.72750271517918,-16.8905716541226,
-337.329737712685)) ;
#46874 = CARTESIAN_POINT('Ctrl Pts',(-8.23150561821859,-16.6507665024935,
-337.33652349363)) ;
#46875 = CARTESIAN_POINT('Ctrl Pts',(-8.92456338412012,-16.2818401990359,
-337.346234643413)) ;
#46876 = CARTESIAN_POINT('Ctrl Pts',(-9.12320383029136,-16.171372963148,-337.349062498541)) ;
#46877 = CARTESIAN_POINT('Ctrl Pts',(-9.48364583691386,-15.9621698076591,
-337.354291929071)) ;
#46878 = CARTESIAN_POINT('Ctrl Pts',(-9.6460598693921,-15.8645495416576,-337.356685837561)) ;
#46879 = CARTESIAN_POINT('Ctrl Pts',(-9.91585921733149,-15.6967094195172,
-337.360731313816)) ;
#46880 = CARTESIAN_POINT('Ctrl Pts',(-10.0240623959671,-15.6278317000411,
-337.362372684548)) ;
#46881 = CARTESIAN_POINT('Ctrl Pts',(-10.2290641077171,-15.4943309127415,
-337.365519765013)) ;
#46882 = CARTESIAN_POINT('Ctrl Pts',(-10.325985789075,-15.4299079840115,-337.367023877579)) ;
#46883 = CARTESIAN_POINT('Ctrl Pts',(-10.584066772803,-15.2548432216093,-337.371073092722)) ;
#46884 = CARTESIAN_POINT('Ctrl Pts',(-10.7440948709388,-15.1425604301122,
-337.373630714292)) ;
#46885 = CARTESIAN_POINT('Ctrl Pts',(-11.1775747870512,-14.8280802293311,
-337.380685921552)) ;
#46886 = CARTESIAN_POINT('Ctrl Pts',(-11.4472908159555,-14.6208643235309,
-337.385218821993)) ;
#46887 = CARTESIAN_POINT('Ctrl Pts',(-12.108585815896,-14.0832868764024,-337.396651785194)) ;
#46888 = CARTESIAN_POINT('Ctrl Pts',(-12.4924694559441,-13.743908685068,-337.403587703407)) ;
#46889 = CARTESIAN_POINT('Ctrl Pts',(-12.9849056572438,-13.2708647267054,
-337.412715766089)) ;
#46890 = CARTESIAN_POINT('Ctrl Pts',(-13.1063463126288,-13.150943387666,-337.414986140838)) ;
#46891 = CARTESIAN_POINT('Ctrl Pts',(-13.3154922174194,-12.9386392466927,
-337.41891798456)) ;
#46892 = CARTESIAN_POINT('Ctrl Pts',(-13.4039322894773,-12.8469964508616,
-337.420587640591)) ;
#46893 = CARTESIAN_POINT('Ctrl Pts',(-13.5405272124373,-12.7025088645293,
-337.423172378803)) ;
#46894 = CARTESIAN_POINT('Ctrl Pts',(-13.5893315541714,-12.6502836558196,
-337.424097098684)) ;
#46895 = CARTESIAN_POINT('Ctrl Pts',(-13.6858676359047,-12.545777687681,-337.425927414341)) ;
#46896 = CARTESIAN_POINT('Ctrl Pts',(-13.7336043834825,-12.4935031671368,
-337.426833075017)) ;
#46897 = CARTESIAN_POINT('Ctrl Pts',(-13.8640542818238,-12.3490017901589,
-337.429311513389)) ;
#46898 = CARTESIAN_POINT('Ctrl Pts',(-13.9461452137241,-12.2562180176238,
-337.430875159676)) ;
#46899 = CARTESIAN_POINT('Ctrl Pts',(-14.3307413724206,-11.8126584497127,
-337.438237118602)) ;
#46900 = CARTESIAN_POINT('Ctrl Pts',(-14.6209792888549,-11.4514634335351,
-337.443905122343)) ;
#46901 = CARTESIAN_POINT('Ctrl Pts',(-15.2475728792096,-10.6089730350663,
-337.456764864175)) ;
#46902 = CARTESIAN_POINT('Ctrl Pts',(-15.5752232609312,-10.1218183474588,
-337.463957871749)) ;
#46903 = CARTESIAN_POINT('Ctrl Pts',(-15.9754219479083,-9.46122825371702,
-337.473655222031)) ;
#46904 = CARTESIAN_POINT('Ctrl Pts',(-16.0692045420226,-9.30105433343085,
-337.476001246936)) ;
#46905 = CARTESIAN_POINT('Ctrl Pts',(-16.2227691078573,-9.0295197336975,-337.479974349549)) ;
#46906 = CARTESIAN_POINT('Ctrl Pts',(-16.2838441178181,-8.91890603389366,
-337.481591728708)) ;
#46907 = CARTESIAN_POINT('Ctrl Pts',(-16.4067146228485,-8.69090391719736,
-337.484924261849)) ;
#46908 = CARTESIAN_POINT('Ctrl Pts',(-16.4683906917594,-8.57345925369965,
-337.4866401775)) ;
#46909 = CARTESIAN_POINT('Ctrl Pts',(-16.6267413860339,-8.26391049300647,
-337.491161467706)) ;
#46910 = CARTESIAN_POINT('Ctrl Pts',(-16.7213460209501,-8.07077026994344,
-337.493981290446)) ;
#46911 = CARTESIAN_POINT('Ctrl Pts',(-16.9283433989182,-7.6289031758779,-337.500426189572)) ;
#46912 = CARTESIAN_POINT('Ctrl Pts',(-17.0386498298657,-7.37925372014498,
-337.504063264857)) ;
#46913 = CARTESIAN_POINT('Ctrl Pts',(-17.27823779395,-6.80296591064329,-337.51242712722)) ;
#46914 = CARTESIAN_POINT('Ctrl Pts',(-17.4038334501075,-6.47490751718258,
-337.517166050968)) ;
#46915 = CARTESIAN_POINT('Ctrl Pts',(-17.6466274330943,-5.7825053639327,-337.527042224929)) ;
#46916 = CARTESIAN_POINT('Ctrl Pts',(-17.76202027054,-5.41769922020092,-337.53217516624)) ;
#46917 = CARTESIAN_POINT('Ctrl Pts',(-17.8973433960072,-4.93890952795463,
-337.538724687259)) ;
#46918 = CARTESIAN_POINT('Ctrl Pts',(-17.92759631809,-4.82794141198704,-337.540229592352)) ;
#46919 = CARTESIAN_POINT('Ctrl Pts',(-17.9726487986361,-4.65642335048746,
-337.542531799876)) ;
#46920 = CARTESIAN_POINT('Ctrl Pts',(-17.9881778285759,-4.5960680671048,-337.543337387056)) ;
#46921 = CARTESIAN_POINT('Ctrl Pts',(-18.0207565375332,-4.46675265129384,
-337.545052846509)) ;
#46922 = CARTESIAN_POINT('Ctrl Pts',(-18.0377149310502,-4.39777051644626,
-337.545961530433)) ;
#46923 = CARTESIAN_POINT('Ctrl Pts',(-18.0834437031337,-4.20704320568332,
-337.548458233123)) ;
#46924 = CARTESIAN_POINT('Ctrl Pts',(-18.1113801670703,-4.08510186161933,
-337.55003690287)) ;
#46925 = CARTESIAN_POINT('Ctrl Pts',(-18.1736031830096,-3.80030795651262,
-337.553691663373)) ;
#46926 = CARTESIAN_POINT('Ctrl Pts',(-18.206936780322,-3.63725809095476,-337.555759699621)) ;
#46927 = CARTESIAN_POINT('Ctrl Pts',(-18.3285272357752,-2.9988830609984,-337.563793052122)) ;
#46928 = CARTESIAN_POINT('Ctrl Pts',(-18.4003974450696,-2.5206319216884,-337.569679408035)) ;
#46929 = CARTESIAN_POINT('Ctrl Pts',(-18.4955769143574,-1.65970475933777,
-337.580319714443)) ;
#46930 = CARTESIAN_POINT('Ctrl Pts',(-18.5258602755883,-1.27807884560058,
-337.585050441076)) ;
#46931 = CARTESIAN_POINT('Ctrl Pts',(-18.5536265740605,-0.703271364018113,
-337.592267949947)) ;
#46932 = CARTESIAN_POINT('Ctrl Pts',(-18.559927741788,-0.510618945880516,
-337.594702036229)) ;
#46933 = CARTESIAN_POINT('Ctrl Pts',(-18.5652136896176,-0.201958564616765,
-337.598631289096)) ;
#46934 = CARTESIAN_POINT('Ctrl Pts',(-18.5661129745813,-0.0859975408256846,
-337.60011409432)) ;
#46935 = CARTESIAN_POINT('Ctrl Pts',(-18.5657180975435,0.158669720775562,
-337.603257501209)) ;
#46936 = CARTESIAN_POINT('Ctrl Pts',(-18.5641720332945,0.287369481770842,
-337.604919654319)) ;
#46937 = CARTESIAN_POINT('Ctrl Pts',(-18.5569820045037,0.608144766603883,
-337.609084567169)) ;
#46938 = CARTESIAN_POINT('Ctrl Pts',(-18.5496941171968,0.80016820018835,-337.611597635363)) ;
#46939 = CARTESIAN_POINT('Ctrl Pts',(-18.5270390753093,1.22354827122444,-337.617180564022)) ;
#46940 = CARTESIAN_POINT('Ctrl Pts',(-18.5103161295274,1.45480025580107,-337.620257828346)) ;
#46941 = CARTESIAN_POINT('Ctrl Pts',(-18.4359831066122,2.27011795631746,-337.631188282154)) ;
#46942 = CARTESIAN_POINT('Ctrl Pts',(-18.3550185601147,2.85170125926168,-337.639142900375)) ;
#46943 = CARTESIAN_POINT('Ctrl Pts',(-18.1992201466161,3.68087530499706,-337.650444836503)) ;
#46944 = CARTESIAN_POINT('Ctrl Pts',(-18.1465620100062,3.93226964993906,-337.653864249844)) ;
#46945 = CARTESIAN_POINT('Ctrl Pts',(-18.0655154317374,4.28278511303226,-337.658587995002)) ;
#46946 = CARTESIAN_POINT('Ctrl Pts',(-18.0414915030655,4.38288495512111,-337.659931884344)) ;
#46947 = CARTESIAN_POINT('Ctrl Pts',(-18.0005995517078,4.54723284426785,-337.662126996871)) ;
#46948 = CARTESIAN_POINT('Ctrl Pts',(-17.9842170348184,4.61159933694331,-337.662983785051)) ;
#46949 = CARTESIAN_POINT('Ctrl Pts',(-17.9479255697805,4.75105265245432,-337.664832950561)) ;
#46950 = CARTESIAN_POINT('Ctrl Pts',(-17.9278900880458,4.82610511464074,-337.665823872147)) ;
#46951 = CARTESIAN_POINT('Ctrl Pts',(-17.864884077229,5.05631650141751,-337.668853042459)) ;
#46952 = CARTESIAN_POINT('Ctrl Pts',(-17.8203658314698,5.21104417927811,-337.67087457091)) ;
#46953 = CARTESIAN_POINT('Ctrl Pts',(-17.7370323068503,5.48711294392608,-337.674469438548)) ;
#46954 = CARTESIAN_POINT('Ctrl Pts',(-17.6989699714832,5.60867056538357,-337.676048098802)) ;
#46955 = CARTESIAN_POINT('Ctrl Pts',(-17.4884455814695,6.25751897518943,-337.68447088185)) ;
#46956 = CARTESIAN_POINT('Ctrl Pts',(-17.2936652738147,6.77727198264912,-337.691213435586)) ;
#46957 = CARTESIAN_POINT('Ctrl Pts',(-16.9306458308721,7.62788834156565,-337.702613668866)) ;
#46958 = CARTESIAN_POINT('Ctrl Pts',(-16.7752431429694,7.96383484331001,-337.707213261177)) ;
#46959 = CARTESIAN_POINT('Ctrl Pts',(-16.5387156677983,8.43746242199008,-337.713891698462)) ;
#46960 = CARTESIAN_POINT('Ctrl Pts',(-16.465694324304,8.57909076646474,-337.715913921227)) ;
#46961 = CARTESIAN_POINT('Ctrl Pts',(-16.3324841324128,8.82949090562173,-337.719537102852)) ;
#46962 = CARTESIAN_POINT('Ctrl Pts',(-16.2730088718536,8.93863131544694,-337.72113277668)) ;
#46963 = CARTESIAN_POINT('Ctrl Pts',(-16.1421833388425,9.17306952012986,-337.724596908037)) ;
#46964 = CARTESIAN_POINT('Ctrl Pts',(-16.0704602772,9.29815001843839,-337.726468049733)) ;
#46965 = CARTESIAN_POINT('Ctrl Pts',(-15.8533064937878,9.66683295239111,-337.732051961852)) ;
#46966 = CARTESIAN_POINT('Ctrl Pts',(-15.7037414723527,9.90795081395331,-337.735794467603)) ;
#46967 = CARTESIAN_POINT('Ctrl Pts',(-15.3163663682105,10.5016283984981,-337.745223608137)) ;
#46968 = CARTESIAN_POINT('Ctrl Pts',(-15.0718592724392,10.8496237119391,-337.750948142807)) ;
#46969 = CARTESIAN_POINT('Ctrl Pts',(-14.7941044717809,11.2174082147167,-337.757156588435)) ;
#46970 = CARTESIAN_POINT('Ctrl Pts',(-14.7725050348352,11.2458378600002,-337.757637532124)) ;
#46971 = CARTESIAN_POINT('Ctrl Pts',(-14.6726897587314,11.3764331028436,-337.759851359177)) ;
#46972 = CARTESIAN_POINT('Ctrl Pts',(-14.5934951752647,11.4778462040384,-337.761583385516)) ;
#46973 = CARTESIAN_POINT('Ctrl Pts',(-14.3045982507987,11.8399708502171,-337.767806282188)) ;
#46974 = CARTESIAN_POINT('Ctrl Pts',(-14.0889114889462,12.0958263341312,-337.772276350352)) ;
#46975 = CARTESIAN_POINT('Ctrl Pts',(-13.8008091834959,12.4194163832969,-337.777959490908)) ;
#46976 = CARTESIAN_POINT('Ctrl Pts',(-13.7346028249548,12.4925947145931,-337.77924665296)) ;
#46977 = CARTESIAN_POINT('Ctrl Pts',(-13.6228442058364,12.6141599246285,-337.781385572522)) ;
#46978 = CARTESIAN_POINT('Ctrl Pts',(-13.5776099528982,12.6628362882938,-337.782242135847)) ;
#46979 = CARTESIAN_POINT('Ctrl Pts',(-13.4773947780995,12.7695229846536,-337.784119160409)) ;
#46980 = CARTESIAN_POINT('Ctrl Pts',(-13.4222987196319,12.8274231381388,-337.78513784651)) ;
#46981 = CARTESIAN_POINT('Ctrl Pts',(-13.2452956139777,13.0110457063218,-337.788371702654)) ;
#46982 = CARTESIAN_POINT('Ctrl Pts',(-13.1219828043096,13.1354000222848,-337.790566714488)) ;
#46983 = CARTESIAN_POINT('Ctrl Pts',(-12.8010380576781,13.4500250669684,-337.796158611634)) ;
#46984 = CARTESIAN_POINT('Ctrl Pts',(-12.6009147774146,13.6376939697119,-337.799531626368)) ;
#46985 = CARTESIAN_POINT('Ctrl Pts',(-11.8531490633726,14.3084071101835,-337.811848320548)) ;
#46986 = CARTESIAN_POINT('Ctrl Pts',(-11.2813020189845,14.7634644109396,-337.820749647775)) ;
#46987 = CARTESIAN_POINT('Ctrl Pts',(-10.5582643959879,15.272237722145,-337.831877368254)) ;
#46988 = CARTESIAN_POINT('Ctrl Pts',(-10.4312850065132,15.3592475440648,-337.833825869107)) ;
#46989 = CARTESIAN_POINT('Ctrl Pts',(-10.1984291940722,15.5145871689236,-337.837391514242)) ;
#46990 = CARTESIAN_POINT('Ctrl Pts',(-10.092911006511,15.5834373746747,-337.839004514752)) ;
#46991 = CARTESIAN_POINT('Ctrl Pts',(-9.89476589075203,15.709869524002,-337.842029224401)) ;
#46992 = CARTESIAN_POINT('Ctrl Pts',(-9.80231648317952,15.7677196836731,-337.843438783243)) ;
#46993 = CARTESIAN_POINT('Ctrl Pts',(-9.56350988578535,15.9142407737393,-337.847075775736)) ;
#46994 = CARTESIAN_POINT('Ctrl Pts',(-9.41642690528055,16.00170881338,-337.849312028745)) ;
#46995 = CARTESIAN_POINT('Ctrl Pts',(-9.08121571305503,16.1948314793187,-337.854398898427)) ;
#46996 = CARTESIAN_POINT('Ctrl Pts',(-8.8924125852895,16.2992651263362,-337.857257337435)) ;
#46997 = CARTESIAN_POINT('Ctrl Pts',(-8.265594563013,16.6318466902534,-337.866713649771)) ;
#46998 = CARTESIAN_POINT('Ctrl Pts',(-7.82029558364206,16.8458111484877,-337.87338359454)) ;
#46999 = CARTESIAN_POINT('Ctrl Pts',(-7.00680726113727,17.1974746421768,-337.885307792654)) ;
#47000 = CARTESIAN_POINT('Ctrl Pts',(-6.64176914850144,17.341723838742,-337.890566815487)) ;
#47001 = CARTESIAN_POINT('Ctrl Pts',(-6.17849982963986,17.5080153045906,-337.897024894798)) ;
#47002 = CARTESIAN_POINT('Ctrl Pts',(-6.08429460441766,17.5409754363863,-337.898326983859)) ;
#47003 = CARTESIAN_POINT('Ctrl Pts',(-5.92768903227221,17.5943545492179,-337.900470442245)) ;
#47004 = CARTESIAN_POINT('Ctrl Pts',(-5.86543801244742,17.6152049725359,-337.901316908699)) ;
#47005 = CARTESIAN_POINT('Ctrl Pts',(-5.75459145447676,17.6516792978701,-337.902813814101)) ;
#47006 = CARTESIAN_POINT('Ctrl Pts',(-5.7060397964305,17.6674337324536,-337.903466051801)) ;
#47007 = CARTESIAN_POINT('Ctrl Pts',(-5.65495066307624,17.6837789836597,-337.904149068195)) ;
#47008 = CARTESIAN_POINT('Ctrl Pts',(-5.65247740102427,17.6845696972152,-337.904182125374)) ;
#47009 = CARTESIAN_POINT('Ctrl Pts',(-5.64753933790878,17.6861472775638,-337.904248110464)) ;
#47010 = CARTESIAN_POINT('Ctrl Pts',(-5.64507453808973,17.6869341480177,-337.904281038414)) ;
#47011 = CARTESIAN_POINT('Ctrl Pts',(-5.64008304778363,17.6885264974097,-337.904347704905)) ;
#47012 = CARTESIAN_POINT('Ctrl Pts',(-5.63755634902524,17.6893319502752,-337.90438144315)) ;
#47013 = CARTESIAN_POINT('Ctrl Pts',(-5.63236943636784,17.6909841933274,-337.904450685226)) ;
#47014 = CARTESIAN_POINT('Ctrl Pts',(-5.62970920386892,17.6918309249259,-337.904486188398)) ;
#47015 = CARTESIAN_POINT('Ctrl Pts',(-5.62417464033936,17.6935911593359,-337.90456003285)) ;
#47016 = CARTESIAN_POINT('Ctrl Pts',(-5.62130027747067,17.6945045618484,-337.904598373009)) ;
#47017 = CARTESIAN_POINT('Ctrl Pts',(-5.61523925041663,17.6964289827091,-337.904679196381)) ;
#47018 = CARTESIAN_POINT('Ctrl Pts',(-5.61205253544679,17.6974398408039,-337.904721677817)) ;
#47019 = CARTESIAN_POINT('Ctrl Pts',(-5.60523954148687,17.6995989658937,-337.904812472392)) ;
#47020 = CARTESIAN_POINT('Ctrl Pts',(-5.60161318226705,17.7007469793557,-337.904860782741)) ;
#47021 = CARTESIAN_POINT('Ctrl Pts',(-5.59374793180748,17.7032342593022,-337.904965527017)) ;
#47022 = CARTESIAN_POINT('Ctrl Pts',(-5.58950891177702,17.7045731179687,-337.90502195649)) ;
#47023 = CARTESIAN_POINT('Ctrl Pts',(-5.58017406068875,17.7075177650895,-337.905146170901)) ;
#47024 = CARTESIAN_POINT('Ctrl Pts',(-5.57507801642473,17.7091228766229,-337.905213948518)) ;
#47025 = CARTESIAN_POINT('Ctrl Pts',(-5.56367286026134,17.712709771202,-337.905365564398)) ;
#47026 = CARTESIAN_POINT('Ctrl Pts',(-5.55736338079426,17.7146903836523,-337.905449390146)) ;
#47027 = CARTESIAN_POINT('Ctrl Pts',(-5.54299761743427,17.7191915185861,-337.905640136348)) ;
#47028 = CARTESIAN_POINT('Ctrl Pts',(-5.534940669784,17.7217099186622,-337.905747034437)) ;
#47029 = CARTESIAN_POINT('Ctrl Pts',(-5.51626417783073,17.7275337433994,-337.905994646337)) ;
#47030 = CARTESIAN_POINT('Ctrl Pts',(-5.50564337478121,17.7308351222599,-337.906135318309)) ;
#47031 = CARTESIAN_POINT('Ctrl Pts',(-5.393457645564,17.7655965054165,-337.907619782775)) ;
#47032 = CARTESIAN_POINT('Ctrl Pts',(-5.29162711782083,17.7961930495159,-337.908954867205)) ;
#47033 = CARTESIAN_POINT('Ctrl Pts',(-4.98817806958313,17.8845341486628,-337.912903326114)) ;
#47034 = CARTESIAN_POINT('Ctrl Pts',(-4.78583774015009,17.9397391147446,-337.91549711237)) ;
#47035 = CARTESIAN_POINT('Ctrl Pts',(-3.76877363567561,18.1987949158494,-337.928417984037)) ;
#47036 = CARTESIAN_POINT('Ctrl Pts',(-2.94181595956697,18.3506270718738,-337.938599472441)) ;
#47037 = CARTESIAN_POINT('Ctrl Pts',(-1.95738059961305,18.4630974589892,-337.951080077392)) ;
#47038 = CARTESIAN_POINT('Ctrl Pts',(-1.80713276387469,18.4784084184793,-337.95299305859)) ;
#47039 = CARTESIAN_POINT('Ctrl Pts',(-1.53029649992009,18.5032105848156,-337.95653542175)) ;
#47040 = CARTESIAN_POINT('Ctrl Pts',(-1.40376527731856,18.5132399194726,-337.958161249225)) ;
#47041 = CARTESIAN_POINT('Ctrl Pts',(-1.16102092305774,18.5299778161289,-337.961294173287)) ;
#47042 = CARTESIAN_POINT('Ctrl Pts',(-1.04482793301391,18.536892457972,-337.962799858185)) ;
#47043 = CARTESIAN_POINT('Ctrl Pts',(-0.794579205922912,18.5494243553547,
-337.966056002095)) ;
#47044 = CARTESIAN_POINT('Ctrl Pts',(-0.660512033239542,18.5546819919181,
-337.967808648295)) ;
#47045 = CARTESIAN_POINT('Ctrl Pts',(0.232271529319654,18.5800052363997,-337.979533061582)) ;
#47046 = CARTESIAN_POINT('Ctrl Pts',(0.991546553996248,18.5549823431925,-337.989794133195)) ;
#47047 = CARTESIAN_POINT('Ctrl Pts',(1.74714810520653,18.4835595300519,-338.)) ;
#47048 = CARTESIAN_POINT('',(-16.8928031616863,7.70244771115141,-338.)) ;
#47049 = CARTESIAN_POINT('Origin',(0.,0.,-338.)) ;
#47050 = CARTESIAN_POINT('Ctrl Pts',(-16.8928031616863,7.70244771115143,-337.999999999999)) ;
#47051 = CARTESIAN_POINT('Ctrl Pts',(-16.9188581960729,7.64530450372309,-337.99919244096)) ;
#47052 = CARTESIAN_POINT('Ctrl Pts',(-16.9446190476498,7.58803854460336,-337.998388608593)) ;
#47053 = CARTESIAN_POINT('Ctrl Pts',(-17.0038275925238,7.45461358547285,-337.996527305167)) ;
#47054 = CARTESIAN_POINT('Ctrl Pts',(-17.0370510917385,7.37836747688368,-337.995472358634)) ;
#47055 = CARTESIAN_POINT('Ctrl Pts',(-17.2554492358772,6.8678149048698,-337.988459126563)) ;
#47056 = CARTESIAN_POINT('Ctrl Pts',(-17.4245119701244,6.42680284526227,-337.982641320138)) ;
#47057 = CARTESIAN_POINT('Ctrl Pts',(-17.7535182551691,5.45975044350684,-337.970040429329)) ;
#47058 = CARTESIAN_POINT('Ctrl Pts',(-17.9072859597764,4.932078039822,-337.963258239092)) ;
#47059 = CARTESIAN_POINT('Ctrl Pts',(-18.0693340115061,4.26752905602644,-337.954633063947)) ;
#47060 = CARTESIAN_POINT('Ctrl Pts',(-18.0998138504038,4.13634795285629,-337.952927002217)) ;
#47061 = CARTESIAN_POINT('Ctrl Pts',(-18.154499088932,3.88880260477542,-337.949698628977)) ;
#47062 = CARTESIAN_POINT('Ctrl Pts',(-18.1790196208309,3.77251487095066,-337.948178370506)) ;
#47063 = CARTESIAN_POINT('Ctrl Pts',(-18.2277242807706,3.53002504267113,-337.944999295962)) ;
#47064 = CARTESIAN_POINT('Ctrl Pts',(-18.2517181472502,3.40379110325536,-337.943339333239)) ;
#47065 = CARTESIAN_POINT('Ctrl Pts',(-18.3077469514219,3.09137325465647,-337.939217610156)) ;
#47066 = CARTESIAN_POINT('Ctrl Pts',(-18.3382542000407,2.90493024922351,-337.936746038841)) ;
#47067 = CARTESIAN_POINT('Ctrl Pts',(-18.4731594511183,1.99337462635964,-337.924604442218)) ;
#47068 = CARTESIAN_POINT('Ctrl Pts',(-18.5374222240515,1.26298472956102,-337.914670290704)) ;
#47069 = CARTESIAN_POINT('Ctrl Pts',(-18.5677967501832,0.200835039614022,
-337.900263869959)) ;
#47070 = CARTESIAN_POINT('Ctrl Pts',(-18.5684331098627,-0.129240748430358,
-337.895797453102)) ;
#47071 = CARTESIAN_POINT('Ctrl Pts',(-18.5568696865713,-0.596662274280294,
-337.889550433306)) ;
#47072 = CARTESIAN_POINT('Ctrl Pts',(-18.5519400413342,-0.734124802416489,
-337.887722984908)) ;
#47073 = CARTESIAN_POINT('Ctrl Pts',(-18.5435270028039,-0.913149806758578,
-337.885360738916)) ;
#47074 = CARTESIAN_POINT('Ctrl Pts',(-18.541430496892,-0.954772960078674,
-337.884812772039)) ;
#47075 = CARTESIAN_POINT('Ctrl Pts',(-18.5381926376051,-1.01501782226077,
-337.884021632401)) ;
#47076 = CARTESIAN_POINT('Ctrl Pts',(-18.5371633378414,-1.03364541064481,
-337.883777287968)) ;
#47077 = CARTESIAN_POINT('Ctrl Pts',(-18.5351704879708,-1.06875011431447,
-337.88331734451)) ;
#47078 = CARTESIAN_POINT('Ctrl Pts',(-18.5342130389737,-1.08522755730566,
-337.883101679288)) ;
#47079 = CARTESIAN_POINT('Ctrl Pts',(-18.5324800310322,-1.11438080504803,
-337.882720514291)) ;
#47080 = CARTESIAN_POINT('Ctrl Pts',(-18.5317134367886,-1.12705713081293,
-337.882554913701)) ;
#47081 = CARTESIAN_POINT('Ctrl Pts',(-18.530436352407,-1.14782126872729,-337.882283884815)) ;
#47082 = CARTESIAN_POINT('Ctrl Pts',(-18.529933572153,-1.15590954973787,-337.882178367521)) ;
#47083 = CARTESIAN_POINT('Ctrl Pts',(-18.5291171570826,-1.16890588540298,
-337.882008914125)) ;
#47084 = CARTESIAN_POINT('Ctrl Pts',(-18.5288068675271,-1.1738141487093,-337.881944938776)) ;
#47085 = CARTESIAN_POINT('Ctrl Pts',(-18.5247310790322,-1.23788201776811,
-337.881110145112)) ;
#47086 = CARTESIAN_POINT('Ctrl Pts',(-18.5206842105924,-1.29702345425174,
-337.880342692485)) ;
#47087 = CARTESIAN_POINT('Ctrl Pts',(-18.5113245475063,-1.4248172221504,-337.878691746081)) ;
#47088 = CARTESIAN_POINT('Ctrl Pts',(-18.5059129440674,-1.49346132935088,
-337.877809409628)) ;
#47089 = CARTESIAN_POINT('Ctrl Pts',(-18.4906740763074,-1.67393991952697,
-337.875499592387)) ;
#47090 = CARTESIAN_POINT('Ctrl Pts',(-18.480214100079,-1.78571820928802,-337.874079138758)) ;
#47091 = CARTESIAN_POINT('Ctrl Pts',(-18.4184518411596,-2.38689574520511,
-337.866479324765)) ;
#47092 = CARTESIAN_POINT('Ctrl Pts',(-18.3487216540359,-2.87420527469133,
-337.860455916264)) ;
#47093 = CARTESIAN_POINT('Ctrl Pts',(-18.1874349418463,-3.75118602144865,
-337.849521072117)) ;
#47094 = CARTESIAN_POINT('Ctrl Pts',(-18.1024847220203,-4.14176686824144,
-337.844617313402)) ;
#47095 = CARTESIAN_POINT('Ctrl Pts',(-17.9575661950423,-4.71785083528004,
-337.837234282909)) ;
#47096 = CARTESIAN_POINT('Ctrl Pts',(-17.9071762018885,-4.9056437372042,-337.834803917681)) ;
#47097 = CARTESIAN_POINT('Ctrl Pts',(-17.817558584524,-5.21982822230585,-337.830689705542)) ;
#47098 = CARTESIAN_POINT('Ctrl Pts',(-17.7799124228897,-5.34665453913763,
-337.829015650587)) ;
#47099 = CARTESIAN_POINT('Ctrl Pts',(-17.7065941232427,-5.58431534615988,
-337.825851622708)) ;
#47100 = CARTESIAN_POINT('Ctrl Pts',(-17.6712285945077,-5.69523776939787,
-337.824363735064)) ;
#47101 = CARTESIAN_POINT('Ctrl Pts',(-17.5953559582878,-5.92569624326049,
-337.821248168713)) ;
#47102 = CARTESIAN_POINT('Ctrl Pts',(-17.5546685132985,-6.0451667140607,-337.819619327982)) ;
#47103 = CARTESIAN_POINT('Ctrl Pts',(-17.4615841985422,-6.30962283433346,
-337.815982651812)) ;
#47104 = CARTESIAN_POINT('Ctrl Pts',(-17.4085932633193,-6.45438947780506,
-337.813970889814)) ;
#47105 = CARTESIAN_POINT('Ctrl Pts',(-17.0927548541525,-7.28503517459725,
-337.802307573286)) ;
#47106 = CARTESIAN_POINT('Ctrl Pts',(-16.7911922035276,-7.95549251413836,
-337.792387711098)) ;
#47107 = CARTESIAN_POINT('Ctrl Pts',(-16.323774399633,-8.84894751894135,-337.778812818181)) ;
#47108 = CARTESIAN_POINT('Ctrl Pts',(-16.1914864699571,-9.0887429847299,-337.77513612963)) ;
#47109 = CARTESIAN_POINT('Ctrl Pts',(-15.966183818221,-9.47660276504974,-337.769177278606)) ;
#47110 = CARTESIAN_POINT('Ctrl Pts',(-15.8762961464612,-9.62643477818321,
-337.76687247728)) ;
#47111 = CARTESIAN_POINT('Ctrl Pts',(-15.7424397449059,-9.84258165761327,
-337.763555351717)) ;
#47112 = CARTESIAN_POINT('Ctrl Pts',(-15.7001385782781,-9.90991783291571,
-337.762523098242)) ;
#47113 = CARTESIAN_POINT('Ctrl Pts',(-15.6216173634878,-10.0331453545823,
-337.760637676208)) ;
#47114 = CARTESIAN_POINT('Ctrl Pts',(-15.5855267590846,-10.0891174237195,
-337.759782834516)) ;
#47115 = CARTESIAN_POINT('Ctrl Pts',(-15.4950212842524,-10.2278356693535,
-337.757667034972)) ;
#47116 = CARTESIAN_POINT('Ctrl Pts',(-15.4402439855551,-10.3103430004259,
-337.756410973078)) ;
#47117 = CARTESIAN_POINT('Ctrl Pts',(-15.1979323683554,-10.6690585084154,
-337.750952284421)) ;
#47118 = CARTESIAN_POINT('Ctrl Pts',(-15.0036270228117,-10.9406185793828,
-337.746824769584)) ;
#47119 = CARTESIAN_POINT('Ctrl Pts',(-14.4783565129213,-11.6344040394412,
-337.736127632206)) ;
#47120 = CARTESIAN_POINT('Ctrl Pts',(-14.1362305270345,-12.0477861713762,
-337.729594818879)) ;
#47121 = CARTESIAN_POINT('Ctrl Pts',(-13.6264495250558,-12.6120816009759,
-337.720182202701)) ;
#47122 = CARTESIAN_POINT('Ctrl Pts',(-13.4732110501547,-12.7756531243153,
-337.717391692523)) ;
#47123 = CARTESIAN_POINT('Ctrl Pts',(-13.1860457861014,-13.0712678967762,
-337.712217592317)) ;
#47124 = CARTESIAN_POINT('Ctrl Pts',(-13.0530017661685,-13.2041278634552,
-337.709841228432)) ;
#47125 = CARTESIAN_POINT('Ctrl Pts',(-12.8253750001033,-13.4246367860071,
-337.705804973176)) ;
#47126 = CARTESIAN_POINT('Ctrl Pts',(-12.7318554801358,-13.5133627460517,
-337.704154833109)) ;
#47127 = CARTESIAN_POINT('Ctrl Pts',(-12.5391174070485,-13.6924446266258,
-337.700769390557)) ;
#47128 = CARTESIAN_POINT('Ctrl Pts',(-12.4398279715769,-13.7827132733262,
-337.699033464451)) ;
#47129 = CARTESIAN_POINT('Ctrl Pts',(-12.1758902405054,-14.0174957017878,
-337.694439584705)) ;
#47130 = CARTESIAN_POINT('Ctrl Pts',(-12.0096478356262,-14.1601852918689,
-337.691566677777)) ;
#47131 = CARTESIAN_POINT('Ctrl Pts',(-11.5277336506861,-14.5592305565574,
-337.683301407167)) ;
#47132 = CARTESIAN_POINT('Ctrl Pts',(-11.2061133370042,-14.8082024617246,
-337.677857999014)) ;
#47133 = CARTESIAN_POINT('Ctrl Pts',(-10.4678344223743,-15.3418811029349,
-337.665608110429)) ;
#47134 = CARTESIAN_POINT('Ctrl Pts',(-10.0472196716053,-15.6205713864155,
-337.658791566909)) ;
#47135 = CARTESIAN_POINT('Ctrl Pts',(-9.47517696226214,-15.9669201060522,
-337.64992499468)) ;
#47136 = CARTESIAN_POINT('Ctrl Pts',(-9.33344809165379,-16.050179532163,-337.647760383374)) ;
#47137 = CARTESIAN_POINT('Ctrl Pts',(-9.12221936603019,-16.1705229585972,
-337.64459154668)) ;
#47138 = CARTESIAN_POINT('Ctrl Pts',(-9.05355920175741,-16.2090642764882,
-337.643570336987)) ;
#47139 = CARTESIAN_POINT('Ctrl Pts',(-8.92579414819752,-16.279718132154,-337.641687842569)) ;
#47140 = CARTESIAN_POINT('Ctrl Pts',(-8.86675606676054,-16.3119483962873,
-337.640825123939)) ;
#47141 = CARTESIAN_POINT('Ctrl Pts',(-8.73191435216094,-16.3846132717879,
-337.638870047247)) ;
#47142 = CARTESIAN_POINT('Ctrl Pts',(-8.65600256777216,-16.424843983839,-337.637780254346)) ;
#47143 = CARTESIAN_POINT('Ctrl Pts',(-8.31409188125779,-16.6030165312821,
-337.632914766127)) ;
#47144 = CARTESIAN_POINT('Ctrl Pts',(-8.04505566291371,-16.7350339677029,
-337.62920175647)) ;
#47145 = CARTESIAN_POINT('Ctrl Pts',(-7.25829576949921,-17.0977423961332,
-337.618537622511)) ;
#47146 = CARTESIAN_POINT('Ctrl Pts',(-6.73305628867108,-17.3113144089846,
-337.611647857577)) ;
#47147 = CARTESIAN_POINT('Ctrl Pts',(-6.05050393443399,-17.5530816852706,
-337.602693858556)) ;
#47148 = CARTESIAN_POINT('Ctrl Pts',(-5.90147321729994,-17.6037464281009,
-337.600739523138)) ;
#47149 = CARTESIAN_POINT('Ctrl Pts',(-5.53637856621129,-17.722707268024,-337.595946058512)) ;
#47150 = CARTESIAN_POINT('Ctrl Pts',(-5.31967403037213,-17.7889546763883,
-337.593095852704)) ;
#47151 = CARTESIAN_POINT('Ctrl Pts',(-4.97275729339706,-17.8881021826791,
-337.58851520856)) ;
#47152 = CARTESIAN_POINT('Ctrl Pts',(-4.84330691640878,-17.92358482132,-337.586802121521)) ;
#47153 = CARTESIAN_POINT('Ctrl Pts',(-4.59169872284972,-17.9896263310643,
-337.583463649905)) ;
#47154 = CARTESIAN_POINT('Ctrl Pts',(-4.46959223747947,-18.0203523236862,
-337.581839493758)) ;
#47155 = CARTESIAN_POINT('Ctrl Pts',(-4.20178716293336,-18.0848513998054,
-337.578268158141)) ;
#47156 = CARTESIAN_POINT('Ctrl Pts',(-4.05597391173209,-18.1181108577903,
-337.576317706154)) ;
#47157 = CARTESIAN_POINT('Ctrl Pts',(-3.17494126956148,-18.3079022791802,
-337.564498191089)) ;
#47158 = CARTESIAN_POINT('Ctrl Pts',(-2.43117433725998,-18.4214255466751,
-337.5543428602)) ;
#47159 = CARTESIAN_POINT('Ctrl Pts',(-1.41255871919411,-18.5141214936157,
-337.540572616883)) ;
#47160 = CARTESIAN_POINT('Ctrl Pts',(-1.14202733898975,-18.5327761189988,
-337.536932398543)) ;
#47161 = CARTESIAN_POINT('Ctrl Pts',(-0.697612801291283,-18.5536527238791,
-337.531022334191)) ;
#47162 = CARTESIAN_POINT('Ctrl Pts',(-0.523934894895575,-18.559369208769,
-337.528730277034)) ;
#47163 = CARTESIAN_POINT('Ctrl Pts',(-0.270782387465692,-18.5641451742232,
-337.525426782088)) ;
#47164 = CARTESIAN_POINT('Ctrl Pts',(-0.191353718588193,-18.5651337977623,
-337.524395659643)) ;
#47165 = CARTESIAN_POINT('Ctrl Pts',(-0.0455977369839269,-18.5660124742976,
-337.522514896667)) ;
#47166 = CARTESIAN_POINT('Ctrl Pts',(0.0207271590437921,-18.5660568976193,
-337.521663564146)) ;
#47167 = CARTESIAN_POINT('Ctrl Pts',(0.185563508850104,-18.5652840142503,
-337.519557938232)) ;
#47168 = CARTESIAN_POINT('Ctrl Pts',(0.284070969452338,-18.5640380324628,
-337.518308504251)) ;
#47169 = CARTESIAN_POINT('Ctrl Pts',(0.727223939508055,-18.5549046272341,
-337.512719425601)) ;
#47170 = CARTESIAN_POINT('Ctrl Pts',(1.07162016243955,-18.5382030339172,-337.50846103083)) ;
#47171 = CARTESIAN_POINT('Ctrl Pts',(1.82721153944864,-18.4804333664853,-337.499151998639)) ;
#47172 = CARTESIAN_POINT('Ctrl Pts',(2.23790565233202,-18.4352081062668,-337.494113170103)) ;
#47173 = CARTESIAN_POINT('Ctrl Pts',(2.92175035722675,-18.3367136906023,-337.485609014814)) ;
#47174 = CARTESIAN_POINT('Ctrl Pts',(3.19582783508557,-18.2909370518057,-337.482170365039)) ;
#47175 = CARTESIAN_POINT('Ctrl Pts',(3.68275729956908,-18.1983307755493,-337.475975111973)) ;
#47176 = CARTESIAN_POINT('Ctrl Pts',(3.89600731066712,-18.1538720701245,-337.473232269572)) ;
#47177 = CARTESIAN_POINT('Ctrl Pts',(4.23848192736388,-18.0761598801779,-337.468770858266)) ;
#47178 = CARTESIAN_POINT('Ctrl Pts',(4.36821665871895,-18.0452478016478,-337.467067682485)) ;
#47179 = CARTESIAN_POINT('Ctrl Pts',(4.62029597270353,-17.9823067363904,-337.463731430486)) ;
#47180 = CARTESIAN_POINT('Ctrl Pts',(4.7426687030866,-17.9504201609849,-337.462099382753)) ;
#47181 = CARTESIAN_POINT('Ctrl Pts',(5.04301789487366,-17.868872625104,-337.458062461319)) ;
#47182 = CARTESIAN_POINT('Ctrl Pts',(5.22059689339074,-17.8178002653068,-337.45564840873)) ;
#47183 = CARTESIAN_POINT('Ctrl Pts',(6.00993472971528,-17.5779703516544,-337.444798602224)) ;
#47184 = CARTESIAN_POINT('Ctrl Pts',(6.61244745600688,-17.3602963749601,-337.436177849526)) ;
#47185 = CARTESIAN_POINT('Ctrl Pts',(7.48630099871245,-16.9924867040809,-337.423413137357)) ;
#47186 = CARTESIAN_POINT('Ctrl Pts',(7.76708008626951,-16.8659946133317,-337.419273212102)) ;
#47187 = CARTESIAN_POINT('Ctrl Pts',(8.21402726250655,-16.6511141724765,-337.412678438344)) ;
#47188 = CARTESIAN_POINT('Ctrl Pts',(8.38222426430207,-16.5670807222096,-337.410195755635)) ;
#47189 = CARTESIAN_POINT('Ctrl Pts',(8.6220390612338,-16.4426789350177,-337.406669094071)) ;
#47190 = CARTESIAN_POINT('Ctrl Pts',(8.69471024507359,-16.4043671597866,-337.40560218554)) ;
#47191 = CARTESIAN_POINT('Ctrl Pts',(8.82556352928745,-16.3342683624853,-337.40368597192)) ;
#47192 = CARTESIAN_POINT('Ctrl Pts',(8.88383401057819,-16.3026497177098,-337.402834588802)) ;
#47193 = CARTESIAN_POINT('Ctrl Pts',(9.02603877402914,-16.2244979430392,-337.400760949613)) ;
#47194 = CARTESIAN_POINT('Ctrl Pts',(9.10978398404738,-16.1776248335793,-337.399543092827)) ;
#47195 = CARTESIAN_POINT('Ctrl Pts',(9.45975445794345,-15.9781633055454,-337.394460462082)) ;
#47196 = CARTESIAN_POINT('Ctrl Pts',(9.72253968998316,-15.8196358939966,-337.390659893475)) ;
#47197 = CARTESIAN_POINT('Ctrl Pts',(10.4538864334989,-15.3533358057312,-337.379986569922)) ;
#47198 = CARTESIAN_POINT('Ctrl Pts',(10.9126092192951,-15.0307558976382,-337.373169450775)) ;
#47199 = CARTESIAN_POINT('Ctrl Pts',(11.5361176770485,-14.5486873504796,-337.363421697105)) ;
#47200 = CARTESIAN_POINT('Ctrl Pts',(11.7136243296819,-14.4061556121394,-337.360589535784)) ;
#47201 = CARTESIAN_POINT('Ctrl Pts',(12.0341315003098,-14.138958388649,-337.355353767798)) ;
#47202 = CARTESIAN_POINT('Ctrl Pts',(12.1779285884804,-14.0152959444733,-337.352957875584)) ;
#47203 = CARTESIAN_POINT('Ctrl Pts',(12.4157196223072,-13.8043776698329,-337.348911106477)) ;
#47204 = CARTESIAN_POINT('Ctrl Pts',(12.51074966661,-13.718311824526,-337.34727047152)) ;
#47205 = CARTESIAN_POINT('Ctrl Pts',(12.6902062354176,-13.5523677244138,-337.344126241697)) ;
#47206 = CARTESIAN_POINT('Ctrl Pts',(12.7747891388532,-13.4726674289487,-337.342624257522)) ;
#47207 = CARTESIAN_POINT('Ctrl Pts',(12.9991890250577,-13.2572078996217,-337.33858503919)) ;
#47208 = CARTESIAN_POINT('Ctrl Pts',(13.1376259631285,-13.1200327920946,-337.336035370251)) ;
#47209 = CARTESIAN_POINT('Ctrl Pts',(13.5146768202029,-12.7344661147369,-337.328931082637)) ;
#47210 = CARTESIAN_POINT('Ctrl Pts',(13.7485772278788,-12.4815760279498,-337.324339548349)) ;
#47211 = CARTESIAN_POINT('Ctrl Pts',(14.311797528098,-11.8375761819423,-337.31285989267)) ;
#47212 = CARTESIAN_POINT('Ctrl Pts',(14.6322550023209,-11.4390939878017,-337.305937237945)) ;
#47213 = CARTESIAN_POINT('Ctrl Pts',(15.0371540915819,-10.8907105851356,-337.296824122601)) ;
#47214 = CARTESIAN_POINT('Ctrl Pts',(15.1365521504998,-10.7521332464124,-337.294555377617)) ;
#47215 = CARTESIAN_POINT('Ctrl Pts',(15.3067700124038,-10.5077822153238,-337.290626306693)) ;
#47216 = CARTESIAN_POINT('Ctrl Pts',(15.3784374653548,-10.4026129651448,-337.288957787267)) ;
#47217 = CARTESIAN_POINT('Ctrl Pts',(15.4886130381895,-10.2373073899003,-337.286375275318)) ;
#47218 = CARTESIAN_POINT('Ctrl Pts',(15.5278650910516,-10.1776717462217,-337.285451637359)) ;
#47219 = CARTESIAN_POINT('Ctrl Pts',(15.6005474331487,-10.0658462289691,-337.283735773406)) ;
#47220 = CARTESIAN_POINT('Ctrl Pts',(15.6340622560933,-10.0137124934336,-337.282942304692)) ;
#47221 = CARTESIAN_POINT('Ctrl Pts',(15.7279697342368,-9.86601474770796,-337.280711249282)) ;
#47222 = CARTESIAN_POINT('Ctrl Pts',(15.7877515570531,-9.77006549592708,-337.279281702452)) ;
#47223 = CARTESIAN_POINT('Ctrl Pts',(16.0208961687605,-9.38814243113036,-337.273658454331)) ;
#47224 = CARTESIAN_POINT('Ctrl Pts',(16.187395595678,-9.09805238087904,-337.269533630386)) ;
#47225 = CARTESIAN_POINT('Ctrl Pts',(16.5907389650162,-8.34915186103024,-337.259091233833)) ;
#47226 = CARTESIAN_POINT('Ctrl Pts',(16.8164487050611,-7.8846692613911,-337.252800595879)) ;
#47227 = CARTESIAN_POINT('Ctrl Pts',(17.0825826789671,-7.27341147551144,-337.244547449132)) ;
#47228 = CARTESIAN_POINT('Ctrl Pts',(17.1409757950113,-7.13471052018993,-337.24267692565)) ;
#47229 = CARTESIAN_POINT('Ctrl Pts',(17.2806318328654,-6.79137226132306,-337.238045680028)) ;
#47230 = CARTESIAN_POINT('Ctrl Pts',(17.3599530449357,-6.58597022196559,-337.235274052071)) ;
#47231 = CARTESIAN_POINT('Ctrl Pts',(17.4814971694678,-6.25376667161011,-337.230780955979)) ;
#47232 = CARTESIAN_POINT('Ctrl Pts',(17.526037015956,-6.12783545161441,-337.229075401567)) ;
#47233 = CARTESIAN_POINT('Ctrl Pts',(17.6099016254636,-5.88232161245492,-337.225744476818)) ;
#47234 = CARTESIAN_POINT('Ctrl Pts',(17.6493768315202,-5.76279795035246,-337.224120242884)) ;
#47235 = CARTESIAN_POINT('Ctrl Pts',(17.7430592433604,-5.4691501119875,-337.220122817102)) ;
#47236 = CARTESIAN_POINT('Ctrl Pts',(17.79592222525,-5.29461105811313,-337.217740791508)) ;
#47237 = CARTESIAN_POINT('Ctrl Pts',(18.0230514555489,-4.50282749600444,-337.206910386925)) ;
#47238 = CARTESIAN_POINT('Ctrl Pts',(18.1678332642373,-3.87758533821819,-337.198274397823)) ;
#47239 = CARTESIAN_POINT('Ctrl Pts',(18.3346749270021,-2.93804249638003,-337.185422898827)) ;
#47240 = CARTESIAN_POINT('Ctrl Pts',(18.3815845547712,-2.62863994926851,-337.181213998003)) ;
#47241 = CARTESIAN_POINT('Ctrl Pts',(18.4443520264968,-2.12988322781615,-337.174526848438)) ;
#47242 = CARTESIAN_POINT('Ctrl Pts',(18.4651621523447,-1.94121383536933,-337.172019742339)) ;
#47243 = CARTESIAN_POINT('Ctrl Pts',(18.4908392449272,-1.67036813412586,-337.168467697072)) ;
#47244 = CARTESIAN_POINT('Ctrl Pts',(18.4980584112429,-1.58842712297686,-337.167399243618)) ;
#47245 = CARTESIAN_POINT('Ctrl Pts',(18.5100986649796,-1.44052772890319,-337.165483537371)) ;
#47246 = CARTESIAN_POINT('Ctrl Pts',(18.5151123225321,-1.37458663145747,-337.164634162172)) ;
#47247 = CARTESIAN_POINT('Ctrl Pts',(18.5264847267926,-1.21364277579546,-337.162572001626)) ;
#47248 = CARTESIAN_POINT('Ctrl Pts',(18.5324651673801,-1.1186152048318,-337.161363511053)) ;
#47249 = CARTESIAN_POINT('Ctrl Pts',(18.5401905767133,-0.978698224377128,
-337.159595047726)) ;
#47250 = CARTESIAN_POINT('Ctrl Pts',(18.5425039991331,-0.933842669186298,
-337.159029749726)) ;
#47251 = CARTESIAN_POINT('Ctrl Pts',(18.5446545937658,-0.888979977513938,
-337.158465839576)) ;
#47252 = CARTESIAN_POINT('Origin',(0.,0.,5.8748638224677)) ;
#47253 = CARTESIAN_POINT('',(16.4056275812262,12.0157134421436,-20.)) ;
#47254 = CARTESIAN_POINT('Ctrl Pts',(18.131496419296,-9.20710722510904,-17.3804829797999)) ;
#47255 = CARTESIAN_POINT('Ctrl Pts',(18.0392880697976,-9.38869252849294,-17.3854844732659)) ;
#47256 = CARTESIAN_POINT('Ctrl Pts',(17.9443414885465,-9.56891311233099,-17.3905038146911)) ;
#47257 = CARTESIAN_POINT('Ctrl Pts',(17.5701229759926,-10.2540548051986,-17.4098161311144)) ;
#47258 = CARTESIAN_POINT('Ctrl Pts',(17.2721382230938,-10.7483995960656,-17.4242445936442)) ;
#47259 = CARTESIAN_POINT('Ctrl Pts',(16.5616564939481,-11.8210463754899,-17.4567247969065)) ;
#47260 = CARTESIAN_POINT('Ctrl Pts',(16.1390709365163,-12.391770864015,-17.474830898209)) ;
#47261 = CARTESIAN_POINT('Ctrl Pts',(15.396419929138,-13.2921607900915,-17.5044848954197)) ;
#47262 = CARTESIAN_POINT('Ctrl Pts',(15.093490552431,-13.6351689547094,-17.5160634408531)) ;
#47263 = CARTESIAN_POINT('Ctrl Pts',(14.5312552237131,-14.2300725343671,-17.536478745888)) ;
#47264 = CARTESIAN_POINT('Ctrl Pts',(14.276316555976,-14.4858250926356,-17.5453598107132)) ;
#47265 = CARTESIAN_POINT('Ctrl Pts',(13.6077030429862,-15.1217694594513,-17.5679043430281)) ;
#47266 = CARTESIAN_POINT('Ctrl Pts',(13.1848361514893,-15.4918556985779,-17.5814829713099)) ;
#47267 = CARTESIAN_POINT('Ctrl Pts',(12.2020625357566,-16.2825420008217,-17.6120991133579)) ;
#47268 = CARTESIAN_POINT('Ctrl Pts',(11.6346663983223,-16.6926939839877,-17.6291545250614)) ;
#47269 = CARTESIAN_POINT('Ctrl Pts',(10.5604626099482,-17.3877776884551,-17.66081384543)) ;
#47270 = CARTESIAN_POINT('Ctrl Pts',(10.060414857346,-17.6818049869029,-17.6753187988438)) ;
#47271 = CARTESIAN_POINT('Ctrl Pts',(8.91168051373702,-18.2927353017547,-17.7081734961953)) ;
#47272 = CARTESIAN_POINT('Ctrl Pts',(8.2573031096123,-18.5972888434117,-17.726582045578)) ;
#47273 = CARTESIAN_POINT('Ctrl Pts',(7.17828568172708,-19.0312729818496,-17.7561200695308)) ;
#47274 = CARTESIAN_POINT('Ctrl Pts',(6.76317000345207,-19.1827180624439,-17.767292775253)) ;
#47275 = CARTESIAN_POINT('Ctrl Pts',(5.99488528466534,-19.4349667135265,-17.7874535544521)) ;
#47276 = CARTESIAN_POINT('Ctrl Pts',(5.64328678425831,-19.5399563845945,-17.7964725552866)) ;
#47277 = CARTESIAN_POINT('Ctrl Pts',(4.72567730241938,-19.7871262705653,-17.8196808131403)) ;
#47278 = CARTESIAN_POINT('Ctrl Pts',(4.15604272880859,-19.9145601152025,-17.833778605361)) ;
#47279 = CARTESIAN_POINT('Ctrl Pts',(2.88299967990383,-20.1423468344708,-17.8651814896079)) ;
#47280 = CARTESIAN_POINT('Ctrl Pts',(2.17822030411272,-20.230698674791,-17.8825061012518)) ;
#47281 = CARTESIAN_POINT('Ctrl Pts',(0.868602317683623,-20.325634622103,-17.9150486797655)) ;
#47282 = CARTESIAN_POINT('Ctrl Pts',(0.265296097316439,-20.3424556284699,
-17.9301722993868)) ;
#47283 = CARTESIAN_POINT('Ctrl Pts',(-1.15491770306433,-20.3188562510556,
-17.9661045858041)) ;
#47284 = CARTESIAN_POINT('Ctrl Pts',(-1.97041103215487,-20.2560417526877,
-17.987010027909)) ;
#47285 = CARTESIAN_POINT('Ctrl Pts',(-3.14179443961057,-20.0943915262186,
-18.0169122951184)) ;
#47286 = CARTESIAN_POINT('Ctrl Pts',(-3.50227553174102,-20.0347077715174,
-18.026089141357)) ;
#47287 = CARTESIAN_POINT('Ctrl Pts',(-4.48000236353235,-19.845632091754,-18.0507675729864)) ;
#47288 = CARTESIAN_POINT('Ctrl Pts',(-5.09315032155366,-19.6971918472939,
-18.0660601840092)) ;
#47289 = CARTESIAN_POINT('Ctrl Pts',(-6.56815585253354,-19.2666092102568,
-18.1033282900962)) ;
#47290 = CARTESIAN_POINT('Ctrl Pts',(-7.41995221080844,-18.9548726938288,
-18.125293132673)) ;
#47291 = CARTESIAN_POINT('Ctrl Pts',(-8.78032793496401,-18.351208549296,-18.1621268936952)) ;
#47292 = CARTESIAN_POINT('Ctrl Pts',(-9.30214924559862,-18.0922918502793,
-18.1766965533733)) ;
#47293 = CARTESIAN_POINT('Ctrl Pts',(-10.4524800009425,-17.4585831937094,
-18.2098677701355)) ;
#47294 = CARTESIAN_POINT('Ctrl Pts',(-11.0733330166196,-17.0715480773121,
-18.2285319087131)) ;
#47295 = CARTESIAN_POINT('Ctrl Pts',(-12.0439042771515,-16.3912365423604,
-18.2586242274562)) ;
#47296 = CARTESIAN_POINT('Ctrl Pts',(-12.4069834564716,-16.118158452108,-18.2701015482033)) ;
#47297 = CARTESIAN_POINT('Ctrl Pts',(-13.0811835987641,-15.5747916610563,
-18.2916452857559)) ;
#47298 = CARTESIAN_POINT('Ctrl Pts',(-13.3938332058954,-15.3067545477776,
-18.3017315576952)) ;
#47299 = CARTESIAN_POINT('Ctrl Pts',(-14.6291706417642,-14.1808411900583,
-18.3424506717248)) ;
#47300 = CARTESIAN_POINT('Ctrl Pts',(-15.4793433494829,-13.2475971267835,
-18.3727075587436)) ;
#47301 = CARTESIAN_POINT('Ctrl Pts',(-16.620333960294,-11.7341595692838,-18.4197532774729)) ;
#47302 = CARTESIAN_POINT('Ctrl Pts',(-16.9789651519995,-11.2089577085238,
-18.4357241466243)) ;
#47303 = CARTESIAN_POINT('Ctrl Pts',(-17.7233698885513,-10.0008919602952,
-18.4716835909609)) ;
#47304 = CARTESIAN_POINT('Ctrl Pts',(-18.0954493625316,-9.31076737217195,
-18.4917221776513)) ;
#47305 = CARTESIAN_POINT('Ctrl Pts',(-18.5733098220373,-8.28698742482051,
-18.5202511192266)) ;
#47306 = CARTESIAN_POINT('Ctrl Pts',(-18.7117895166592,-7.96937496976673,
-18.528935573816)) ;
#47307 = CARTESIAN_POINT('Ctrl Pts',(-19.0774375610909,-7.06858593448309,
-18.5529948971681)) ;
#47308 = CARTESIAN_POINT('Ctrl Pts',(-19.2859010918836,-6.47823755171429,
-18.5681650384943)) ;
#47309 = CARTESIAN_POINT('Ctrl Pts',(-19.7235806666917,-5.02902603547314,
-18.6048806464667)) ;
#47310 = CARTESIAN_POINT('Ctrl Pts',(-19.9243744415255,-4.16293504547565,
-18.6264206249536)) ;
#47311 = CARTESIAN_POINT('Ctrl Pts',(-20.1618437593218,-2.71290870931743,
-18.6627820931617)) ;
#47312 = CARTESIAN_POINT('Ctrl Pts',(-20.2311443524559,-2.13555772365329,
-18.6773243644515)) ;
#47313 = CARTESIAN_POINT('Ctrl Pts',(-20.3312334377397,-0.831367206766867,
-18.7103583237921)) ;
#47314 = CARTESIAN_POINT('Ctrl Pts',(-20.3479569346091,-0.104238561547288,
-18.7289109228162)) ;
#47315 = CARTESIAN_POINT('Ctrl Pts',(-20.3116316681115,1.08238597041301,-18.7590567051804)) ;
#47316 = CARTESIAN_POINT('Ctrl Pts',(-20.2819215890569,1.54194745073483,-18.7706938389194)) ;
#47317 = CARTESIAN_POINT('Ctrl Pts',(-20.1964218123784,2.40701582080961,-18.7923238442201)) ;
#47318 = CARTESIAN_POINT('Ctrl Pts',(-20.1439404616109,2.8126223988546,-18.802342674701)) ;
#47319 = CARTESIAN_POINT('Ctrl Pts',(-19.8777793350564,4.47422145692789,-18.8433429946405)) ;
#47320 = CARTESIAN_POINT('Ctrl Pts',(-19.5585444436011,5.71035190922039,-18.8739342271753)) ;
#47321 = CARTESIAN_POINT('Ctrl Pts',(-18.9064149085717,7.51574001898014,-18.9215985866594)) ;
#47322 = CARTESIAN_POINT('Ctrl Pts',(-18.6582669194175,8.1122091081497,-18.9378313896639)) ;
#47323 = CARTESIAN_POINT('Ctrl Pts',(-18.042613859589,9.41363785633099,-18.9743314254983)) ;
#47324 = CARTESIAN_POINT('Ctrl Pts',(-17.6613113815884,10.1109134205892,-18.9946466873114)) ;
#47325 = CARTESIAN_POINT('Ctrl Pts',(-17.062985930353,11.0674381369411,-19.0231005806699)) ;
#47326 = CARTESIAN_POINT('Ctrl Pts',(-16.8787946855523,11.3463637879838,-19.0314635066024)) ;
#47327 = CARTESIAN_POINT('Ctrl Pts',(-16.3482877364534,12.1081986931649,-19.0544110746184)) ;
#47328 = CARTESIAN_POINT('Ctrl Pts',(-15.9875575837926,12.5806597499504,-19.0688219222257)) ;
#47329 = CARTESIAN_POINT('Ctrl Pts',(-15.027264263384,13.7302625779835,-19.1051518820726)) ;
#47330 = CARTESIAN_POINT('Ctrl Pts',(-14.4022799806571,14.3844743018147,-19.1270626367402)) ;
#47331 = CARTESIAN_POINT('Ctrl Pts',(-13.3066276267042,15.3881280367831,-19.1638352984844)) ;
#47332 = CARTESIAN_POINT('Ctrl Pts',(-12.860715339133,15.7627033012444,-19.1784005190965)) ;
#47333 = CARTESIAN_POINT('Ctrl Pts',(-11.8204440375694,16.5629878757434,-19.2115495917081)) ;
#47334 = CARTESIAN_POINT('Ctrl Pts',(-11.2179617554914,16.9768310124098,-19.2301957471706)) ;
#47335 = CARTESIAN_POINT('Ctrl Pts',(-10.2059338281782,17.5945493022491,-19.2602986820123)) ;
#47336 = CARTESIAN_POINT('Ctrl Pts',(-9.80948093800944,17.8186233743188,-19.2718037416389)) ;
#47337 = CARTESIAN_POINT('Ctrl Pts',(-9.03996607034749,18.2200795073311,-19.2933981553172)) ;
#47338 = CARTESIAN_POINT('Ctrl Pts',(-8.66836432068795,18.3997757310214,-19.3035075428875)) ;
#47339 = CARTESIAN_POINT('Ctrl Pts',(-7.14632614940413,19.0794412868354,-19.3441158933636)) ;
#47340 = CARTESIAN_POINT('Ctrl Pts',(-5.95624797314513,19.4837926646047,-19.3742441947023)) ;
#47341 = CARTESIAN_POINT('Ctrl Pts',(-4.12108653028286,19.9233309719072,-19.4210791918915)) ;
#47342 = CARTESIAN_POINT('Ctrl Pts',(-3.49911297105361,20.0419227756955,-19.4369773843277)) ;
#47343 = CARTESIAN_POINT('Ctrl Pts',(-2.09862764729727,20.241764340111,-19.4728226578717)) ;
#47344 = CARTESIAN_POINT('Ctrl Pts',(-1.31890353021939,20.3074801811141,-19.4928210962884)) ;
#47345 = CARTESIAN_POINT('Ctrl Pts',(-0.187803421990395,20.337378771627,-19.5214014161937)) ;
#47346 = CARTESIAN_POINT('Ctrl Pts',(0.161914956698301,20.3376015066546,-19.5301707882459)) ;
#47347 = CARTESIAN_POINT('Ctrl Pts',(1.15595780452201,20.312591554997,-19.5547863673276)) ;
#47348 = CARTESIAN_POINT('Ctrl Pts',(1.79931576067825,20.2657368425544,-19.5704073318224)) ;
#47349 = CARTESIAN_POINT('Ctrl Pts',(3.30625118125827,20.0836539576361,-19.607215050388)) ;
#47350 = CARTESIAN_POINT('Ctrl Pts',(4.16548676969294,19.923181500246,-19.6283980813291)) ;
#47351 = CARTESIAN_POINT('Ctrl Pts',(5.57236233053807,19.5654130363426,-19.6643152294202)) ;
#47352 = CARTESIAN_POINT('Ctrl Pts',(6.12664242751008,19.3989910319172,-19.6787849902183)) ;
#47353 = CARTESIAN_POINT('Ctrl Pts',(7.3512118882454,18.9735881024619,-19.7115176714718)) ;
#47354 = CARTESIAN_POINT('Ctrl Pts',(8.01640277169513,18.7022629887867,-19.7298383725935)) ;
#47355 = CARTESIAN_POINT('Ctrl Pts',(9.06919283051794,18.206331787221,-19.7593974306874)) ;
#47356 = CARTESIAN_POINT('Ctrl Pts',(9.4661845219242,18.0031144675481,-19.7706756191561)) ;
#47357 = CARTESIAN_POINT('Ctrl Pts',(10.1794300911626,17.6078893296198,-19.7910070494607)) ;
#47358 = CARTESIAN_POINT('Ctrl Pts',(10.4977411847119,17.4199883525408,-19.8000923211161)) ;
#47359 = CARTESIAN_POINT('Ctrl Pts',(11.8216570136236,16.5890007556669,-19.838268640101)) ;
#47360 = CARTESIAN_POINT('Ctrl Pts',(12.774733576001,15.8667174416586,-19.8668885241356)) ;
#47361 = CARTESIAN_POINT('Ctrl Pts',(14.05552448074,14.7054672911806,-19.9095925665322)) ;
#47362 = CARTESIAN_POINT('Ctrl Pts',(14.4377408826382,14.3303931535161,-19.9229461035312)) ;
#47363 = CARTESIAN_POINT('Ctrl Pts',(15.3773834578425,13.3325123212659,-19.9574605973473)) ;
#47364 = CARTESIAN_POINT('Ctrl Pts',(15.9120360749949,12.6896375056191,-19.9787923753823)) ;
#47365 = CARTESIAN_POINT('Ctrl Pts',(16.4056275812262,12.0157134421436,-20.)) ;
#47366 = CARTESIAN_POINT('',(-6.42208446149247,19.2945281628512,-20.)) ;
#47367 = CARTESIAN_POINT('Origin',(0.,0.,-20.)) ;
#47368 = CARTESIAN_POINT('Ctrl Pts',(-6.42208446149245,19.2945281628512,-20.)) ;
#47369 = CARTESIAN_POINT('Ctrl Pts',(-7.54571498564493,18.9205335220539,-19.9705725095626)) ;
#47370 = CARTESIAN_POINT('Ctrl Pts',(-8.63452990372283,18.4491019182255,-19.9421975689781)) ;
#47371 = CARTESIAN_POINT('Ctrl Pts',(-10.1459115821159,17.6314420079567,-19.9000036142141)) ;
#47372 = CARTESIAN_POINT('Ctrl Pts',(-10.6054902547094,17.3588835819478,-19.8867846332647)) ;
#47373 = CARTESIAN_POINT('Ctrl Pts',(-11.9472687509246,16.4899314064032,-19.8467902829131)) ;
#47374 = CARTESIAN_POINT('Ctrl Pts',(-12.7939173067031,15.8420548380586,-19.8195712878972)) ;
#47375 = CARTESIAN_POINT('Ctrl Pts',(-13.9842075231014,14.7733010061046,-19.7787395703855)) ;
#47376 = CARTESIAN_POINT('Ctrl Pts',(-14.3682039091627,14.4001113127303,-19.7651257336831)) ;
#47377 = CARTESIAN_POINT('Ctrl Pts',(-14.9683002199986,13.768973175322,-19.7433693969149)) ;
#47378 = CARTESIAN_POINT('Ctrl Pts',(-15.1935127722465,13.520051913782,-19.7350962864897)) ;
#47379 = CARTESIAN_POINT('Ctrl Pts',(-15.9335392446829,12.6602665613523,-19.7073313067766)) ;
#47380 = CARTESIAN_POINT('Ctrl Pts',(-16.4184954931035,12.0246845484445,-19.6881006359245)) ;
#47381 = CARTESIAN_POINT('Ctrl Pts',(-17.2171424766637,10.8392629004378,-19.6532888760962)) ;
#47382 = CARTESIAN_POINT('Ctrl Pts',(-17.5449572090063,10.300198181734,-19.6378172777258)) ;
#47383 = CARTESIAN_POINT('Ctrl Pts',(-18.3925895184266,8.74811018225945,-19.5938446790031)) ;
#47384 = CARTESIAN_POINT('Ctrl Pts',(-18.8531967406469,7.70543268113117,-19.5648555002104)) ;
#47385 = CARTESIAN_POINT('Ctrl Pts',(-19.3390435870962,6.29662912142951,-19.5270029720676)) ;
#47386 = CARTESIAN_POINT('Ctrl Pts',(-19.4452445627443,5.96058812792489,-19.5180795762446)) ;
#47387 = CARTESIAN_POINT('Ctrl Pts',(-19.6305781766564,5.31634412890872,-19.5012577483459)) ;
#47388 = CARTESIAN_POINT('Ctrl Pts',(-19.7113142315708,5.00871318993154,-19.4933601878428)) ;
#47389 = CARTESIAN_POINT('Ctrl Pts',(-19.976994825352,3.89015795895933,-19.4650831866032)) ;
#47390 = CARTESIAN_POINT('Ctrl Pts',(-20.1193671996939,3.06997267309098,-19.4450654003448)) ;
#47391 = CARTESIAN_POINT('Ctrl Pts',(-20.2856203357511,1.57215683266874,-19.4084118232149)) ;
#47392 = CARTESIAN_POINT('Ctrl Pts',(-20.3266397573979,0.897649872820425,
-19.3918768530545)) ;
#47393 = CARTESIAN_POINT('Ctrl Pts',(-20.3411464537278,-0.4289457122021,-19.358925212286)) ;
#47394 = CARTESIAN_POINT('Ctrl Pts',(-20.316972380584,-1.08021060794756,-19.3425451896674)) ;
#47395 = CARTESIAN_POINT('Ctrl Pts',(-20.2047868624575,-2.39473514853497,
-19.3090962526814)) ;
#47396 = CARTESIAN_POINT('Ctrl Pts',(-20.1152286599606,-3.05708074427671,
-19.2920406744007)) ;
#47397 = CARTESIAN_POINT('Ctrl Pts',(-19.9221328784407,-4.09660761996546,
-19.2652764658035)) ;
#47398 = CARTESIAN_POINT('Ctrl Pts',(-19.8400481041837,-4.47728374715785,
-19.2554806275714)) ;
#47399 = CARTESIAN_POINT('Ctrl Pts',(-19.6242251330395,-5.355048577903,-19.2330595194619)) ;
#47400 = CARTESIAN_POINT('Ctrl Pts',(-19.4824433060686,-5.84988613599767,
-19.2205251144961)) ;
#47401 = CARTESIAN_POINT('Ctrl Pts',(-19.1080581525078,-6.99109103039179,
-19.191361003802)) ;
#47402 = CARTESIAN_POINT('Ctrl Pts',(-18.8611800192939,-7.63211157594126,
-19.1747723303905)) ;
#47403 = CARTESIAN_POINT('Ctrl Pts',(-18.3513642252671,-8.779115095633,-19.1440765904924)) ;
#47404 = CARTESIAN_POINT('Ctrl Pts',(-18.098672083105,-9.2888907775145,-19.1300488599284)) ;
#47405 = CARTESIAN_POINT('Ctrl Pts',(-17.3838252732944,-10.590779540001,-19.092982809457)) ;
#47406 = CARTESIAN_POINT('Ctrl Pts',(-16.8888974076893,-11.3634108985209,
-19.0696867614093)) ;
#47407 = CARTESIAN_POINT('Ctrl Pts',(-15.9795337904982,-12.591693677508,-19.0307844809173)) ;
#47408 = CARTESIAN_POINT('Ctrl Pts',(-15.5935090752394,-13.0667031896461,
-19.0152319620333)) ;
#47409 = CARTESIAN_POINT('Ctrl Pts',(-14.9408962332899,-13.7995714139715,
-18.9907698364742)) ;
#47410 = CARTESIAN_POINT('Ctrl Pts',(-14.6876572894402,-14.0688050518226,
-18.9816878457799)) ;
#47411 = CARTESIAN_POINT('Ctrl Pts',(-13.8758016307955,-14.8861124076801,
-18.9535595955181)) ;
#47412 = CARTESIAN_POINT('Ctrl Pts',(-13.292799794239,-15.408948506576,-18.9347128214389)) ;
#47413 = CARTESIAN_POINT('Ctrl Pts',(-12.1995339469984,-16.2810586743814,
-18.9006225636591)) ;
#47414 = CARTESIAN_POINT('Ctrl Pts',(-11.700739747079,-16.6431421471916,-18.8854887862647)) ;
#47415 = CARTESIAN_POINT('Ctrl Pts',(-10.5940858660567,-17.3721097278627,
-18.8525118436365)) ;
#47416 = CARTESIAN_POINT('Ctrl Pts',(-9.98189435482839,-17.7309509640586,
-18.8346221442252)) ;
#47417 = CARTESIAN_POINT('Ctrl Pts',(-8.82726945297243,-18.3289604427553,
-18.8015896385066)) ;
#47418 = CARTESIAN_POINT('Ctrl Pts',(-8.29071525236168,-18.5778232834481,
-18.7865055273131)) ;
#47419 = CARTESIAN_POINT('Ctrl Pts',(-7.4025904895691,-18.9436015118526,-18.762216332225)) ;
#47420 = CARTESIAN_POINT('Ctrl Pts',(-7.05732577562666,-19.0749192245182,
-18.7529378888639)) ;
#47421 = CARTESIAN_POINT('Ctrl Pts',(-6.28728242922303,-19.3440254796917,
-18.7327229980836)) ;
#47422 = CARTESIAN_POINT('Ctrl Pts',(-5.8611544756378,-19.4773744475153,-18.721828990046)) ;
#47423 = CARTESIAN_POINT('Ctrl Pts',(-4.73953746200831,-19.788218377024,-18.6935374442036)) ;
#47424 = CARTESIAN_POINT('Ctrl Pts',(-4.03843667378955,-19.9431148823256,
-18.6762152167227)) ;
#47425 = CARTESIAN_POINT('Ctrl Pts',(-2.76005634444794,-20.1553613272529,
-18.6445452508762)) ;
#47426 = CARTESIAN_POINT('Ctrl Pts',(-2.18571633844797,-20.2257048668193,
-18.6302907601886)) ;
#47427 = CARTESIAN_POINT('Ctrl Pts',(-0.923294002832888,-20.3259168481181,
-18.598704599547)) ;
#47428 = CARTESIAN_POINT('Ctrl Pts',(-0.235108075118919,-20.3455174101044,
-18.5813167925383)) ;
#47429 = CARTESIAN_POINT('Ctrl Pts',(1.02241373347908,-20.317513281118,-18.5493380518093)) ;
#47430 = CARTESIAN_POINT('Ctrl Pts',(1.59130339713737,-20.2808882980299,-18.534798406541)) ;
#47431 = CARTESIAN_POINT('Ctrl Pts',(2.51888859506176,-20.1818973626806,-18.5112095472917)) ;
#47432 = CARTESIAN_POINT('Ctrl Pts',(2.87878247588108,-20.1337129863791,-18.5020908386088)) ;
#47433 = CARTESIAN_POINT('Ctrl Pts',(3.67771435434724,-20.0048869989137,-18.4820370164804)) ;
#47434 = CARTESIAN_POINT('Ctrl Pts',(4.11577711690003,-19.919374249163,-18.4711476139617)) ;
#47435 = CARTESIAN_POINT('Ctrl Pts',(5.25042337946643,-19.6588530614843,-18.4428501496224)) ;
#47436 = CARTESIAN_POINT('Ctrl Pts',(5.94117238174564,-19.4612414859511,-18.4255175039371)) ;
#47437 = CARTESIAN_POINT('Ctrl Pts',(7.16761236786596,-19.0389789873187,-18.3938184776607)) ;
#47438 = CARTESIAN_POINT('Ctrl Pts',(7.70689567547357,-18.8271383639402,-18.3795452897704)) ;
#47439 = CARTESIAN_POINT('Ctrl Pts',(8.85389579923341,-18.3190241824908,-18.3482561934812)) ;
#47440 = CARTESIAN_POINT('Ctrl Pts',(9.45737807719095,-18.0148856618515,-18.3311935019025)) ;
#47441 = CARTESIAN_POINT('Ctrl Pts',(10.5452420009221,-17.3968786234229,-18.2993935396737)) ;
#47442 = CARTESIAN_POINT('Ctrl Pts',(11.0335764341507,-17.0913342525883,-18.2847025827745)) ;
#47443 = CARTESIAN_POINT('Ctrl Pts',(11.8091211314112,-16.558979096446,-18.2609167990149)) ;
#47444 = CARTESIAN_POINT('Ctrl Pts',(12.1043472471194,-16.3444153955662,-18.2517514945396)) ;
#47445 = CARTESIAN_POINT('Ctrl Pts',(12.7495456306156,-15.8484255848568,-18.231585389155)) ;
#47446 = CARTESIAN_POINT('Ctrl Pts',(13.0962931409228,-15.5631172451814,-18.2206311136396)) ;
#47447 = CARTESIAN_POINT('Ctrl Pts',(13.9708355679073,-14.7935922487522,-18.1923172717652)) ;
#47448 = CARTESIAN_POINT('Ctrl Pts',(14.4830007830972,-14.2925612255671,-18.1750308200972)) ;
#47449 = CARTESIAN_POINT('Ctrl Pts',(15.3592998966792,-13.339737377673,-18.1433928139863)) ;
#47450 = CARTESIAN_POINT('Ctrl Pts',(15.7325739393583,-12.8973949257823,-18.1291335339469)) ;
#47451 = CARTESIAN_POINT('Ctrl Pts',(16.4991502949351,-11.906095263746,-18.0978771568599)) ;
#47452 = CARTESIAN_POINT('Ctrl Pts',(16.8850095394674,-11.3522467141343,-18.0808334142567)) ;
#47453 = CARTESIAN_POINT('Ctrl Pts',(17.5481505136909,-10.2915765998809,-18.0490381106713)) ;
#47454 = CARTESIAN_POINT('Ctrl Pts',(17.8327627888323,-9.79013316761127,-18.0343325139809)) ;
#47455 = CARTESIAN_POINT('Ctrl Pts',(18.1076721718333,-9.25391181964499,-18.0190947825227)) ;
#47456 = CARTESIAN_POINT('Ctrl Pts',(18.1196070436432,-9.23052089544325,-18.0184310503742)) ;
#47457 = CARTESIAN_POINT('Ctrl Pts',(18.1314964403967,-9.20710718355568,-18.0177676543358)) ;
#47458 = CARTESIAN_POINT('Origin',(0.,0.,-10.)) ;
#47459 = CARTESIAN_POINT('',(-15.4053915293257,-15.8878358795928,-19.9995644016859)) ;
#47460 = CARTESIAN_POINT('Ctrl Pts',(0.000517204814065366,-22.1295393890992,
-19.6112894184499)) ;
#47461 = CARTESIAN_POINT('Ctrl Pts',(-0.443938333285866,-22.1294510254483,
-19.6216081794502)) ;
#47462 = CARTESIAN_POINT('Ctrl Pts',(-0.888412087382889,-22.1159901751952,
-19.631889439891)) ;
#47463 = CARTESIAN_POINT('Ctrl Pts',(-1.33208775265979,-22.089181583779,-19.6421021187407)) ;
#47464 = CARTESIAN_POINT('Ctrl Pts',(-1.77574594138311,-22.0623740483635,
-19.6523143953091)) ;
#47465 = CARTESIAN_POINT('Ctrl Pts',(-2.21860527133772,-22.0222244031857,
-19.6624606548461)) ;
#47466 = CARTESIAN_POINT('Ctrl Pts',(-2.6598611774855,-21.9688516945317,-19.6725658729284)) ;
#47467 = CARTESIAN_POINT('Ctrl Pts',(-3.10116451285207,-21.9154732490119,
-19.682672177189)) ;
#47468 = CARTESIAN_POINT('Ctrl Pts',(-3.54085748810537,-21.8488099814255,
-19.6927032784351)) ;
#47469 = CARTESIAN_POINT('Ctrl Pts',(-3.97813233981979,-21.7689943996938,
-19.7026926516773)) ;
#47470 = CARTESIAN_POINT('Ctrl Pts',(-4.41541786596682,-21.6891768695626,
-19.7126822687728)) ;
#47471 = CARTESIAN_POINT('Ctrl Pts',(-4.85028556482805,-21.5962062291834,
-19.7226302422428)) ;
#47472 = CARTESIAN_POINT('Ctrl Pts',(-5.28192893157152,-21.490233790291,-19.7325803346779)) ;
#47473 = CARTESIAN_POINT('Ctrl Pts',(-5.7136591075495,-21.3842400389287,-19.7425324282092)) ;
#47474 = CARTESIAN_POINT('Ctrl Pts',(-6.14216362728143,-21.2652390974891,
-19.7524867832956)) ;
#47475 = CARTESIAN_POINT('Ctrl Pts',(-6.56663819984437,-21.133423656613,-19.7625076025576)) ;
#47476 = CARTESIAN_POINT('Ctrl Pts',(-6.85602864659768,-21.0435569560147,
-19.7693394119297)) ;
#47477 = CARTESIAN_POINT('Ctrl Pts',(-7.14354602853844,-20.9477349414254,
-19.7762025441723)) ;
#47478 = CARTESIAN_POINT('Ctrl Pts',(-7.4289363685051,-20.8460303363535,-19.7831221737644)) ;
#47479 = CARTESIAN_POINT('Ctrl Pts',(-7.84649270955411,-20.6972257104976,
-19.793246325879)) ;
#47480 = CARTESIAN_POINT('Ctrl Pts',(-8.25960939184134,-20.5357846370997,
-19.8034926402938)) ;
#47481 = CARTESIAN_POINT('Ctrl Pts',(-8.66753180167299,-20.3620402476045,
-19.8137830126411)) ;
#47482 = CARTESIAN_POINT('Ctrl Pts',(-9.07538988208743,-20.1883232576222,
-19.8240717621953)) ;
#47483 = CARTESIAN_POINT('Ctrl Pts',(-9.47805541762666,-20.0023069804755,
-19.8344044009316)) ;
#47484 = CARTESIAN_POINT('Ctrl Pts',(-9.87479772637341,-19.8043587983951,
-19.8447226647033)) ;
#47485 = CARTESIAN_POINT('Ctrl Pts',(-10.2714974529698,-19.6064318619925,
-19.8550398210211)) ;
#47486 = CARTESIAN_POINT('Ctrl Pts',(-10.6622752997502,-19.3965756633295,
-19.865342510328)) ;
#47487 = CARTESIAN_POINT('Ctrl Pts',(-11.0464231416791,-19.1751901534458,
-19.8755941555047)) ;
#47488 = CARTESIAN_POINT('Ctrl Pts',(-11.4416425018511,-18.9474240956482,
-19.8861412631681)) ;
#47489 = CARTESIAN_POINT('Ctrl Pts',(-11.8298441287601,-18.7074544386025,
-19.8966341791439)) ;
#47490 = CARTESIAN_POINT('Ctrl Pts',(-12.2102804888824,-18.4557519688425,
-19.9070581446796)) ;
#47491 = CARTESIAN_POINT('Ctrl Pts',(-12.5800624893015,-18.2110985851639,
-19.9171901805)) ;
#47492 = CARTESIAN_POINT('Ctrl Pts',(-12.942508194326,-17.9553604838846,-19.927257195051)) ;
#47493 = CARTESIAN_POINT('Ctrl Pts',(-13.2969522795948,-17.6890023990348,
-19.9372689073098)) ;
#47494 = CARTESIAN_POINT('Ctrl Pts',(-13.6667150179138,-17.4111326336167,
-19.9477133139)) ;
#47495 = CARTESIAN_POINT('Ctrl Pts',(-14.0277693542131,-17.1217047382201,
-19.9580974249735)) ;
#47496 = CARTESIAN_POINT('Ctrl Pts',(-14.3793841502957,-16.8212842661519,
-19.9684582702009)) ;
#47497 = CARTESIAN_POINT('Ctrl Pts',(-14.7309989463784,-16.5208637940836,
-19.9788191154282)) ;
#47498 = CARTESIAN_POINT('Ctrl Pts',(-15.0731741100143,-16.209450612742,-19.9891568361822)) ;
#47499 = CARTESIAN_POINT('Ctrl Pts',(-15.4052041408659,-15.8876506360391,
-19.9995334132552)) ;
#47500 = CARTESIAN_POINT('Origin',(0.,0.,-20.)) ;
#47501 = CARTESIAN_POINT('Origin',(0.,0.,-328.125)) ;
#47502 = CARTESIAN_POINT('',(1.53120055501316,-19.364905768565,-337.99978912964)) ;
#47503 = CARTESIAN_POINT('Ctrl Pts',(2.0594453916303E-9,-19.425,-336.519643262718)) ;
#47504 = CARTESIAN_POINT('Ctrl Pts',(-0.0932399363564652,-19.4250000000099,
-336.520817928714)) ;
#47505 = CARTESIAN_POINT('Ctrl Pts',(-0.186482031227195,-19.4243286729344,
-336.521988828568)) ;
#47506 = CARTESIAN_POINT('Ctrl Pts',(-0.437812431282591,-19.420709152349,
-336.525134336585)) ;
#47507 = CARTESIAN_POINT('Ctrl Pts',(-0.595872264667102,-19.4165022608218,
-336.527101170528)) ;
#47508 = CARTESIAN_POINT('Ctrl Pts',(-0.877973804678461,-19.4055459512161,
-336.530591059154)) ;
#47509 = CARTESIAN_POINT('Ctrl Pts',(-1.00203536493703,-19.399535480021,-336.532118765596)) ;
#47510 = CARTESIAN_POINT('Ctrl Pts',(-1.27015707153849,-19.3839667876486,
-336.535405727605)) ;
#47511 = CARTESIAN_POINT('Ctrl Pts',(-1.41418564513392,-19.3739914948649,
-336.537162194948)) ;
#47512 = CARTESIAN_POINT('Ctrl Pts',(-1.83867860905591,-19.3398326232978,
-336.542314408147)) ;
#47513 = CARTESIAN_POINT('Ctrl Pts',(-2.11874382755672,-19.3111571366231,
-336.545681488894)) ;
#47514 = CARTESIAN_POINT('Ctrl Pts',(-2.80579095317782,-19.2256848282012,
-336.553891732014)) ;
#47515 = CARTESIAN_POINT('Ctrl Pts',(-3.21178331669986,-19.1620423860537,
-336.558698785826)) ;
#47516 = CARTESIAN_POINT('Ctrl Pts',(-4.15907185381896,-18.9825939798755,
-336.569960638012)) ;
#47517 = CARTESIAN_POINT('Ctrl Pts',(-4.69804248177032,-18.8564351352946,
-336.576400596075)) ;
#47518 = CARTESIAN_POINT('Ctrl Pts',(-5.34085268612161,-18.6766955049485,
-336.584413229374)) ;
#47519 = CARTESIAN_POINT('Ctrl Pts',(-5.45054292064655,-18.6449790617679,
-336.585792685071)) ;
#47520 = CARTESIAN_POINT('Ctrl Pts',(-5.61962219651297,-18.5944709599256,
-336.587941886695)) ;
#47521 = CARTESIAN_POINT('Ctrl Pts',(-5.67921127609178,-18.576357640339,-336.588703753552)) ;
#47522 = CARTESIAN_POINT('Ctrl Pts',(-5.80618975223359,-18.5370918480951,
-336.590337599799)) ;
#47523 = CARTESIAN_POINT('Ctrl Pts',(-5.87355296840774,-18.5158577746769,
-336.591210649143)) ;
#47524 = CARTESIAN_POINT('Ctrl Pts',(-6.05719493870232,-18.4568675697922,
-336.593606392374)) ;
#47525 = CARTESIAN_POINT('Ctrl Pts',(-6.17323538701914,-18.4183803794854,
-336.595137448162)) ;
#47526 = CARTESIAN_POINT('Ctrl Pts',(-6.69814358877089,-18.2387659571691,
-336.602129414365)) ;
#47527 = CARTESIAN_POINT('Ctrl Pts',(-7.10259073286086,-18.0851020201597,
-336.607697398786)) ;
#47528 = CARTESIAN_POINT('Ctrl Pts',(-8.14504514366601,-17.6486685146565,
-336.622273874247)) ;
#47529 = CARTESIAN_POINT('Ctrl Pts',(-8.77354446913076,-17.3448028278548,
-336.631274998696)) ;
#47530 = CARTESIAN_POINT('Ctrl Pts',(-9.54353642583983,-16.9199467795189,
-336.642327423058)) ;
#47531 = CARTESIAN_POINT('Ctrl Pts',(-9.70149727682105,-16.829873358518,-336.644597576333)) ;
#47532 = CARTESIAN_POINT('Ctrl Pts',(-9.96663503107536,-16.673711551087,-336.648411961506)) ;
#47533 = CARTESIAN_POINT('Ctrl Pts',(-10.0744762034533,-16.6087747894376,
-336.649964558199)) ;
#47534 = CARTESIAN_POINT('Ctrl Pts',(-10.2951897376559,-16.4729310964918,
-336.653144959106)) ;
#47535 = CARTESIAN_POINT('Ctrl Pts',(-10.4079788399579,-16.4019013278264,
-336.654771724497)) ;
#47536 = CARTESIAN_POINT('Ctrl Pts',(-10.7026634114779,-16.2120578610165,
-336.659027533178)) ;
#47537 = CARTESIAN_POINT('Ctrl Pts',(-10.8833122174686,-16.0913436227656,
-336.661641959856)) ;
#47538 = CARTESIAN_POINT('Ctrl Pts',(-11.1823562497442,-15.8841747560948,
-336.665986907985)) ;
#47539 = CARTESIAN_POINT('Ctrl Pts',(-11.3018661284412,-15.7993645773874,
-336.667728062783)) ;
#47540 = CARTESIAN_POINT('Ctrl Pts',(-11.8073219637408,-15.4319978673641,
-336.675121317241)) ;
#47541 = CARTESIAN_POINT('Ctrl Pts',(-12.1837204501755,-15.1365903169809,
-336.680696112652)) ;
#47542 = CARTESIAN_POINT('Ctrl Pts',(-12.8827794222124,-14.5449654146986,
-336.691396514641)) ;
#47543 = CARTESIAN_POINT('Ctrl Pts',(-13.2070842919666,-14.2511384541469,
-336.696517709031)) ;
#47544 = CARTESIAN_POINT('Ctrl Pts',(-13.6071877956029,-13.8632395980686,
-336.703199766062)) ;
#47545 = CARTESIAN_POINT('Ctrl Pts',(-13.6924122803886,-13.7790717299404,
-336.704645401288)) ;
#47546 = CARTESIAN_POINT('Ctrl Pts',(-13.8214511986546,-13.6492532364941,
-336.706873235367)) ;
#47547 = CARTESIAN_POINT('Ctrl Pts',(-13.8658301763447,-13.6041677680148,
-336.707646616925)) ;
#47548 = CARTESIAN_POINT('Ctrl Pts',(-13.9584666964118,-13.5091323235117,
-336.709277089246)) ;
#47549 = CARTESIAN_POINT('Ctrl Pts',(-14.0066781541244,-13.4591387430914,
-336.710135019795)) ;
#47550 = CARTESIAN_POINT('Ctrl Pts',(-14.1348614913577,-13.3247824730548,
-336.712439903972)) ;
#47551 = CARTESIAN_POINT('Ctrl Pts',(-14.2143459513204,-13.2399587027821,
-336.713894223156)) ;
#47552 = CARTESIAN_POINT('Ctrl Pts',(-14.5497838709389,-12.8754855253364,
-336.720129798047)) ;
#47553 = CARTESIAN_POINT('Ctrl Pts',(-14.7982826011156,-12.5890892999906,
-336.724994902363)) ;
#47554 = CARTESIAN_POINT('Ctrl Pts',(-15.5393599941566,-11.6827085792831,
-336.74008021623)) ;
#47555 = CARTESIAN_POINT('Ctrl Pts',(-16.0025444915835,-11.0397449952403,
-336.750323075549)) ;
#47556 = CARTESIAN_POINT('Ctrl Pts',(-16.5066143176558,-10.2413653851955,
-336.762164130865)) ;
#47557 = CARTESIAN_POINT('Ctrl Pts',(-16.5865072431808,-10.111461750974,-336.764065870962)) ;
#47558 = CARTESIAN_POINT('Ctrl Pts',(-16.7295214137403,-9.87266807926668,
-336.767516173564)) ;
#47559 = CARTESIAN_POINT('Ctrl Pts',(-16.79312990494,-9.76407956648395,-336.769068295499)) ;
#47560 = CARTESIAN_POINT('Ctrl Pts',(-16.9219603268634,-9.53916490331754,
-336.772249007843)) ;
#47561 = CARTESIAN_POINT('Ctrl Pts',(-16.9870485830582,-9.42276970164219,
-336.773876546069)) ;
#47562 = CARTESIAN_POINT('Ctrl Pts',(-17.1551866137313,-9.11468904250896,
-336.778137517084)) ;
#47563 = CARTESIAN_POINT('Ctrl Pts',(-17.2562226619409,-8.92192601160737,
-336.780756263977)) ;
#47564 = CARTESIAN_POINT('Ctrl Pts',(-17.4200006206966,-8.59626567971618,
-336.78510972126)) ;
#47565 = CARTESIAN_POINT('Ctrl Pts',(-17.4845118295128,-8.4642809146057,-336.786855079297)) ;
#47566 = CARTESIAN_POINT('Ctrl Pts',(-17.7535687328234,-7.89760772597241,
-336.794276859595)) ;
#47567 = CARTESIAN_POINT('Ctrl Pts',(-17.9434481261956,-7.45614378709459,
-336.799875357001)) ;
#47568 = CARTESIAN_POINT('Ctrl Pts',(-18.2783043009703,-6.59050055233403,
-336.810720433661)) ;
#47569 = CARTESIAN_POINT('Ctrl Pts',(-18.4253553299155,-6.16744554815007,
-336.81596267458)) ;
#47570 = CARTESIAN_POINT('Ctrl Pts',(-18.5909222067315,-5.63213207966579,
-336.822691517152)) ;
#47571 = CARTESIAN_POINT('Ctrl Pts',(-18.6232528645947,-5.52428755110498,
-336.824052080844)) ;
#47572 = CARTESIAN_POINT('Ctrl Pts',(-18.6719336766177,-5.35661860306861,
-336.826178946924)) ;
#47573 = CARTESIAN_POINT('Ctrl Pts',(-18.6889379856181,-5.29698660022334,
-336.82693763165)) ;
#47574 = CARTESIAN_POINT('Ctrl Pts',(-18.7248065741668,-5.16887692633256,
-336.828573314663)) ;
#47575 = CARTESIAN_POINT('Ctrl Pts',(-18.7435813891906,-5.1003751440834,-336.829451452423)) ;
#47576 = CARTESIAN_POINT('Ctrl Pts',(-18.7941633921243,-4.91176991077936,
-336.831877348192)) ;
#47577 = CARTESIAN_POINT('Ctrl Pts',(-18.8251946493792,-4.79146194903191,
-336.833433805025)) ;
#47578 = CARTESIAN_POINT('Ctrl Pts',(-18.8944370392451,-4.51194837952161,
-336.837064297007)) ;
#47579 = CARTESIAN_POINT('Ctrl Pts',(-18.9317938281932,-4.35254081475044,
-336.839145477567)) ;
#47580 = CARTESIAN_POINT('Ctrl Pts',(-19.0646827902067,-3.75136873252276,
-336.847012439797)) ;
#47581 = CARTESIAN_POINT('Ctrl Pts',(-19.1468027682881,-3.30678710058974,
-336.852863885669)) ;
#47582 = CARTESIAN_POINT('Ctrl Pts',(-19.2246853040365,-2.78352972482662,
-336.859680770063)) ;
#47583 = CARTESIAN_POINT('Ctrl Pts',(-19.2355759996943,-2.70724559876217,
-336.860672957291)) ;
#47584 = CARTESIAN_POINT('Ctrl Pts',(-19.3082840794795,-2.17535867310543,
-336.867577301558)) ;
#47585 = CARTESIAN_POINT('Ctrl Pts',(-19.3543626779806,-1.71775049508685,
-336.873443741863)) ;
#47586 = CARTESIAN_POINT('Ctrl Pts',(-19.3941296516603,-1.10544937641824,
-336.881140759919)) ;
#47587 = CARTESIAN_POINT('Ctrl Pts',(-19.4022748737262,-0.951847193779062,
-336.88305930149)) ;
#47588 = CARTESIAN_POINT('Ctrl Pts',(-19.4137775513485,-0.672141883388968,
-336.886530025245)) ;
#47589 = CARTESIAN_POINT('Ctrl Pts',(-19.4177325949734,-0.546071830203471,
-336.888085926079)) ;
#47590 = CARTESIAN_POINT('Ctrl Pts',(-19.4233317105399,-0.287156076884228,
-336.891264417035)) ;
#47591 = CARTESIAN_POINT('Ctrl Pts',(-19.4248413276285,-0.15431397456903,
-336.892886058407)) ;
#47592 = CARTESIAN_POINT('Ctrl Pts',(-19.4252255241112,0.193340499314378,
-336.897107539617)) ;
#47593 = CARTESIAN_POINT('Ctrl Pts',(-19.4218997918328,0.408137110628826,
-336.899693220993)) ;
#47594 = CARTESIAN_POINT('Ctrl Pts',(-19.4103906319138,0.766900900875649,
-336.903981670201)) ;
#47595 = CARTESIAN_POINT('Ctrl Pts',(-19.4041655807187,0.91091143649217,-336.905694974084)) ;
#47596 = CARTESIAN_POINT('Ctrl Pts',(-19.371101702899,1.51888849071464,-336.912902078713)) ;
#47597 = CARTESIAN_POINT('Ctrl Pts',(-19.3292199688169,1.98188273930557,-336.918322554117)) ;
#47598 = CARTESIAN_POINT('Ctrl Pts',(-19.2559858084066,2.55958247990601,-336.92512500964)) ;
#47599 = CARTESIAN_POINT('Ctrl Pts',(-19.240138773627,2.67610012650855,-336.926499271397)) ;
#47600 = CARTESIAN_POINT('Ctrl Pts',(-19.1732660256986,3.13644959152543,-336.931946149509)) ;
#47601 = CARTESIAN_POINT('Ctrl Pts',(-19.1140734604698,3.47902873041371,-336.9360368036)) ;
#47602 = CARTESIAN_POINT('Ctrl Pts',(-19.0229289232856,3.93347609997459,-336.941598865425)) ;
#47603 = CARTESIAN_POINT('Ctrl Pts',(-18.9991200440024,4.04691197644356,-336.942998710324)) ;
#47604 = CARTESIAN_POINT('Ctrl Pts',(-18.9608952318669,4.22125492561033,-336.945172078281)) ;
#47605 = CARTESIAN_POINT('Ctrl Pts',(-18.9471977708225,4.28231686861727,-336.945937437026)) ;
#47606 = CARTESIAN_POINT('Ctrl Pts',(-18.9175017472154,4.41176669421849,-336.947569760949)) ;
#47607 = CARTESIAN_POINT('Ctrl Pts',(-18.9014268759759,4.48013613065623,-336.948437722995)) ;
#47608 = CARTESIAN_POINT('Ctrl Pts',(-18.8568240761534,4.66532651464416,-336.950803163031)) ;
#47609 = CARTESIAN_POINT('Ctrl Pts',(-18.8275815835364,4.78197212226039,-336.952308667788)) ;
#47610 = CARTESIAN_POINT('Ctrl Pts',(-18.6928706717891,5.29892205193121,-336.959038826722)) ;
#47611 = CARTESIAN_POINT('Ctrl Pts',(-18.5757051307394,5.69606590667437,-336.964362233717)) ;
#47612 = CARTESIAN_POINT('Ctrl Pts',(-18.2190052609059,6.77661939431064,-336.979035108164)) ;
#47613 = CARTESIAN_POINT('Ctrl Pts',(-17.953814835661,7.4508565854904,-336.988385055213)) ;
#47614 = CARTESIAN_POINT('Ctrl Pts',(-17.5764752896891,8.27227528831179,-336.999742246111)) ;
#47615 = CARTESIAN_POINT('Ctrl Pts',(-17.4990702768557,8.43478284480902,-337.001988909423)) ;
#47616 = CARTESIAN_POINT('Ctrl Pts',(-17.3638367771565,8.70882151620314,-337.005776342066)) ;
#47617 = CARTESIAN_POINT('Ctrl Pts',(-17.3071645599781,8.82091008723147,-337.007325189855)) ;
#47618 = CARTESIAN_POINT('Ctrl Pts',(-17.1878709717617,9.05127756119131,-337.010508195806)) ;
#47619 = CARTESIAN_POINT('Ctrl Pts',(-17.1251062666605,9.16947487288916,-337.012141207953)) ;
#47620 = CARTESIAN_POINT('Ctrl Pts',(-16.9558324021988,9.48044700104593,-337.016438833474)) ;
#47621 = CARTESIAN_POINT('Ctrl Pts',(-16.8472575684354,9.67207529140804,-337.019088264878)) ;
#47622 = CARTESIAN_POINT('Ctrl Pts',(-16.6595544060381,9.99060652608387,-337.023502313373)) ;
#47623 = CARTESIAN_POINT('Ctrl Pts',(-16.5821769365317,10.118516683347,-337.025277677188)) ;
#47624 = CARTESIAN_POINT('Ctrl Pts',(-16.2419306873566,10.6665802097644,-337.032906647488)) ;
#47625 = CARTESIAN_POINT('Ctrl Pts',(-15.9645121626727,11.0774815469406,-337.038677730783)) ;
#47626 = CARTESIAN_POINT('Ctrl Pts',(-15.6020939760801,11.5723446442803,-337.045847318519)) ;
#47627 = CARTESIAN_POINT('Ctrl Pts',(-15.5316408375656,11.6667317567326,-337.047225373313)) ;
#47628 = CARTESIAN_POINT('Ctrl Pts',(-15.2576708533874,12.0268930907225,-337.052533094905)) ;
#47629 = CARTESIAN_POINT('Ctrl Pts',(-15.0481555965974,12.2880303329275,-337.056485097318)) ;
#47630 = CARTESIAN_POINT('Ctrl Pts',(-14.7680945245478,12.6191839013059,-337.061709953994)) ;
#47631 = CARTESIAN_POINT('Ctrl Pts',(-14.7036145813474,12.6942560406728,-337.062909198853)) ;
#47632 = CARTESIAN_POINT('Ctrl Pts',(-14.5948240913371,12.8189766513426,-337.06492929665)) ;
#47633 = CARTESIAN_POINT('Ctrl Pts',(-14.5508269920663,12.8688960870743,-337.065745449478)) ;
#47634 = CARTESIAN_POINT('Ctrl Pts',(-14.4540721229268,12.9775443097679,-337.067539251871)) ;
#47635 = CARTESIAN_POINT('Ctrl Pts',(-14.4012111900408,13.0361794052395,-337.068518417823)) ;
#47636 = CARTESIAN_POINT('Ctrl Pts',(-14.2354383726852,13.2178212515843,-337.071584096622)) ;
#47637 = CARTESIAN_POINT('Ctrl Pts',(-14.1212970547502,13.3396954103467,-337.073687756638)) ;
#47638 = CARTESIAN_POINT('Ctrl Pts',(-13.9132447483226,13.5561797537833,-337.077497611279)) ;
#47639 = CARTESIAN_POINT('Ctrl Pts',(-13.8199040787608,13.6513237506652,-337.079198274931)) ;
#47640 = CARTESIAN_POINT('Ctrl Pts',(-13.3099664473865,14.160522833174,-337.088427065569)) ;
#47641 = CARTESIAN_POINT('Ctrl Pts',(-12.8757312236508,14.5564817439944,-337.096054398083)) ;
#47642 = CARTESIAN_POINT('Ctrl Pts',(-12.3479303372895,14.9956357558583,-337.10485421796)) ;
#47643 = CARTESIAN_POINT('Ctrl Pts',(-12.2711515105281,15.0585296745026,-337.10612355679)) ;
#47644 = CARTESIAN_POINT('Ctrl Pts',(-11.945087914446,15.3214771646536,-337.111466894374)) ;
#47645 = CARTESIAN_POINT('Ctrl Pts',(-11.6913670941144,15.5159506307828,-337.115508352529)) ;
#47646 = CARTESIAN_POINT('Ctrl Pts',(-11.3116032948264,15.7924282601706,-337.121376512292)) ;
#47647 = CARTESIAN_POINT('Ctrl Pts',(-11.1892233030353,15.8793715684466,-337.123241042065)) ;
#47648 = CARTESIAN_POINT('Ctrl Pts',(-10.9639990229506,16.0354827570472,-337.126624455108)) ;
#47649 = CARTESIAN_POINT('Ctrl Pts',(-10.8614770186616,16.1051016403574,-337.128146816652)) ;
#47650 = CARTESIAN_POINT('Ctrl Pts',(-10.6324475662309,16.2574453400723,-337.131509175431)) ;
#47651 = CARTESIAN_POINT('Ctrl Pts',(-10.5056265021067,16.3396842721349,-337.133345350818)) ;
#47652 = CARTESIAN_POINT('Ctrl Pts',(-10.101409512572,16.5951529466455,-337.139120625776)) ;
#47653 = CARTESIAN_POINT('Ctrl Pts',(-9.8205920893311,16.7628621397094,-337.143018620762)) ;
#47654 = CARTESIAN_POINT('Ctrl Pts',(-9.06285985566667,17.1898145876359,-337.153292347504)) ;
#47655 = CARTESIAN_POINT('Ctrl Pts',(-8.57908789853119,17.4362956180977,-337.159597424921)) ;
#47656 = CARTESIAN_POINT('Ctrl Pts',(-7.76701170969713,17.808058549328,-337.170054129785)) ;
#47657 = CARTESIAN_POINT('Ctrl Pts',(-7.44450265829797,17.945272340401,-337.174177318783)) ;
#47658 = CARTESIAN_POINT('Ctrl Pts',(-7.01043634613248,18.1162326784918,-337.179775428474)) ;
#47659 = CARTESIAN_POINT('Ctrl Pts',(-6.90203370641882,18.1578091982948,-337.181177576077)) ;
#47660 = CARTESIAN_POINT('Ctrl Pts',(-6.73460577951777,18.2203081853747,-337.18335367559)) ;
#47661 = CARTESIAN_POINT('Ctrl Pts',(-6.67584107059158,18.2419212629816,-337.18411943076)) ;
#47662 = CARTESIAN_POINT('Ctrl Pts',(-6.55098358702901,18.2871584796726,-337.185751567099)) ;
#47663 = CARTESIAN_POINT('Ctrl Pts',(-6.48486521753937,18.3107092791357,-337.186618936748)) ;
#47664 = CARTESIAN_POINT('Ctrl Pts',(-6.30533538774961,18.3735619081618,-337.188980944462)) ;
#47665 = CARTESIAN_POINT('Ctrl Pts',(-6.19168498276405,18.412171750099,-337.190483572315)) ;
#47666 = CARTESIAN_POINT('Ctrl Pts',(-5.68643268984749,18.5786112907339,-337.19718507131)) ;
#47667 = CARTESIAN_POINT('Ctrl Pts',(-5.29118084729902,18.6950185484329,-337.202481808619)) ;
#47668 = CARTESIAN_POINT('Ctrl Pts',(-4.1888230164595,18.9819158715144,-337.217169350238)) ;
#47669 = CARTESIAN_POINT('Ctrl Pts',(-3.47538560463534,19.1254038215622,-337.22656164516)) ;
#47670 = CARTESIAN_POINT('Ctrl Pts',(-2.57772929742838,19.2540442355816,-337.237954489448)) ;
#47671 = CARTESIAN_POINT('Ctrl Pts',(-2.39952706875236,19.2770635144706,-337.240197090344)) ;
#47672 = CARTESIAN_POINT('Ctrl Pts',(-2.0963074048896,19.3119621556334,-337.2439798348)) ;
#47673 = CARTESIAN_POINT('Ctrl Pts',(-1.97144749576689,19.3251075509596,-337.245528008096)) ;
#47674 = CARTESIAN_POINT('Ctrl Pts',(-1.71316020523088,19.3497710669643,-337.248711408511)) ;
#47675 = CARTESIAN_POINT('Ctrl Pts',(-1.57972340281974,19.3611216684549,-337.250345471092)) ;
#47676 = CARTESIAN_POINT('Ctrl Pts',(-1.22604286094508,19.3875262547419,-337.254650306721)) ;
#47677 = CARTESIAN_POINT('Ctrl Pts',(-1.00564154611199,19.4002072330722,-337.257305798409)) ;
#47678 = CARTESIAN_POINT('Ctrl Pts',(-0.635190896935972,19.415191437799,-337.261731862867)) ;
#47679 = CARTESIAN_POINT('Ctrl Pts',(-0.485244701709166,19.419517596499,-337.263513201341)) ;
#47680 = CARTESIAN_POINT('Ctrl Pts',(0.16336220447468,19.4307138145487,-337.271184261728)) ;
#47681 = CARTESIAN_POINT('Ctrl Pts',(0.662134599086393,19.4201159752898,-337.276990505297)) ;
#47682 = CARTESIAN_POINT('Ctrl Pts',(1.20783267635062,19.3874719004165,-337.283380895291)) ;
#47683 = CARTESIAN_POINT('Ctrl Pts',(1.25570985958266,19.3844298139345,-337.283941931733)) ;
#47684 = CARTESIAN_POINT('Ctrl Pts',(1.395782743042,19.3750085474562,-337.285584852241)) ;
#47685 = CARTESIAN_POINT('Ctrl Pts',(1.48794475547531,19.368148751909,-337.286667738227)) ;
#47686 = CARTESIAN_POINT('Ctrl Pts',(1.88838266320089,19.3354683289965,-337.291385896569)) ;
#47687 = CARTESIAN_POINT('Ctrl Pts',(2.19606541730352,19.3029433116019,-337.29504426411)) ;
#47688 = CARTESIAN_POINT('Ctrl Pts',(2.60014212586808,19.2504419077123,-337.299954209917)) ;
#47689 = CARTESIAN_POINT('Ctrl Pts',(2.69734790130677,19.2370623271617,-337.301143502725)) ;
#47690 = CARTESIAN_POINT('Ctrl Pts',(2.86019102082799,19.213389753102,-337.303152330722)) ;
#47691 = CARTESIAN_POINT('Ctrl Pts',(2.92588448927209,19.2034954746021,-337.303967295423)) ;
#47692 = CARTESIAN_POINT('Ctrl Pts',(3.069978889725,19.1810364420111,-337.305765633271)) ;
#47693 = CARTESIAN_POINT('Ctrl Pts',(3.14835597542005,19.168327626682,-337.306750599416)) ;
#47694 = CARTESIAN_POINT('Ctrl Pts',(3.39396437152533,19.1269552801246,-337.309856105849)) ;
#47695 = CARTESIAN_POINT('Ctrl Pts',(3.56089924296837,19.0965810779338,-337.311994403014)) ;
#47696 = CARTESIAN_POINT('Ctrl Pts',(4.24480424374507,18.9628633802921,-337.320839658585)) ;
#47697 = CARTESIAN_POINT('Ctrl Pts',(4.75786115287742,18.8406822483589,-337.32766953999)) ;
#47698 = CARTESIAN_POINT('Ctrl Pts',(5.79705977888661,18.5480430759569,-337.341585146711)) ;
#47699 = CARTESIAN_POINT('Ctrl Pts',(6.32218009726688,18.3756862808139,-337.348659829125)) ;
#47700 = CARTESIAN_POINT('Ctrl Pts',(6.98316398906478,18.1270430833586,-337.357518497918)) ;
#47701 = CARTESIAN_POINT('Ctrl Pts',(7.12644009423608,18.071195918201,-337.359436493387)) ;
#47702 = CARTESIAN_POINT('Ctrl Pts',(7.3859998816988,17.96645592234,-337.362906624052)) ;
#47703 = CARTESIAN_POINT('Ctrl Pts',(7.50249928539296,17.9181203585504,-337.364462471747)) ;
#47704 = CARTESIAN_POINT('Ctrl Pts',(7.74074988192156,17.8165392927236,-337.367641257893)) ;
#47705 = CARTESIAN_POINT('Ctrl Pts',(7.8624421385309,17.7631721485228,-337.369263243321)) ;
#47706 = CARTESIAN_POINT('Ctrl Pts',(8.1795219363518,17.6202225803425,-337.373486617498)) ;
#47707 = CARTESIAN_POINT('Ctrl Pts',(8.3739870365675,17.5286384015881,-337.376073825126)) ;
#47708 = CARTESIAN_POINT('Ctrl Pts',(8.69636839493244,17.3702220413318,-337.380365228753)) ;
#47709 = CARTESIAN_POINT('Ctrl Pts',(8.82513170059193,17.3051578307364,-337.382079966096)) ;
#47710 = CARTESIAN_POINT('Ctrl Pts',(9.36618704376962,17.024152655507,-337.389296405992)) ;
#47711 = CARTESIAN_POINT('Ctrl Pts',(9.77137318787817,16.7948652796383,-337.394724590126)) ;
#47712 = CARTESIAN_POINT('Ctrl Pts',(10.2506937447463,16.5004041543493,-337.401296060926)) ;
#47713 = CARTESIAN_POINT('Ctrl Pts',(10.3330728971278,16.4489411210363,-337.402431181123)) ;
#47714 = CARTESIAN_POINT('Ctrl Pts',(10.4970816763267,16.3447649892405,-337.40470492403)) ;
#47715 = CARTESIAN_POINT('Ctrl Pts',(10.5787087060405,16.2920529208536,-337.405843515871)) ;
#47716 = CARTESIAN_POINT('Ctrl Pts',(10.9158725803599,16.0707212380225,-337.410580805371)) ;
#47717 = CARTESIAN_POINT('Ctrl Pts',(11.1678002286557,15.8966849562444,-337.414202277922)) ;
#47718 = CARTESIAN_POINT('Ctrl Pts',(11.4946003574772,15.6593212896827,-337.41906970904)) ;
#47719 = CARTESIAN_POINT('Ctrl Pts',(11.5732574072799,15.6012785879781,-337.420254641382)) ;
#47720 = CARTESIAN_POINT('Ctrl Pts',(11.7045901431073,15.5028256000307,-337.422258507024)) ;
#47721 = CARTESIAN_POINT('Ctrl Pts',(11.7575028574325,15.4627345113222,-337.423072925929)) ;
#47722 = CARTESIAN_POINT('Ctrl Pts',(11.8733950277655,15.3739861211554,-337.42487304485)) ;
#47723 = CARTESIAN_POINT('Ctrl Pts',(11.9362829281707,15.325211534463,-337.425860370187)) ;
#47724 = CARTESIAN_POINT('Ctrl Pts',(12.1332173947047,15.1705255638806,-337.428982981354)) ;
#47725 = CARTESIAN_POINT('Ctrl Pts',(12.2661674205437,15.0632316214504,-337.431136296907)) ;
#47726 = CARTESIAN_POINT('Ctrl Pts',(12.8050036585797,14.6165128023483,-337.440021943715)) ;
#47727 = CARTESIAN_POINT('Ctrl Pts',(13.198355784914,14.2623269309345,-337.446877316693)) ;
#47728 = CARTESIAN_POINT('Ctrl Pts',(13.9648139426531,13.5132899410866,-337.460690061848)) ;
#47729 = CARTESIAN_POINT('Ctrl Pts',(14.3368116993991,13.1179597125527,-337.467638608945)) ;
#47730 = CARTESIAN_POINT('Ctrl Pts',(14.7939145599327,12.5894835434343,-337.476407665366)) ;
#47731 = CARTESIAN_POINT('Ctrl Pts',(14.8946301218606,12.4701642940459,-337.47835597195)) ;
#47732 = CARTESIAN_POINT('Ctrl Pts',(15.074408188939,12.2518929203845,-337.481862923775)) ;
#47733 = CARTESIAN_POINT('Ctrl Pts',(15.1539623131608,12.1533570934209,-337.48342557294)) ;
#47734 = CARTESIAN_POINT('Ctrl Pts',(15.3144572905008,11.9505416693763,-337.486600761112)) ;
#47735 = CARTESIAN_POINT('Ctrl Pts',(15.3953102058076,11.8462007418484,-337.488212528314)) ;
#47736 = CARTESIAN_POINT('Ctrl Pts',(15.6021035715943,11.5736400806449,-337.492368320408)) ;
#47737 = CARTESIAN_POINT('Ctrl Pts',(15.726389120725,11.4041863366053,-337.494899045294)) ;
#47738 = CARTESIAN_POINT('Ctrl Pts',(15.9286325223914,11.1188480541375,-337.499080127157)) ;
#47739 = CARTESIAN_POINT('Ctrl Pts',(16.0081337859861,11.0040796445726,-337.500740824433)) ;
#47740 = CARTESIAN_POINT('Ctrl Pts',(16.3331325634966,10.5239331943914,-337.507609150096)) ;
#47741 = CARTESIAN_POINT('Ctrl Pts',(16.5674121801883,10.1511202984857,-337.512750377675)) ;
#47742 = CARTESIAN_POINT('Ctrl Pts',(16.853072742282,9.66027327562971,-337.519383277446)) ;
#47743 = CARTESIAN_POINT('Ctrl Pts',(16.9162310729595,9.54924431010841,-337.520875193007)) ;
#47744 = CARTESIAN_POINT('Ctrl Pts',(17.0230269867075,9.35711793672063,-337.523446932676)) ;
#47745 = CARTESIAN_POINT('Ctrl Pts',(17.0671914236388,9.27631827682224,-337.524525523965)) ;
#47746 = CARTESIAN_POINT('Ctrl Pts',(17.2610199150946,8.91563511160627,-337.529331919052)) ;
#47747 = CARTESIAN_POINT('Ctrl Pts',(17.4043854383439,8.63242287166826,-337.533082992207)) ;
#47748 = CARTESIAN_POINT('Ctrl Pts',(17.5831957620059,8.25661027154145,-337.53809699867)) ;
#47749 = CARTESIAN_POINT('Ctrl Pts',(17.6249631048044,8.16707180681088,-337.539294333569)) ;
#47750 = CARTESIAN_POINT('Ctrl Pts',(17.6937042573408,8.01672496429396,-337.541312228957)) ;
#47751 = CARTESIAN_POINT('Ctrl Pts',(17.7210520972795,7.95608962197797,-337.542128113579)) ;
#47752 = CARTESIAN_POINT('Ctrl Pts',(17.7802073843699,7.82311288135791,-337.543922645513)) ;
#47753 = CARTESIAN_POINT('Ctrl Pts',(17.8118858492631,7.75071559647389,-337.544902823159)) ;
#47754 = CARTESIAN_POINT('Ctrl Pts',(17.9093048273225,7.52432462206485,-337.547975404492)) ;
#47755 = CARTESIAN_POINT('Ctrl Pts',(17.9734965838463,7.36967304658117,-337.550085060593)) ;
#47756 = CARTESIAN_POINT('Ctrl Pts',(18.085387465715,7.08994347194395,-337.553908160173)) ;
#47757 = CARTESIAN_POINT('Ctrl Pts',(18.133808447491,6.9651654221299,-337.555616078197)) ;
#47758 = CARTESIAN_POINT('Ctrl Pts',(18.389625055928,6.28518656532974,-337.564920679992)) ;
#47759 = CARTESIAN_POINT('Ctrl Pts',(18.57281810745,5.72121569961133,-337.572617637987)) ;
#47760 = CARTESIAN_POINT('Ctrl Pts',(18.8307872349467,4.7829675983396,-337.585085442069)) ;
#47761 = CARTESIAN_POINT('Ctrl Pts',(18.9208384729872,4.41329803828753,-337.589916870298)) ;
#47762 = CARTESIAN_POINT('Ctrl Pts',(19.0331797067387,3.88512102122246,-337.596678763912)) ;
#47763 = CARTESIAN_POINT('Ctrl Pts',(19.0644569198124,3.72861603666048,-337.59866529174)) ;
#47764 = CARTESIAN_POINT('Ctrl Pts',(19.1167065649677,3.44930022317928,-337.602180030141)) ;
#47765 = CARTESIAN_POINT('Ctrl Pts',(19.1384328238181,3.32663959816111,-337.603713073483)) ;
#47766 = CARTESIAN_POINT('Ctrl Pts',(19.1823460880826,3.0640330293644,-337.606973445629)) ;
#47767 = CARTESIAN_POINT('Ctrl Pts',(19.2041847784371,2.92403606526248,-337.608698414885)) ;
#47768 = CARTESIAN_POINT('Ctrl Pts',(19.2624764725422,2.52148451402979,-337.613623062732)) ;
#47769 = CARTESIAN_POINT('Ctrl Pts',(19.2950896924794,2.25840610683482,-337.616798053456)) ;
#47770 = CARTESIAN_POINT('Ctrl Pts',(19.3856405529217,1.38127449765102,-337.627271882569)) ;
#47771 = CARTESIAN_POINT('Ctrl Pts',(19.4197204569346,0.765137940033008,-337.634436772549)) ;
#47772 = CARTESIAN_POINT('Ctrl Pts',(19.4250288628456,0.0704377258478807,
-337.642566019914)) ;
#47773 = CARTESIAN_POINT('Ctrl Pts',(19.4251551013299,-0.00755514414413087,
-337.643479601952)) ;
#47774 = CARTESIAN_POINT('Ctrl Pts',(19.423378799504,-0.410894534108805,-337.648212343182)) ;
#47775 = CARTESIAN_POINT('Ctrl Pts',(19.4137722757462,-0.736154497479361,
-337.652055527468)) ;
#47776 = CARTESIAN_POINT('Ctrl Pts',(19.3905843014776,-1.16004341642344,-337.657169549116)) ;
#47777 = CARTESIAN_POINT('Ctrl Pts',(19.3844090824792,-1.2590253236515,-337.658371313284)) ;
#47778 = CARTESIAN_POINT('Ctrl Pts',(19.3728216180188,-1.42437376003337,-337.660394431619)) ;
#47779 = CARTESIAN_POINT('Ctrl Pts',(19.3678256397745,-1.49076760344238,-337.66121105553)) ;
#47780 = CARTESIAN_POINT('Ctrl Pts',(19.3561650874913,-1.63576297692322,-337.663004535752)) ;
#47781 = CARTESIAN_POINT('Ctrl Pts',(19.3493628925497,-1.71435207654343,-337.663982894112)) ;
#47782 = CARTESIAN_POINT('Ctrl Pts',(19.3267137023345,-1.9586953823791,-337.667041913255)) ;
#47783 = CARTESIAN_POINT('Ctrl Pts',(19.3092140658688,-2.12428861987821,-337.669139607738)) ;
#47784 = CARTESIAN_POINT('Ctrl Pts',(19.2739436468233,-2.42143271303208,-337.672936202221)) ;
#47785 = CARTESIAN_POINT('Ctrl Pts',(19.2569493122032,-2.55306545557215,-337.674629568155)) ;
#47786 = CARTESIAN_POINT('Ctrl Pts',(19.158147945621,-3.26112695382692,-337.683784288383)) ;
#47787 = CARTESIAN_POINT('Ctrl Pts',(19.0518061448702,-3.83383173886034,-337.691343720935)) ;
#47788 = CARTESIAN_POINT('Ctrl Pts',(18.8710604105343,-4.61087650934077,-337.701570707971)) ;
#47789 = CARTESIAN_POINT('Ctrl Pts',(18.8187247777371,-4.82003123637859,-337.704321703155)) ;
#47790 = CARTESIAN_POINT('Ctrl Pts',(18.699415622909,-5.26523152325532,-337.710163781735)) ;
#47791 = CARTESIAN_POINT('Ctrl Pts',(18.6314294828479,-5.5009674961467,-337.713248835298)) ;
#47792 = CARTESIAN_POINT('Ctrl Pts',(18.5177961075829,-5.86867311400223,-337.71804331602)) ;
#47793 = CARTESIAN_POINT('Ctrl Pts',(18.4751602237666,-6.00154576531985,-337.71977224667)) ;
#47794 = CARTESIAN_POINT('Ctrl Pts',(18.3916264722974,-6.2525454030299,-337.723031577909)) ;
#47795 = CARTESIAN_POINT('Ctrl Pts',(18.3510127988556,-6.37075957928543,-337.724563813404)) ;
#47796 = CARTESIAN_POINT('Ctrl Pts',(18.2536965123682,-6.645363736268,-337.728117337735)) ;
#47797 = CARTESIAN_POINT('Ctrl Pts',(18.1961203046822,-6.80143378384901,-337.7301325414)) ;
#47798 = CARTESIAN_POINT('Ctrl Pts',(17.9656966456587,-7.40215859360995,-337.737878292566)) ;
#47799 = CARTESIAN_POINT('Ctrl Pts',(17.7784962285236,-7.84112753817686,-337.743510764866)) ;
#47800 = CARTESIAN_POINT('Ctrl Pts',(17.3953448438544,-8.65512564404414,-337.754049919798)) ;
#47801 = CARTESIAN_POINT('Ctrl Pts',(17.2029338957534,-9.03151632359954,-337.758964239384)) ;
#47802 = CARTESIAN_POINT('Ctrl Pts',(16.8465190735595,-9.67594443290407,-337.767610170652)) ;
#47803 = CARTESIAN_POINT('Ctrl Pts',(16.688005909082,-9.94683686084418,-337.771320054849)) ;
#47804 = CARTESIAN_POINT('Ctrl Pts',(16.4712252339049,-10.2975269018185,-337.776287484352)) ;
#47805 = CARTESIAN_POINT('Ctrl Pts',(16.4188140152371,-10.3808895233145,-337.777480888215)) ;
#47806 = CARTESIAN_POINT('Ctrl Pts',(16.3299831404541,-10.5198236429627,-337.779493866971)) ;
#47807 = CARTESIAN_POINT('Ctrl Pts',(16.2939081144171,-10.5756133256486,-337.780308809749)) ;
#47808 = CARTESIAN_POINT('Ctrl Pts',(16.2142944310176,-10.6973607463315,-337.782102523974)) ;
#47809 = CARTESIAN_POINT('Ctrl Pts',(16.1706381198371,-10.7632399215596,-337.783082839436)) ;
#47810 = CARTESIAN_POINT('Ctrl Pts',(16.0329876166242,-10.9682323107964,-337.786161332381)) ;
#47811 = CARTESIAN_POINT('Ctrl Pts',(15.9375912427134,-11.1063944268197,-337.788276904272)) ;
#47812 = CARTESIAN_POINT('Ctrl Pts',(15.5341777262881,-11.6747539505318,-337.79712238335)) ;
#47813 = CARTESIAN_POINT('Ctrl Pts',(15.2104400300485,-12.0935136001958,-337.803977800465)) ;
#47814 = CARTESIAN_POINT('Ctrl Pts',(14.5158755752377,-12.9198651109586,-337.817894000775)) ;
#47815 = CARTESIAN_POINT('Ctrl Pts',(14.143990343901,-13.3259558286898,-337.824944474059)) ;
#47816 = CARTESIAN_POINT('Ctrl Pts',(13.6455313489594,-13.8258560376481,-337.833803399733)) ;
#47817 = CARTESIAN_POINT('Ctrl Pts',(13.5343802059128,-13.9346823968351,-337.835744256679)) ;
#47818 = CARTESIAN_POINT('Ctrl Pts',(13.3305276830712,-14.1295309583979,-337.839241357412)) ;
#47819 = CARTESIAN_POINT('Ctrl Pts',(13.2382705233153,-14.2160053114218,-337.840801544594)) ;
#47820 = CARTESIAN_POINT('Ctrl Pts',(13.0655495863411,-14.3747603711127,-337.843681483417)) ;
#47821 = CARTESIAN_POINT('Ctrl Pts',(12.9853137199658,-14.4472817285672,-337.845003317439)) ;
#47822 = CARTESIAN_POINT('Ctrl Pts',(12.7792615853497,-14.6304190811857,-337.848358120345)) ;
#47823 = CARTESIAN_POINT('Ctrl Pts',(12.652612293352,-14.7400845119042,-337.850382936227)) ;
#47824 = CARTESIAN_POINT('Ctrl Pts',(12.3654495801427,-14.9823099252617,-337.854895579216)) ;
#47825 = CARTESIAN_POINT('Ctrl Pts',(12.2041917960066,-15.1139556963398,-337.857376236079)) ;
#47826 = CARTESIAN_POINT('Ctrl Pts',(11.6914709470792,-15.5189678843399,-337.865115078004)) ;
#47827 = CARTESIAN_POINT('Ctrl Pts',(11.3327070999895,-15.7828580212535,-337.870313771805)) ;
#47828 = CARTESIAN_POINT('Ctrl Pts',(10.5614813047907,-16.3102711070265,-337.881226384946)) ;
#47829 = CARTESIAN_POINT('Ctrl Pts',(10.1474871481526,-16.5710088104313,-337.886936250085)) ;
#47830 = CARTESIAN_POINT('Ctrl Pts',(9.62105156827939,-16.8754306810581,-337.894229141809)) ;
#47831 = CARTESIAN_POINT('Ctrl Pts',(9.51746124238996,-16.9340699593464,-337.895665975063)) ;
#47832 = CARTESIAN_POINT('Ctrl Pts',(9.35810298882791,-17.0223535623432,-337.89788351065)) ;
#47833 = CARTESIAN_POINT('Ctrl Pts',(9.30271850351345,-17.0526842691746,-337.898655525394)) ;
#47834 = CARTESIAN_POINT('Ctrl Pts',(9.18879212812195,-17.1143546011128,-337.900247202577)) ;
#47835 = CARTESIAN_POINT('Ctrl Pts',(9.13023547909524,-17.1456651740403,-337.901067298396)) ;
#47836 = CARTESIAN_POINT('Ctrl Pts',(9.06606251051121,-17.17955685227,-337.901967734198)) ;
#47837 = CARTESIAN_POINT('Ctrl Pts',(9.06060413306961,-17.1824362599913,-337.902044336065)) ;
#47838 = CARTESIAN_POINT('Ctrl Pts',(9.04958456724378,-17.188242599348,-337.902199008658)) ;
#47839 = CARTESIAN_POINT('Ctrl Pts',(9.04402332873731,-17.1911694344214,-337.902277080563)) ;
#47840 = CARTESIAN_POINT('Ctrl Pts',(9.03267677446241,-17.1971340049961,-337.902436396597)) ;
#47841 = CARTESIAN_POINT('Ctrl Pts',(9.02689134429441,-17.2001715211215,-337.902517643385)) ;
#47842 = CARTESIAN_POINT('Ctrl Pts',(9.01497191707914,-17.2064218907538,-337.902685060046)) ;
#47843 = CARTESIAN_POINT('Ctrl Pts',(9.00883773257188,-17.2096343847425,-337.902771234227)) ;
#47844 = CARTESIAN_POINT('Ctrl Pts',(8.99608488712258,-17.2163044078818,-337.902950419322)) ;
#47845 = CARTESIAN_POINT('Ctrl Pts',(8.98946594761668,-17.2197614018833,-337.903043436559)) ;
#47846 = CARTESIAN_POINT('Ctrl Pts',(8.97558855136614,-17.2269992203051,-337.903238492989)) ;
#47847 = CARTESIAN_POINT('Ctrl Pts',(8.96832969536919,-17.2307792759047,-337.903340541123)) ;
#47848 = CARTESIAN_POINT('Ctrl Pts',(8.9589461933142,-17.2356582069534,-337.903472483073)) ;
#47849 = CARTESIAN_POINT('Ctrl Pts',(8.95682372965082,-17.2367612792422,-337.903502328782)) ;
#47850 = CARTESIAN_POINT('Ctrl Pts',(8.95196222830745,-17.2392867250484,-337.903570694032)) ;
#47851 = CARTESIAN_POINT('Ctrl Pts',(8.9492230553523,-17.2407088378356,-337.903609216545)) ;
#47852 = CARTESIAN_POINT('Ctrl Pts',(8.94289952007592,-17.2439899523679,-337.90369815401)) ;
#47853 = CARTESIAN_POINT('Ctrl Pts',(8.93931491686858,-17.2458484894362,-337.903748574223)) ;
#47854 = CARTESIAN_POINT('Ctrl Pts',(8.93096187477265,-17.2501760520133,-337.90386607647)) ;
#47855 = CARTESIAN_POINT('Ctrl Pts',(8.92619299117249,-17.2526442181607,-337.903933168145)) ;
#47856 = CARTESIAN_POINT('Ctrl Pts',(8.91495806009663,-17.2584530232681,-337.904091246069)) ;
#47857 = CARTESIAN_POINT('Ctrl Pts',(8.90849115757613,-17.2617920061912,-337.904182250673)) ;
#47858 = CARTESIAN_POINT('Ctrl Pts',(8.80826529037772,-17.3134691757035,-337.905592871701)) ;
#47859 = CARTESIAN_POINT('Ctrl Pts',(8.7141160559612,-17.3610464444985,-337.906920752603)) ;
#47860 = CARTESIAN_POINT('Ctrl Pts',(8.43574439803903,-17.4988835292732,-337.910850172303)) ;
#47861 = CARTESIAN_POINT('Ctrl Pts',(8.25047444042984,-17.5869946166852,-337.913469461293)) ;
#47862 = CARTESIAN_POINT('Ctrl Pts',(7.33160715050241,-18.0062758340354,-337.926426155621)) ;
#47863 = CARTESIAN_POINT('Ctrl Pts',(6.57930689612149,-18.2945665075286,-337.93689276559)) ;
#47864 = CARTESIAN_POINT('Ctrl Pts',(5.60189958709704,-18.6010081373859,-337.949832343576)) ;
#47865 = CARTESIAN_POINT('Ctrl Pts',(5.39140373704929,-18.6631066197335,-337.952584002111)) ;
#47866 = CARTESIAN_POINT('Ctrl Pts',(5.05086177376709,-18.7573277964724,-337.9569769935)) ;
#47867 = CARTESIAN_POINT('Ctrl Pts',(4.9214570522249,-18.7916952738028,-337.958632868949)) ;
#47868 = CARTESIAN_POINT('Ctrl Pts',(4.67692817944004,-18.8539384648727,-337.961736862916)) ;
#47869 = CARTESIAN_POINT('Ctrl Pts',(4.56188419248772,-18.882104371263,-337.963186848473)) ;
#47870 = CARTESIAN_POINT('Ctrl Pts',(4.32476558709997,-18.9378639085973,-337.966154868259)) ;
#47871 = CARTESIAN_POINT('Ctrl Pts',(4.20266735727822,-18.9653334780393,-337.967672033542)) ;
#47872 = CARTESIAN_POINT('Ctrl Pts',(3.90121292933478,-19.0301003635033,-337.971392103434)) ;
#47873 = CARTESIAN_POINT('Ctrl Pts',(3.72157823831249,-19.0660441021907,-337.973586477635)) ;
#47874 = CARTESIAN_POINT('Ctrl Pts',(2.87644088366972,-19.2227513923221,-337.983820717492)) ;
#47875 = CARTESIAN_POINT('Ctrl Pts',(2.20543290841547,-19.3112440804199,-337.991668592314)) ;
#47876 = CARTESIAN_POINT('Ctrl Pts',(1.53118156877294,-19.3645580379065,-337.999588035935)) ;
#47877 = CARTESIAN_POINT('',(16.0043568677506,-11.0086868540114,-338.)) ;
#47878 = CARTESIAN_POINT('Origin',(0.,0.,-338.)) ;
#47879 = CARTESIAN_POINT('Ctrl Pts',(16.0043568677512,-11.0086868540105,-338.)) ;
#47880 = CARTESIAN_POINT('Ctrl Pts',(16.2343017349983,-10.6743945115965,-337.995013456726)) ;
#47881 = CARTESIAN_POINT('Ctrl Pts',(16.4537823394767,-10.3328760929934,-337.990026913451)) ;
#47882 = CARTESIAN_POINT('Ctrl Pts',(16.6623602288354,-9.98480728930328,-337.985040370177)) ;
#47883 = CARTESIAN_POINT('Ctrl Pts',(16.8709240018669,-9.63676204253544,-337.980054164386)) ;
#47884 = CARTESIAN_POINT('Ctrl Pts',(17.0685864148693,-9.2821674950807,-337.975067958596)) ;
#47885 = CARTESIAN_POINT('Ctrl Pts',(17.2549536395104,-8.92172628465741,-337.970081752805)) ;
#47886 = CARTESIAN_POINT('Ctrl Pts',(17.4413144679775,-8.56129744467485,-337.965095718143)) ;
#47887 = CARTESIAN_POINT('Ctrl Pts',(17.6163807764168,-8.19502254852781,-337.96010968348)) ;
#47888 = CARTESIAN_POINT('Ctrl Pts',(17.7798050182231,-7.82362821930908,-337.955123648818)) ;
#47889 = CARTESIAN_POINT('Ctrl Pts',(17.9432291025103,-7.45223424806482,-337.950137618961)) ;
#47890 = CARTESIAN_POINT('Ctrl Pts',(18.0950110498037,-7.075721065873,-337.945151589104)) ;
#47891 = CARTESIAN_POINT('Ctrl Pts',(18.2348510554591,-6.69483621795347,-337.940165559248)) ;
#47892 = CARTESIAN_POINT('Ctrl Pts',(18.3747130970232,-6.3138913504159,-337.935178743695)) ;
#47893 = CARTESIAN_POINT('Ctrl Pts',(18.5026293537671,-5.92857365703956,-337.930191928143)) ;
#47894 = CARTESIAN_POINT('Ctrl Pts',(18.6183489284098,-5.53964874157018,-337.92520511259)) ;
#47895 = CARTESIAN_POINT('Ctrl Pts',(18.7340719628011,-5.15071219814223,-337.920218147944)) ;
#47896 = CARTESIAN_POINT('Ctrl Pts',(18.8375975227664,-4.7581684399421,-337.915231183297)) ;
#47897 = CARTESIAN_POINT('Ctrl Pts',(18.9287248027228,-4.36279753630466,-337.91024421865)) ;
#47898 = CARTESIAN_POINT('Ctrl Pts',(19.0198727933892,-3.96733677579774,-337.905256120604)) ;
#47899 = CARTESIAN_POINT('Ctrl Pts',(19.0986168186598,-3.56904781118808,-337.900268022559)) ;
#47900 = CARTESIAN_POINT('Ctrl Pts',(19.1648069165423,-3.16872227430096,-337.895279924513)) ;
#47901 = CARTESIAN_POINT('Ctrl Pts',(19.2283855015679,-2.78419147590161,-337.89048863056)) ;
#47902 = CARTESIAN_POINT('Ctrl Pts',(19.2803815197814,-2.39778188479241,-337.885697336607)) ;
#47903 = CARTESIAN_POINT('Ctrl Pts',(19.3207068719133,-2.01020172360925,-337.880906042654)) ;
#47904 = CARTESIAN_POINT('Ctrl Pts',(19.362471040198,-1.60879262933786,-337.875943794431)) ;
#47905 = CARTESIAN_POINT('Ctrl Pts',(19.3917280541838,-1.20601620829655,-337.870981546209)) ;
#47906 = CARTESIAN_POINT('Ctrl Pts',(19.4084091842075,-0.802669258394608,
-337.866019297986)) ;
#47907 = CARTESIAN_POINT('Ctrl Pts',(19.4250365960367,-0.400621205500163,
-337.861073029677)) ;
#47908 = CARTESIAN_POINT('Ctrl Pts',(19.4291689995692,0.00199346573810244,
-337.856126761368)) ;
#47909 = CARTESIAN_POINT('Ctrl Pts',(19.4207904046784,0.40438231607356,-337.851180493058)) ;
#47910 = CARTESIAN_POINT('Ctrl Pts',(19.412412909012,0.806718375258068,-337.846234873672)) ;
#47911 = CARTESIAN_POINT('Ctrl Pts',(19.3915276979543,1.20882843310241,-337.841289254285)) ;
#47912 = CARTESIAN_POINT('Ctrl Pts',(19.3581708977425,1.60992064829172,-337.836343634898)) ;
#47913 = CARTESIAN_POINT('Ctrl Pts',(19.3248167459013,2.01098101867452,-337.83139840817)) ;
#47914 = CARTESIAN_POINT('Ctrl Pts',(19.278993002637,2.41102346896342,-337.826453181442)) ;
#47915 = CARTESIAN_POINT('Ctrl Pts',(19.2207877568638,2.80926022390157,-337.821507954714)) ;
#47916 = CARTESIAN_POINT('Ctrl Pts',(19.1622361315391,3.20986688668423,-337.81653329893)) ;
#47917 = CARTESIAN_POINT('Ctrl Pts',(19.0911551833977,3.60864604900755,-337.811558643146)) ;
#47918 = CARTESIAN_POINT('Ctrl Pts',(19.0076872531245,4.00480340184232,-337.806583987363)) ;
#47919 = CARTESIAN_POINT('Ctrl Pts',(18.9247063336755,4.39864929303818,-337.801638357232)) ;
#47920 = CARTESIAN_POINT('Ctrl Pts',(18.8294826609021,4.78990365494282,-337.796692727102)) ;
#47921 = CARTESIAN_POINT('Ctrl Pts',(18.7222072098571,5.17779704036152,-337.791747096972)) ;
#47922 = CARTESIAN_POINT('Ctrl Pts',(18.6139873675078,5.56910521580501,-337.786757928361)) ;
#47923 = CARTESIAN_POINT('Ctrl Pts',(18.4935026142637,5.95699271935316,-337.781768759751)) ;
#47924 = CARTESIAN_POINT('Ctrl Pts',(18.3610006351633,6.34068455890482,-337.77677959114)) ;
#47925 = CARTESIAN_POINT('Ctrl Pts',(18.2284986560629,6.72437639845648,-337.77179042253)) ;
#47926 = CARTESIAN_POINT('Ctrl Pts',(18.0839795396159,7.10387233988891,-337.766801253919)) ;
#47927 = CARTESIAN_POINT('Ctrl Pts',(17.9277416233235,7.47841596110801,-337.761812085309)) ;
#47928 = CARTESIAN_POINT('Ctrl Pts',(17.7722615228434,7.85114289732963,-337.756847116143)) ;
#47929 = CARTESIAN_POINT('Ctrl Pts',(17.6051348821206,8.21906435576997,-337.751882146978)) ;
#47930 = CARTESIAN_POINT('Ctrl Pts',(17.426684576462,8.58145032453731,-337.746917177812)) ;
#47931 = CARTESIAN_POINT('Ctrl Pts',(17.248259600405,8.94378485549855,-337.741952913385)) ;
#47932 = CARTESIAN_POINT('Ctrl Pts',(17.0585142738589,9.30058525420489,-337.736988648957)) ;
#47933 = CARTESIAN_POINT('Ctrl Pts',(16.8578184523581,9.6511440786745,-337.73202438453)) ;
#47934 = CARTESIAN_POINT('Ctrl Pts',(16.6571422865929,10.0016685701346,-337.727060606292)) ;
#47935 = CARTESIAN_POINT('Ctrl Pts',(16.4455178853756,10.3459525034175,-337.722096828054)) ;
#47936 = CARTESIAN_POINT('Ctrl Pts',(16.2233604970649,10.6833140542752,-337.717133049817)) ;
#47937 = CARTESIAN_POINT('Ctrl Pts',(16.0012150938113,11.0206574049845,-337.712169539367)) ;
#47938 = CARTESIAN_POINT('Ctrl Pts',(15.7685379686291,11.3510789221508,-337.707206028918)) ;
#47939 = CARTESIAN_POINT('Ctrl Pts',(15.5257879761034,11.67392533474,-337.702242518468)) ;
#47940 = CARTESIAN_POINT('Ctrl Pts',(15.2830131018267,11.9968048389226,-337.697278499262)) ;
#47941 = CARTESIAN_POINT('Ctrl Pts',(15.030163436591,12.3121074963065,-337.692314480055)) ;
#47942 = CARTESIAN_POINT('Ctrl Pts',(14.7677396345522,12.6192111911195,-337.687350460849)) ;
#47943 = CARTESIAN_POINT('Ctrl Pts',(14.5053145445756,12.9263163931527,-337.682386417279)) ;
#47944 = CARTESIAN_POINT('Ctrl Pts',(14.2333153789608,13.2252223739513,-337.67742237371)) ;
#47945 = CARTESIAN_POINT('Ctrl Pts',(13.9522822298859,13.515341119543,-337.672458330141)) ;
#47946 = CARTESIAN_POINT('Ctrl Pts',(13.6711888550596,13.8055220379407,-337.667493222771)) ;
#47947 = CARTESIAN_POINT('Ctrl Pts',(13.3810577905449,14.0869117864317,-337.662528115401)) ;
#47948 = CARTESIAN_POINT('Ctrl Pts',(13.082466514253,14.358958698438,-337.657563008031)) ;
#47949 = CARTESIAN_POINT('Ctrl Pts',(12.7848863979647,14.6300843412099,-337.652614714675)) ;
#47950 = CARTESIAN_POINT('Ctrl Pts',(12.4789034688143,14.8919301874873,-337.647666421319)) ;
#47951 = CARTESIAN_POINT('Ctrl Pts',(12.1651233976083,15.143988831248,-337.642718127963)) ;
#47952 = CARTESIAN_POINT('Ctrl Pts',(11.850458423498,15.3967583150089,-337.637755879741)) ;
#47953 = CARTESIAN_POINT('Ctrl Pts',(11.5278693550387,15.6397518520347,-337.632793631518)) ;
#47954 = CARTESIAN_POINT('Ctrl Pts',(11.1979882450328,15.8724819818486,-337.627831383295)) ;
#47955 = CARTESIAN_POINT('Ctrl Pts',(10.8685001565858,16.1049348361361,-337.622875047113)) ;
#47956 = CARTESIAN_POINT('Ctrl Pts',(10.531737588431,16.3271485899504,-337.617918710931)) ;
#47957 = CARTESIAN_POINT('Ctrl Pts',(10.188361177574,16.5386795577913,-337.612962374749)) ;
#47958 = CARTESIAN_POINT('Ctrl Pts',(9.84502269901286,16.7501871581119,-337.608006586086)) ;
#47959 = CARTESIAN_POINT('Ctrl Pts',(9.49507203939322,16.9510142048205,-337.603050797424)) ;
#47960 = CARTESIAN_POINT('Ctrl Pts',(9.1391974995517,17.1407611868373,-337.598095008761)) ;
#47961 = CARTESIAN_POINT('Ctrl Pts',(8.7833453758918,17.3304962168814,-337.593139532258)) ;
#47962 = CARTESIAN_POINT('Ctrl Pts',(8.42157032719244,17.5091524646376,-337.588184055756)) ;
#47963 = CARTESIAN_POINT('Ctrl Pts',(8.05458533401213,17.6763763282274,-337.583228579253)) ;
#47964 = CARTESIAN_POINT('Ctrl Pts',(7.68674442969674,17.843990204405,-337.5782615452)) ;
#47965 = CARTESIAN_POINT('Ctrl Pts',(7.31366946010517,18.0001181892563,-337.573294511147)) ;
#47966 = CARTESIAN_POINT('Ctrl Pts',(6.93610020148422,18.1444520169381,-337.568327477094)) ;
#47967 = CARTESIAN_POINT('Ctrl Pts',(6.55937125107006,18.2884646190511,-337.563371497542)) ;
#47968 = CARTESIAN_POINT('Ctrl Pts',(6.17816822458658,18.4207354381156,-337.558415517989)) ;
#47969 = CARTESIAN_POINT('Ctrl Pts',(5.79324431870531,18.5410071264694,-337.553459538437)) ;
#47970 = CARTESIAN_POINT('Ctrl Pts',(5.40703253177549,18.6616812206643,-337.548486977134)) ;
#47971 = CARTESIAN_POINT('Ctrl Pts',(5.01707514759405,18.7702756607823,-337.543514415831)) ;
#47972 = CARTESIAN_POINT('Ctrl Pts',(4.62414806207482,18.8665810283689,-337.538541854528)) ;
#47973 = CARTESIAN_POINT('Ctrl Pts',(4.23122097655567,18.9628863959555,-337.533569293225)) ;
#47974 = CARTESIAN_POINT('Ctrl Pts',(3.83532442586498,19.0469026401326,-337.528596731922)) ;
#47975 = CARTESIAN_POINT('Ctrl Pts',(3.43724593561117,19.1184718368944,-337.523624170618)) ;
#47976 = CARTESIAN_POINT('Ctrl Pts',(3.03999305919983,19.1898925993122,-337.518661922396)) ;
#47977 = CARTESIAN_POINT('Ctrl Pts',(2.64046091834604,19.2489370421643,-337.513699674173)) ;
#47978 = CARTESIAN_POINT('Ctrl Pts',(2.23943738365606,19.2954799164126,-337.50873742595)) ;
#47979 = CARTESIAN_POINT('Ctrl Pts',(1.83867898436969,19.3419920189913,-337.503778458502)) ;
#47980 = CARTESIAN_POINT('Ctrl Pts',(1.43643139837477,19.3760190500696,-337.498819491053)) ;
#47981 = CARTESIAN_POINT('Ctrl Pts',(1.03348786716827,19.3974876679537,-337.493860523605)) ;
#47982 = CARTESIAN_POINT('Ctrl Pts',(0.630587385590106,19.4189539921765,-337.488902085962)) ;
#47983 = CARTESIAN_POINT('Ctrl Pts',(0.226991344155984,19.4278645704372,-337.483943648319)) ;
#47984 = CARTESIAN_POINT('Ctrl Pts',(-0.1765038782194,19.4241980884919,-337.478985210676)) ;
#47985 = CARTESIAN_POINT('Ctrl Pts',(-0.579974687761069,19.4205318283813,
-337.474027073035)) ;
#47986 = CARTESIAN_POINT('Ctrl Pts',(-0.983344453241035,19.4042900304248,
-337.469068935394)) ;
#47987 = CARTESIAN_POINT('Ctrl Pts',(-1.38581710366883,19.3755035019784,-337.464110797754)) ;
#47988 = CARTESIAN_POINT('Ctrl Pts',(-1.78885075407456,19.3466768484657,-337.459145749047)) ;
#47989 = CARTESIAN_POINT('Ctrl Pts',(-2.190984548107,19.3052704731956,-337.45418070034)) ;
#47990 = CARTESIAN_POINT('Ctrl Pts',(-2.59142281899507,19.2513675559216,-337.449215651633)) ;
#47991 = CARTESIAN_POINT('Ctrl Pts',(-2.9913446005162,19.1975341631802,-337.444257006897)) ;
#47992 = CARTESIAN_POINT('Ctrl Pts',(-3.38957499610439,19.1312364889784,-337.439298362161)) ;
#47993 = CARTESIAN_POINT('Ctrl Pts',(-3.78532867959759,19.0526090545997,-337.434339717424)) ;
#47994 = CARTESIAN_POINT('Ctrl Pts',(-4.18184902264361,18.973829302059,-337.429371466732)) ;
#47995 = CARTESIAN_POINT('Ctrl Pts',(-4.57588281161247,18.8826720066114,-337.42440321604)) ;
#47996 = CARTESIAN_POINT('Ctrl Pts',(-4.96665098629062,18.7793238158454,-337.419434965348)) ;
#47997 = CARTESIAN_POINT('Ctrl Pts',(-5.35741916096867,18.6759756250794,-337.414466714656)) ;
#47998 = CARTESIAN_POINT('Ctrl Pts',(-5.74492149171522,18.5604366065672,-337.409498463964)) ;
#47999 = CARTESIAN_POINT('Ctrl Pts',(-6.12839324434191,18.4329439114512,-337.404530213272)) ;
#48000 = CARTESIAN_POINT('Ctrl Pts',(-6.51140169961259,18.3056052486156,-337.399567965049)) ;
#48001 = CARTESIAN_POINT('Ctrl Pts',(-6.89049071154255,18.1663080725525,-337.394605716827)) ;
#48002 = CARTESIAN_POINT('Ctrl Pts',(-7.26490843457078,18.0153193265427,-337.389643468604)) ;
#48003 = CARTESIAN_POINT('Ctrl Pts',(-7.63904959350638,17.8644421085482,-337.384684885752)) ;
#48004 = CARTESIAN_POINT('Ctrl Pts',(-8.00852614156413,17.7018906748922,-337.379726302899)) ;
#48005 = CARTESIAN_POINT('Ctrl Pts',(-8.3726065231162,17.5279800607221,-337.374767720047)) ;
#48006 = CARTESIAN_POINT('Ctrl Pts',(-8.73664794995709,17.3540880540851,-337.369809667737)) ;
#48007 = CARTESIAN_POINT('Ctrl Pts',(-9.0952941493864,17.1688393966988,-337.364851615428)) ;
#48008 = CARTESIAN_POINT('Ctrl Pts',(-9.44783570051987,16.9725963121728,-337.359893563118)) ;
#48009 = CARTESIAN_POINT('Ctrl Pts',(-9.80035592538492,16.7763650989643,-337.354935810736)) ;
#48010 = CARTESIAN_POINT('Ctrl Pts',(-10.1467720323834,16.569140902698,-337.349978058353)) ;
#48011 = CARTESIAN_POINT('Ctrl Pts',(-10.4863998065743,16.3513315695291,-337.345020305971)) ;
#48012 = CARTESIAN_POINT('Ctrl Pts',(-10.8265471948195,16.1331889986239,-337.340054968467)) ;
#48013 = CARTESIAN_POINT('Ctrl Pts',(-11.1598852547188,15.9044289941104,-337.335089630963)) ;
#48014 = CARTESIAN_POINT('Ctrl Pts',(-11.4857549166979,15.6655053858326,-337.330124293459)) ;
#48015 = CARTESIAN_POINT('Ctrl Pts',(-11.8111603124545,15.4269221718106,-337.325166030068)) ;
#48016 = CARTESIAN_POINT('Ctrl Pts',(-12.129118392427,15.1782044459368,-337.320207766676)) ;
#48017 = CARTESIAN_POINT('Ctrl Pts',(-12.4390040007212,14.9198459935095,-337.315249503284)) ;
#48018 = CARTESIAN_POINT('Ctrl Pts',(-12.7495527944879,14.6609346287566,-337.310280628725)) ;
#48019 = CARTESIAN_POINT('Ctrl Pts',(-13.0519943349544,14.3923413713668,-337.305311754165)) ;
#48020 = CARTESIAN_POINT('Ctrl Pts',(-13.3457335522706,14.1146031099638,-337.300342879605)) ;
#48021 = CARTESIAN_POINT('Ctrl Pts',(-13.6394727695868,13.8368648485608,-337.295374005045)) ;
#48022 = CARTESIAN_POINT('Ctrl Pts',(-13.9245094942263,13.5499817525959,-337.290405130486)) ;
#48023 = CARTESIAN_POINT('Ctrl Pts',(-14.2002854317668,13.2545282321307,-337.285436255926)) ;
#48024 = CARTESIAN_POINT('Ctrl Pts',(-14.4756936030728,12.9594687193142,-337.280474007703)) ;
#48025 = CARTESIAN_POINT('Ctrl Pts',(-14.7419390172365,12.6557830606652,-337.275511759481)) ;
#48026 = CARTESIAN_POINT('Ctrl Pts',(-14.9984890994669,12.34406536491,-337.270549511258)) ;
#48027 = CARTESIAN_POINT('Ctrl Pts',(-15.2548349838703,12.0325957769535,-337.265591212675)) ;
#48028 = CARTESIAN_POINT('Ctrl Pts',(-15.5015008131982,11.7131071164413,-337.260632914091)) ;
#48029 = CARTESIAN_POINT('Ctrl Pts',(-15.737994926772,11.3862259192807,-337.255674615508)) ;
#48030 = CARTESIAN_POINT('Ctrl Pts',(-15.9744635701517,11.0593799269182,-337.250716850929)) ;
#48031 = CARTESIAN_POINT('Ctrl Pts',(-16.2007625467101,10.7251431803851,-337.245759086349)) ;
#48032 = CARTESIAN_POINT('Ctrl Pts',(-16.4164422069112,10.3841730661207,-337.24080132177)) ;
#48033 = CARTESIAN_POINT('Ctrl Pts',(-16.6321086950101,10.0432237757631,-337.235843859974)) ;
#48034 = CARTESIAN_POINT('Ctrl Pts',(-16.8371570355162,9.69554213976692,-337.230886398178)) ;
#48035 = CARTESIAN_POINT('Ctrl Pts',(-17.0311815382854,9.34181355037479,-337.225928936382)) ;
#48036 = CARTESIAN_POINT('Ctrl Pts',(-17.2255227194305,8.98750762052518,-337.220963383232)) ;
#48037 = CARTESIAN_POINT('Ctrl Pts',(-17.4088039209296,8.62713518445671,-337.215997830082)) ;
#48038 = CARTESIAN_POINT('Ctrl Pts',(-17.5806634233294,8.26141020623035,-337.211032276932)) ;
#48039 = CARTESIAN_POINT('Ctrl Pts',(-17.7522604231468,7.89624384565332,-337.206074308294)) ;
#48040 = CARTESIAN_POINT('Ctrl Pts',(-17.9124705016481,7.52574150354035,-337.201116339656)) ;
#48041 = CARTESIAN_POINT('Ctrl Pts',(-18.0609809485656,7.15063578820439,-337.196158371019)) ;
#48042 = CARTESIAN_POINT('Ctrl Pts',(-18.2098321739573,6.77466933912253,-337.191189025612)) ;
#48043 = CARTESIAN_POINT('Ctrl Pts',(-18.3469299105402,6.3940785832791,-337.186219680206)) ;
#48044 = CARTESIAN_POINT('Ctrl Pts',(-18.4720083696769,6.00961993728291,-337.1812503348)) ;
#48045 = CARTESIAN_POINT('Ctrl Pts',(-18.5970868288136,5.62516129128671,-337.176280989393)) ;
#48046 = CARTESIAN_POINT('Ctrl Pts',(-18.7101459426383,5.23683498527479,-337.171311643987)) ;
#48047 = CARTESIAN_POINT('Ctrl Pts',(-18.8109701982584,4.84541279977611,-337.166342298581)) ;
#48048 = CARTESIAN_POINT('Ctrl Pts',(-18.9116504573976,4.45454964064387,-337.161380050358)) ;
#48049 = CARTESIAN_POINT('Ctrl Pts',(-19.0001575430551,4.06049559657047,-337.156417802135)) ;
#48050 = CARTESIAN_POINT('Ctrl Pts',(-19.0763080860834,3.66402712937957,-337.151455553913)) ;
#48051 = CARTESIAN_POINT('Ctrl Pts',(-19.1524030914331,3.26784781230418,-337.146496924728)) ;
#48052 = CARTESIAN_POINT('Ctrl Pts',(-19.2161595261519,2.86925782576096,-337.141538295544)) ;
#48053 = CARTESIAN_POINT('Ctrl Pts',(-19.2674454258209,2.46904268148838,-337.13657966636)) ;
#48054 = CARTESIAN_POINT('Ctrl Pts',(-19.3187258345555,2.06887038632536,-337.131621568072)) ;
#48055 = CARTESIAN_POINT('Ctrl Pts',(-19.3575383448397,1.66707351628882,-337.126663469785)) ;
#48056 = CARTESIAN_POINT('Ctrl Pts',(-19.3838026435953,1.26444457140185,-337.121705371497)) ;
#48057 = CARTESIAN_POINT('Ctrl Pts',(-19.410065351173,0.861840019105448,-337.116747573587)) ;
#48058 = CARTESIAN_POINT('Ctrl Pts',(-19.4237813504955,0.458403729426894,
-337.111789775677)) ;
#48059 = CARTESIAN_POINT('Ctrl Pts',(-19.4249223293586,0.054931761158904,
-337.106831977768)) ;
#48060 = CARTESIAN_POINT('Ctrl Pts',(-19.4260650354402,-0.349150984618357,
-337.101866674723)) ;
#48061 = CARTESIAN_POINT('Ctrl Pts',(-19.414594606145,-0.753269278588067,
-337.096901371679)) ;
#48062 = CARTESIAN_POINT('Ctrl Pts',(-19.3905349991719,-1.15662329471983,
-337.091936068635)) ;
#48063 = CARTESIAN_POINT('Ctrl Pts',(-19.3665092900312,-1.55940902115316,
-337.086977761258)) ;
#48064 = CARTESIAN_POINT('Ctrl Pts',(-19.3299298808642,-1.96143238532242,
-337.082019453881)) ;
#48065 = CARTESIAN_POINT('Ctrl Pts',(-19.2808726908508,-2.36190035336035,
-337.077061146504)) ;
#48066 = CARTESIAN_POINT('Ctrl Pts',(-19.2317116787782,-2.76321585076371,
-337.072092345626)) ;
#48067 = CARTESIAN_POINT('Ctrl Pts',(-19.1700200304732,-3.1629691223927,-337.067123544748)) ;
#48068 = CARTESIAN_POINT('Ctrl Pts',(-19.0959261857177,-3.56036909738586,
-337.06215474387)) ;
#48069 = CARTESIAN_POINT('Ctrl Pts',(-19.0218323409622,-3.95776907237912,
-337.057185942992)) ;
#48070 = CARTESIAN_POINT('Ctrl Pts',(-18.9353363501988,-4.35281551644903,
-337.052217142113)) ;
#48071 = CARTESIAN_POINT('Ctrl Pts',(-18.8366181158727,-4.74472791177481,
-337.047248341235)) ;
#48072 = CARTESIAN_POINT('Ctrl Pts',(-18.7380300671962,-5.13612346874673,
-337.042286093013)) ;
#48073 = CARTESIAN_POINT('Ctrl Pts',(-18.6272257920955,-5.52449728803654,
-337.03732384479)) ;
#48074 = CARTESIAN_POINT('Ctrl Pts',(-18.5044157247767,-5.9090797663118,-337.032361596567)) ;
#48075 = CARTESIAN_POINT('Ctrl Pts',(-18.3817005203881,-6.29336517919538,
-337.027403181364)) ;
#48076 = CARTESIAN_POINT('Ctrl Pts',(-18.246998136401,-6.67386487967097,-337.022444766161)) ;
#48077 = CARTESIAN_POINT('Ctrl Pts',(-18.1005684515657,-7.04982600708585,
-337.017486350958)) ;
#48078 = CARTESIAN_POINT('Ctrl Pts',(-17.9541544989108,-7.42574674181475,
-337.01252846848)) ;
#48079 = CARTESIAN_POINT('Ctrl Pts',(-17.7960158480842,-7.79712965630204,
-337.007570586001)) ;
#48080 = CARTESIAN_POINT('Ctrl Pts',(-17.6264610784141,-8.16324046265651,
-337.002612703523)) ;
#48081 = CARTESIAN_POINT('Ctrl Pts',(-17.4569166283541,-8.52932898641299,
-336.997655122796)) ;
#48082 = CARTESIAN_POINT('Ctrl Pts',(-17.2759575472525,-8.89014582773247,
-336.992697542069)) ;
#48083 = CARTESIAN_POINT('Ctrl Pts',(-17.0839397811535,-9.24497845070083,
-336.987739961342)) ;
#48084 = CARTESIAN_POINT('Ctrl Pts',(-16.8916166484252,-9.6003753654231,-336.982774496554)) ;
#48085 = CARTESIAN_POINT('Ctrl Pts',(-16.6881997307688,-9.94976879672292,
-336.977809031767)) ;
#48086 = CARTESIAN_POINT('Ctrl Pts',(-16.474092771076,-10.2924677492807,-336.972843566979)) ;
#48087 = CARTESIAN_POINT('Ctrl Pts',(-16.2603038521978,-10.6346576466718,
-336.96788547804)) ;
#48088 = CARTESIAN_POINT('Ctrl Pts',(-16.0358567651614,-10.9701727451947,
-336.962927389101)) ;
#48089 = CARTESIAN_POINT('Ctrl Pts',(-15.8011975416849,-11.298353032573,-336.957969300161)) ;
#48090 = CARTESIAN_POINT('Ctrl Pts',(-15.566014685756,-11.6272656408298,-336.95300014745)) ;
#48091 = CARTESIAN_POINT('Ctrl Pts',(-15.3205741935904,-11.9488104632796,
-336.948030994738)) ;
#48092 = CARTESIAN_POINT('Ctrl Pts',(-15.0653674490457,-12.2623541224854,
-336.943061842026)) ;
#48093 = CARTESIAN_POINT('Ctrl Pts',(-14.8101607045009,-12.5758977816913,
-336.938092689314)) ;
#48094 = CARTESIAN_POINT('Ctrl Pts',(-14.5451878640831,-12.8814400959192,
-336.933123536602)) ;
#48095 = CARTESIAN_POINT('Ctrl Pts',(-14.2709804714685,-13.1783815919469,
-336.92815438389)) ;
#48096 = CARTESIAN_POINT('Ctrl Pts',(-13.9971540818256,-13.474910496646,-336.923192135668)) ;
#48097 = CARTESIAN_POINT('Ctrl Pts',(-13.7140459973768,-13.7629413078253,
-336.918229887445)) ;
#48098 = CARTESIAN_POINT('Ctrl Pts',(-13.4222092028062,-14.041898914182,-336.913267639222)) ;
#48099 = CARTESIAN_POINT('Ctrl Pts',(-13.1305916962671,-14.3206469100115,
-336.908309119664)) ;
#48100 = CARTESIAN_POINT('Ctrl Pts',(-12.8302587639553,-14.5903351670511,
-336.903350600107)) ;
#48101 = CARTESIAN_POINT('Ctrl Pts',(-12.5217988324315,-14.8504268962248,
-336.898392080549)) ;
#48102 = CARTESIAN_POINT('Ctrl Pts',(-12.2133719893451,-15.1104907254088,
-336.893434092891)) ;
#48103 = CARTESIAN_POINT('Ctrl Pts',(-11.896820069674,-15.3609599298619,-336.888476105232)) ;
#48104 = CARTESIAN_POINT('Ctrl Pts',(-11.5727653789981,-15.6013373299427,
-336.883518117574)) ;
#48105 = CARTESIAN_POINT('Ctrl Pts',(-11.2487303713828,-15.8417001295161,
-336.878560431063)) ;
#48106 = CARTESIAN_POINT('Ctrl Pts',(-10.9171936937525,-16.0719722079235,
-336.873602744553)) ;
#48107 = CARTESIAN_POINT('Ctrl Pts',(-10.5788088385077,-16.2916981483917,
-336.868645058042)) ;
#48108 = CARTESIAN_POINT('Ctrl Pts',(-10.2398984606226,-16.5117653303624,
-336.863679672084)) ;
#48109 = CARTESIAN_POINT('Ctrl Pts',(-9.89411881045544,-16.7212534506777,
-336.858714286126)) ;
#48110 = CARTESIAN_POINT('Ctrl Pts',(-9.54215496921257,-16.9197489208183,
-336.853748900168)) ;
#48111 = CARTESIAN_POINT('Ctrl Pts',(-9.19070083574343,-17.1179569333501,
-336.848790704993)) ;
#48112 = CARTESIAN_POINT('Ctrl Pts',(-8.83308062432166,-17.3052040074392,
-336.843832509819)) ;
#48113 = CARTESIAN_POINT('Ctrl Pts',(-8.47000180393536,-17.4811239467413,
-336.838874314644)) ;
#48114 = CARTESIAN_POINT('Ctrl Pts',(-8.10613313326873,-17.6574265864532,
-336.833905333294)) ;
#48115 = CARTESIAN_POINT('Ctrl Pts',(-7.7367822872336,-17.8223526376824,-336.828936351944)) ;
#48116 = CARTESIAN_POINT('Ctrl Pts',(-7.36268369354387,-17.975581042871,-336.823967370594)) ;
#48117 = CARTESIAN_POINT('Ctrl Pts',(-6.98858509985413,-18.1288094480596,
-336.818998389244)) ;
#48118 = CARTESIAN_POINT('Ctrl Pts',(-6.60973898280513,-18.2703401225257,
-336.814029407894)) ;
#48119 = CARTESIAN_POINT('Ctrl Pts',(-6.22689881125947,-18.3999009832753,
-336.809060426544)) ;
#48120 = CARTESIAN_POINT('Ctrl Pts',(-5.84457801049804,-18.5292860784421,
-336.804098186241)) ;
#48121 = CARTESIAN_POINT('Ctrl Pts',(-5.45817133665694,-18.6467685768008,
-336.799135945939)) ;
#48122 = CARTESIAN_POINT('Ctrl Pts',(-5.06843896709861,-18.7521079198259,
-336.794173705636)) ;
#48123 = CARTESIAN_POINT('Ctrl Pts',(-4.678771758865,-18.8574296506337,-336.789212294996)) ;
#48124 = CARTESIAN_POINT('Ctrl Pts',(-4.28578019389307,-18.9506122193553,
-336.784250884355)) ;
#48125 = CARTESIAN_POINT('Ctrl Pts',(-3.89023860289182,-19.0314652250574,
-336.779289473715)) ;
#48126 = CARTESIAN_POINT('Ctrl Pts',(-3.49473589180154,-19.1123102832827,
-336.774328550758)) ;
#48127 = CARTESIAN_POINT('Ctrl Pts',(-3.09668388704589,-19.1808281510339,
-336.769367627801)) ;
#48128 = CARTESIAN_POINT('Ctrl Pts',(-2.6968677880342,-19.236879402176,-336.764406704844)) ;
#48129 = CARTESIAN_POINT('Ctrl Pts',(-2.29708549967659,-19.2929259133152,
-336.75944620141)) ;
#48130 = CARTESIAN_POINT('Ctrl Pts',(-1.89553964953067,-19.3365078815061,
-336.754485697977)) ;
#48131 = CARTESIAN_POINT('Ctrl Pts',(-1.49302284378186,-19.3675374735134,
-336.749525194543)) ;
#48132 = CARTESIAN_POINT('Ctrl Pts',(-1.09050631887719,-19.3985670438707,
-336.74456469457)) ;
#48133 = CARTESIAN_POINT('Ctrl Pts',(-0.68701907567866,-19.4170442368549,
-336.739604194598)) ;
#48134 = CARTESIAN_POINT('Ctrl Pts',(-0.28335779853895,-19.4229331811137,
-336.734643694625)) ;
#48135 = CARTESIAN_POINT('Ctrl Pts',(-0.188776922157074,-19.4243130050911,
-336.733481412134)) ;
#48136 = CARTESIAN_POINT('Ctrl Pts',(-0.0941865001972844,-19.4250019592322,
-336.732319129643)) ;
#48137 = CARTESIAN_POINT('Ctrl Pts',(0.000403208488304671,-19.4249999958153,
-336.731156847152)) ;
#48138 = CARTESIAN_POINT('Origin',(0.,0.,-341.375)) ;
#48139 = CARTESIAN_POINT('',(-1.61653377487451E-15,-13.2000000000001,-341.25)) ;
#48140 = CARTESIAN_POINT('',(1.61653377487452E-15,13.2000000000001,-341.25)) ;
#48141 = CARTESIAN_POINT('Origin',(0.,0.,-341.25)) ;
#48142 = CARTESIAN_POINT('',(1.6471499448532E-15,13.4500000000001,-341.5)) ;
#48143 = CARTESIAN_POINT('',(1.63184185986386E-15,13.3250000000001,-341.375)) ;
#48144 = CARTESIAN_POINT('Origin',(0.,0.,-341.5)) ;
#48145 = CARTESIAN_POINT('Origin',(0.,0.,-341.25)) ;
#48146 = CARTESIAN_POINT('Origin',(0.,13.2000000000001,-341.5)) ;
#48147 = CARTESIAN_POINT('',(-2.11251572852918E-15,17.25,-341.5)) ;
#48148 = CARTESIAN_POINT('Origin',(0.,0.,-341.5)) ;
#48149 = CARTESIAN_POINT('Origin',(0.,0.,-219.9625)) ;
#48150 = CARTESIAN_POINT('',(-1.61653377487451E-15,-13.2000000000001,-98.425)) ;
#48151 = CARTESIAN_POINT('Origin',(0.,0.,-98.425)) ;
#48152 = CARTESIAN_POINT('',(-1.61653377487452E-15,-13.2000000000001,-219.9625)) ;
#48153 = CARTESIAN_POINT('Origin',(0.,0.,-341.375)) ;
#48154 = CARTESIAN_POINT('',(-2.14313189850786E-15,-17.5,-341.25)) ;
#48155 = CARTESIAN_POINT('',(-2.14313189850787E-15,17.5,-341.25)) ;
#48156 = CARTESIAN_POINT('Origin',(0.,0.,-341.25)) ;
#48157 = CARTESIAN_POINT('',(-2.12782381351853E-15,17.375,-341.375)) ;
#48158 = CARTESIAN_POINT('Origin',(0.,0.,-341.25)) ;
#48159 = CARTESIAN_POINT('Origin',(0.,0.,-339.75)) ;
#48160 = CARTESIAN_POINT('',(-2.14313189850786E-15,-17.5,-338.)) ;
#48161 = CARTESIAN_POINT('',(-2.14313189850787E-15,-17.5,-339.75)) ;
#48162 = CARTESIAN_POINT('Origin',(0.,0.,-338.)) ;
#48163 = CARTESIAN_POINT('Origin',(0.,0.,-315.875)) ;
#48164 = CARTESIAN_POINT('',(-2.44929359829469E-15,-19.9999999999999,-315.75)) ;
#48165 = CARTESIAN_POINT('',(-2.44929359829469E-15,19.9999999999999,-315.75)) ;
#48166 = CARTESIAN_POINT('Origin',(0.,0.,-315.75)) ;
#48167 = CARTESIAN_POINT('',(-2.41867742831599E-15,19.7499999999997,-316.)) ;
#48168 = CARTESIAN_POINT('',(-2.43398551330534E-15,19.8749999999998,-315.875)) ;
#48169 = CARTESIAN_POINT('Origin',(0.,0.,-316.)) ;
#48170 = CARTESIAN_POINT('Origin',(0.,0.,-315.75)) ;
#48171 = CARTESIAN_POINT('Origin',(0.,0.,-281.)) ;
#48172 = CARTESIAN_POINT('',(-2.44929359829469E-15,-19.9999999999999,-246.)) ;
#48173 = CARTESIAN_POINT('',(-2.44929359829469E-15,-19.9999999999999,-281.)) ;
#48174 = CARTESIAN_POINT('Origin',(0.,0.,-246.)) ;
#48175 = CARTESIAN_POINT('',(5.00000000000251,19.3649167310363,-303.5)) ;
#48176 = CARTESIAN_POINT('',(5.00000000000251,19.3649167310363,-258.5)) ;
#48177 = CARTESIAN_POINT('',(5.00000000000251,19.3649167310363,-281.)) ;
#48178 = CARTESIAN_POINT('',(-5.00000000000251,19.3649167310363,-258.5)) ;
#48179 = CARTESIAN_POINT('Ctrl Pts',(5.00000000000251,19.3649167310363,-258.5)) ;
#48180 = CARTESIAN_POINT('Ctrl Pts',(5.00000000000251,19.3649167310363,-257.869252946608)) ;
#48181 = CARTESIAN_POINT('Ctrl Pts',(4.87339527045222,19.3989431732835,-257.198391459947)) ;
#48182 = CARTESIAN_POINT('Ctrl Pts',(4.36231992558286,19.5202238889459,-255.967346574847)) ;
#48183 = CARTESIAN_POINT('Ctrl Pts',(3.97798553913109,19.6055530258166,-255.406917727262)) ;
#48184 = CARTESIAN_POINT('Ctrl Pts',(3.0931441353592,19.7644752333869,-254.52207632349)) ;
#48185 = CARTESIAN_POINT('Ctrl Pts',(2.5326895230115,19.8486251890166,-254.137693703462)) ;
#48186 = CARTESIAN_POINT('Ctrl Pts',(1.30155327908315,19.9671830048977,-253.626583144847)) ;
#48187 = CARTESIAN_POINT('Ctrl Pts',(0.630658863716503,19.9999999999999,-253.499999999998)) ;
#48188 = CARTESIAN_POINT('Ctrl Pts',(-0.630658863716505,19.9999999999999,
-253.499999999997)) ;
#48189 = CARTESIAN_POINT('Ctrl Pts',(-1.30155327908312,19.9671830048977,-253.626583144847)) ;
#48190 = CARTESIAN_POINT('Ctrl Pts',(-2.53268952301149,19.8486251890166,-254.137693703461)) ;
#48191 = CARTESIAN_POINT('Ctrl Pts',(-3.0931441353592,19.7644752333869,-254.52207632349)) ;
#48192 = CARTESIAN_POINT('Ctrl Pts',(-3.97798553913109,19.6055530258166,-255.406917727262)) ;
#48193 = CARTESIAN_POINT('Ctrl Pts',(-4.36231992558286,19.5202238889459,-255.967346574847)) ;
#48194 = CARTESIAN_POINT('Ctrl Pts',(-4.87339527045222,19.3989431732835,-257.198391459947)) ;
#48195 = CARTESIAN_POINT('Ctrl Pts',(-5.00000000000251,19.3649167310363,-257.869252946608)) ;
#48196 = CARTESIAN_POINT('Ctrl Pts',(-5.00000000000251,19.3649167310363,-258.5)) ;
#48197 = CARTESIAN_POINT('',(-5.00000000000251,19.3649167310363,-303.5)) ;
#48198 = CARTESIAN_POINT('',(-5.00000000000251,19.3649167310363,-281.)) ;
#48199 = CARTESIAN_POINT('Ctrl Pts',(-5.00000000000251,19.3649167310363,-303.5)) ;
#48200 = CARTESIAN_POINT('Ctrl Pts',(-5.00000000000251,19.3649167310363,-304.130747053392)) ;
#48201 = CARTESIAN_POINT('Ctrl Pts',(-4.87339527045224,19.3989431732835,-304.801608540053)) ;
#48202 = CARTESIAN_POINT('Ctrl Pts',(-4.36231992558289,19.5202238889459,-306.032653425153)) ;
#48203 = CARTESIAN_POINT('Ctrl Pts',(-3.97798553913108,19.6055530258166,-306.593082272738)) ;
#48204 = CARTESIAN_POINT('Ctrl Pts',(-3.0931441353592,19.7644752333869,-307.47792367651)) ;
#48205 = CARTESIAN_POINT('Ctrl Pts',(-2.53268952301149,19.8486251890166,-307.862306296539)) ;
#48206 = CARTESIAN_POINT('Ctrl Pts',(-1.30155327908312,19.9671830048977,-308.373416855153)) ;
#48207 = CARTESIAN_POINT('Ctrl Pts',(-0.630658863716505,19.9999999999999,
-308.500000000003)) ;
#48208 = CARTESIAN_POINT('Ctrl Pts',(0.630658863716504,19.9999999999999,-308.500000000003)) ;
#48209 = CARTESIAN_POINT('Ctrl Pts',(1.30155327908312,19.9671830048977,-308.373416855153)) ;
#48210 = CARTESIAN_POINT('Ctrl Pts',(2.53268952301149,19.8486251890166,-307.862306296539)) ;
#48211 = CARTESIAN_POINT('Ctrl Pts',(3.0931441353592,19.7644752333869,-307.47792367651)) ;
#48212 = CARTESIAN_POINT('Ctrl Pts',(3.97798553913108,19.6055530258166,-306.593082272738)) ;
#48213 = CARTESIAN_POINT('Ctrl Pts',(4.36231992558286,19.5202238889459,-306.032653425153)) ;
#48214 = CARTESIAN_POINT('Ctrl Pts',(4.87339527045222,19.3989431732835,-304.801608540053)) ;
#48215 = CARTESIAN_POINT('Ctrl Pts',(5.00000000000251,19.3649167310363,-304.130747053392)) ;
#48216 = CARTESIAN_POINT('Ctrl Pts',(5.00000000000251,19.3649167310363,-303.5)) ;
#48217 = CARTESIAN_POINT('Origin',(0.,18.,-316.)) ;
#48218 = CARTESIAN_POINT('',(-2.20436423846523E-15,-18.,-316.)) ;
#48219 = CARTESIAN_POINT('Origin',(0.,0.,-316.)) ;
#48220 = CARTESIAN_POINT('Origin',(0.,0.,-245.875)) ;
#48221 = CARTESIAN_POINT('',(-2.75545529808154E-15,-22.5,-245.75)) ;
#48222 = CARTESIAN_POINT('',(-2.75545529808155E-15,22.5,-245.75)) ;
#48223 = CARTESIAN_POINT('Origin',(0.,0.,-245.75)) ;
#48224 = CARTESIAN_POINT('',(-2.72483912810286E-15,22.25,-246.)) ;
#48225 = CARTESIAN_POINT('',(-2.7401472130922E-15,22.375,-245.875)) ;
#48226 = CARTESIAN_POINT('Origin',(0.,0.,-246.)) ;
#48227 = CARTESIAN_POINT('Origin',(0.,0.,-245.75)) ;
#48228 = CARTESIAN_POINT('Origin',(0.,0.,-225.)) ;
#48229 = CARTESIAN_POINT('',(-2.75545529808154E-15,-22.5,-204.)) ;
#48230 = CARTESIAN_POINT('',(-2.75545529808154E-15,-22.5,-225.)) ;
#48231 = CARTESIAN_POINT('Origin',(0.,0.,-204.)) ;
#48232 = CARTESIAN_POINT('Origin',(0.,20.,-246.)) ;
#48233 = CARTESIAN_POINT('Origin',(-1.0184458207166E-15,0.,-36.917598465851)) ;
#48234 = CARTESIAN_POINT('',(-4.10256677714363E-15,-33.5,-36.75)) ;
#48235 = CARTESIAN_POINT('',(-3.08053568558583E-15,33.5000000000001,-36.7499999999998)) ;
#48236 = CARTESIAN_POINT('Origin',(0.,0.,-36.75)) ;
#48237 = CARTESIAN_POINT('',(-5.09581437442459E-15,33.2649649327683,-37.0851969317022)) ;
#48238 = CARTESIAN_POINT('',(-4.08817503000501E-15,33.3824824663842,-36.917598465851)) ;
#48239 = CARTESIAN_POINT('',(-4.07378328286638E-15,-33.2649649327684,-37.0851969317021)) ;
#48240 = CARTESIAN_POINT('Origin',(-2.03689164143319E-15,0.,-37.0851969317021)) ;
#48241 = CARTESIAN_POINT('Origin',(-2.03689164143319E-15,0.,-37.0851969317021)) ;
#48242 = CARTESIAN_POINT('Origin',(0.,0.,-36.75)) ;
#48243 = CARTESIAN_POINT('Origin',(0.,0.,-35.5)) ;
#48244 = CARTESIAN_POINT('',(-4.10256677714363E-15,-33.5,-34.25)) ;
#48245 = CARTESIAN_POINT('',(-4.10256677714363E-15,-33.5,-35.5)) ;
#48246 = CARTESIAN_POINT('',(-4.10256677714363E-15,33.5,-34.25)) ;
#48247 = CARTESIAN_POINT('Origin',(0.,0.,-34.25)) ;
#48248 = CARTESIAN_POINT('Origin',(0.,0.,-34.25)) ;
#48249 = CARTESIAN_POINT('Origin',(0.,0.,-39.435)) ;
#48250 = CARTESIAN_POINT('',(-2.45725380248917E-15,-20.065,-41.87)) ;
#48251 = CARTESIAN_POINT('',(3.2799102898164E-15,-26.7825,-39.435)) ;
#48252 = CARTESIAN_POINT('Origin',(0.,0.,-41.87)) ;
#48253 = CARTESIAN_POINT('Origin',(0.,0.,-34.125)) ;
#48254 = CARTESIAN_POINT('',(4.07195060716495E-15,33.25,-34.)) ;
#48255 = CARTESIAN_POINT('',(4.08725869215429E-15,33.375,-34.125)) ;
#48256 = CARTESIAN_POINT('Origin',(0.,0.,-34.)) ;
#48257 = CARTESIAN_POINT('Origin',(0.,33.5,-34.)) ;
#48258 = CARTESIAN_POINT('',(-2.81668763803891E-15,-23.,-34.)) ;
#48259 = CARTESIAN_POINT('Origin',(0.,0.,-34.)) ;
#48260 = CARTESIAN_POINT('Origin',(-4.78454817191255E-16,0.,-0.124961805206562)) ;
#48261 = CARTESIAN_POINT('',(-1.91381926876502E-15,-15.6275202784794,-0.249923610413125)) ;
#48262 = CARTESIAN_POINT('',(-2.39616382493652E-15,15.6275202784794,-0.249923610413161)) ;
#48263 = CARTESIAN_POINT('Origin',(-9.56909634382509E-16,0.,-0.249923610413125)) ;
#48264 = CARTESIAN_POINT('',(-1.94519223636168E-15,15.8837,9.71445146547012E-16)) ;
#48265 = CARTESIAN_POINT('',(-1.92950575256335E-15,15.7556101392397,-0.124961805206562)) ;
#48266 = CARTESIAN_POINT('Origin',(0.,0.,9.71445146547012E-16)) ;
#48267 = CARTESIAN_POINT('Origin',(-9.56909634382509E-16,0.,-0.249923610413125)) ;
#48268 = CARTESIAN_POINT('Origin',(0.,0.,-49.2125)) ;
#48269 = CARTESIAN_POINT('',(1.76555492062875E-15,-14.41685,-49.2125)) ;
#48270 = CARTESIAN_POINT('Origin',(0.,22.225,9.73307724266206E-16)) ;
#48271 = CARTESIAN_POINT('Ctrl Pts',(19.8220328557588,-9.83935203800092,1.06632628357545E-15)) ;
#48272 = CARTESIAN_POINT('Ctrl Pts',(18.7256935583061,-11.8448496981576,1.06632628357545E-15)) ;
#48273 = CARTESIAN_POINT('Ctrl Pts',(17.312558092614,-13.6768414356383,1.8727957933688E-14)) ;
#48274 = CARTESIAN_POINT('Ctrl Pts',(14.015585104321,-16.8064082536566,1.87419927850467E-14)) ;
#48275 = CARTESIAN_POINT('Ctrl Pts',(12.1519545368752,-18.0953645953734,1.88595907275818E-14)) ;
#48276 = CARTESIAN_POINT('Ctrl Pts',(7.64400019407915,-20.2482066689093,1.8890824010698E-14)) ;
#48277 = CARTESIAN_POINT('Ctrl Pts',(4.95667918313636,-20.9612135442109,1.93508252162319E-14)) ;
#48278 = CARTESIAN_POINT('Ctrl Pts',(-0.455353294293309,-21.3054222919409,
1.93680485543092E-14)) ;
#48279 = CARTESIAN_POINT('Ctrl Pts',(-3.17087267179517,-20.9577083375656,
1.9003901490213E-14)) ;
#48280 = CARTESIAN_POINT('Ctrl Pts',(-8.50806489536336,-19.201173436068,1.90220305273563E-14)) ;
#48281 = CARTESIAN_POINT('Ctrl Pts',(-10.5078011878526,-17.8999277787963,
1.90472637662253E-14)) ;
#48282 = CARTESIAN_POINT('Ctrl Pts',(-13.6119178368781,-15.531364223185,1.90472637662253E-14)) ;
#48283 = CARTESIAN_POINT('Ctrl Pts',(-15.1685873535527,-13.8859540469984,
1.06094944223971E-15)) ;
#48284 = CARTESIAN_POINT('Ctrl Pts',(-16.4382148282781,-11.9710934804215,
1.06094944223971E-15)) ;
#48285 = CARTESIAN_POINT('Ctrl Pts',(19.8228138270522,9.84020336516649,1.34055093414798E-14)) ;
#48286 = CARTESIAN_POINT('Ctrl Pts',(19.6074231646947,10.2350439781308,-1.20645810543802E-14)) ;
#48287 = CARTESIAN_POINT('Ctrl Pts',(19.3802577079734,10.622633695729,-2.56087321916339E-14)) ;
#48288 = CARTESIAN_POINT('Ctrl Pts',(19.1415354306511,11.0024033777635,2.41473507855972E-15)) ;
#48289 = CARTESIAN_POINT('Ctrl Pts',(19.1139547928099,11.0462798445128,5.65240988001737E-15)) ;
#48290 = CARTESIAN_POINT('Ctrl Pts',(19.0862198398917,11.0900519047123,-5.99600758964009E-16)) ;
#48291 = CARTESIAN_POINT('Ctrl Pts',(19.0583308674199,11.1337186616126,-1.60982338570648E-15)) ;
#48292 = CARTESIAN_POINT('Ctrl Pts',(18.8185994249655,11.5090747142446,-1.67263190955323E-14)) ;
#48293 = CARTESIAN_POINT('Ctrl Pts',(18.5674911810468,11.8766522063334,6.20331908650578E-15)) ;
#48294 = CARTESIAN_POINT('Ctrl Pts',(18.305518211608,12.2360701986977,-3.88578058618805E-16)) ;
#48295 = CARTESIAN_POINT('Ctrl Pts',(18.0280899316194,12.6166923507932,-7.36936959124135E-15)) ;
#48296 = CARTESIAN_POINT('Ctrl Pts',(17.7384771323971,12.9881646223063,-2.38201952126546E-14)) ;
#48297 = CARTESIAN_POINT('Ctrl Pts',(17.4372377992249,13.3499967502053,-2.71727085277007E-14)) ;
#48298 = CARTESIAN_POINT('Ctrl Pts',(17.150352123501,13.6945880537969,-3.03654789990466E-14)) ;
#48299 = CARTESIAN_POINT('Ctrl Pts',(16.8529207396947,14.0304360740663,-1.60020091492236E-14)) ;
#48300 = CARTESIAN_POINT('Ctrl Pts',(16.5453886606796,14.3570789058094,-2.22044604925031E-15)) ;
#48301 = CARTESIAN_POINT('Ctrl Pts',(16.2391851977278,14.6823105582225,1.15015772258955E-14)) ;
#48302 = CARTESIAN_POINT('Ctrl Pts',(15.9229677023102,14.9984167156392,-1.2744609087233E-14)) ;
#48303 = CARTESIAN_POINT('Ctrl Pts',(15.5971461057912,15.3048990809629,-2.96984659087229E-15)) ;
#48304 = CARTESIAN_POINT('Ctrl Pts',(15.2750178968041,15.6079072807955,6.69411298045808E-15)) ;
#48305 = CARTESIAN_POINT('Ctrl Pts',(14.9435016656073,15.9015088957369,-1.53065317057012E-14)) ;
#48306 = CARTESIAN_POINT('Ctrl Pts',(14.6029711553433,16.1851766092926,-4.90996132640475E-14)) ;
#48307 = CARTESIAN_POINT('Ctrl Pts',(14.5441544529413,16.234171923916,-5.49363813695624E-14)) ;
#48308 = CARTESIAN_POINT('Ctrl Pts',(14.4850687865257,16.2828707685809,-3.91470895560732E-14)) ;
#48309 = CARTESIAN_POINT('Ctrl Pts',(14.4257160273708,16.3312702768893,-2.78943534937071E-14)) ;
#48310 = CARTESIAN_POINT('Ctrl Pts',(14.3863249576248,16.3633919243846,-2.14168009086151E-14)) ;
#48311 = CARTESIAN_POINT('Ctrl Pts',(14.3468162906582,16.3953816143755,2.55660740366257E-14)) ;
#48312 = CARTESIAN_POINT('Ctrl Pts',(14.3072086441427,16.4272241757195,1.9151347174784E-14)) ;
#48313 = CARTESIAN_POINT('Ctrl Pts',(13.9605448541076,16.7059244765716,-3.87855050643946E-14)) ;
#48314 = CARTESIAN_POINT('Ctrl Pts',(13.6059581611611,16.9736384700472,-5.8062702315595E-15)) ;
#48315 = CARTESIAN_POINT('Ctrl Pts',(13.2439289076318,17.2299784476699,-1.18238752122579E-14)) ;
#48316 = CARTESIAN_POINT('Ctrl Pts',(12.8825651717075,17.4858471960581,-2.02521983471332E-14)) ;
#48317 = CARTESIAN_POINT('Ctrl Pts',(12.5137857853607,17.7303840336224,-2.6898344299621E-15)) ;
#48318 = CARTESIAN_POINT('Ctrl Pts',(12.1380355501591,17.9631634907815,4.9960036108132E-16)) ;
#48319 = CARTESIAN_POINT('Ctrl Pts',(11.8446125856444,18.1449407246962,2.99022664375559E-15)) ;
#48320 = CARTESIAN_POINT('Ctrl Pts',(11.5469380627986,18.3195475322449,-8.13343317425171E-15)) ;
#48321 = CARTESIAN_POINT('Ctrl Pts',(11.2452123078566,18.4867623983207,8.49320613838245E-15)) ;
#48322 = CARTESIAN_POINT('Ctrl Pts',(10.857561087322,18.7015967167841,2.95407530613509E-14)) ;
#48323 = CARTESIAN_POINT('Ctrl Pts',(10.4632229713425,18.9042311381886,9.732185371864E-15)) ;
#48324 = CARTESIAN_POINT('Ctrl Pts',(10.0628171189943,19.0945064137273,-4.9960036108132E-16)) ;
#48325 = CARTESIAN_POINT('Ctrl Pts',(9.66298658844184,19.2845082928793,-8.45008909837143E-15)) ;
#48326 = CARTESIAN_POINT('Ctrl Pts',(9.25710520567581,19.4621866299123,1.22637826195654E-14)) ;
#48327 = CARTESIAN_POINT('Ctrl Pts',(8.8457760432505,19.627332765732,-5.55111512312578E-17)) ;
#48328 = CARTESIAN_POINT('Ctrl Pts',(8.53780141147367,19.7509826914229,-9.2793404086585E-15)) ;
#48329 = CARTESIAN_POINT('Ctrl Pts',(8.22677244688017,19.8676060859205,1.04033125354434E-15)) ;
#48330 = CARTESIAN_POINT('Ctrl Pts',(7.91294008103285,19.977096345354,-8.71525074330748E-15)) ;
#48331 = CARTESIAN_POINT('Ctrl Pts',(7.63833676091647,20.0729003223583,-1.75224632892377E-14)) ;
#48332 = CARTESIAN_POINT('Ctrl Pts',(7.36158700918664,20.1632427620598,1.52212933278802E-14)) ;
#48333 = CARTESIAN_POINT('Ctrl Pts',(7.08285900561331,20.2480417027558,8.82627304576999E-15)) ;
#48334 = CARTESIAN_POINT('Ctrl Pts',(7.02245463792221,20.266418852981,9.81933546972611E-15)) ;
#48335 = CARTESIAN_POINT('Ctrl Pts',(6.96195203920544,20.2845371110464,6.60519354014801E-15)) ;
#48336 = CARTESIAN_POINT('Ctrl Pts',(6.90139191111684,20.3023843105404,2.60902410786912E-15)) ;
#48337 = CARTESIAN_POINT('Ctrl Pts',(6.4810143637177,20.4262704743915,-2.51303476199288E-14)) ;
#48338 = CARTESIAN_POINT('Ctrl Pts',(6.05750679718693,20.5372117643199,4.43698005455285E-15)) ;
#48339 = CARTESIAN_POINT('Ctrl Pts',(5.63148115000663,20.6351157318689,8.38218383591993E-15)) ;
#48340 = CARTESIAN_POINT('Ctrl Pts',(5.20377541173699,20.733405797261,1.23429460743014E-14)) ;
#48341 = CARTESIAN_POINT('Ctrl Pts',(4.77353116434053,20.8185556423175,6.00693556424402E-16)) ;
#48342 = CARTESIAN_POINT('Ctrl Pts',(4.34135215828707,20.8904217445994,-5.82867087928207E-15)) ;
#48343 = CARTESIAN_POINT('Ctrl Pts',(3.91039323098268,20.9620849626529,-1.2239884662578E-14)) ;
#48344 = CARTESIAN_POINT('Ctrl Pts',(3.47750992241484,21.0205394167474,-1.30572816134376E-14)) ;
#48345 = CARTESIAN_POINT('Ctrl Pts',(3.04329351149669,21.0655916653857,-1.51545442861334E-14)) ;
#48346 = CARTESIAN_POINT('Ctrl Pts',(2.6136131553603,21.110173274355,-1.72298978413111E-14)) ;
#48347 = CARTESIAN_POINT('Ctrl Pts',(2.18262690328141,21.1416312474094,-1.65856428524431E-14)) ;
#48348 = CARTESIAN_POINT('Ctrl Pts',(1.75090813930699,21.1597273498772,-1.80966353013901E-14)) ;
#48349 = CARTESIAN_POINT('Ctrl Pts',(1.52712976980441,21.1691073366708,-1.88798475561534E-14)) ;
#48350 = CARTESIAN_POINT('Ctrl Pts',(1.30315464273741,21.1748964269943,-1.84395128730138E-15)) ;
#48351 = CARTESIAN_POINT('Ctrl Pts',(1.07906332965069,21.1770559515521,1.4432899320127E-15)) ;
#48352 = CARTESIAN_POINT('Ctrl Pts',(0.641773282680246,21.1812700309928,8.82403367971152E-15)) ;
#48353 = CARTESIAN_POINT('Ctrl Pts',(0.204039724449181,21.1716658755645,3.6105059716605E-16)) ;
#48354 = CARTESIAN_POINT('Ctrl Pts',(-0.233502727656554,21.1483303925341,
-2.20934381900406E-14)) ;
#48355 = CARTESIAN_POINT('Ctrl Pts',(-0.513863661777233,21.1333778826941,
-3.64814396771792E-14)) ;
#48356 = CARTESIAN_POINT('Ctrl Pts',(-0.794145855950668,21.1127866005285,
-1.39896370025936E-14)) ;
#48357 = CARTESIAN_POINT('Ctrl Pts',(-1.07417808744935,21.0865689806994,-1.18793863634892E-14)) ;
#48358 = CARTESIAN_POINT('Ctrl Pts',(-1.14281457396794,21.0801429871617,-1.17339881484418E-14)) ;
#48359 = CARTESIAN_POINT('Ctrl Pts',(-1.21144568059705,21.0733778889363,-1.76353721084238E-15)) ;
#48360 = CARTESIAN_POINT('Ctrl Pts',(-1.28002014750725,21.066279033268,-2.99760216648792E-15)) ;
#48361 = CARTESIAN_POINT('Ctrl Pts',(-1.70928825621511,21.0218410305531,-1.07227038464811E-14)) ;
#48362 = CARTESIAN_POINT('Ctrl Pts',(-2.13658153340179,20.9643096570965,-1.92478364575703E-15)) ;
#48363 = CARTESIAN_POINT('Ctrl Pts',(-2.56131517767835,20.893916388905,-6.88338275267597E-15)) ;
#48364 = CARTESIAN_POINT('Ctrl Pts',(-2.98873827821317,20.8230773834421,-1.18733802090783E-14)) ;
#48365 = CARTESIAN_POINT('Ctrl Pts',(-3.41356976186588,20.73921296819,2.40111047890402E-14)) ;
#48366 = CARTESIAN_POINT('Ctrl Pts',(-3.83520895094919,20.6425063982639,2.66453525910038E-15)) ;
#48367 = CARTESIAN_POINT('Ctrl Pts',(-4.27817603871496,20.540908091567,-1.97618140539818E-14)) ;
#48368 = CARTESIAN_POINT('Ctrl Pts',(-4.71762046092072,20.4251358631229,6.40030023097509E-15)) ;
#48369 = CARTESIAN_POINT('Ctrl Pts',(-5.15283049846049,20.2953424105776,-1.14352971536391E-14)) ;
#48370 = CARTESIAN_POINT('Ctrl Pts',(-5.56435027920578,20.1726141448519,-2.83000302527855E-14)) ;
#48371 = CARTESIAN_POINT('Ctrl Pts',(-5.9720844719591,20.0373489532768,-1.23970021057823E-14)) ;
#48372 = CARTESIAN_POINT('Ctrl Pts',(-6.37541049791806,19.8896279309333,-1.36557432028894E-14)) ;
#48373 = CARTESIAN_POINT('Ctrl Pts',(-6.77519136264614,19.7432053490764,-1.49034201983767E-14)) ;
#48374 = CARTESIAN_POINT('Ctrl Pts',(-7.17064166815835,19.5845447436151,-2.78931875295902E-14)) ;
#48375 = CARTESIAN_POINT('Ctrl Pts',(-7.5611279233789,19.4136819694644,-3.05311331771918E-14)) ;
#48376 = CARTESIAN_POINT('Ctrl Pts',(-7.9453202571054,19.2455731895258,-3.31265599842719E-14)) ;
#48377 = CARTESIAN_POINT('Ctrl Pts',(-8.3247076496214,19.0656521971063,-2.66868924829354E-15)) ;
#48378 = CARTESIAN_POINT('Ctrl Pts',(-8.6986542569747,18.8739144354475,4.9960036108132E-15)) ;
#48379 = CARTESIAN_POINT('Ctrl Pts',(-8.77774295260813,18.8333624176592,6.61706541144845E-15)) ;
#48380 = CARTESIAN_POINT('Ctrl Pts',(-8.85658814700664,18.7922816896624,5.54102316483117E-15)) ;
#48381 = CARTESIAN_POINT('Ctrl Pts',(-8.93518360999352,18.7506719960506,1.16573417585641E-14)) ;
#48382 = CARTESIAN_POINT('Ctrl Pts',(-9.03512384585114,18.6977620387133,1.74862619942157E-14)) ;
#48383 = CARTESIAN_POINT('Ctrl Pts',(-9.13460192966983,18.6440276319535,2.15689584339014E-14)) ;
#48384 = CARTESIAN_POINT('Ctrl Pts',(-9.23360112208329,18.5894827195556,1.88737914186277E-14)) ;
#48385 = CARTESIAN_POINT('Ctrl Pts',(-9.60858213954734,18.3828819761573,8.66525895502832E-15)) ;
#48386 = CARTESIAN_POINT('Ctrl Pts',(-9.97673794510111,18.16463371319,-3.538201205195E-15)) ;
#48387 = CARTESIAN_POINT('Ctrl Pts',(-10.337640427971,17.9352025800157,6.43929354282591E-15)) ;
#48388 = CARTESIAN_POINT('Ctrl Pts',(-10.6998376712863,17.7049483481643,1.64525831832557E-14)) ;
#48389 = CARTESIAN_POINT('Ctrl Pts',(-11.0547298655919,17.4634304923052,-8.11039614496874E-15)) ;
#48390 = CARTESIAN_POINT('Ctrl Pts',(-11.4018536678929,17.2110758102307,8.88178419700125E-16)) ;
#48391 = CARTESIAN_POINT('Ctrl Pts',(-11.6973988559854,16.9962181384567,8.54966805149802E-15)) ;
#48392 = CARTESIAN_POINT('Ctrl Pts',(-11.9873123492652,16.7735039907288,-5.06816677905142E-15)) ;
#48393 = CARTESIAN_POINT('Ctrl Pts',(-12.2712874273964,16.5431754731543,-1.0325074129014E-14)) ;
#48394 = CARTESIAN_POINT('Ctrl Pts',(-12.45058942981,16.3977459351616,-1.36442879859274E-14)) ;
#48395 = CARTESIAN_POINT('Ctrl Pts',(-12.6275235917963,16.2492804225787,1.01350113779492E-14)) ;
#48396 = CARTESIAN_POINT('Ctrl Pts',(-12.802008271987,16.0978363572816,-1.11022302462516E-15)) ;
#48397 = CARTESIAN_POINT('Ctrl Pts',(-12.9038690872333,16.0094262118262,-7.6749755440494E-15)) ;
#48398 = CARTESIAN_POINT('Ctrl Pts',(-13.0048967359161,15.9199994139826,-2.97934760950595E-14)) ;
#48399 = CARTESIAN_POINT('Ctrl Pts',(-13.1050699521942,15.8295709857237,-2.56461518688411E-14)) ;
#48400 = CARTESIAN_POINT('Ctrl Pts',(-13.1481766308034,15.7906576979317,-2.52283304015882E-14)) ;
#48401 = CARTESIAN_POINT('Ctrl Pts',(-13.1911199874146,15.7515634969923,1.05548090712835E-14)) ;
#48402 = CARTESIAN_POINT('Ctrl Pts',(-13.2338908622103,15.7122967829054,6.66133814775094E-15)) ;
#48403 = CARTESIAN_POINT('Ctrl Pts',(-13.5479994724106,15.4239226720676,-2.37149819284577E-14)) ;
#48404 = CARTESIAN_POINT('Ctrl Pts',(-13.8529315665021,15.1261364324721,-1.00319302306805E-14)) ;
#48405 = CARTESIAN_POINT('Ctrl Pts',(-14.1482389299246,14.8193621077826,-9.76996261670138E-15)) ;
#48406 = CARTESIAN_POINT('Ctrl Pts',(-14.4425915472528,14.5135796025483,-9.3945195395561E-15)) ;
#48407 = CARTESIAN_POINT('Ctrl Pts',(-14.7273819262516,14.1988666297625,1.38838895804111E-14)) ;
#48408 = CARTESIAN_POINT('Ctrl Pts',(-15.0021274209657,13.8756091472101,-5.10702591327572E-15)) ;
#48409 = CARTESIAN_POINT('Ctrl Pts',(-15.2735129861793,13.5563048590604,-2.38656968809E-14)) ;
#48410 = CARTESIAN_POINT('Ctrl Pts',(-15.5350981239967,13.2286633506192,-1.0903397624211E-15)) ;
#48411 = CARTESIAN_POINT('Ctrl Pts',(-15.7863751831239,12.8930295683571,6.66133814775094E-16)) ;
#48412 = CARTESIAN_POINT('Ctrl Pts',(-16.0074080429584,12.5977933259076,2.21119478985973E-15)) ;
#48413 = CARTESIAN_POINT('Ctrl Pts',(-16.2204644323149,12.2963724144037,-5.1689895147707E-15)) ;
#48414 = CARTESIAN_POINT('Ctrl Pts',(-16.4251684725406,11.9889877181628,4.66293670342566E-15)) ;
#48415 = CARTESIAN_POINT('Origin',(0.,0.,-55.875)) ;
#48416 = CARTESIAN_POINT('',(-4.10256677714363E-15,-33.5,-55.75)) ;
#48417 = CARTESIAN_POINT('',(-4.10256677714363E-15,33.5,-55.75)) ;
#48418 = CARTESIAN_POINT('Origin',(0.,0.,-55.75)) ;
#48419 = CARTESIAN_POINT('',(-4.07195060716495E-15,33.25,-56.)) ;
#48420 = CARTESIAN_POINT('',(-4.08725869215429E-15,33.375,-55.875)) ;
#48421 = CARTESIAN_POINT('Origin',(0.,0.,-56.)) ;
#48422 = CARTESIAN_POINT('Origin',(0.,0.,-55.75)) ;
#48423 = CARTESIAN_POINT('Origin',(0.,0.,-49.935)) ;
#48424 = CARTESIAN_POINT('',(-4.10256677714363E-15,-33.5,-44.12)) ;
#48425 = CARTESIAN_POINT('',(-4.10256677714363E-15,-33.5,-49.935)) ;
#48426 = CARTESIAN_POINT('',(-4.10256677714363E-15,33.5,-44.12)) ;
#48427 = CARTESIAN_POINT('Origin',(0.,0.,-44.12)) ;
#48428 = CARTESIAN_POINT('Origin',(0.,0.,-44.12)) ;
#48429 = CARTESIAN_POINT('',(27.103076092507,-19.6894201622032,-49.935)) ;
#48430 = CARTESIAN_POINT('Ctrl Pts',(27.103076092507,-19.6894201622032,-49.935)) ;
#48431 = CARTESIAN_POINT('Ctrl Pts',(27.103076092507,-19.6894201622032,-49.4951866852561)) ;
#48432 = CARTESIAN_POINT('Ctrl Pts',(27.1553769624387,-19.6180456661006,-49.0262784098868)) ;
#48433 = CARTESIAN_POINT('Ctrl Pts',(27.3640256598749,-19.3259492202238,-48.1640465487623)) ;
#48434 = CARTESIAN_POINT('Ctrl Pts',(27.5199265959608,-19.1049894709151,-47.7706954545604)) ;
#48435 = CARTESIAN_POINT('Ctrl Pts',(27.8703439079723,-18.590075637148,-47.1495583377523)) ;
#48436 = CARTESIAN_POINT('Ctrl Pts',(28.088216344668,-18.2616609897394,-46.8802501289145)) ;
#48437 = CARTESIAN_POINT('Ctrl Pts',(28.5492221416872,-17.5322010777203,-46.5229621057665)) ;
#48438 = CARTESIAN_POINT('Ctrl Pts',(28.7919452620208,-17.130887957438,-46.435)) ;
#48439 = CARTESIAN_POINT('Ctrl Pts',(29.2317567915366,-16.369112042562,-46.435)) ;
#48440 = CARTESIAN_POINT('Ctrl Pts',(29.4579425884063,-15.9582510941262,-46.5229621057665)) ;
#48441 = CARTESIAN_POINT('Ctrl Pts',(29.8591705047475,-15.1942784066061,-46.8802501289145)) ;
#48442 = CARTESIAN_POINT('Ctrl Pts',(30.0346497140305,-14.841388017939,-47.1495583377523)) ;
#48443 = CARTESIAN_POINT('Ctrl Pts',(30.3053695188271,-14.2804608069275,-47.7706954545604)) ;
#48444 = CARTESIAN_POINT('Ctrl Pts',(30.4187758068994,-14.034966761149,-48.1640465487623)) ;
#48445 = CARTESIAN_POINT('Ctrl Pts',(30.5674144006656,-13.7082234657643,-49.0262784098868)) ;
#48446 = CARTESIAN_POINT('Ctrl Pts',(30.603076092507,-13.6272423357122,-49.4951866852561)) ;
#48447 = CARTESIAN_POINT('Ctrl Pts',(30.603076092507,-13.6272423357122,-50.3748133147439)) ;
#48448 = CARTESIAN_POINT('Ctrl Pts',(30.5674144006656,-13.7082234657643,-50.8437215901132)) ;
#48449 = CARTESIAN_POINT('Ctrl Pts',(30.4187758068994,-14.0349667611491,-51.7059534512376)) ;
#48450 = CARTESIAN_POINT('Ctrl Pts',(30.3053695188271,-14.2804608069275,-52.0993045454395)) ;
#48451 = CARTESIAN_POINT('Ctrl Pts',(30.0346497140305,-14.841388017939,-52.7204416622477)) ;
#48452 = CARTESIAN_POINT('Ctrl Pts',(29.8591705047475,-15.1942784066061,-52.9897498710854)) ;
#48453 = CARTESIAN_POINT('Ctrl Pts',(29.4579425884063,-15.9582510941262,-53.3470378942334)) ;
#48454 = CARTESIAN_POINT('Ctrl Pts',(29.2317567915366,-16.369112042562,-53.435)) ;
#48455 = CARTESIAN_POINT('Ctrl Pts',(28.7919452620208,-17.130887957438,-53.435)) ;
#48456 = CARTESIAN_POINT('Ctrl Pts',(28.5492221416872,-17.5322010777204,-53.3470378942334)) ;
#48457 = CARTESIAN_POINT('Ctrl Pts',(28.088216344668,-18.2616609897394,-52.9897498710854)) ;
#48458 = CARTESIAN_POINT('Ctrl Pts',(27.8703439079723,-18.590075637148,-52.7204416622477)) ;
#48459 = CARTESIAN_POINT('Ctrl Pts',(27.5199265959608,-19.1049894709151,-52.0993045454395)) ;
#48460 = CARTESIAN_POINT('Ctrl Pts',(27.3640256598749,-19.3259492202238,-51.7059534512376)) ;
#48461 = CARTESIAN_POINT('Ctrl Pts',(27.1553769624387,-19.6180456661006,-50.8437215901132)) ;
#48462 = CARTESIAN_POINT('Ctrl Pts',(27.103076092507,-19.6894201622032,-50.3748133147439)) ;
#48463 = CARTESIAN_POINT('Ctrl Pts',(27.103076092507,-19.6894201622032,-49.935)) ;
#48464 = CARTESIAN_POINT('',(-30.603076092507,-13.6272423357121,-49.935)) ;
#48465 = CARTESIAN_POINT('Ctrl Pts',(-30.603076092507,-13.6272423357121,-49.935)) ;
#48466 = CARTESIAN_POINT('Ctrl Pts',(-30.603076092507,-13.6272423357121,-49.4951866852561)) ;
#48467 = CARTESIAN_POINT('Ctrl Pts',(-30.5674144006657,-13.7082234657643,
-49.0262784098868)) ;
#48468 = CARTESIAN_POINT('Ctrl Pts',(-30.4187758068994,-14.034966761149,-48.1640465487624)) ;
#48469 = CARTESIAN_POINT('Ctrl Pts',(-30.3053695188271,-14.2804608069275,
-47.7706954545604)) ;
#48470 = CARTESIAN_POINT('Ctrl Pts',(-30.0346497140305,-14.8413880179389,
-47.1495583377523)) ;
#48471 = CARTESIAN_POINT('Ctrl Pts',(-29.8591705047475,-15.1942784066061,
-46.8802501289145)) ;
#48472 = CARTESIAN_POINT('Ctrl Pts',(-29.4579425884064,-15.9582510941262,
-46.5229621057665)) ;
#48473 = CARTESIAN_POINT('Ctrl Pts',(-29.2317567915366,-16.369112042562,-46.435)) ;
#48474 = CARTESIAN_POINT('Ctrl Pts',(-28.7919452620208,-17.130887957438,-46.435)) ;
#48475 = CARTESIAN_POINT('Ctrl Pts',(-28.5492221416873,-17.5322010777203,
-46.5229621057665)) ;
#48476 = CARTESIAN_POINT('Ctrl Pts',(-28.088216344668,-18.2616609897393,-46.8802501289145)) ;
#48477 = CARTESIAN_POINT('Ctrl Pts',(-27.8703439079724,-18.5900756371479,
-47.1495583377523)) ;
#48478 = CARTESIAN_POINT('Ctrl Pts',(-27.5199265959608,-19.1049894709151,
-47.7706954545604)) ;
#48479 = CARTESIAN_POINT('Ctrl Pts',(-27.364025659875,-19.3259492202238,-48.1640465487624)) ;
#48480 = CARTESIAN_POINT('Ctrl Pts',(-27.1553769624387,-19.6180456661006,
-49.0262784098868)) ;
#48481 = CARTESIAN_POINT('Ctrl Pts',(-27.103076092507,-19.6894201622032,-49.4951866852561)) ;
#48482 = CARTESIAN_POINT('Ctrl Pts',(-27.103076092507,-19.6894201622032,-50.3748133147439)) ;
#48483 = CARTESIAN_POINT('Ctrl Pts',(-27.1553769624387,-19.6180456661006,
-50.8437215901132)) ;
#48484 = CARTESIAN_POINT('Ctrl Pts',(-27.364025659875,-19.3259492202238,-51.7059534512376)) ;
#48485 = CARTESIAN_POINT('Ctrl Pts',(-27.5199265959608,-19.1049894709151,
-52.0993045454395)) ;
#48486 = CARTESIAN_POINT('Ctrl Pts',(-27.8703439079724,-18.5900756371479,
-52.7204416622477)) ;
#48487 = CARTESIAN_POINT('Ctrl Pts',(-28.088216344668,-18.2616609897393,-52.9897498710855)) ;
#48488 = CARTESIAN_POINT('Ctrl Pts',(-28.5492221416873,-17.5322010777203,
-53.3470378942334)) ;
#48489 = CARTESIAN_POINT('Ctrl Pts',(-28.7919452620208,-17.130887957438,-53.435)) ;
#48490 = CARTESIAN_POINT('Ctrl Pts',(-29.2317567915366,-16.369112042562,-53.435)) ;
#48491 = CARTESIAN_POINT('Ctrl Pts',(-29.4579425884064,-15.9582510941262,
-53.3470378942334)) ;
#48492 = CARTESIAN_POINT('Ctrl Pts',(-29.8591705047475,-15.1942784066061,
-52.9897498710855)) ;
#48493 = CARTESIAN_POINT('Ctrl Pts',(-30.0346497140305,-14.8413880179389,
-52.7204416622477)) ;
#48494 = CARTESIAN_POINT('Ctrl Pts',(-30.3053695188271,-14.2804608069275,
-52.0993045454395)) ;
#48495 = CARTESIAN_POINT('Ctrl Pts',(-30.4187758068994,-14.034966761149,-51.7059534512376)) ;
#48496 = CARTESIAN_POINT('Ctrl Pts',(-30.5674144006656,-13.7082234657643,
-50.8437215901132)) ;
#48497 = CARTESIAN_POINT('Ctrl Pts',(-30.603076092507,-13.6272423357121,-50.3748133147439)) ;
#48498 = CARTESIAN_POINT('Ctrl Pts',(-30.603076092507,-13.6272423357121,-49.935)) ;
#48499 = CARTESIAN_POINT('',(3.5,33.3166624979154,-49.935)) ;
#48500 = CARTESIAN_POINT('Ctrl Pts',(3.5,33.3166624979154,-49.935)) ;
#48501 = CARTESIAN_POINT('Ctrl Pts',(3.5,33.3166624979154,-49.4951866852561)) ;
#48502 = CARTESIAN_POINT('Ctrl Pts',(3.41203743822697,33.3262691318649,-49.0262784098868)) ;
#48503 = CARTESIAN_POINT('Ctrl Pts',(3.05475014702442,33.3609159813728,-48.1640465487623)) ;
#48504 = CARTESIAN_POINT('Ctrl Pts',(2.7854429228663,33.3854502778426,-47.7706954545604)) ;
#48505 = CARTESIAN_POINT('Ctrl Pts',(2.16430580605813,33.4314636550869,-47.1495583377523)) ;
#48506 = CARTESIAN_POINT('Ctrl Pts',(1.77095416007957,33.4559393963454,-46.8802501289145)) ;
#48507 = CARTESIAN_POINT('Ctrl Pts',(0.908720446719096,33.4904521718465,-46.5229621057665)) ;
#48508 = CARTESIAN_POINT('Ctrl Pts',(0.439811529515813,33.5,-46.435)) ;
#48509 = CARTESIAN_POINT('Ctrl Pts',(-0.439811529515812,33.5,-46.435)) ;
#48510 = CARTESIAN_POINT('Ctrl Pts',(-0.908720446719095,33.4904521718465,
-46.5229621057665)) ;
#48511 = CARTESIAN_POINT('Ctrl Pts',(-1.77095416007956,33.4559393963454,-46.8802501289145)) ;
#48512 = CARTESIAN_POINT('Ctrl Pts',(-2.16430580605813,33.4314636550869,-47.1495583377523)) ;
#48513 = CARTESIAN_POINT('Ctrl Pts',(-2.7854429228663,33.3854502778426,-47.7706954545604)) ;
#48514 = CARTESIAN_POINT('Ctrl Pts',(-3.05475014702442,33.3609159813728,-48.1640465487623)) ;
#48515 = CARTESIAN_POINT('Ctrl Pts',(-3.41203743822697,33.3262691318649,-49.0262784098868)) ;
#48516 = CARTESIAN_POINT('Ctrl Pts',(-3.5,33.3166624979154,-49.4951866852561)) ;
#48517 = CARTESIAN_POINT('Ctrl Pts',(-3.5,33.3166624979154,-50.3748133147439)) ;
#48518 = CARTESIAN_POINT('Ctrl Pts',(-3.41203743822697,33.3262691318649,-50.8437215901132)) ;
#48519 = CARTESIAN_POINT('Ctrl Pts',(-3.05475014702442,33.3609159813728,-51.7059534512376)) ;
#48520 = CARTESIAN_POINT('Ctrl Pts',(-2.7854429228663,33.3854502778426,-52.0993045454395)) ;
#48521 = CARTESIAN_POINT('Ctrl Pts',(-2.16430580605813,33.4314636550869,-52.7204416622477)) ;
#48522 = CARTESIAN_POINT('Ctrl Pts',(-1.77095416007956,33.4559393963454,-52.9897498710854)) ;
#48523 = CARTESIAN_POINT('Ctrl Pts',(-0.908720446719096,33.4904521718465,
-53.3470378942334)) ;
#48524 = CARTESIAN_POINT('Ctrl Pts',(-0.439811529515812,33.5,-53.435)) ;
#48525 = CARTESIAN_POINT('Ctrl Pts',(0.439811529515812,33.5,-53.435)) ;
#48526 = CARTESIAN_POINT('Ctrl Pts',(0.908720446719096,33.4904521718465,-53.3470378942334)) ;
#48527 = CARTESIAN_POINT('Ctrl Pts',(1.77095416007957,33.4559393963454,-52.9897498710854)) ;
#48528 = CARTESIAN_POINT('Ctrl Pts',(2.16430580605813,33.4314636550869,-52.7204416622477)) ;
#48529 = CARTESIAN_POINT('Ctrl Pts',(2.7854429228663,33.3854502778426,-52.0993045454395)) ;
#48530 = CARTESIAN_POINT('Ctrl Pts',(3.05475014702442,33.3609159813728,-51.7059534512376)) ;
#48531 = CARTESIAN_POINT('Ctrl Pts',(3.41203743822697,33.3262691318649,-50.8437215901132)) ;
#48532 = CARTESIAN_POINT('Ctrl Pts',(3.5,33.3166624979154,-50.3748133147439)) ;
#48533 = CARTESIAN_POINT('Ctrl Pts',(3.5,33.3166624979154,-49.935)) ;
#48534 = CARTESIAN_POINT('Origin',(0.,22.5,-56.)) ;
#48535 = CARTESIAN_POINT('',(-2.75545529808154E-15,-22.5,-56.)) ;
#48536 = CARTESIAN_POINT('Origin',(0.,0.,-56.)) ;
#48537 = CARTESIAN_POINT('Origin',(0.,0.,-43.995)) ;
#48538 = CARTESIAN_POINT('',(4.07195060716495E-15,33.25,-43.87)) ;
#48539 = CARTESIAN_POINT('',(4.08725869215429E-15,33.375,-43.995)) ;
#48540 = CARTESIAN_POINT('Origin',(0.,0.,-43.87)) ;
#48541 = CARTESIAN_POINT('Origin',(0.,33.5,-43.87)) ;
#48542 = CARTESIAN_POINT('',(-2.45725380248917E-15,-20.065,-43.87)) ;
#48543 = CARTESIAN_POINT('Origin',(0.,0.,-43.87)) ;
#48544 = CARTESIAN_POINT('Ctrl Pts',(27.103076092507,-19.6894201622032,-49.935)) ;
#48545 = CARTESIAN_POINT('Ctrl Pts',(18.4427076638945,-14.6893541186624,-49.935)) ;
#48546 = CARTESIAN_POINT('Ctrl Pts',(27.103076092507,-19.6894201622032,-49.4951866852561)) ;
#48547 = CARTESIAN_POINT('Ctrl Pts',(18.4427076638945,-14.6893541186624,-49.4951866852561)) ;
#48548 = CARTESIAN_POINT('Ctrl Pts',(27.1553769624387,-19.6180456661006,-49.0262784098868)) ;
#48549 = CARTESIAN_POINT('Ctrl Pts',(18.4950085338262,-14.6179796225598,-49.0262784098868)) ;
#48550 = CARTESIAN_POINT('Ctrl Pts',(27.3640256598749,-19.3259492202238,-48.1640465487623)) ;
#48551 = CARTESIAN_POINT('Ctrl Pts',(18.7036572312625,-14.325883176683,-48.1640465487623)) ;
#48552 = CARTESIAN_POINT('Ctrl Pts',(27.5199265959608,-19.1049894709151,-47.7706954545604)) ;
#48553 = CARTESIAN_POINT('Ctrl Pts',(18.8595581673483,-14.1049234273743,-47.7706954545604)) ;
#48554 = CARTESIAN_POINT('Ctrl Pts',(27.8703439079723,-18.590075637148,-47.1495583377523)) ;
#48555 = CARTESIAN_POINT('Ctrl Pts',(19.2099754793599,-13.5900095936072,-47.1495583377523)) ;
#48556 = CARTESIAN_POINT('Ctrl Pts',(28.088216344668,-18.2616609897394,-46.8802501289145)) ;
#48557 = CARTESIAN_POINT('Ctrl Pts',(19.4278479160555,-13.2615949461985,-46.8802501289145)) ;
#48558 = CARTESIAN_POINT('Ctrl Pts',(28.5492221416872,-17.5322010777203,-46.5229621057665)) ;
#48559 = CARTESIAN_POINT('Ctrl Pts',(19.8888537130748,-12.5321350341795,-46.5229621057665)) ;
#48560 = CARTESIAN_POINT('Ctrl Pts',(28.7919452620208,-17.130887957438,-46.435)) ;
#48561 = CARTESIAN_POINT('Ctrl Pts',(20.1315768334083,-12.1308219138972,-46.435)) ;
#48562 = CARTESIAN_POINT('Ctrl Pts',(29.2317567915366,-16.369112042562,-46.435)) ;
#48563 = CARTESIAN_POINT('Ctrl Pts',(20.5713883629241,-11.3690459990212,-46.435)) ;
#48564 = CARTESIAN_POINT('Ctrl Pts',(29.4579425884063,-15.9582510941262,-46.5229621057665)) ;
#48565 = CARTESIAN_POINT('Ctrl Pts',(20.7975741597939,-10.9581850505854,-46.5229621057665)) ;
#48566 = CARTESIAN_POINT('Ctrl Pts',(29.8591705047475,-15.1942784066061,-46.8802501289145)) ;
#48567 = CARTESIAN_POINT('Ctrl Pts',(21.198802076135,-10.1942123630653,-46.8802501289145)) ;
#48568 = CARTESIAN_POINT('Ctrl Pts',(30.0346497140305,-14.841388017939,-47.1495583377523)) ;
#48569 = CARTESIAN_POINT('Ctrl Pts',(21.374281285418,-9.84132197439817,-47.1495583377523)) ;
#48570 = CARTESIAN_POINT('Ctrl Pts',(30.3053695188271,-14.2804608069275,-47.7706954545604)) ;
#48571 = CARTESIAN_POINT('Ctrl Pts',(21.6450010902146,-9.28039476338673,-47.7706954545604)) ;
#48572 = CARTESIAN_POINT('Ctrl Pts',(30.4187758068994,-14.034966761149,-48.1640465487623)) ;
#48573 = CARTESIAN_POINT('Ctrl Pts',(21.7584073782869,-9.03490071760825,-48.1640465487623)) ;
#48574 = CARTESIAN_POINT('Ctrl Pts',(30.5674144006656,-13.7082234657643,-49.0262784098868)) ;
#48575 = CARTESIAN_POINT('Ctrl Pts',(21.9070459720532,-8.70815742222352,-49.0262784098868)) ;
#48576 = CARTESIAN_POINT('Ctrl Pts',(30.603076092507,-13.6272423357122,-49.4951866852561)) ;
#48577 = CARTESIAN_POINT('Ctrl Pts',(21.9427076638945,-8.62717629217136,-49.4951866852561)) ;
#48578 = CARTESIAN_POINT('Ctrl Pts',(30.603076092507,-13.6272423357122,-50.3748133147439)) ;
#48579 = CARTESIAN_POINT('Ctrl Pts',(21.9427076638945,-8.62717629217136,-50.3748133147439)) ;
#48580 = CARTESIAN_POINT('Ctrl Pts',(30.5674144006656,-13.7082234657643,-50.8437215901132)) ;
#48581 = CARTESIAN_POINT('Ctrl Pts',(21.9070459720532,-8.70815742222352,-50.8437215901132)) ;
#48582 = CARTESIAN_POINT('Ctrl Pts',(30.4187758068994,-14.0349667611491,-51.7059534512376)) ;
#48583 = CARTESIAN_POINT('Ctrl Pts',(21.7584073782869,-9.03490071760825,-51.7059534512376)) ;
#48584 = CARTESIAN_POINT('Ctrl Pts',(30.3053695188271,-14.2804608069275,-52.0993045454395)) ;
#48585 = CARTESIAN_POINT('Ctrl Pts',(21.6450010902146,-9.28039476338673,-52.0993045454395)) ;
#48586 = CARTESIAN_POINT('Ctrl Pts',(30.0346497140305,-14.841388017939,-52.7204416622477)) ;
#48587 = CARTESIAN_POINT('Ctrl Pts',(21.374281285418,-9.84132197439817,-52.7204416622477)) ;
#48588 = CARTESIAN_POINT('Ctrl Pts',(29.8591705047475,-15.1942784066061,-52.9897498710854)) ;
#48589 = CARTESIAN_POINT('Ctrl Pts',(21.198802076135,-10.1942123630653,-52.9897498710854)) ;
#48590 = CARTESIAN_POINT('Ctrl Pts',(29.4579425884063,-15.9582510941262,-53.3470378942334)) ;
#48591 = CARTESIAN_POINT('Ctrl Pts',(20.7975741597939,-10.9581850505854,-53.3470378942334)) ;
#48592 = CARTESIAN_POINT('Ctrl Pts',(29.2317567915366,-16.369112042562,-53.435)) ;
#48593 = CARTESIAN_POINT('Ctrl Pts',(20.5713883629241,-11.3690459990212,-53.435)) ;
#48594 = CARTESIAN_POINT('Ctrl Pts',(28.7919452620208,-17.130887957438,-53.435)) ;
#48595 = CARTESIAN_POINT('Ctrl Pts',(20.1315768334083,-12.1308219138972,-53.435)) ;
#48596 = CARTESIAN_POINT('Ctrl Pts',(28.5492221416872,-17.5322010777204,-53.3470378942334)) ;
#48597 = CARTESIAN_POINT('Ctrl Pts',(19.8888537130748,-12.5321350341795,-53.3470378942334)) ;
#48598 = CARTESIAN_POINT('Ctrl Pts',(28.088216344668,-18.2616609897394,-52.9897498710854)) ;
#48599 = CARTESIAN_POINT('Ctrl Pts',(19.4278479160555,-13.2615949461986,-52.9897498710854)) ;
#48600 = CARTESIAN_POINT('Ctrl Pts',(27.8703439079723,-18.590075637148,-52.7204416622477)) ;
#48601 = CARTESIAN_POINT('Ctrl Pts',(19.2099754793599,-13.5900095936072,-52.7204416622477)) ;
#48602 = CARTESIAN_POINT('Ctrl Pts',(27.5199265959608,-19.1049894709151,-52.0993045454395)) ;
#48603 = CARTESIAN_POINT('Ctrl Pts',(18.8595581673483,-14.1049234273743,-52.0993045454395)) ;
#48604 = CARTESIAN_POINT('Ctrl Pts',(27.3640256598749,-19.3259492202238,-51.7059534512376)) ;
#48605 = CARTESIAN_POINT('Ctrl Pts',(18.7036572312625,-14.325883176683,-51.7059534512376)) ;
#48606 = CARTESIAN_POINT('Ctrl Pts',(27.1553769624387,-19.6180456661006,-50.8437215901132)) ;
#48607 = CARTESIAN_POINT('Ctrl Pts',(18.4950085338262,-14.6179796225598,-50.8437215901132)) ;
#48608 = CARTESIAN_POINT('Ctrl Pts',(27.103076092507,-19.6894201622032,-50.3748133147439)) ;
#48609 = CARTESIAN_POINT('Ctrl Pts',(18.4427076638945,-14.6893541186624,-50.3748133147439)) ;
#48610 = CARTESIAN_POINT('Ctrl Pts',(27.103076092507,-19.6894201622032,-49.935)) ;
#48611 = CARTESIAN_POINT('Ctrl Pts',(18.4427076638945,-14.6893541186624,-49.935)) ;
#48612 = CARTESIAN_POINT('',(18.4427987905013,-14.6894573115498,-49.9350000240614)) ;
#48613 = CARTESIAN_POINT('Ctrl Pts',(27.103076092507,-19.6894201622032,-49.935)) ;
#48614 = CARTESIAN_POINT('Ctrl Pts',(18.4428206926806,-14.6894193758625,-49.935)) ;
#48615 = CARTESIAN_POINT('Ctrl Pts',(18.4427987905013,-14.6894573115498,-49.9350000240614)) ;
#48616 = CARTESIAN_POINT('Ctrl Pts',(18.4427531120374,-14.6895275477814,-49.7823947044338)) ;
#48617 = CARTESIAN_POINT('Ctrl Pts',(18.44886735586,-14.681117357845,-49.6112134273951)) ;
#48618 = CARTESIAN_POINT('Ctrl Pts',(18.4853437963175,-14.6307823444917,-49.1998503646376)) ;
#48619 = CARTESIAN_POINT('Ctrl Pts',(18.5175132400749,-14.5863573189043,-48.9745962929381)) ;
#48620 = CARTESIAN_POINT('Ctrl Pts',(18.6657603536904,-14.3796102913098,-48.2662983684852)) ;
#48621 = CARTESIAN_POINT('Ctrl Pts',(18.819056053797,-14.1621995813133,-47.883172642928)) ;
#48622 = CARTESIAN_POINT('Ctrl Pts',(19.1522667831666,-13.6773365162311,-47.2139532467364)) ;
#48623 = CARTESIAN_POINT('Ctrl Pts',(19.3750593745531,-13.3405007077791,-46.9533770888002)) ;
#48624 = CARTESIAN_POINT('Ctrl Pts',(19.7974436197774,-12.6811571505934,-46.5664922879644)) ;
#48625 = CARTESIAN_POINT('Ctrl Pts',(20.0358995829733,-12.2890367087697,-46.4734326225838)) ;
#48626 = CARTESIAN_POINT('Ctrl Pts',(20.4843327090169,-11.5262783305788,-46.4045524997322)) ;
#48627 = CARTESIAN_POINT('Ctrl Pts',(20.7104180554908,-11.1164311593209,-46.4925278051967)) ;
#48628 = CARTESIAN_POINT('Ctrl Pts',(21.108737346578,-10.3719551438664,-46.7651000997357)) ;
#48629 = CARTESIAN_POINT('Ctrl Pts',(21.285707958859,-10.0190112984326,-47.0172803610138)) ;
#48630 = CARTESIAN_POINT('Ctrl Pts',(21.5947015506035,-9.38960342665918,-47.6023005356928)) ;
#48631 = CARTESIAN_POINT('Ctrl Pts',(21.7078493371503,-9.14418273779913,-47.9944593073979)) ;
#48632 = CARTESIAN_POINT('Ctrl Pts',(21.8061586042231,-8.93024469048519,-48.4438880038744)) ;
#48633 = CARTESIAN_POINT('Ctrl Pts',(21.8303892027021,-8.87707989392543,-48.5725202466068)) ;
#48634 = CARTESIAN_POINT('Ctrl Pts',(21.8812156221636,-8.76494580189594,-48.9021343175402)) ;
#48635 = CARTESIAN_POINT('Ctrl Pts',(21.9045461994582,-8.71293077313088,-49.1073011631895)) ;
#48636 = CARTESIAN_POINT('Ctrl Pts',(21.9350469301527,-8.64473773197279,-49.5238351190534)) ;
#48637 = CARTESIAN_POINT('Ctrl Pts',(21.9428220546626,-8.62724233571215,-49.7302427331702)) ;
#48638 = CARTESIAN_POINT('Ctrl Pts',(21.9428220546626,-8.62724233571215,-49.9349999999999)) ;
#48639 = CARTESIAN_POINT('Ctrl Pts',(21.9428220546626,-8.62724233571214,-50.1455828409762)) ;
#48640 = CARTESIAN_POINT('Ctrl Pts',(21.9346003886721,-8.64575634274508,-50.3651730635469)) ;
#48641 = CARTESIAN_POINT('Ctrl Pts',(21.8828966189749,-8.76128851199987,-51.0288729348249)) ;
#48642 = CARTESIAN_POINT('Ctrl Pts',(21.8146962770843,-8.91397276739595,-51.4570912893389)) ;
#48643 = CARTESIAN_POINT('Ctrl Pts',(21.6503326879261,-9.26650739525063,-52.0447545851038)) ;
#48644 = CARTESIAN_POINT('Ctrl Pts',(21.5887973035584,-9.39696090923297,-52.2259765012846)) ;
#48645 = CARTESIAN_POINT('Ctrl Pts',(21.4513830427457,-9.68202705953242,-52.5458841412737)) ;
#48646 = CARTESIAN_POINT('Ctrl Pts',(21.3762106229735,-9.83562627323664,-52.6891786697716)) ;
#48647 = CARTESIAN_POINT('Ctrl Pts',(21.2102533734648,-10.1669521283806,-52.9435506339985)) ;
#48648 = CARTESIAN_POINT('Ctrl Pts',(21.1181821598937,-10.347396276298,-53.0578107060786)) ;
#48649 = CARTESIAN_POINT('Ctrl Pts',(20.9269456889309,-10.712576459322,-53.2347269698551)) ;
#48650 = CARTESIAN_POINT('Ctrl Pts',(20.8290550037948,-10.8958458805748,-53.3020383948391)) ;
#48651 = CARTESIAN_POINT('Ctrl Pts',(20.6215184026939,-11.2749481451676,-53.3980021942758)) ;
#48652 = CARTESIAN_POINT('Ctrl Pts',(20.5100659904938,-11.4741500863567,-53.4280956303302)) ;
#48653 = CARTESIAN_POINT('Ctrl Pts',(20.3007086380488,-11.8388564562127,-53.4385899044817)) ;
#48654 = CARTESIAN_POINT('Ctrl Pts',(20.1905268829027,-12.0278357833663,-53.4290562483249)) ;
#48655 = CARTESIAN_POINT('Ctrl Pts',(19.9467874918082,-12.4337355258641,-53.3497426101656)) ;
#48656 = CARTESIAN_POINT('Ctrl Pts',(19.8292512709116,-12.6251940105125,-53.2913599998512)) ;
#48657 = CARTESIAN_POINT('Ctrl Pts',(19.6045297561846,-12.983107603713,-53.1317914335173)) ;
#48658 = CARTESIAN_POINT('Ctrl Pts',(19.4976150092651,-13.1499610391986,-53.0347656954103)) ;
#48659 = CARTESIAN_POINT('Ctrl Pts',(19.2900755252539,-13.4679315770041,-52.8014456739523)) ;
#48660 = CARTESIAN_POINT('Ctrl Pts',(19.1872844094319,-13.6224261317564,-52.6636415879439)) ;
#48661 = CARTESIAN_POINT('Ctrl Pts',(19.0121283157254,-13.8814349031294,-52.3760206544823)) ;
#48662 = CARTESIAN_POINT('Ctrl Pts',(18.9262394436352,-14.0068222128443,-52.2154232168395)) ;
#48663 = CARTESIAN_POINT('Ctrl Pts',(18.7059260228408,-14.3234467106669,-51.690363352432)) ;
#48664 = CARTESIAN_POINT('Ctrl Pts',(18.5760427442282,-14.5051400890156,-51.2863619910567)) ;
#48665 = CARTESIAN_POINT('Ctrl Pts',(18.4709264873325,-14.6507434167168,-50.5442029076166)) ;
#48666 = CARTESIAN_POINT('Ctrl Pts',(18.4508136331523,-14.678417533721,-50.3167637435239)) ;
#48667 = CARTESIAN_POINT('Ctrl Pts',(18.4435200648678,-14.6884594034969,-50.0351173441296)) ;
#48668 = CARTESIAN_POINT('Ctrl Pts',(18.4428140859908,-14.6894337928618,-49.9861001018761)) ;
#48669 = CARTESIAN_POINT('Ctrl Pts',(18.4427987905013,-14.6894573115498,-49.9350000240614)) ;
#48670 = CARTESIAN_POINT('Origin',(-8.66025403784438,5.,-49.935)) ;
#48671 = CARTESIAN_POINT('Ctrl Pts',(-30.603076092507,-13.6272423357121,-49.935)) ;
#48672 = CARTESIAN_POINT('Ctrl Pts',(-21.9427076638945,-8.62717629217139,
-49.935)) ;
#48673 = CARTESIAN_POINT('Ctrl Pts',(-30.603076092507,-13.6272423357121,-49.4951866852561)) ;
#48674 = CARTESIAN_POINT('Ctrl Pts',(-21.9427076638945,-8.62717629217139,
-49.4951866852561)) ;
#48675 = CARTESIAN_POINT('Ctrl Pts',(-30.5674144006657,-13.7082234657643,
-49.0262784098868)) ;
#48676 = CARTESIAN_POINT('Ctrl Pts',(-21.9070459720532,-8.70815742222356,
-49.0262784098868)) ;
#48677 = CARTESIAN_POINT('Ctrl Pts',(-30.4187758068994,-14.034966761149,-48.1640465487624)) ;
#48678 = CARTESIAN_POINT('Ctrl Pts',(-21.758407378287,-9.03490071760828,-48.1640465487624)) ;
#48679 = CARTESIAN_POINT('Ctrl Pts',(-30.3053695188271,-14.2804608069275,
-47.7706954545604)) ;
#48680 = CARTESIAN_POINT('Ctrl Pts',(-21.6450010902146,-9.28039476338676,
-47.7706954545604)) ;
#48681 = CARTESIAN_POINT('Ctrl Pts',(-30.0346497140305,-14.8413880179389,
-47.1495583377523)) ;
#48682 = CARTESIAN_POINT('Ctrl Pts',(-21.374281285418,-9.8413219743982,-47.1495583377523)) ;
#48683 = CARTESIAN_POINT('Ctrl Pts',(-29.8591705047475,-15.1942784066061,
-46.8802501289145)) ;
#48684 = CARTESIAN_POINT('Ctrl Pts',(-21.198802076135,-10.1942123630653,-46.8802501289145)) ;
#48685 = CARTESIAN_POINT('Ctrl Pts',(-29.4579425884064,-15.9582510941262,
-46.5229621057665)) ;
#48686 = CARTESIAN_POINT('Ctrl Pts',(-20.797574159794,-10.9581850505854,-46.5229621057665)) ;
#48687 = CARTESIAN_POINT('Ctrl Pts',(-29.2317567915366,-16.369112042562,-46.435)) ;
#48688 = CARTESIAN_POINT('Ctrl Pts',(-20.5713883629241,-11.3690459990212,
-46.435)) ;
#48689 = CARTESIAN_POINT('Ctrl Pts',(-28.7919452620208,-17.130887957438,-46.435)) ;
#48690 = CARTESIAN_POINT('Ctrl Pts',(-20.1315768334083,-12.1308219138972,
-46.435)) ;
#48691 = CARTESIAN_POINT('Ctrl Pts',(-28.5492221416873,-17.5322010777203,
-46.5229621057665)) ;
#48692 = CARTESIAN_POINT('Ctrl Pts',(-19.8888537130748,-12.5321350341795,
-46.5229621057665)) ;
#48693 = CARTESIAN_POINT('Ctrl Pts',(-28.088216344668,-18.2616609897393,-46.8802501289145)) ;
#48694 = CARTESIAN_POINT('Ctrl Pts',(-19.4278479160555,-13.2615949461985,
-46.8802501289145)) ;
#48695 = CARTESIAN_POINT('Ctrl Pts',(-27.8703439079724,-18.5900756371479,
-47.1495583377523)) ;
#48696 = CARTESIAN_POINT('Ctrl Pts',(-19.2099754793599,-13.5900095936071,
-47.1495583377523)) ;
#48697 = CARTESIAN_POINT('Ctrl Pts',(-27.5199265959608,-19.1049894709151,
-47.7706954545604)) ;
#48698 = CARTESIAN_POINT('Ctrl Pts',(-18.8595581673484,-14.1049234273743,
-47.7706954545604)) ;
#48699 = CARTESIAN_POINT('Ctrl Pts',(-27.364025659875,-19.3259492202238,-48.1640465487624)) ;
#48700 = CARTESIAN_POINT('Ctrl Pts',(-18.7036572312625,-14.325883176683,-48.1640465487624)) ;
#48701 = CARTESIAN_POINT('Ctrl Pts',(-27.1553769624387,-19.6180456661006,
-49.0262784098868)) ;
#48702 = CARTESIAN_POINT('Ctrl Pts',(-18.4950085338262,-14.6179796225598,
-49.0262784098868)) ;
#48703 = CARTESIAN_POINT('Ctrl Pts',(-27.103076092507,-19.6894201622032,-49.4951866852561)) ;
#48704 = CARTESIAN_POINT('Ctrl Pts',(-18.4427076638945,-14.6893541186624,
-49.4951866852561)) ;
#48705 = CARTESIAN_POINT('Ctrl Pts',(-27.103076092507,-19.6894201622032,-50.3748133147439)) ;
#48706 = CARTESIAN_POINT('Ctrl Pts',(-18.4427076638945,-14.6893541186624,
-50.3748133147439)) ;
#48707 = CARTESIAN_POINT('Ctrl Pts',(-27.1553769624387,-19.6180456661006,
-50.8437215901132)) ;
#48708 = CARTESIAN_POINT('Ctrl Pts',(-18.4950085338262,-14.6179796225598,
-50.8437215901132)) ;
#48709 = CARTESIAN_POINT('Ctrl Pts',(-27.364025659875,-19.3259492202238,-51.7059534512376)) ;
#48710 = CARTESIAN_POINT('Ctrl Pts',(-18.7036572312625,-14.325883176683,-51.7059534512376)) ;
#48711 = CARTESIAN_POINT('Ctrl Pts',(-27.5199265959608,-19.1049894709151,
-52.0993045454395)) ;
#48712 = CARTESIAN_POINT('Ctrl Pts',(-18.8595581673484,-14.1049234273743,
-52.0993045454395)) ;
#48713 = CARTESIAN_POINT('Ctrl Pts',(-27.8703439079724,-18.5900756371479,
-52.7204416622477)) ;
#48714 = CARTESIAN_POINT('Ctrl Pts',(-19.2099754793599,-13.5900095936072,
-52.7204416622477)) ;
#48715 = CARTESIAN_POINT('Ctrl Pts',(-28.088216344668,-18.2616609897393,-52.9897498710855)) ;
#48716 = CARTESIAN_POINT('Ctrl Pts',(-19.4278479160555,-13.2615949461985,
-52.9897498710855)) ;
#48717 = CARTESIAN_POINT('Ctrl Pts',(-28.5492221416873,-17.5322010777203,
-53.3470378942334)) ;
#48718 = CARTESIAN_POINT('Ctrl Pts',(-19.8888537130748,-12.5321350341795,
-53.3470378942334)) ;
#48719 = CARTESIAN_POINT('Ctrl Pts',(-28.7919452620208,-17.130887957438,-53.435)) ;
#48720 = CARTESIAN_POINT('Ctrl Pts',(-20.1315768334083,-12.1308219138972,
-53.435)) ;
#48721 = CARTESIAN_POINT('Ctrl Pts',(-29.2317567915366,-16.369112042562,-53.435)) ;
#48722 = CARTESIAN_POINT('Ctrl Pts',(-20.5713883629241,-11.3690459990212,
-53.435)) ;
#48723 = CARTESIAN_POINT('Ctrl Pts',(-29.4579425884064,-15.9582510941262,
-53.3470378942334)) ;
#48724 = CARTESIAN_POINT('Ctrl Pts',(-20.797574159794,-10.9581850505854,-53.3470378942334)) ;
#48725 = CARTESIAN_POINT('Ctrl Pts',(-29.8591705047475,-15.1942784066061,
-52.9897498710855)) ;
#48726 = CARTESIAN_POINT('Ctrl Pts',(-21.198802076135,-10.1942123630653,-52.9897498710855)) ;
#48727 = CARTESIAN_POINT('Ctrl Pts',(-30.0346497140305,-14.8413880179389,
-52.7204416622477)) ;
#48728 = CARTESIAN_POINT('Ctrl Pts',(-21.374281285418,-9.8413219743982,-52.7204416622477)) ;
#48729 = CARTESIAN_POINT('Ctrl Pts',(-30.3053695188271,-14.2804608069275,
-52.0993045454395)) ;
#48730 = CARTESIAN_POINT('Ctrl Pts',(-21.6450010902146,-9.28039476338676,
-52.0993045454395)) ;
#48731 = CARTESIAN_POINT('Ctrl Pts',(-30.4187758068994,-14.034966761149,-51.7059534512376)) ;
#48732 = CARTESIAN_POINT('Ctrl Pts',(-21.758407378287,-9.03490071760827,-51.7059534512376)) ;
#48733 = CARTESIAN_POINT('Ctrl Pts',(-30.5674144006656,-13.7082234657643,
-50.8437215901132)) ;
#48734 = CARTESIAN_POINT('Ctrl Pts',(-21.9070459720532,-8.70815742222355,
-50.8437215901132)) ;
#48735 = CARTESIAN_POINT('Ctrl Pts',(-30.603076092507,-13.6272423357121,-50.3748133147439)) ;
#48736 = CARTESIAN_POINT('Ctrl Pts',(-21.9427076638945,-8.62717629217139,
-50.3748133147439)) ;
#48737 = CARTESIAN_POINT('Ctrl Pts',(-30.603076092507,-13.6272423357121,-49.935)) ;
#48738 = CARTESIAN_POINT('Ctrl Pts',(-21.9427076638945,-8.62717629217139,
-49.935)) ;
#48739 = CARTESIAN_POINT('',(-21.9428425948598,-8.62720361368415,-49.9350000240614)) ;
#48740 = CARTESIAN_POINT('Ctrl Pts',(-30.603076092507,-13.6272423357121,-49.935)) ;
#48741 = CARTESIAN_POINT('Ctrl Pts',(-21.9428206926805,-8.62724154937146,
-49.935)) ;
#48742 = CARTESIAN_POINT('Ctrl Pts',(-21.9428425948598,-8.62720361368415,
-49.9350000240614)) ;
#48743 = CARTESIAN_POINT('Ctrl Pts',(-21.9428805819887,-8.62712893685822,
-49.7823947044339)) ;
#48744 = CARTESIAN_POINT('Ctrl Pts',(-21.9386542657645,-8.6366291223017,-49.6112134273954)) ;
#48745 = CARTESIAN_POINT('Ctrl Pts',(-21.9133010857295,-8.69338615305404,
-49.1998503646382)) ;
#48746 = CARTESIAN_POINT('Ctrl Pts',(-21.8909126068857,-8.74345822136723,
-48.9745962929387)) ;
#48747 = CARTESIAN_POINT('Ctrl Pts',(-21.7859879856397,-8.97521750159318,
-48.2662983684853)) ;
#48748 = CARTESIAN_POINT('Ctrl Pts',(-21.6743526377812,-9.21668082717488,
-47.883172642928)) ;
#48749 = CARTESIAN_POINT('Ctrl Pts',(-21.4210542707481,-9.74768131616324,
-47.2139532467367)) ;
#48750 = CARTESIAN_POINT('Ctrl Pts',(-21.2407421994177,-10.109043264305,-46.9533770888004)) ;
#48751 = CARTESIAN_POINT('Ctrl Pts',(-20.8809260516853,-10.8045105294205,
-46.5664922879644)) ;
#48752 = CARTESIAN_POINT('Ctrl Pts',(-20.6605677693207,-11.207079672144,-46.4734326225838)) ;
#48753 = CARTESIAN_POINT('Ctrl Pts',(-20.22421619988,-11.9768133402915,-46.4045524997322)) ;
#48754 = CARTESIAN_POINT('Ctrl Pts',(-19.9823208111384,-12.3775325793903,
-46.4925278051966)) ;
#48755 = CARTESIAN_POINT('Ctrl Pts',(-19.53674531479,-13.0947252120165,-46.7651000997356)) ;
#48756 = CARTESIAN_POINT('Ctrl Pts',(-19.3195722846755,-13.4244581806921,
-47.0172803610137)) ;
#48757 = CARTESIAN_POINT('Ctrl Pts',(-18.92898587425,-14.0067584166363,-47.6023005356929)) ;
#48758 = CARTESIAN_POINT('Ctrl Pts',(-18.7730192163563,-14.2274576185978,
-47.994459307398)) ;
#48759 = CARTESIAN_POINT('Ctrl Pts',(-18.6368980660828,-14.4195649649672,
-48.4438880038746)) ;
#48760 = CARTESIAN_POINT('Ctrl Pts',(-18.6029713009145,-14.4671316770788,
-48.5725202466069)) ;
#48761 = CARTESIAN_POINT('Ctrl Pts',(-18.5312735383174,-14.5672156935307,
-48.9021343175404)) ;
#48762 = CARTESIAN_POINT('Ctrl Pts',(-18.4978924906756,-14.6134280805353,
-49.1073011631897)) ;
#48763 = CARTESIAN_POINT('Ctrl Pts',(-18.4540859500186,-14.6739390087297,
-49.5238351190534)) ;
#48764 = CARTESIAN_POINT('Ctrl Pts',(-18.4428220546626,-14.6894201622032,
-49.7302427331703)) ;
#48765 = CARTESIAN_POINT('Ctrl Pts',(-18.4428220546626,-14.6894201622032,
-49.935)) ;
#48766 = CARTESIAN_POINT('Ctrl Pts',(-18.4428220546626,-14.6894201622032,
-50.1455828409762)) ;
#48767 = CARTESIAN_POINT('Ctrl Pts',(-18.4547448220837,-14.6730429870775,
-50.3651730635468)) ;
#48768 = CARTESIAN_POINT('Ctrl Pts',(-18.5289467307641,-14.570500124421,-51.0288729348248)) ;
#48769 = CARTESIAN_POINT('Ctrl Pts',(-18.6270750037497,-14.4350947680988,
-51.4570912893389)) ;
#48770 = CARTESIAN_POINT('Ctrl Pts',(-18.8501971526065,-14.1164844105032,
-52.0447545851039)) ;
#48771 = CARTESIAN_POINT('Ctrl Pts',(-18.9324055175443,-13.997966447418,-52.2259765012847)) ;
#48772 = CARTESIAN_POINT('Ctrl Pts',(-19.1105729150563,-13.7364291315622,
-52.5458841412738)) ;
#48773 = CARTESIAN_POINT('Ctrl Pts',(-19.2060075262394,-13.5945282995234,
-52.6891786697718)) ;
#48774 = CARTESIAN_POINT('Ctrl Pts',(-19.4099655089703,-13.2851421779347,
-52.9435506339987)) ;
#48775 = CARTESIAN_POINT('Ctrl Pts',(-19.5201991182455,-13.1151840940661,
-53.0578107060788)) ;
#48776 = CARTESIAN_POINT('Ctrl Pts',(-19.7408361982214,-12.7669783605705,
-53.234726969855)) ;
#48777 = CARTESIAN_POINT('Ctrl Pts',(-19.850606830195,-12.5905678298225,-53.302038394839)) ;
#48778 = CARTESIAN_POINT('Ctrl Pts',(-20.075150721414,-12.2212847287579,-53.3980021942757)) ;
#48779 = CARTESIAN_POINT('Ctrl Pts',(-20.1919384568669,-12.025163137885,-53.4280956303302)) ;
#48780 = CARTESIAN_POINT('Ctrl Pts',(-20.4031047618617,-11.6615011672705,
-53.4385899044817)) ;
#48781 = CARTESIAN_POINT('Ctrl Pts',(-20.5116747823938,-11.4715913047036,
-53.4290562483249)) ;
#48782 = CARTESIAN_POINT('Ctrl Pts',(-20.7413245752393,-11.0575569288639,
-53.3497426101657)) ;
#48783 = CARTESIAN_POINT('Ctrl Pts',(-20.8483643762666,-10.8600383333785,
-53.2913599998514)) ;
#48784 = CARTESIAN_POINT('Ctrl Pts',(-21.0459658829745,-10.4864669962478,
-53.1317914335176)) ;
#48785 = CARTESIAN_POINT('Ctrl Pts',(-21.1370078233539,-10.3104493916336,
-53.0347656954107)) ;
#48786 = CARTESIAN_POINT('Ctrl Pts',(-21.3086086447428,-9.97172965728879,
-52.8014456739528)) ;
#48787 = CARTESIAN_POINT('Ctrl Pts',(-21.3910092959937,-9.80546266232745,
-52.6636415879444)) ;
#48788 = CARTESIAN_POINT('Ctrl Pts',(-21.5277394249525,-9.52426864986341,
-52.3760206544828)) ;
#48789 = CARTESIAN_POINT('Ctrl Pts',(-21.5933835844328,-9.38719304987331,
-52.2154232168399)) ;
#48790 = CARTESIAN_POINT('Ctrl Pts',(-21.7574317326105,-9.03808378175918,
-51.6903633524324)) ;
#48791 = CARTESIAN_POINT('Ctrl Pts',(-21.8498411746536,-8.83475487377964,
-51.2863619910574)) ;
#48792 = CARTESIAN_POINT('Ctrl Pts',(-21.9233792268706,-8.67091986110646,
-50.5442029076174)) ;
#48793 = CARTESIAN_POINT('Ctrl Pts',(-21.9372892881334,-8.63966455994172,
-50.3167637435247)) ;
#48794 = CARTESIAN_POINT('Ctrl Pts',(-21.9423390183187,-8.62832720963509,
-50.0351173441301)) ;
#48795 = CARTESIAN_POINT('Ctrl Pts',(-21.9428298748233,-8.62722861931059,
-49.9861001018763)) ;
#48796 = CARTESIAN_POINT('Ctrl Pts',(-21.9428425948598,-8.62720361368415,
-49.9350000240614)) ;
#48797 = CARTESIAN_POINT('Origin',(8.66025403784439,5.,-49.935)) ;
#48798 = CARTESIAN_POINT('Ctrl Pts',(3.5,33.3166624979154,-49.935)) ;
#48799 = CARTESIAN_POINT('Ctrl Pts',(3.5,23.3165304108338,-49.935)) ;
#48800 = CARTESIAN_POINT('Ctrl Pts',(3.5,33.3166624979154,-49.4951866852561)) ;
#48801 = CARTESIAN_POINT('Ctrl Pts',(3.5,23.3165304108338,-49.4951866852561)) ;
#48802 = CARTESIAN_POINT('Ctrl Pts',(3.41203743822697,33.3262691318649,-49.0262784098868)) ;
#48803 = CARTESIAN_POINT('Ctrl Pts',(3.41203743822697,23.3261370447833,-49.0262784098868)) ;
#48804 = CARTESIAN_POINT('Ctrl Pts',(3.05475014702442,33.3609159813728,-48.1640465487623)) ;
#48805 = CARTESIAN_POINT('Ctrl Pts',(3.05475014702442,23.3607838942912,-48.1640465487623)) ;
#48806 = CARTESIAN_POINT('Ctrl Pts',(2.7854429228663,33.3854502778426,-47.7706954545604)) ;
#48807 = CARTESIAN_POINT('Ctrl Pts',(2.7854429228663,23.385318190761,-47.7706954545604)) ;
#48808 = CARTESIAN_POINT('Ctrl Pts',(2.16430580605813,33.4314636550869,-47.1495583377523)) ;
#48809 = CARTESIAN_POINT('Ctrl Pts',(2.16430580605813,23.4313315680053,-47.1495583377523)) ;
#48810 = CARTESIAN_POINT('Ctrl Pts',(1.77095416007957,33.4559393963454,-46.8802501289145)) ;
#48811 = CARTESIAN_POINT('Ctrl Pts',(1.77095416007957,23.4558073092638,-46.8802501289145)) ;
#48812 = CARTESIAN_POINT('Ctrl Pts',(0.908720446719096,33.4904521718465,-46.5229621057665)) ;
#48813 = CARTESIAN_POINT('Ctrl Pts',(0.908720446719096,23.4903200847649,-46.5229621057665)) ;
#48814 = CARTESIAN_POINT('Ctrl Pts',(0.439811529515813,33.5,-46.435)) ;
#48815 = CARTESIAN_POINT('Ctrl Pts',(0.439811529515813,23.4998679129184,-46.435)) ;
#48816 = CARTESIAN_POINT('Ctrl Pts',(-0.439811529515812,33.5,-46.435)) ;
#48817 = CARTESIAN_POINT('Ctrl Pts',(-0.439811529515812,23.4998679129184,
-46.435)) ;
#48818 = CARTESIAN_POINT('Ctrl Pts',(-0.908720446719095,33.4904521718465,
-46.5229621057665)) ;
#48819 = CARTESIAN_POINT('Ctrl Pts',(-0.908720446719095,23.4903200847649,
-46.5229621057665)) ;
#48820 = CARTESIAN_POINT('Ctrl Pts',(-1.77095416007956,33.4559393963454,-46.8802501289145)) ;
#48821 = CARTESIAN_POINT('Ctrl Pts',(-1.77095416007956,23.4558073092638,-46.8802501289145)) ;
#48822 = CARTESIAN_POINT('Ctrl Pts',(-2.16430580605813,33.4314636550869,-47.1495583377523)) ;
#48823 = CARTESIAN_POINT('Ctrl Pts',(-2.16430580605813,23.4313315680053,-47.1495583377523)) ;
#48824 = CARTESIAN_POINT('Ctrl Pts',(-2.7854429228663,33.3854502778426,-47.7706954545604)) ;
#48825 = CARTESIAN_POINT('Ctrl Pts',(-2.7854429228663,23.385318190761,-47.7706954545604)) ;
#48826 = CARTESIAN_POINT('Ctrl Pts',(-3.05475014702442,33.3609159813728,-48.1640465487623)) ;
#48827 = CARTESIAN_POINT('Ctrl Pts',(-3.05475014702442,23.3607838942912,-48.1640465487623)) ;
#48828 = CARTESIAN_POINT('Ctrl Pts',(-3.41203743822697,33.3262691318649,-49.0262784098868)) ;
#48829 = CARTESIAN_POINT('Ctrl Pts',(-3.41203743822697,23.3261370447833,-49.0262784098868)) ;
#48830 = CARTESIAN_POINT('Ctrl Pts',(-3.5,33.3166624979154,-49.4951866852561)) ;
#48831 = CARTESIAN_POINT('Ctrl Pts',(-3.5,23.3165304108338,-49.4951866852561)) ;
#48832 = CARTESIAN_POINT('Ctrl Pts',(-3.5,33.3166624979154,-50.3748133147439)) ;
#48833 = CARTESIAN_POINT('Ctrl Pts',(-3.5,23.3165304108338,-50.3748133147439)) ;
#48834 = CARTESIAN_POINT('Ctrl Pts',(-3.41203743822697,33.3262691318649,-50.8437215901132)) ;
#48835 = CARTESIAN_POINT('Ctrl Pts',(-3.41203743822697,23.3261370447833,-50.8437215901132)) ;
#48836 = CARTESIAN_POINT('Ctrl Pts',(-3.05475014702442,33.3609159813728,-51.7059534512376)) ;
#48837 = CARTESIAN_POINT('Ctrl Pts',(-3.05475014702442,23.3607838942912,-51.7059534512376)) ;
#48838 = CARTESIAN_POINT('Ctrl Pts',(-2.7854429228663,33.3854502778426,-52.0993045454395)) ;
#48839 = CARTESIAN_POINT('Ctrl Pts',(-2.7854429228663,23.385318190761,-52.0993045454395)) ;
#48840 = CARTESIAN_POINT('Ctrl Pts',(-2.16430580605813,33.4314636550869,-52.7204416622477)) ;
#48841 = CARTESIAN_POINT('Ctrl Pts',(-2.16430580605813,23.4313315680053,-52.7204416622477)) ;
#48842 = CARTESIAN_POINT('Ctrl Pts',(-1.77095416007956,33.4559393963454,-52.9897498710854)) ;
#48843 = CARTESIAN_POINT('Ctrl Pts',(-1.77095416007956,23.4558073092638,-52.9897498710854)) ;
#48844 = CARTESIAN_POINT('Ctrl Pts',(-0.908720446719096,33.4904521718465,
-53.3470378942334)) ;
#48845 = CARTESIAN_POINT('Ctrl Pts',(-0.908720446719096,23.4903200847649,
-53.3470378942334)) ;
#48846 = CARTESIAN_POINT('Ctrl Pts',(-0.439811529515812,33.5,-53.435)) ;
#48847 = CARTESIAN_POINT('Ctrl Pts',(-0.439811529515812,23.4998679129184,
-53.435)) ;
#48848 = CARTESIAN_POINT('Ctrl Pts',(0.439811529515812,33.5,-53.435)) ;
#48849 = CARTESIAN_POINT('Ctrl Pts',(0.439811529515812,23.4998679129184,-53.435)) ;
#48850 = CARTESIAN_POINT('Ctrl Pts',(0.908720446719096,33.4904521718465,-53.3470378942334)) ;
#48851 = CARTESIAN_POINT('Ctrl Pts',(0.908720446719096,23.4903200847649,-53.3470378942334)) ;
#48852 = CARTESIAN_POINT('Ctrl Pts',(1.77095416007957,33.4559393963454,-52.9897498710854)) ;
#48853 = CARTESIAN_POINT('Ctrl Pts',(1.77095416007957,23.4558073092638,-52.9897498710854)) ;
#48854 = CARTESIAN_POINT('Ctrl Pts',(2.16430580605813,33.4314636550869,-52.7204416622477)) ;
#48855 = CARTESIAN_POINT('Ctrl Pts',(2.16430580605813,23.4313315680053,-52.7204416622477)) ;
#48856 = CARTESIAN_POINT('Ctrl Pts',(2.7854429228663,33.3854502778426,-52.0993045454395)) ;
#48857 = CARTESIAN_POINT('Ctrl Pts',(2.7854429228663,23.385318190761,-52.0993045454395)) ;
#48858 = CARTESIAN_POINT('Ctrl Pts',(3.05475014702442,33.3609159813728,-51.7059534512376)) ;
#48859 = CARTESIAN_POINT('Ctrl Pts',(3.05475014702442,23.3607838942912,-51.7059534512376)) ;
#48860 = CARTESIAN_POINT('Ctrl Pts',(3.41203743822697,33.3262691318649,-50.8437215901132)) ;
#48861 = CARTESIAN_POINT('Ctrl Pts',(3.41203743822697,23.3261370447833,-50.8437215901132)) ;
#48862 = CARTESIAN_POINT('Ctrl Pts',(3.5,33.3166624979154,-50.3748133147439)) ;
#48863 = CARTESIAN_POINT('Ctrl Pts',(3.5,23.3165304108338,-50.3748133147439)) ;
#48864 = CARTESIAN_POINT('Ctrl Pts',(3.5,33.3166624979154,-49.935)) ;
#48865 = CARTESIAN_POINT('Ctrl Pts',(3.5,23.3165304108338,-49.935)) ;
#48866 = CARTESIAN_POINT('',(3.50004380435856,23.3166609252339,-49.9350000240614)) ;
#48867 = CARTESIAN_POINT('Ctrl Pts',(3.5,33.3166624979154,-49.935)) ;
#48868 = CARTESIAN_POINT('Ctrl Pts',(3.5,23.3166609252339,-49.935)) ;
#48869 = CARTESIAN_POINT('Ctrl Pts',(3.50004380435856,23.3166609252339,-49.9350000240614)) ;
#48870 = CARTESIAN_POINT('Ctrl Pts',(3.50012746995133,23.3166564846396,-49.7823947044339)) ;
#48871 = CARTESIAN_POINT('Ctrl Pts',(3.4897869099045,23.3177464801467,-49.6112134273953)) ;
#48872 = CARTESIAN_POINT('Ctrl Pts',(3.42795728941205,23.3241684975459,-49.199850364638)) ;
#48873 = CARTESIAN_POINT('Ctrl Pts',(3.37339936681084,23.3298155402716,-48.9745962929384)) ;
#48874 = CARTESIAN_POINT('Ctrl Pts',(3.12022763194928,23.3548277929032,-48.266298368485)) ;
#48875 = CARTESIAN_POINT('Ctrl Pts',(2.85529658398398,23.3788804084882,-47.8831726429277)) ;
#48876 = CARTESIAN_POINT('Ctrl Pts',(2.26878748758131,23.4250178323947,-47.2139532467363)) ;
#48877 = CARTESIAN_POINT('Ctrl Pts',(1.86568282486425,23.4495439720844,-46.9533770888)) ;
#48878 = CARTESIAN_POINT('Ctrl Pts',(1.08348243190786,23.4856676800141,-46.5664922879645)) ;
#48879 = CARTESIAN_POINT('Ctrl Pts',(0.624668186347566,23.4961163809137,-46.4734326225838)) ;
#48880 = CARTESIAN_POINT('Ctrl Pts',(-0.260116509136987,23.5030916708706,
-46.4045524997322)) ;
#48881 = CARTESIAN_POINT('Ctrl Pts',(-0.728097244352491,23.4939637387114,
-46.4925278051967)) ;
#48882 = CARTESIAN_POINT('Ctrl Pts',(-1.57199203178796,23.466680355883,-46.7651000997356)) ;
#48883 = CARTESIAN_POINT('Ctrl Pts',(-1.96613567418351,23.4434694791248,-47.0172803610138)) ;
#48884 = CARTESIAN_POINT('Ctrl Pts',(-2.66571567635337,23.3963618432954,-47.6023005356928)) ;
#48885 = CARTESIAN_POINT('Ctrl Pts',(-2.9348301207939,23.3716403563969,-47.9944593073978)) ;
#48886 = CARTESIAN_POINT('Ctrl Pts',(-3.16926053814024,23.3498096554524,-48.4438880038744)) ;
#48887 = CARTESIAN_POINT('Ctrl Pts',(-3.22741790178752,23.3442115710042,-48.5725202466068)) ;
#48888 = CARTESIAN_POINT('Ctrl Pts',(-3.34994208384615,23.3321614954266,-48.9021343175402)) ;
#48889 = CARTESIAN_POINT('Ctrl Pts',(-3.40665370878256,23.3263588536661,-49.1073011631896)) ;
#48890 = CARTESIAN_POINT('Ctrl Pts',(-3.48096098013405,23.3186767407025,-49.5238351190535)) ;
#48891 = CARTESIAN_POINT('Ctrl Pts',(-3.5,23.3166624979154,-49.7302427331703)) ;
#48892 = CARTESIAN_POINT('Ctrl Pts',(-3.5,23.3166624979154,-49.935)) ;
#48893 = CARTESIAN_POINT('Ctrl Pts',(-3.5,23.3166624979154,-50.1455828409761)) ;
#48894 = CARTESIAN_POINT('Ctrl Pts',(-3.47985556658837,23.3187993298226,-50.3651730635468)) ;
#48895 = CARTESIAN_POINT('Ctrl Pts',(-3.35394988821085,23.3317886364208,-51.0288729348247)) ;
#48896 = CARTESIAN_POINT('Ctrl Pts',(-3.18762127333464,23.3490675354948,-51.4570912893388)) ;
#48897 = CARTESIAN_POINT('Ctrl Pts',(-2.80013553531963,23.3829918057539,-52.0447545851038)) ;
#48898 = CARTESIAN_POINT('Ctrl Pts',(-2.65639178601418,23.3949273566511,-52.2259765012846)) ;
#48899 = CARTESIAN_POINT('Ctrl Pts',(-2.34081012768953,23.4184561910947,-52.5458841412736)) ;
#48900 = CARTESIAN_POINT('Ctrl Pts',(-2.17020309673431,23.4301545727601,-52.6891786697715)) ;
#48901 = CARTESIAN_POINT('Ctrl Pts',(-1.8002878644947,23.4520943063154,-52.9435506339984)) ;
#48902 = CARTESIAN_POINT('Ctrl Pts',(-1.59798304164838,23.4625803703643,-53.0578107060785)) ;
#48903 = CARTESIAN_POINT('Ctrl Pts',(-1.18610949070958,23.4795548198924,-53.234726969855)) ;
#48904 = CARTESIAN_POINT('Ctrl Pts',(-0.978448173599702,23.4864137103971,
-53.3020383948391)) ;
#48905 = CARTESIAN_POINT('Ctrl Pts',(-0.546367681279802,23.496232873925,-53.3980021942758)) ;
#48906 = CARTESIAN_POINT('Ctrl Pts',(-0.318127533626824,23.4993132242412,
-53.4280956303302)) ;
#48907 = CARTESIAN_POINT('Ctrl Pts',(0.102396123813041,23.5003576234828,-53.4385899044817)) ;
#48908 = CARTESIAN_POINT('Ctrl Pts',(0.321147899491233,23.4994270880695,-53.4290562483249)) ;
#48909 = CARTESIAN_POINT('Ctrl Pts',(0.794537083431156,23.4912924547276,-53.3497426101656)) ;
#48910 = CARTESIAN_POINT('Ctrl Pts',(1.01911310535502,23.4852323438906,-53.2913599998513)) ;
#48911 = CARTESIAN_POINT('Ctrl Pts',(1.44143612678983,23.4695745999603,-53.1317914335174)) ;
#48912 = CARTESIAN_POINT('Ctrl Pts',(1.63939281408875,23.4604104308317,-53.0347656954105)) ;
#48913 = CARTESIAN_POINT('Ctrl Pts',(2.01853311948898,23.4396612342924,-52.8014456739525)) ;
#48914 = CARTESIAN_POINT('Ctrl Pts',(2.20372488656182,23.4278887940833,-52.6636415879441)) ;
#48915 = CARTESIAN_POINT('Ctrl Pts',(2.51561110922712,23.4057035529924,-52.3760206544825)) ;
#48916 = CARTESIAN_POINT('Ctrl Pts',(2.66714414079755,23.3940152627173,-52.2154232168398)) ;
#48917 = CARTESIAN_POINT('Ctrl Pts',(3.0515057097697,23.3615304924259,-51.6903633524322)) ;
#48918 = CARTESIAN_POINT('Ctrl Pts',(3.27379843042537,23.339894962795,-51.2863619910571)) ;
#48919 = CARTESIAN_POINT('Ctrl Pts',(3.45245273953815,23.3216632778232,-50.5442029076169)) ;
#48920 = CARTESIAN_POINT('Ctrl Pts',(3.48647565498117,23.3180820936627,-50.3167637435242)) ;
#48921 = CARTESIAN_POINT('Ctrl Pts',(3.49881895345089,23.316786613132,-50.0351173441297)) ;
#48922 = CARTESIAN_POINT('Ctrl Pts',(3.50001578883256,23.3166624121724,-49.9861001018762)) ;
#48923 = CARTESIAN_POINT('Ctrl Pts',(3.50004380435856,23.3166609252339,-49.9350000240614)) ;
#48924 = CARTESIAN_POINT('Origin',(0.,-10.,-49.935)) ;
#48925 = CARTESIAN_POINT('Ctrl Pts',(16.7609414886787,-7.98064845424476,-317.752799113276)) ;
#48926 = CARTESIAN_POINT('Ctrl Pts',(15.4331208186407,-10.7693750356367,-317.792519869162)) ;
#48927 = CARTESIAN_POINT('Ctrl Pts',(11.3606506581665,-15.6667943575778,-317.87193861083)) ;
#48928 = CARTESIAN_POINT('Ctrl Pts',(2.47769983667288,-19.1925023884035,-317.991055338281)) ;
#48929 = CARTESIAN_POINT('Ctrl Pts',(-7.00582195046985,-18.0388785509995,
-318.110149295626)) ;
#48930 = CARTESIAN_POINT('Ctrl Pts',(-14.7825411735154,-12.4887043542397,
-318.229243252972)) ;
#48931 = CARTESIAN_POINT('Ctrl Pts',(-18.9557365910499,-3.89435973286506,
-318.348337210317)) ;
#48932 = CARTESIAN_POINT('Ctrl Pts',(-18.5088006439409,5.64913768061575,-318.467431167663)) ;
#48933 = CARTESIAN_POINT('Ctrl Pts',(-13.5503917473811,13.8157328865779,-318.586525125009)) ;
#48934 = CARTESIAN_POINT('Ctrl Pts',(-5.2892196625952,18.6148302662477,-318.705619082354)) ;
#48935 = CARTESIAN_POINT('Ctrl Pts',(4.26118141986884,18.8767092069171,-318.8247130397)) ;
#48936 = CARTESIAN_POINT('Ctrl Pts',(12.7729410982788,14.5375272811165,-318.943806997045)) ;
#48937 = CARTESIAN_POINT('Ctrl Pts',(18.1713965148236,6.65493323331481,-319.062900954391)) ;
#48938 = CARTESIAN_POINT('Ctrl Pts',(19.140707108569,-2.84975204642665,-319.181994911737)) ;
#48939 = CARTESIAN_POINT('Ctrl Pts',(15.4446141670581,-11.659831090839,-319.301088869082)) ;
#48940 = CARTESIAN_POINT('Ctrl Pts',(7.9840110955058,-17.6279134214656,-319.420182826427)) ;
#48941 = CARTESIAN_POINT('Ctrl Pts',(-1.42263490016496,-19.2993231591151,
-319.539276783773)) ;
#48942 = CARTESIAN_POINT('Ctrl Pts',(-10.4825243720861,-16.2666667828338,
-319.658370741119)) ;
#48943 = CARTESIAN_POINT('Ctrl Pts',(-16.9873766041342,-9.26913160922992,
-319.777464698464)) ;
#48944 = CARTESIAN_POINT('Ctrl Pts',(-19.351682444702,-0.0123147099169769,
-319.89655865581)) ;
#48945 = CARTESIAN_POINT('Ctrl Pts',(-16.9991599245348,9.24750381339812,-320.015652613156)) ;
#48946 = CARTESIAN_POINT('Ctrl Pts',(-10.5032188933883,16.2533122115955,-320.134746570501)) ;
#48947 = CARTESIAN_POINT('Ctrl Pts',(-1.44719654578774,19.2974969134576,-320.253840527847)) ;
#48948 = CARTESIAN_POINT('Ctrl Pts',(7.96156917065858,17.638060587787,-320.372934485192)) ;
#48949 = CARTESIAN_POINT('Ctrl Pts',(15.4297617489728,11.6794784702161,-320.492028442538)) ;
#48950 = CARTESIAN_POINT('Ctrl Pts',(19.1370649157766,2.87411053553889,-320.611122399883)) ;
#48951 = CARTESIAN_POINT('Ctrl Pts',(18.1798511593771,-6.63180041816628,-320.730216357229)) ;
#48952 = CARTESIAN_POINT('Ctrl Pts',(12.7914341974471,-14.5212594541618,-320.849310314575)) ;
#48953 = CARTESIAN_POINT('Ctrl Pts',(4.28520049872143,-18.8712697412915,-320.96840427192)) ;
#48954 = CARTESIAN_POINT('Ctrl Pts',(-5.26551887922155,-18.6215486975565,
-321.087498229266)) ;
#48955 = CARTESIAN_POINT('Ctrl Pts',(-13.5328072801144,-13.8329639659074,
-321.206592186611)) ;
#48956 = CARTESIAN_POINT('Ctrl Pts',(-18.5015747815521,-5.67269738003963,
-321.325686143957)) ;
#48957 = CARTESIAN_POINT('Ctrl Pts',(-18.9607213428039,3.87024690728918,-321.444780101302)) ;
#48958 = CARTESIAN_POINT('Ctrl Pts',(-14.7983334120984,12.4698473602217,-321.563874058648)) ;
#48959 = CARTESIAN_POINT('Ctrl Pts',(-7.0289620206353,18.0300154707455,-321.682968015994)) ;
#48960 = CARTESIAN_POINT('Ctrl Pts',(2.45366646868374,19.1955017080385,-321.802061973339)) ;
#48961 = CARTESIAN_POINT('Ctrl Pts',(11.3382320461671,15.6822274894264,-321.921155930684)) ;
#48962 = CARTESIAN_POINT('Ctrl Pts',(17.4591880788544,8.34652721735456,-322.04024988803)) ;
#48963 = CARTESIAN_POINT('Ctrl Pts',(19.324597160073,-1.02357684799465,-322.159343845376)) ;
#48964 = CARTESIAN_POINT('Ctrl Pts',(16.479779731245,-10.1441916865021,-322.278437802722)) ;
#48965 = CARTESIAN_POINT('Ctrl Pts',(9.61813883505806,-16.7922354173708,-322.397531760066)) ;
#48966 = CARTESIAN_POINT('Ctrl Pts',(0.412148292514622,-19.347296936467,-322.516625717413)) ;
#48967 = CARTESIAN_POINT('Ctrl Pts',(-8.89430032412952,-17.1865990442275,
-322.635719674758)) ;
#48968 = CARTESIAN_POINT('Ctrl Pts',(-16.0328295358823,-10.8367957458002,
-322.754813632104)) ;
#48969 = CARTESIAN_POINT('Ctrl Pts',(-19.2634760587788,-1.84560426302867,
-322.873907589449)) ;
#48970 = CARTESIAN_POINT('Ctrl Pts',(-17.7987938844656,7.5954395015143,-322.993001546795)) ;
#48971 = CARTESIAN_POINT('Ctrl Pts',(-11.9957883750258,15.1851515048236,-323.11209550414)) ;
#48972 = CARTESIAN_POINT('Ctrl Pts',(-3.26889886712957,19.0735960206599,-323.231189461486)) ;
#48973 = CARTESIAN_POINT('Ctrl Pts',(6.25476037288962,18.3129936831907,-323.350283418831)) ;
#48974 = CARTESIAN_POINT('Ctrl Pts',(14.2538683957045,13.0887356425588,-323.469377376177)) ;
#48975 = CARTESIAN_POINT('Ctrl Pts',(18.7787022470048,4.6741958539612,-323.588471333522)) ;
#48976 = CARTESIAN_POINT('Ctrl Pts',(18.7263674041569,-4.87964433205772,-323.707565290868)) ;
#48977 = CARTESIAN_POINT('Ctrl Pts',(14.109620094995,-13.2441075855554,-323.826659248214)) ;
#48978 = CARTESIAN_POINT('Ctrl Pts',(6.05375806237365,-18.3804183381417,-323.94575320556)) ;
#48979 = CARTESIAN_POINT('Ctrl Pts',(-3.47766237255771,-19.0366391305122,
-324.064847162905)) ;
#48980 = CARTESIAN_POINT('Ctrl Pts',(-12.1614285270647,-15.0528210360699,
-324.18394112025)) ;
#48981 = CARTESIAN_POINT('Ctrl Pts',(-17.880937130756,-7.39999001950697,-324.303035077596)) ;
#48982 = CARTESIAN_POINT('Ctrl Pts',(-19.2421005953424,2.0565334039527,-324.422129034941)) ;
#48983 = CARTESIAN_POINT('Ctrl Pts',(-15.9131454725967,11.0117921398302,-324.541222992288)) ;
#48984 = CARTESIAN_POINT('Ctrl Pts',(-8.70547975928213,17.2830086247616,-324.660316949633)) ;
#48985 = CARTESIAN_POINT('Ctrl Pts',(0.624081753732046,19.3416205868979,-324.779410906979)) ;
#48986 = CARTESIAN_POINT('Ctrl Pts',(9.80152799124969,16.6858567055935,-324.898504864324)) ;
#48987 = CARTESIAN_POINT('Ctrl Pts',(16.5899248425925,9.96303963055379,-325.01759882167)) ;
#48988 = CARTESIAN_POINT('Ctrl Pts',(19.3346511767194,0.81180591118477,-325.136692779015)) ;
#48989 = CARTESIAN_POINT('Ctrl Pts',(17.366700409186,-8.53729944774287,-325.255786736361)) ;
#48990 = CARTESIAN_POINT('Ctrl Pts',(11.1657458702521,-15.8055017042738,-325.374880693706)) ;
#48991 = CARTESIAN_POINT('Ctrl Pts',(2.24322400617006,-19.2212307363757,-325.493974651052)) ;
#48992 = CARTESIAN_POINT('Ctrl Pts',(-7.22606698817188,-17.9519280537023,
-325.613068608397)) ;
#48993 = CARTESIAN_POINT('Ctrl Pts',(-14.9340580180631,-12.3069767236302,
-325.732162565743)) ;
#48994 = CARTESIAN_POINT('Ctrl Pts',(-19.0019837262,-3.66229155476228,-325.851256523089)) ;
#48995 = CARTESIAN_POINT('Ctrl Pts',(-18.438317544,5.87504988144573,-325.970350480434)) ;
#48996 = CARTESIAN_POINT('Ctrl Pts',(-13.3804489017432,13.9803917023341,-326.08944443778)) ;
#48997 = CARTESIAN_POINT('Ctrl Pts',(-5.0611955790579,18.6781172571911,-326.208538395126)) ;
#48998 = CARTESIAN_POINT('Ctrl Pts',(4.49168643930156,18.8231909593949,-326.327632352471)) ;
#48999 = CARTESIAN_POINT('Ctrl Pts',(12.9497533696173,14.3802521754293,-326.446726309816)) ;
#49000 = CARTESIAN_POINT('Ctrl Pts',(18.2514144450072,6.43223411572022,-326.565820267162)) ;
#49001 = CARTESIAN_POINT('Ctrl Pts',(19.1044292975231,-3.08359306309894,-326.684914224507)) ;
#49002 = CARTESIAN_POINT('Ctrl Pts',(15.300881915333,-11.8478174182373,-326.804008181853)) ;
#49003 = CARTESIAN_POINT('Ctrl Pts',(7.76785862077557,-17.7242245926442,-326.923102139199)) ;
#49004 = CARTESIAN_POINT('Ctrl Pts',(-1.6585223101039,-19.2804841409582,-327.042196096544)) ;
#49005 = CARTESIAN_POINT('Ctrl Pts',(-10.6806507907074,-16.1372693988114,
-327.16129005389)) ;
#49006 = CARTESIAN_POINT('Ctrl Pts',(-17.0994502558485,-9.06071552972577,
-327.280384011235)) ;
#49007 = CARTESIAN_POINT('Ctrl Pts',(-19.3503861823524,0.22432021013761,-327.399477968581)) ;
#49008 = CARTESIAN_POINT('Ctrl Pts',(-16.8848097168634,9.45467957088808,-327.518571925927)) ;
#49009 = CARTESIAN_POINT('Ctrl Pts',(-10.30368674416,16.3805312624797,-327.637665883272)) ;
#49010 = CARTESIAN_POINT('Ctrl Pts',(-1.21111693240772,19.3137505611646,-327.756759840617)) ;
#49011 = CARTESIAN_POINT('Ctrl Pts',(8.176653603817,17.5393871274351,-327.875853797964)) ;
#49012 = CARTESIAN_POINT('Ctrl Pts',(15.5714257738071,11.4899288219582,-327.994947755309)) ;
#49013 = CARTESIAN_POINT('Ctrl Pts',(19.1707789825913,2.63988601335093,-328.114041712654)) ;
#49014 = CARTESIAN_POINT('Ctrl Pts',(18.0973977155121,-6.85360933300335,-328.23313567)) ;
#49015 = CARTESIAN_POINT('Ctrl Pts',(12.6129106553152,-14.6765884920131,-328.352229627345)) ;
#49016 = CARTESIAN_POINT('Ctrl Pts',(4.05412064094016,-18.9222586070362,-328.471323584691)) ;
#49017 = CARTESIAN_POINT('Ctrl Pts',(-5.49283105979263,-18.5557692352387,
-328.590417542037)) ;
#49018 = CARTESIAN_POINT('Ctrl Pts',(-13.7009461338816,-13.6664494291431,
-328.709511499382)) ;
#49019 = CARTESIAN_POINT('Ctrl Pts',(-18.5695577162308,-5.4460344459454,-328.828605456728)) ;
#49020 = CARTESIAN_POINT('Ctrl Pts',(-18.911978024821,4.10181083809812,-328.947699414073)) ;
#49021 = CARTESIAN_POINT('Ctrl Pts',(-14.6447446618728,12.6498703057146,-329.066793371419)) ;
#49022 = CARTESIAN_POINT('Ctrl Pts',(-6.80796395116725,18.1146181798696,-329.185887328764)) ;
#49023 = CARTESIAN_POINT('Ctrl Pts',(2.68820722530604,19.1640629010829,-329.30498128611)) ;
#49024 = CARTESIAN_POINT('Ctrl Pts',(11.5291479288101,15.5424101412383,-329.424075243456)) ;
#49025 = CARTESIAN_POINT('Ctrl Pts',(17.5599447642324,8.13241076434041,-329.543169200801)) ;
#49026 = CARTESIAN_POINT('Ctrl Pts',(19.3106359571767,-1.25980311646076,-329.662263158147)) ;
#49027 = CARTESIAN_POINT('Ctrl Pts',(16.3545035792121,-10.3449493783388,-329.781357115492)) ;
#49028 = CARTESIAN_POINT('Ctrl Pts',(9.41208286212398,-16.9085913416631,-329.900451072838)) ;
#49029 = CARTESIAN_POINT('Ctrl Pts',(0.175537106117643,-19.3508902039991,
-330.019545030184)) ;
#49030 = CARTESIAN_POINT('Ctrl Pts',(-9.10379451103152,-17.0765538228228,
-330.138638987529)) ;
#49031 = CARTESIAN_POINT('Ctrl Pts',(-16.1641440768252,-10.6399347378867,
-330.257732944874)) ;
#49032 = CARTESIAN_POINT('Ctrl Pts',(-19.2846040132411,-1.60991087186129,
-330.376826902221)) ;
#49033 = CARTESIAN_POINT('Ctrl Pts',(-17.7045854710373,7.81251676872362,-330.495920859566)) ;
#49034 = CARTESIAN_POINT('Ctrl Pts',(-11.80920619224,15.330701682311,-330.615014816912)) ;
#49035 = CARTESIAN_POINT('Ctrl Pts',(-3.03542093123559,19.1121423376101,-330.734108774257)) ;
#49036 = CARTESIAN_POINT('Ctrl Pts',(6.47822555538839,18.2351407621758,-330.853202731602)) ;
#49037 = CARTESIAN_POINT('Ctrl Pts',(14.4128528523085,12.9134595527517,-330.972296688948)) ;
#49038 = CARTESIAN_POINT('Ctrl Pts',(18.8344547015049,4.44421883572467,-331.091390646294)) ;
#49039 = CARTESIAN_POINT('Ctrl Pts',(18.6652986113538,-5.10826709480303,-331.210484603639)) ;
#49040 = CARTESIAN_POINT('Ctrl Pts',(13.9466151179208,-13.4156509985701,-331.329578560985)) ;
#49041 = CARTESIAN_POINT('Ctrl Pts',(5.82854814913269,-18.4530699732075,-331.44867251833)) ;
#49042 = CARTESIAN_POINT('Ctrl Pts',(-3.71018398435288,-18.9926906931352,
-331.567766475676)) ;
#49043 = CARTESIAN_POINT('Ctrl Pts',(-12.3445864277812,-14.9029846302641,
-331.686860433021)) ;
#49044 = CARTESIAN_POINT('Ctrl Pts',(-17.9700879473739,-7.18078715229037,
-331.805954390367)) ;
#49045 = CARTESIAN_POINT('Ctrl Pts',(-19.2155144808514,2.2916736676591,-331.925048347713)) ;
#49046 = CARTESIAN_POINT('Ctrl Pts',(-15.7773025942279,11.20555611351,-332.044142305059)) ;
#49047 = CARTESIAN_POINT('Ctrl Pts',(-8.49349080604967,17.3881677841687,-332.163236262404)) ;
#49048 = CARTESIAN_POINT('Ctrl Pts',(0.860546054667159,19.3325431707949,-332.282330219749)) ;
#49049 = CARTESIAN_POINT('Ctrl Pts',(10.0048312291659,16.5647552664916,-332.401424177095)) ;
#49050 = CARTESIAN_POINT('Ctrl Pts',(16.710513368693,9.75943174153013,-332.520518134441)) ;
#49051 = CARTESIAN_POINT('Ctrl Pts',(19.3431324366477,0.57531947747291,-332.639612091786)) ;
#49052 = CARTESIAN_POINT('Ctrl Pts',(17.2610071590549,-8.74902262072224,-332.758706049132)) ;
#49053 = CARTESIAN_POINT('Ctrl Pts',(10.9716400519316,-15.9408556713152,-332.877800006477)) ;
#49054 = CARTESIAN_POINT('Ctrl Pts',(2.00801746598928,-19.2472239769566,-332.996893963823)) ;
#49055 = CARTESIAN_POINT('Ctrl Pts',(-7.44504440929992,-17.8622249091877,
-333.115987921168)) ;
#49056 = CARTESIAN_POINT('Ctrl Pts',(-15.0834322060208,-12.1234416668381,
-333.235081878514)) ;
#49057 = CARTESIAN_POINT('Ctrl Pts',(-19.0453458361247,-3.42965988769476,
-333.35417583586)) ;
#49058 = CARTESIAN_POINT('Ctrl Pts',(-18.3650983848235,6.10007592400356,-333.473269793205)) ;
#49059 = CARTESIAN_POINT('Ctrl Pts',(-13.2084950977309,14.1429636998782,-333.592363750551)) ;
#49060 = CARTESIAN_POINT('Ctrl Pts',(-4.83241958817477,18.7386094971499,-333.711457707896)) ;
#49061 = CARTESIAN_POINT('Ctrl Pts',(4.7215221745996,18.7668589091946,-333.830551665242)) ;
#49062 = CARTESIAN_POINT('Ctrl Pts',(13.1246281020728,14.2208263524006,-333.949645622587)) ;
#49063 = CARTESIAN_POINT('Ctrl Pts',(18.3287037621201,6.2085733758486,-334.068739579933)) ;
#49064 = CARTESIAN_POINT('Ctrl Pts',(19.0652945043705,-3.31697308166238,-334.187833537278)) ;
#49065 = CARTESIAN_POINT('Ctrl Pts',(15.1548618260305,-12.0340320756082,-334.306927494624)) ;
#49066 = CARTESIAN_POINT('Ctrl Pts',(7.55054454364082,-17.8178854541545,-334.42602145197)) ;
#49067 = CARTESIAN_POINT('Ctrl Pts',(-1.89416168865372,-19.2587620697709,
-334.545115409315)) ;
#49068 = CARTESIAN_POINT('Ctrl Pts',(-10.8771801286315,-16.0054589878645,
-334.664209366661)) ;
#49069 = CARTESIAN_POINT('Ctrl Pts',(-17.2089669919832,-8.85094458414816,
-334.783303324007)) ;
#49070 = CARTESIAN_POINT('Ctrl Pts',(-19.3461964286075,0.460921585997261,
-334.902397281352)) ;
#49071 = CARTESIAN_POINT('Ctrl Pts',(-16.7679346944988,9.66044155535967,-335.021491238698)) ;
#49072 = CARTESIAN_POINT('Ctrl Pts',(-10.1026138686454,16.5053009055333,-335.140585196043)) ;
#49073 = CARTESIAN_POINT('Ctrl Pts',(-0.974856218396629,19.3271161925352,
-335.259679153389)) ;
#49074 = CARTESIAN_POINT('Ctrl Pts',(8.39051536853628,17.4380909737272,-335.378773110734)) ;
#49075 = CARTESIAN_POINT('Ctrl Pts',(15.7107613779483,11.2986610663483,-335.49786706808)) ;
#49076 = CARTESIAN_POINT('Ctrl Pts',(19.2016264118602,2.4052667439143,-335.616961025425)) ;
#49077 = CARTESIAN_POINT('Ctrl Pts',(18.0122381377377,-7.07439341485539,-335.736054982772)) ;
#49078 = CARTESIAN_POINT('Ctrl Pts',(12.4325010853337,-14.8297229190515,-335.855148940116)) ;
#49079 = CARTESIAN_POINT('Ctrl Pts',(3.82243456137157,-18.9704179897003,-335.974242897462)) ;
#49080 = CARTESIAN_POINT('Ctrl Pts',(-5.71932188314611,-18.4872151129394,
-336.093336854808)) ;
#49081 = CARTESIAN_POINT('Ctrl Pts',(-13.86703627375,-13.4978912961108,-336.212430812153)) ;
#49082 = CARTESIAN_POINT('Ctrl Pts',(-18.6347638921671,-5.21855721929272,
-336.331524769499)) ;
#49083 = CARTESIAN_POINT('Ctrl Pts',(-18.8604068147111,4.3327615466108,-336.450618726845)) ;
#49084 = CARTESIAN_POINT('Ctrl Pts',(-14.4889659622868,12.8280014299124,-336.56971268419)) ;
#49085 = CARTESIAN_POINT('Ctrl Pts',(-6.585948076489,18.1965127310871,-336.688806641536)) ;
#49086 = CARTESIAN_POINT('Ctrl Pts',(2.92234642591305,19.1297573198475,-336.807900598881)) ;
#49087 = CARTESIAN_POINT('Ctrl Pts',(11.7183389770801,15.4002710753346,-336.926994556227)) ;
#49088 = CARTESIAN_POINT('Ctrl Pts',(17.6580774691844,7.91707335905638,-337.046088513572)) ;
#49089 = CARTESIAN_POINT('Ctrl Pts',(19.2937835006079,-1.49583085020681,-337.165182470918)) ;
#49090 = CARTESIAN_POINT('Ctrl Pts',(16.2267895858379,-10.544181217555,-337.284276428263)) ;
#49091 = CARTESIAN_POINT('Ctrl Pts',(9.20460358311207,-17.0223752841955,-337.403370385609)) ;
#49092 = CARTESIAN_POINT('Ctrl Pts',(-0.0610673351825857,-19.3516803088222,
-337.522464342955)) ;
#49093 = CARTESIAN_POINT('Ctrl Pts',(-9.31199539433652,-16.9637679291851,
-337.6415583003)) ;
#49094 = CARTESIAN_POINT('Ctrl Pts',(-16.2928939482416,-10.4418748891603,
-337.760652257646)) ;
#49095 = CARTESIAN_POINT('Ctrl Pts',(-19.3035682799848,-1.37177778166763,
-337.879764674221)) ;
#49096 = CARTESIAN_POINT('Ctrl Pts',(-18.1711237806586,4.89578622149652,-337.959179105016)) ;
#49097 = CARTESIAN_POINT('Ctrl Pts',(-16.8891883469502,7.70553220148658,-337.998895550028)) ;
#49098 = CARTESIAN_POINT('Ctrl Pts',(17.0212170400392,-8.10457751145466,-317.919234059516)) ;
#49099 = CARTESIAN_POINT('Ctrl Pts',(15.6727770475582,-10.9366093778782,-317.958954815403)) ;
#49100 = CARTESIAN_POINT('Ctrl Pts',(11.5370667393196,-15.9100792316539,-318.038373557071)) ;
#49101 = CARTESIAN_POINT('Ctrl Pts',(2.51617528219197,-19.4905369077951,-318.157490284521)) ;
#49102 = CARTESIAN_POINT('Ctrl Pts',(-7.11461322404616,-18.318998797464,-318.276584241867)) ;
#49103 = CARTESIAN_POINT('Ctrl Pts',(-15.0120947494314,-12.6826376373893,
-318.395678199212)) ;
#49104 = CARTESIAN_POINT('Ctrl Pts',(-19.2500944465446,-3.95483405809031,
-318.514772156558)) ;
#49105 = CARTESIAN_POINT('Ctrl Pts',(-18.7962181673464,5.7368614177057,-318.633866113904)) ;
#49106 = CARTESIAN_POINT('Ctrl Pts',(-13.7608116504385,14.0302731913054,-318.752960071249)) ;
#49107 = CARTESIAN_POINT('Ctrl Pts',(-5.37135434249244,18.9038942913386,-318.872054028595)) ;
#49108 = CARTESIAN_POINT('Ctrl Pts',(4.3273520072581,19.1698398702525,-318.99114798594)) ;
#49109 = CARTESIAN_POINT('Ctrl Pts',(12.9712882071864,14.7632761109818,-319.110241943286)) ;
#49110 = CARTESIAN_POINT('Ctrl Pts',(18.4535745923546,6.75827566295925,-319.229335900631)) ;
#49111 = CARTESIAN_POINT('Ctrl Pts',(19.4379373148482,-2.89400497730318,-319.348429857977)) ;
#49112 = CARTESIAN_POINT('Ctrl Pts',(15.6844488726799,-11.8408930537357,-319.467523815322)) ;
#49113 = CARTESIAN_POINT('Ctrl Pts',(8.1079923701469,-17.9016519157027,-319.586617772668)) ;
#49114 = CARTESIAN_POINT('Ctrl Pts',(-1.44472656388653,-19.5990164656943,
-319.705711730014)) ;
#49115 = CARTESIAN_POINT('Ctrl Pts',(-10.6453042978102,-16.5192668929505,
-319.824805687359)) ;
#49116 = CARTESIAN_POINT('Ctrl Pts',(-17.2511683973814,-9.41306912860228,
-319.943899644705)) ;
#49117 = CARTESIAN_POINT('Ctrl Pts',(-19.652188822667,-0.0125059412935629,
-320.06299360205)) ;
#49118 = CARTESIAN_POINT('Ctrl Pts',(-17.2631346973726,9.39110548132147,-320.182087559396)) ;
#49119 = CARTESIAN_POINT('Ctrl Pts',(-10.6663201780257,16.505704942646,-320.301181516741)) ;
#49120 = CARTESIAN_POINT('Ctrl Pts',(-1.46966961981743,19.5971618608248,-320.420275474087)) ;
#49121 = CARTESIAN_POINT('Ctrl Pts',(8.08520195148935,17.9119566542768,-320.539369431433)) ;
#49122 = CARTESIAN_POINT('Ctrl Pts',(15.6693658159213,11.8608455312784,-320.658463388778)) ;
#49123 = CARTESIAN_POINT('Ctrl Pts',(19.434238563554,2.918741721968,-320.777557346124)) ;
#49124 = CARTESIAN_POINT('Ctrl Pts',(18.4621605265063,-6.73478362537551,-320.896651303469)) ;
#49125 = CARTESIAN_POINT('Ctrl Pts',(12.9900684800548,-14.7467556659011,-321.015745260815)) ;
#49126 = CARTESIAN_POINT('Ctrl Pts',(4.35174407106482,-19.1643159368233,-321.134839218161)) ;
#49127 = CARTESIAN_POINT('Ctrl Pts',(-5.34728551687813,-18.9107170511193,
-321.253933175506)) ;
#49128 = CARTESIAN_POINT('Ctrl Pts',(-13.7429541193398,-14.0477718468136,
-321.373027132851)) ;
#49129 = CARTESIAN_POINT('Ctrl Pts',(-18.7888800967433,-5.7607869685206,-321.492121090197)) ;
#49130 = CARTESIAN_POINT('Ctrl Pts',(-19.2551566049893,3.93034679179602,-321.611215047543)) ;
#49131 = CARTESIAN_POINT('Ctrl Pts',(-15.0281322208737,12.6634878188591,-321.730309004888)) ;
#49132 = CARTESIAN_POINT('Ctrl Pts',(-7.13811262930777,18.3099980851382,-321.849402962234)) ;
#49133 = CARTESIAN_POINT('Ctrl Pts',(2.49176870735705,19.4935828029504,-321.968496919579)) ;
#49134 = CARTESIAN_POINT('Ctrl Pts',(11.5142999955279,15.9257520199028,-322.087590876925)) ;
#49135 = CARTESIAN_POINT('Ctrl Pts',(17.7303064886763,8.47613789435082,-322.206684834271)) ;
#49136 = CARTESIAN_POINT('Ctrl Pts',(19.6246829389091,-1.03947166086367,-322.325778791616)) ;
#49137 = CARTESIAN_POINT('Ctrl Pts',(16.7356892073772,-10.3017177470814,-322.444872748962)) ;
#49138 = CARTESIAN_POINT('Ctrl Pts',(9.76749598125699,-17.0529969226109,-322.563966706307)) ;
#49139 = CARTESIAN_POINT('Ctrl Pts',(0.418548417719366,-19.6477352132116,
-322.683060663653)) ;
#49140 = CARTESIAN_POINT('Ctrl Pts',(-9.03241720273038,-17.4534845020206,
-322.802154620998)) ;
#49141 = CARTESIAN_POINT('Ctrl Pts',(-16.2817984586686,-11.0050770436988,
-322.921248578344)) ;
#49142 = CARTESIAN_POINT('Ctrl Pts',(-19.5626127066636,-1.874264089058,-323.04034253569)) ;
#49143 = CARTESIAN_POINT('Ctrl Pts',(-18.0751859293253,7.71338676631542,-323.159436493035)) ;
#49144 = CARTESIAN_POINT('Ctrl Pts',(-12.1820673161834,15.4209570938522,-323.278530450381)) ;
#49145 = CARTESIAN_POINT('Ctrl Pts',(-3.31966060122183,19.3697840793114,-323.397624407726)) ;
#49146 = CARTESIAN_POINT('Ctrl Pts',(6.35188864016391,18.5973705799881,-323.516718365072)) ;
#49147 = CARTESIAN_POINT('Ctrl Pts',(14.4752123732022,13.2919866286851,-323.635812322417)) ;
#49148 = CARTESIAN_POINT('Ctrl Pts',(19.070310990134,4.74678001660378,-323.754906279763)) ;
#49149 = CARTESIAN_POINT('Ctrl Pts',(19.0171634554639,-4.95541884149247,-323.874000237108)) ;
#49150 = CARTESIAN_POINT('Ctrl Pts',(14.3287240846003,-13.4497712952244,-323.993094194454)) ;
#49151 = CARTESIAN_POINT('Ctrl Pts',(6.14776502603686,-18.6658422518537,-324.1121881518)) ;
#49152 = CARTESIAN_POINT('Ctrl Pts',(-3.53166593149108,-19.3322532968818,
-324.231282109145)) ;
#49153 = CARTESIAN_POINT('Ctrl Pts',(-12.3502796436532,-15.2865717055856,
-324.350376066491)) ;
#49154 = CARTESIAN_POINT('Ctrl Pts',(-18.1586047530488,-7.51490220887834,
-324.469470023836)) ;
#49155 = CARTESIAN_POINT('Ctrl Pts',(-19.5409053101712,2.08846868431664,-324.588563981182)) ;
#49156 = CARTESIAN_POINT('Ctrl Pts',(-16.160255858046,11.1827909033899,-324.707657938528)) ;
#49157 = CARTESIAN_POINT('Ctrl Pts',(-8.84066450088723,17.5513911975433,-324.826751895873)) ;
#49158 = CARTESIAN_POINT('Ctrl Pts',(0.633772929055101,19.6419707173401,-324.945845853219)) ;
#49159 = CARTESIAN_POINT('Ctrl Pts',(9.953732931755,16.9449662882446,-325.064939810564)) ;
#49160 = CARTESIAN_POINT('Ctrl Pts',(16.8475447285846,10.1177526360744,-325.18403376791)) ;
#49161 = CARTESIAN_POINT('Ctrl Pts',(19.6348930813154,0.82441219772747,-325.303127725255)) ;
#49162 = CARTESIAN_POINT('Ctrl Pts',(17.6363826061774,-8.66987256855422,-325.422221682601)) ;
#49163 = CARTESIAN_POINT('Ctrl Pts',(11.3391353343638,-16.0509405224563,-325.541315639947)) ;
#49164 = CARTESIAN_POINT('Ctrl Pts',(2.27805834798945,-19.5197113695261,-325.660409597292)) ;
#49165 = CARTESIAN_POINT('Ctrl Pts',(-7.33827837980427,-18.2306980723983,
-325.779503554638)) ;
#49166 = CARTESIAN_POINT('Ctrl Pts',(-15.1659644528732,-12.4980880137978,
-325.898597511983)) ;
#49167 = CARTESIAN_POINT('Ctrl Pts',(-19.2970597393595,-3.71916216398806,
-326.017691469329)) ;
#49168 = CARTESIAN_POINT('Ctrl Pts',(-18.7246405568311,5.96628174024054,-326.136785426674)) ;
#49169 = CARTESIAN_POINT('Ctrl Pts',(-13.5882298141522,14.1974889436208,-326.25587938402)) ;
#49170 = CARTESIAN_POINT('Ctrl Pts',(-5.13978934246745,18.9681640466733,-326.374973341366)) ;
#49171 = CARTESIAN_POINT('Ctrl Pts',(4.56143646887577,19.1154905541777,-326.494067298711)) ;
#49172 = CARTESIAN_POINT('Ctrl Pts',(13.1508461423911,14.6035587281184,-326.613161256057)) ;
#49173 = CARTESIAN_POINT('Ctrl Pts',(18.5348350965852,6.53211831864999,-326.732255213402)) ;
#49174 = CARTESIAN_POINT('Ctrl Pts',(19.4010961567326,-3.13147723984469,-326.851349170748)) ;
#49175 = CARTESIAN_POINT('Ctrl Pts',(15.5384846466298,-12.0317985635109,-326.970443128093)) ;
#49176 = CARTESIAN_POINT('Ctrl Pts',(7.88848332952349,-17.9994586737014,-327.089537085439)) ;
#49177 = CARTESIAN_POINT('Ctrl Pts',(-1.68427699751195,-19.5798849021668,
-327.208631042785)) ;
#49178 = CARTESIAN_POINT('Ctrl Pts',(-10.8465073611941,-16.3878601363941,
-327.32772500013)) ;
#49179 = CARTESIAN_POINT('Ctrl Pts',(-17.3649824066712,-9.20141661932822,
-327.446818957476)) ;
#49180 = CARTESIAN_POINT('Ctrl Pts',(-19.6508724310546,0.227803610304238,
-327.565912914822)) ;
#49181 = CARTESIAN_POINT('Ctrl Pts',(-17.1470087801823,9.60149840799883,-327.685006872167)) ;
#49182 = CARTESIAN_POINT('Ctrl Pts',(-10.4636895548728,16.634899539393,-327.804100829513)) ;
#49183 = CARTESIAN_POINT('Ctrl Pts',(-1.22992399808227,19.6136679064725,-327.923194786858)) ;
#49184 = CARTESIAN_POINT('Ctrl Pts',(8.30362636524895,17.8117509238366,-328.042288744204)) ;
#49185 = CARTESIAN_POINT('Ctrl Pts',(15.8132296982158,11.6683524243107,-328.161382701549)) ;
#49186 = CARTESIAN_POINT('Ctrl Pts',(19.4684761658357,2.68087999857057,-328.280476658895)) ;
#49187 = CARTESIAN_POINT('Ctrl Pts',(18.3784266882447,-6.96003694323999,-328.39957061624)) ;
#49188 = CARTESIAN_POINT('Ctrl Pts',(12.808772700254,-14.9044967610342,-328.518664573586)) ;
#49189 = CARTESIAN_POINT('Ctrl Pts',(4.11707584460909,-19.2160965931217,-328.637758530931)) ;
#49190 = CARTESIAN_POINT('Ctrl Pts',(-5.57812755901271,-18.8439161195818,
-328.756852488277)) ;
#49191 = CARTESIAN_POINT('Ctrl Pts',(-13.9137039501156,-13.8786715565644,
-328.875946445623)) ;
#49192 = CARTESIAN_POINT('Ctrl Pts',(-18.8579187176923,-5.53060425481351,
-328.995040402968)) ;
#49193 = CARTESIAN_POINT('Ctrl Pts',(-19.2056563668791,4.16550660830191,-329.114134360314)) ;
#49194 = CARTESIAN_POINT('Ctrl Pts',(-14.8721584377622,12.8463062857986,-329.23322831766)) ;
#49195 = CARTESIAN_POINT('Ctrl Pts',(-6.91368274818291,18.395914563944,-329.352322275005)) ;
#49196 = CARTESIAN_POINT('Ctrl Pts',(2.72995157589699,19.4616557923449,-329.471416232351)) ;
#49197 = CARTESIAN_POINT('Ctrl Pts',(11.7081805527181,15.7837634907333,-329.590510189696)) ;
#49198 = CARTESIAN_POINT('Ctrl Pts',(17.8326277939093,8.25869649220413,-329.709604147042)) ;
#49199 = CARTESIAN_POINT('Ctrl Pts',(19.6105049367488,-1.27936621504706,-329.828698104387)) ;
#49200 = CARTESIAN_POINT('Ctrl Pts',(16.6084676801657,-10.5055929439203,-329.947792061733)) ;
#49201 = CARTESIAN_POINT('Ctrl Pts',(9.55824022792855,-17.1711597025844,-330.066886019078)) ;
#49202 = CARTESIAN_POINT('Ctrl Pts',(0.178262968331908,-19.6513842794997,
-330.185979976424)) ;
#49203 = CARTESIAN_POINT('Ctrl Pts',(-9.24516456100345,-17.3417304219163,
-330.305073933769)) ;
#49204 = CARTESIAN_POINT('Ctrl Pts',(-16.4151521430909,-10.8051590412002,
-330.424167891115)) ;
#49205 = CARTESIAN_POINT('Ctrl Pts',(-19.5840687506908,-1.63491068706249,
-330.54326184846)) ;
#49206 = CARTESIAN_POINT('Ctrl Pts',(-17.9795145821613,7.93383496023844,-330.662355805807)) ;
#49207 = CARTESIAN_POINT('Ctrl Pts',(-11.9925877555544,15.5687674756795,-330.781449763152)) ;
#49208 = CARTESIAN_POINT('Ctrl Pts',(-3.08255705762935,19.408928970268,-330.900543720498)) ;
#49209 = CARTESIAN_POINT('Ctrl Pts',(6.57882394536576,18.5183087046937,-331.019637677843)) ;
#49210 = CARTESIAN_POINT('Ctrl Pts',(14.6366656509717,13.1139887299065,-331.138731635189)) ;
#49211 = CARTESIAN_POINT('Ctrl Pts',(19.1269292075056,4.51323175535192,-331.257825592534)) ;
#49212 = CARTESIAN_POINT('Ctrl Pts',(18.9551463439922,-5.18759181743238,-331.37691954988)) ;
#49213 = CARTESIAN_POINT('Ctrl Pts',(14.1631878529239,-13.6239785536106,-331.496013507225)) ;
#49214 = CARTESIAN_POINT('Ctrl Pts',(5.91905789670097,-18.739622072015,-331.615107464571)) ;
#49215 = CARTESIAN_POINT('Ctrl Pts',(-3.76779830051932,-19.287622397617,-331.734201421916)) ;
#49216 = CARTESIAN_POINT('Ctrl Pts',(-12.5362817475804,-15.1344085359069,
-331.853295379262)) ;
#49217 = CARTESIAN_POINT('Ctrl Pts',(-18.2491399655233,-7.29229540715344,
-331.972389336607)) ;
#49218 = CARTESIAN_POINT('Ctrl Pts',(-19.5139063480122,2.32726036950342,-332.091483293954)) ;
#49219 = CARTESIAN_POINT('Ctrl Pts',(-16.0223035170261,11.3795637787544,-332.210577251299)) ;
#49220 = CARTESIAN_POINT('Ctrl Pts',(-8.62538363581782,17.6581833414827,-332.329671208644)) ;
#49221 = CARTESIAN_POINT('Ctrl Pts',(0.873909212041135,19.6327523408094,-332.44876516599)) ;
#49222 = CARTESIAN_POINT('Ctrl Pts',(10.1601932036826,16.8219843018086,-332.567859123336)) ;
#49223 = CARTESIAN_POINT('Ctrl Pts',(16.9700058371495,9.91098298220524,-332.686953080681)) ;
#49224 = CARTESIAN_POINT('Ctrl Pts',(19.6435060441439,0.584253438271538,-332.806047038027)) ;
#49225 = CARTESIAN_POINT('Ctrl Pts',(17.5290480777822,-8.88488352614997,-332.925140995372)) ;
#49226 = CARTESIAN_POINT('Ctrl Pts',(11.1420153059574,-16.1883963599938,-333.044234952718)) ;
#49227 = CARTESIAN_POINT('Ctrl Pts',(2.03919935714112,-19.5461082512168,-333.163328910063)) ;
#49228 = CARTESIAN_POINT('Ctrl Pts',(-7.56065623455701,-18.1396019550955,
-333.282422867409)) ;
#49229 = CARTESIAN_POINT('Ctrl Pts',(-15.317658227064,-12.3117028970533,-333.401516824754)) ;
#49230 = CARTESIAN_POINT('Ctrl Pts',(-19.3410952062716,-3.4829180306727,-333.5206107821)) ;
#49231 = CARTESIAN_POINT('Ctrl Pts',(-18.6502843996501,6.19480214362151,-333.639704739446)) ;
#49232 = CARTESIAN_POINT('Ctrl Pts',(-13.4136057919318,14.3625854721601,-333.758798696791)) ;
#49233 = CARTESIAN_POINT('Ctrl Pts',(-4.9074607589567,19.0295956521874,-333.877892654137)) ;
#49234 = CARTESIAN_POINT('Ctrl Pts',(4.79484125324946,19.0582837407409,-333.996986611482)) ;
#49235 = CARTESIAN_POINT('Ctrl Pts',(13.3284364512622,14.4416572300797,-334.116080568828)) ;
#49236 = CARTESIAN_POINT('Ctrl Pts',(18.6133246159446,6.30498441932446,-334.235174526174)) ;
#49237 = CARTESIAN_POINT('Ctrl Pts',(19.3613536513061,-3.36848134557823,-334.354268483519)) ;
#49238 = CARTESIAN_POINT('Ctrl Pts',(15.3901970558699,-12.2209048915347,-334.473362440865)) ;
#49239 = CARTESIAN_POINT('Ctrl Pts',(7.66779464832591,-18.0945739661805,-334.59245639821)) ;
#49240 = CARTESIAN_POINT('Ctrl Pts',(-1.92357554814441,-19.5578255155574,
-334.711550355556)) ;
#49241 = CARTESIAN_POINT('Ctrl Pts',(-11.0460885433012,-16.2540028817536,
-334.830644312901)) ;
#49242 = CARTESIAN_POINT('Ctrl Pts',(-17.4761997948187,-8.98838820467845,
-334.949738270247)) ;
#49243 = CARTESIAN_POINT('Ctrl Pts',(-19.6466176159009,0.468079096809521,
-335.068832227593)) ;
#49244 = CARTESIAN_POINT('Ctrl Pts',(-17.0283188412208,9.81045560760757,-335.187926184938)) ;
#49245 = CARTESIAN_POINT('Ctrl Pts',(-10.2594942799648,16.7616066922016,-335.307020142284)) ;
#49246 = CARTESIAN_POINT('Ctrl Pts',(-0.989994463459544,19.6272410886586,
-335.426114099629)) ;
#49247 = CARTESIAN_POINT('Ctrl Pts',(8.52080912412389,17.7088817730344,-335.545208056975)) ;
#49248 = CARTESIAN_POINT('Ctrl Pts',(15.9547290024818,11.4741145300255,-335.66430201432)) ;
#49249 = CARTESIAN_POINT('Ctrl Pts',(19.4998026154309,2.44261739801477,-335.783395971666)) ;
#49250 = CARTESIAN_POINT('Ctrl Pts',(18.2919446933451,-7.18424951380041,-335.902489929011)) ;
#49251 = CARTESIAN_POINT('Ctrl Pts',(12.6255616050522,-15.0600091659121,-336.021583886357)) ;
#49252 = CARTESIAN_POINT('Ctrl Pts',(3.8817919825327,-19.2650038281594,-336.140677843703)) ;
#49253 = CARTESIAN_POINT('Ctrl Pts',(-5.80813548932383,-18.7742974412137,
-336.259771801048)) ;
#49254 = CARTESIAN_POINT('Ctrl Pts',(-14.0823732531388,-13.7074959356636,
-336.378865758394)) ;
#49255 = CARTESIAN_POINT('Ctrl Pts',(-18.9241374604587,-5.29959460364702,
-336.49795971574)) ;
#49256 = CARTESIAN_POINT('Ctrl Pts',(-19.1532843231671,4.40004367996941,-336.617053673085)) ;
#49257 = CARTESIAN_POINT('Ctrl Pts',(-14.7139606982344,13.0272035539266,-336.736147630431)) ;
#49258 = CARTESIAN_POINT('Ctrl Pts',(-6.68821925666094,18.4790808306846,-336.855241587776)) ;
#49259 = CARTESIAN_POINT('Ctrl Pts',(2.96772665278063,19.4268174901953,-336.974335545122)) ;
#49260 = CARTESIAN_POINT('Ctrl Pts',(11.9003094911082,15.6394171906014,-337.093429502467)) ;
#49261 = CARTESIAN_POINT('Ctrl Pts',(17.932284371724,8.0400151779919,-337.212523459813)) ;
#49262 = CARTESIAN_POINT('Ctrl Pts',(19.5933907835188,-1.51905915152522,-337.331617417158)) ;
#49263 = CARTESIAN_POINT('Ctrl Pts',(16.4787704551177,-10.7079185936385,-337.450711374504)) ;
#49264 = CARTESIAN_POINT('Ctrl Pts',(9.34753906643606,-17.2867105612771,-337.569805331849)) ;
#49265 = CARTESIAN_POINT('Ctrl Pts',(-0.0620156312162582,-19.6521866536198,
-337.688899289195)) ;
#49266 = CARTESIAN_POINT('Ctrl Pts',(-9.45659853236213,-17.2271931105152,
-337.807993246541)) ;
#49267 = CARTESIAN_POINT('Ctrl Pts',(-16.5459013320153,-10.6040235814547,
-337.927087203886)) ;
#49268 = CARTESIAN_POINT('Ctrl Pts',(-19.603327507752,-1.39307970069821,-338.046199620463)) ;
#49269 = CARTESIAN_POINT('Ctrl Pts',(-18.4532976229839,4.97181139341203,-338.125614051257)) ;
#49270 = CARTESIAN_POINT('Ctrl Pts',(-17.1514554046811,7.82518906226747,-338.165330496269)) ;
#49271 = CARTESIAN_POINT('Ctrl Pts',(17.2814925913997,-8.22850656866457,-318.085669005756)) ;
#49272 = CARTESIAN_POINT('Ctrl Pts',(15.9124332764758,-11.1038437201197,-318.125389761643)) ;
#49273 = CARTESIAN_POINT('Ctrl Pts',(11.7134828204727,-16.15336410573,-318.204808503311)) ;
#49274 = CARTESIAN_POINT('Ctrl Pts',(2.55465072771105,-19.7885714271867,-318.323925230762)) ;
#49275 = CARTESIAN_POINT('Ctrl Pts',(-7.22340449762248,-18.5991190439285,
-318.443019188107)) ;
#49276 = CARTESIAN_POINT('Ctrl Pts',(-15.2416483253474,-12.8765709205389,
-318.562113145453)) ;
#49277 = CARTESIAN_POINT('Ctrl Pts',(-19.5444523020393,-4.01530838331557,
-318.681207102798)) ;
#49278 = CARTESIAN_POINT('Ctrl Pts',(-19.083635690752,5.82458515479567,-318.800301060144)) ;
#49279 = CARTESIAN_POINT('Ctrl Pts',(-13.9712315534961,14.2448134960331,-318.919395017489)) ;
#49280 = CARTESIAN_POINT('Ctrl Pts',(-5.45348902238969,19.1929583164294,-319.038488974835)) ;
#49281 = CARTESIAN_POINT('Ctrl Pts',(4.39352259464737,19.4629705335878,-319.157582932181)) ;
#49282 = CARTESIAN_POINT('Ctrl Pts',(13.1696353160941,14.9890249408472,-319.276676889526)) ;
#49283 = CARTESIAN_POINT('Ctrl Pts',(18.7357526698857,6.8616180926037,-319.395770846872)) ;
#49284 = CARTESIAN_POINT('Ctrl Pts',(19.7351675211273,-2.93825790817971,-319.514864804217)) ;
#49285 = CARTESIAN_POINT('Ctrl Pts',(15.9242835783017,-12.0219550166326,-319.633958761563)) ;
#49286 = CARTESIAN_POINT('Ctrl Pts',(8.231973644788,-18.1753904099397,-319.753052718909)) ;
#49287 = CARTESIAN_POINT('Ctrl Pts',(-1.46681822760808,-19.8987097722735,
-319.872146676254)) ;
#49288 = CARTESIAN_POINT('Ctrl Pts',(-10.8080842235345,-16.7718670030672,
-319.991240633599)) ;
#49289 = CARTESIAN_POINT('Ctrl Pts',(-17.5149601906285,-9.5570066479746,-320.110334590946)) ;
#49290 = CARTESIAN_POINT('Ctrl Pts',(-19.9526952006321,-0.0126971726701712,
-320.229428548291)) ;
#49291 = CARTESIAN_POINT('Ctrl Pts',(-17.5271094702105,9.53470714924482,-320.348522505636)) ;
#49292 = CARTESIAN_POINT('Ctrl Pts',(-10.8294214626632,16.7580976736966,-320.467616462982)) ;
#49293 = CARTESIAN_POINT('Ctrl Pts',(-1.4921426938471,19.8968268081918,-320.586710420328)) ;
#49294 = CARTESIAN_POINT('Ctrl Pts',(8.20883473232013,18.1858527207668,-320.705804377673)) ;
#49295 = CARTESIAN_POINT('Ctrl Pts',(15.9089698828699,12.0422125923406,-320.824898335019)) ;
#49296 = CARTESIAN_POINT('Ctrl Pts',(19.7314122113315,2.96337290839712,-320.943992292364)) ;
#49297 = CARTESIAN_POINT('Ctrl Pts',(18.7444698936355,-6.83776683258475,-321.06308624971)) ;
#49298 = CARTESIAN_POINT('Ctrl Pts',(13.1887027626624,-14.9722518776403,-321.182180207055)) ;
#49299 = CARTESIAN_POINT('Ctrl Pts',(4.41828764340822,-19.4573621323549,-321.301274164401)) ;
#49300 = CARTESIAN_POINT('Ctrl Pts',(-5.42905215453471,-19.199885404682,-321.420368121746)) ;
#49301 = CARTESIAN_POINT('Ctrl Pts',(-13.9531009585651,-14.2625797277198,
-321.539462079092)) ;
#49302 = CARTESIAN_POINT('Ctrl Pts',(-19.0761854119345,-5.84887655700157,
-321.658556036438)) ;
#49303 = CARTESIAN_POINT('Ctrl Pts',(-19.5495918671744,3.99044667630287,-321.777649993783)) ;
#49304 = CARTESIAN_POINT('Ctrl Pts',(-15.2579310296489,12.8571282774965,-321.896743951129)) ;
#49305 = CARTESIAN_POINT('Ctrl Pts',(-7.24726323798025,18.5899806995311,-322.015837908475)) ;
#49306 = CARTESIAN_POINT('Ctrl Pts',(2.52987094603034,19.7916638978624,-322.13493186582)) ;
#49307 = CARTESIAN_POINT('Ctrl Pts',(11.6903679448888,16.169276550379,-322.254025823166)) ;
#49308 = CARTESIAN_POINT('Ctrl Pts',(18.0014248984984,8.60574857134709,-322.373119780511)) ;
#49309 = CARTESIAN_POINT('Ctrl Pts',(19.9247687177452,-1.0553664737327,-322.492213737857)) ;
#49310 = CARTESIAN_POINT('Ctrl Pts',(16.9915986835093,-10.4592438076606,-322.611307695202)) ;
#49311 = CARTESIAN_POINT('Ctrl Pts',(9.91685312745595,-17.3137584278511,-322.730401652548)) ;
#49312 = CARTESIAN_POINT('Ctrl Pts',(0.424948542924112,-19.9481734899561,
-322.849495609893)) ;
#49313 = CARTESIAN_POINT('Ctrl Pts',(-9.17053408133125,-17.7203699598135,
-322.968589567239)) ;
#49314 = CARTESIAN_POINT('Ctrl Pts',(-16.5307673814548,-11.1733583415976,
-323.087683524584)) ;
#49315 = CARTESIAN_POINT('Ctrl Pts',(-19.8617493545485,-1.90292391508733,
-323.20677748193)) ;
#49316 = CARTESIAN_POINT('Ctrl Pts',(-18.3515779741851,7.83133403111656,-323.325871439276)) ;
#49317 = CARTESIAN_POINT('Ctrl Pts',(-12.3683462573407,15.6567626828807,-323.444965396621)) ;
#49318 = CARTESIAN_POINT('Ctrl Pts',(-3.37042233531407,19.665972137963,-323.564059353967)) ;
#49319 = CARTESIAN_POINT('Ctrl Pts',(6.44901690743819,18.8817474767855,-323.683153311313)) ;
#49320 = CARTESIAN_POINT('Ctrl Pts',(14.6965563507,13.4952376148113,-323.802247268658)) ;
#49321 = CARTESIAN_POINT('Ctrl Pts',(19.3619197332629,4.81936417924636,-323.921341226004)) ;
#49322 = CARTESIAN_POINT('Ctrl Pts',(19.3079595067709,-5.0311933509272,-324.040435183349)) ;
#49323 = CARTESIAN_POINT('Ctrl Pts',(14.5478280742058,-13.6554350048934,-324.159529140695)) ;
#49324 = CARTESIAN_POINT('Ctrl Pts',(6.24177198970008,-18.9512661655657,-324.27862309804)) ;
#49325 = CARTESIAN_POINT('Ctrl Pts',(-3.58566949042444,-19.6278674632513,
-324.397717055386)) ;
#49326 = CARTESIAN_POINT('Ctrl Pts',(-12.5391307602418,-15.5203223751015,
-324.516811012731)) ;
#49327 = CARTESIAN_POINT('Ctrl Pts',(-18.4362723753415,-7.62981439824971,
-324.635904970077)) ;
#49328 = CARTESIAN_POINT('Ctrl Pts',(-19.8397100249999,2.12040396468059,-324.754998927422)) ;
#49329 = CARTESIAN_POINT('Ctrl Pts',(-16.4073662434953,11.3537896669496,-324.874092884768)) ;
#49330 = CARTESIAN_POINT('Ctrl Pts',(-8.97584924249228,17.8197737703252,-324.993186842114)) ;
#49331 = CARTESIAN_POINT('Ctrl Pts',(0.643464104378149,19.9423208477824,-325.112280799459)) ;
#49332 = CARTESIAN_POINT('Ctrl Pts',(10.1059378722603,17.2040758708956,-325.231374756805)) ;
#49333 = CARTESIAN_POINT('Ctrl Pts',(17.1051646145768,10.272465641595,-325.350468714151)) ;
#49334 = CARTESIAN_POINT('Ctrl Pts',(19.9351349859114,0.837018484270181,-325.469562671496)) ;
#49335 = CARTESIAN_POINT('Ctrl Pts',(17.906064803169,-8.80244568936556,-325.588656628842)) ;
#49336 = CARTESIAN_POINT('Ctrl Pts',(11.5125247984757,-16.2963793406389,-325.707750586187)) ;
#49337 = CARTESIAN_POINT('Ctrl Pts',(2.31289268980884,-19.8181920026764,-325.826844543533)) ;
#49338 = CARTESIAN_POINT('Ctrl Pts',(-7.45048977143667,-18.5094680910942,
-325.945938500878)) ;
#49339 = CARTESIAN_POINT('Ctrl Pts',(-15.3978708876834,-12.6891993039652,
-326.065032458224)) ;
#49340 = CARTESIAN_POINT('Ctrl Pts',(-19.592135752519,-3.77603277321385,-326.184126415569)) ;
#49341 = CARTESIAN_POINT('Ctrl Pts',(-19.0109635696622,6.05751359903536,-326.303220372915)) ;
#49342 = CARTESIAN_POINT('Ctrl Pts',(-13.7960107265613,14.4145861849075,-326.42231433026)) ;
#49343 = CARTESIAN_POINT('Ctrl Pts',(-5.21838310587703,19.2582108361555,-326.541408287606)) ;
#49344 = CARTESIAN_POINT('Ctrl Pts',(4.63118649845001,19.4077901489607,-326.660502244952)) ;
#49345 = CARTESIAN_POINT('Ctrl Pts',(13.351938915165,14.8268652808078,-326.779596202297)) ;
#49346 = CARTESIAN_POINT('Ctrl Pts',(18.8182557481633,6.63200252157975,-326.898690159643)) ;
#49347 = CARTESIAN_POINT('Ctrl Pts',(19.6977630159421,-3.17936141659043,-327.017784116988)) ;
#49348 = CARTESIAN_POINT('Ctrl Pts',(15.7760873779264,-12.2157797087843,-327.136878074334)) ;
#49349 = CARTESIAN_POINT('Ctrl Pts',(8.00910803827142,-18.2746927547583,-327.25597203168)) ;
#49350 = CARTESIAN_POINT('Ctrl Pts',(-1.71003168492,-19.8792856633756,-327.375065989025)) ;
#49351 = CARTESIAN_POINT('Ctrl Pts',(-11.0123639316808,-16.6384508739767,
-327.494159946371)) ;
#49352 = CARTESIAN_POINT('Ctrl Pts',(-17.6305145574939,-9.34211770893069,
-327.613253903716)) ;
#49353 = CARTESIAN_POINT('Ctrl Pts',(-19.9513586797568,0.231287010470866,
-327.732347861062)) ;
#49354 = CARTESIAN_POINT('Ctrl Pts',(-17.409207843501,9.74831724510958,-327.851441818407)) ;
#49355 = CARTESIAN_POINT('Ctrl Pts',(-10.6236923655856,16.8892678163062,-327.970535775753)) ;
#49356 = CARTESIAN_POINT('Ctrl Pts',(-1.2487310637568,19.9135852517806,-328.089629733099)) ;
#49357 = CARTESIAN_POINT('Ctrl Pts',(8.43059912668088,18.084114720238,-328.208723690444)) ;
#49358 = CARTESIAN_POINT('Ctrl Pts',(16.0550336226244,11.8467760266631,-328.32781764779)) ;
#49359 = CARTESIAN_POINT('Ctrl Pts',(19.7661733490801,2.7218739837902,-328.446911605136)) ;
#49360 = CARTESIAN_POINT('Ctrl Pts',(18.6594556609773,-7.06646455347665,-328.566005562481)) ;
#49361 = CARTESIAN_POINT('Ctrl Pts',(13.0046347451928,-15.1324050300553,-328.685099519827)) ;
#49362 = CARTESIAN_POINT('Ctrl Pts',(4.18003104827804,-19.5099345792074,-328.804193477172)) ;
#49363 = CARTESIAN_POINT('Ctrl Pts',(-5.66342405823282,-19.1320630039249,
-328.923287434518)) ;
#49364 = CARTESIAN_POINT('Ctrl Pts',(-14.1264617663495,-14.0908936839856,
-329.042381391863)) ;
#49365 = CARTESIAN_POINT('Ctrl Pts',(-19.1462797191538,-5.61517406368159,
-329.161475349209)) ;
#49366 = CARTESIAN_POINT('Ctrl Pts',(-19.4993347089371,4.22920237850569,-329.280569306554)) ;
#49367 = CARTESIAN_POINT('Ctrl Pts',(-15.0995722136517,13.0427422658826,-329.3996632639)) ;
#49368 = CARTESIAN_POINT('Ctrl Pts',(-7.01940154519854,18.6772109480185,-329.518757221246)) ;
#49369 = CARTESIAN_POINT('Ctrl Pts',(2.77169592648789,19.7592486836067,-329.637851178591)) ;
#49370 = CARTESIAN_POINT('Ctrl Pts',(11.8872131766261,16.0251168402282,-329.756945135937)) ;
#49371 = CARTESIAN_POINT('Ctrl Pts',(18.1053108235861,8.38498222006786,-329.876039093282)) ;
#49372 = CARTESIAN_POINT('Ctrl Pts',(19.9103739163207,-1.29892931363334,-329.995133050628)) ;
#49373 = CARTESIAN_POINT('Ctrl Pts',(16.8624317811191,-10.6662365095016,-330.114227007973)) ;
#49374 = CARTESIAN_POINT('Ctrl Pts',(9.70439759373315,-17.4337280635058,-330.233320965319)) ;
#49375 = CARTESIAN_POINT('Ctrl Pts',(0.180988830546168,-19.9518783550005,
-330.352414922664)) ;
#49376 = CARTESIAN_POINT('Ctrl Pts',(-9.38653461097536,-17.6069070210097,
-330.47150888001)) ;
#49377 = CARTESIAN_POINT('Ctrl Pts',(-16.6661602093566,-10.9703833445135,
-330.590602837355)) ;
#49378 = CARTESIAN_POINT('Ctrl Pts',(-19.8835334881402,-1.65991050226371,
-330.709696794702)) ;
#49379 = CARTESIAN_POINT('Ctrl Pts',(-18.2544436932851,8.05515315175324,-330.828790752047)) ;
#49380 = CARTESIAN_POINT('Ctrl Pts',(-12.1759693188687,15.8068332690481,-330.947884709393)) ;
#49381 = CARTESIAN_POINT('Ctrl Pts',(-3.12969318402311,19.7057156029259,-331.066978666738)) ;
#49382 = CARTESIAN_POINT('Ctrl Pts',(6.67942233534311,18.8014766472115,-331.186072624084)) ;
#49383 = CARTESIAN_POINT('Ctrl Pts',(14.860478449635,13.3145179070613,-331.305166581429)) ;
#49384 = CARTESIAN_POINT('Ctrl Pts',(19.4194037135064,4.58224467497918,-331.424260538775)) ;
#49385 = CARTESIAN_POINT('Ctrl Pts',(19.2449940766305,-5.26691654006172,-331.54335449612)) ;
#49386 = CARTESIAN_POINT('Ctrl Pts',(14.3797605879269,-13.8323061086509,-331.662448453466)) ;
#49387 = CARTESIAN_POINT('Ctrl Pts',(6.00956764426923,-19.0261741708225,-331.781542410811)) ;
#49388 = CARTESIAN_POINT('Ctrl Pts',(-3.82541261668574,-19.5825541020987,
-331.900636368157)) ;
#49389 = CARTESIAN_POINT('Ctrl Pts',(-12.7279770673796,-15.3658324415495,
-332.019730325502)) ;
#49390 = CARTESIAN_POINT('Ctrl Pts',(-18.5281919836726,-7.40380366201654,
-332.138824282848)) ;
#49391 = CARTESIAN_POINT('Ctrl Pts',(-19.8122982151729,2.36284707134774,-332.257918240194)) ;
#49392 = CARTESIAN_POINT('Ctrl Pts',(-16.2673044398244,11.553571443999,-332.377012197539)) ;
#49393 = CARTESIAN_POINT('Ctrl Pts',(-8.75727646558595,17.9281988987967,-332.496106154885)) ;
#49394 = CARTESIAN_POINT('Ctrl Pts',(0.887272369415106,19.9329615108239,-332.615200112231)) ;
#49395 = CARTESIAN_POINT('Ctrl Pts',(10.3155551781992,17.0792133371256,-332.734294069576)) ;
#49396 = CARTESIAN_POINT('Ctrl Pts',(17.229498305606,10.0625342228804,-332.853388026922)) ;
#49397 = CARTESIAN_POINT('Ctrl Pts',(19.9438796516401,0.593187399070185,-332.972481984267)) ;
#49398 = CARTESIAN_POINT('Ctrl Pts',(17.7970889965095,-9.02074443157773,-333.091575941613)) ;
#49399 = CARTESIAN_POINT('Ctrl Pts',(11.3123905599832,-16.4359370486724,-333.210669898958)) ;
#49400 = CARTESIAN_POINT('Ctrl Pts',(2.07038124829295,-19.8449925254769,-333.329763856304)) ;
#49401 = CARTESIAN_POINT('Ctrl Pts',(-7.67626805981411,-18.4169790010034,
-333.448857813649)) ;
#49402 = CARTESIAN_POINT('Ctrl Pts',(-15.5518842481071,-12.4999641272684,
-333.567951770995)) ;
#49403 = CARTESIAN_POINT('Ctrl Pts',(-19.6368445764187,-3.53617617365065,
-333.68704572834)) ;
#49404 = CARTESIAN_POINT('Ctrl Pts',(-18.9354704144768,6.28952836323949,-333.806139685686)) ;
#49405 = CARTESIAN_POINT('Ctrl Pts',(-13.6187164861328,14.582207244442,-333.925233643031)) ;
#49406 = CARTESIAN_POINT('Ctrl Pts',(-4.98250192973862,19.320581807225,-334.044327600378)) ;
#49407 = CARTESIAN_POINT('Ctrl Pts',(4.86816033189934,19.3497085722871,-334.163421557723)) ;
#49408 = CARTESIAN_POINT('Ctrl Pts',(13.5322448004516,14.6624881077588,-334.282515515069)) ;
#49409 = CARTESIAN_POINT('Ctrl Pts',(18.8979454697689,6.40139546280031,-334.401609472414)) ;
#49410 = CARTESIAN_POINT('Ctrl Pts',(19.6574127982416,-3.41998960949409,-334.52070342976)) ;
#49411 = CARTESIAN_POINT('Ctrl Pts',(15.6255322857092,-12.4077777074612,-334.639797387105)) ;
#49412 = CARTESIAN_POINT('Ctrl Pts',(7.785044753011,-18.3712624782065,-334.758891344451)) ;
#49413 = CARTESIAN_POINT('Ctrl Pts',(-1.95298940763513,-19.8568889613439,
-334.877985301796)) ;
#49414 = CARTESIAN_POINT('Ctrl Pts',(-11.214996957971,-16.5025467756427,-334.997079259142)) ;
#49415 = CARTESIAN_POINT('Ctrl Pts',(-17.7434325976543,-9.12583182520876,
-335.116173216487)) ;
#49416 = CARTESIAN_POINT('Ctrl Pts',(-19.9470388031943,0.475236607621789,
-335.235267173833)) ;
#49417 = CARTESIAN_POINT('Ctrl Pts',(-17.2887029879428,9.96046965985546,-335.354361131178)) ;
#49418 = CARTESIAN_POINT('Ctrl Pts',(-10.4163746912842,17.0179124788699,-335.473455088524)) ;
#49419 = CARTESIAN_POINT('Ctrl Pts',(-1.00513270852244,19.927365984782,-335.592549045869)) ;
#49420 = CARTESIAN_POINT('Ctrl Pts',(8.65110287971146,17.9796725723416,-335.711643003215)) ;
#49421 = CARTESIAN_POINT('Ctrl Pts',(16.1986966270153,11.6495679937027,-335.830736960561)) ;
#49422 = CARTESIAN_POINT('Ctrl Pts',(19.7979788190015,2.47996805211521,-335.949830917907)) ;
#49423 = CARTESIAN_POINT('Ctrl Pts',(18.5716512489525,-7.29410561274543,-336.068924875252)) ;
#49424 = CARTESIAN_POINT('Ctrl Pts',(12.8186221247707,-15.2902954127728,-336.188018832597)) ;
#49425 = CARTESIAN_POINT('Ctrl Pts',(3.94114940369384,-19.5595896666186,-336.307112789943)) ;
#49426 = CARTESIAN_POINT('Ctrl Pts',(-5.89694909550156,-19.0613797694881,
-336.426206747289)) ;
#49427 = CARTESIAN_POINT('Ctrl Pts',(-14.2977102325278,-13.9171005752164,
-336.545300704634)) ;
#49428 = CARTESIAN_POINT('Ctrl Pts',(-19.2135110287503,-5.3806319880013,-336.66439466198)) ;
#49429 = CARTESIAN_POINT('Ctrl Pts',(-19.4461618316232,4.46732581332802,-336.783488619325)) ;
#49430 = CARTESIAN_POINT('Ctrl Pts',(-14.9389554341818,13.2264056779408,-336.902582576671)) ;
#49431 = CARTESIAN_POINT('Ctrl Pts',(-6.79049043683288,18.7616489302821,-337.021676534017)) ;
#49432 = CARTESIAN_POINT('Ctrl Pts',(3.0131068796482,19.723877660543,-337.140770491362)) ;
#49433 = CARTESIAN_POINT('Ctrl Pts',(12.0822800051361,15.8785633058685,-337.259864448708)) ;
#49434 = CARTESIAN_POINT('Ctrl Pts',(18.2064912742636,8.16295699692743,-337.378958406053)) ;
#49435 = CARTESIAN_POINT('Ctrl Pts',(19.8929980664296,-1.54228745284361,-337.498052363399)) ;
#49436 = CARTESIAN_POINT('Ctrl Pts',(16.7307513243974,-10.8716559697218,-337.617146320744)) ;
#49437 = CARTESIAN_POINT('Ctrl Pts',(9.49047454976006,-17.5510458383587,-337.73624027809)) ;
#49438 = CARTESIAN_POINT('Ctrl Pts',(-0.0629639272499312,-19.9526929984175,
-337.855334235436)) ;
#49439 = CARTESIAN_POINT('Ctrl Pts',(-9.60120167038777,-17.4906182918455,
-337.974428192781)) ;
#49440 = CARTESIAN_POINT('Ctrl Pts',(-16.7989087157891,-10.7661722737493,
-338.093522150127)) ;
#49441 = CARTESIAN_POINT('Ctrl Pts',(-19.9030867355192,-1.41438161972877,
-338.212634566703)) ;
#49442 = CARTESIAN_POINT('Ctrl Pts',(-18.7354714653092,5.04783656532755,-338.292048997497)) ;
#49443 = CARTESIAN_POINT('Ctrl Pts',(-17.4137224624119,7.94484592304836,-338.33176544251)) ;
#49444 = CARTESIAN_POINT('Ctrl Pts',(17.5417681427602,-8.35243562587447,-318.252103951997)) ;
#49445 = CARTESIAN_POINT('Ctrl Pts',(16.1520895053933,-11.2710780623612,-318.291824707884)) ;
#49446 = CARTESIAN_POINT('Ctrl Pts',(11.8898989016257,-16.396648979806,-318.371243449552)) ;
#49447 = CARTESIAN_POINT('Ctrl Pts',(2.59312617323014,-20.0866059465783,-318.490360177002)) ;
#49448 = CARTESIAN_POINT('Ctrl Pts',(-7.3321957711988,-18.8792392903931,-318.609454134348)) ;
#49449 = CARTESIAN_POINT('Ctrl Pts',(-15.4712019012634,-13.0705042036884,
-318.728548091693)) ;
#49450 = CARTESIAN_POINT('Ctrl Pts',(-19.8388101575339,-4.07578270854084,
-318.847642049039)) ;
#49451 = CARTESIAN_POINT('Ctrl Pts',(-19.3710532141577,5.91230889188563,-318.966736006384)) ;
#49452 = CARTESIAN_POINT('Ctrl Pts',(-14.1816514565534,14.4593538007606,-319.08582996373)) ;
#49453 = CARTESIAN_POINT('Ctrl Pts',(-5.53562370228694,19.4820223415202,-319.204923921076)) ;
#49454 = CARTESIAN_POINT('Ctrl Pts',(4.45969318203664,19.7561011969232,-319.324017878421)) ;
#49455 = CARTESIAN_POINT('Ctrl Pts',(13.3679824250016,15.2147737707125,-319.443111835767)) ;
#49456 = CARTESIAN_POINT('Ctrl Pts',(19.0179307474167,6.96496052224815,-319.562205793112)) ;
#49457 = CARTESIAN_POINT('Ctrl Pts',(20.0323977274064,-2.98251083905622,-319.681299750458)) ;
#49458 = CARTESIAN_POINT('Ctrl Pts',(16.1641182839235,-12.2030169795293,-319.800393707803)) ;
#49459 = CARTESIAN_POINT('Ctrl Pts',(8.35595491942909,-18.4491289041768,-319.91948766515)) ;
#49460 = CARTESIAN_POINT('Ctrl Pts',(-1.48890989132965,-20.1984030788527,
-320.038581622495)) ;
#49461 = CARTESIAN_POINT('Ctrl Pts',(-10.9708641492585,-17.0244671131838,
-320.15767557984)) ;
#49462 = CARTESIAN_POINT('Ctrl Pts',(-17.7787519838756,-9.70094416734697,
-320.276769537186)) ;
#49463 = CARTESIAN_POINT('Ctrl Pts',(-20.2532015785971,-0.0128884040467512,
-320.395863494531)) ;
#49464 = CARTESIAN_POINT('Ctrl Pts',(-17.7910842430484,9.67830881716817,-320.514957451877)) ;
#49465 = CARTESIAN_POINT('Ctrl Pts',(-10.9925227473007,17.0104904047472,-320.634051409222)) ;
#49466 = CARTESIAN_POINT('Ctrl Pts',(-1.51461576787678,20.1964917555588,-320.753145366568)) ;
#49467 = CARTESIAN_POINT('Ctrl Pts',(8.3324675131509,18.4597487872566,-320.872239323914)) ;
#49468 = CARTESIAN_POINT('Ctrl Pts',(16.1485739498185,12.2235796534028,-320.991333281259)) ;
#49469 = CARTESIAN_POINT('Ctrl Pts',(20.0285858591089,3.00800409482623,-321.110427238605)) ;
#49470 = CARTESIAN_POINT('Ctrl Pts',(19.0267792607647,-6.94075003979398,-321.229521195951)) ;
#49471 = CARTESIAN_POINT('Ctrl Pts',(13.3873370452701,-15.1977480893796,-321.348615153296)) ;
#49472 = CARTESIAN_POINT('Ctrl Pts',(4.4848312157516,-19.7504083278867,-321.467709110641)) ;
#49473 = CARTESIAN_POINT('Ctrl Pts',(-5.51081879219129,-19.4890537582448,
-321.586803067987)) ;
#49474 = CARTESIAN_POINT('Ctrl Pts',(-14.1632477977904,-14.4773876086261,
-321.705897025332)) ;
#49475 = CARTESIAN_POINT('Ctrl Pts',(-19.3634907271257,-5.93696614548253,
-321.824990982678)) ;
#49476 = CARTESIAN_POINT('Ctrl Pts',(-19.8440271293597,4.05054656080969,-321.944084940023)) ;
#49477 = CARTESIAN_POINT('Ctrl Pts',(-15.4877298384242,13.0507687361339,-322.06317889737)) ;
#49478 = CARTESIAN_POINT('Ctrl Pts',(-7.35641384665271,18.869963313924,-322.182272854715)) ;
#49479 = CARTESIAN_POINT('Ctrl Pts',(2.56797318470365,20.0897449927744,-322.301366812061)) ;
#49480 = CARTESIAN_POINT('Ctrl Pts',(11.8664358942496,16.4128010808553,-322.420460769406)) ;
#49481 = CARTESIAN_POINT('Ctrl Pts',(18.2725433083203,8.73535924834337,-322.539554726752)) ;
#49482 = CARTESIAN_POINT('Ctrl Pts',(20.2248544965814,-1.07126128660173,-322.658648684097)) ;
#49483 = CARTESIAN_POINT('Ctrl Pts',(17.2475081596413,-10.6167698682398,-322.777742641443)) ;
#49484 = CARTESIAN_POINT('Ctrl Pts',(10.0662102736548,-17.5745199330913,-322.896836598788)) ;
#49485 = CARTESIAN_POINT('Ctrl Pts',(0.431348668128854,-20.2486117667006,
-323.015930556134)) ;
#49486 = CARTESIAN_POINT('Ctrl Pts',(-9.30865095993212,-17.9872554176065,
-323.135024513479)) ;
#49487 = CARTESIAN_POINT('Ctrl Pts',(-16.779736304241,-11.3416396394963,-323.254118470825)) ;
#49488 = CARTESIAN_POINT('Ctrl Pts',(-20.1608860024333,-1.93158374111668,
-323.37321242817)) ;
#49489 = CARTESIAN_POINT('Ctrl Pts',(-18.6279700190449,7.94928129591769,-323.492306385517)) ;
#49490 = CARTESIAN_POINT('Ctrl Pts',(-12.5546251984983,15.8925682719091,-323.611400342862)) ;
#49491 = CARTESIAN_POINT('Ctrl Pts',(-3.42118406940633,19.9621601966145,-323.730494300208)) ;
#49492 = CARTESIAN_POINT('Ctrl Pts',(6.54614517471249,19.1661243735829,-323.849588257553)) ;
#49493 = CARTESIAN_POINT('Ctrl Pts',(14.9179003281977,13.6984886009376,-323.968682214899)) ;
#49494 = CARTESIAN_POINT('Ctrl Pts',(19.653528476392,4.89194834188894,-324.087776172244)) ;
#49495 = CARTESIAN_POINT('Ctrl Pts',(19.5987555580779,-5.10696786036194,-324.20687012959)) ;
#49496 = CARTESIAN_POINT('Ctrl Pts',(14.7669320638112,-13.8610987145625,-324.325964086935)) ;
#49497 = CARTESIAN_POINT('Ctrl Pts',(6.33577895336331,-19.2366900792777,-324.445058044282)) ;
#49498 = CARTESIAN_POINT('Ctrl Pts',(-3.63967304935781,-19.9234816296209,
-324.564152001626)) ;
#49499 = CARTESIAN_POINT('Ctrl Pts',(-12.7279818768303,-15.7540730446173,
-324.683245958972)) ;
#49500 = CARTESIAN_POINT('Ctrl Pts',(-18.7139399976343,-7.74472658762109,
-324.802339916318)) ;
#49501 = CARTESIAN_POINT('Ctrl Pts',(-20.1385147398288,2.15233924504454,-324.921433873664)) ;
#49502 = CARTESIAN_POINT('Ctrl Pts',(-16.6544766289445,11.5247884305093,-325.040527831009)) ;
#49503 = CARTESIAN_POINT('Ctrl Pts',(-9.11103398409737,18.0881563431071,-325.159621788354)) ;
#49504 = CARTESIAN_POINT('Ctrl Pts',(0.653155279701203,20.2426709782248,-325.2787157457)) ;
#49505 = CARTESIAN_POINT('Ctrl Pts',(10.2581428127656,17.4631854535467,-325.397809703047)) ;
#49506 = CARTESIAN_POINT('Ctrl Pts',(17.3627845005688,10.4271786471158,-325.516903660391)) ;
#49507 = CARTESIAN_POINT('Ctrl Pts',(20.2353768905073,0.849624770812879,-325.635997617737)) ;
#49508 = CARTESIAN_POINT('Ctrl Pts',(18.1757470001605,-8.9350188101769,-325.755091575082)) ;
#49509 = CARTESIAN_POINT('Ctrl Pts',(11.6859142625875,-16.5418181588214,-325.874185532428)) ;
#49510 = CARTESIAN_POINT('Ctrl Pts',(2.34772703162821,-20.1166726358267,-325.993279489773)) ;
#49511 = CARTESIAN_POINT('Ctrl Pts',(-7.56270116306905,-18.7882381097902,
-326.112373447119)) ;
#49512 = CARTESIAN_POINT('Ctrl Pts',(-15.6297773224935,-12.8803105941328,
-326.231467404464)) ;
#49513 = CARTESIAN_POINT('Ctrl Pts',(-19.8872117656786,-3.83290338243963,
-326.35056136181)) ;
#49514 = CARTESIAN_POINT('Ctrl Pts',(-19.2972865824933,6.14874545783015,-326.469655319156)) ;
#49515 = CARTESIAN_POINT('Ctrl Pts',(-14.0037916389702,14.6316834261942,-326.588749276501)) ;
#49516 = CARTESIAN_POINT('Ctrl Pts',(-5.2969768692866,19.5482576256378,-326.707843233846)) ;
#49517 = CARTESIAN_POINT('Ctrl Pts',(4.70093652802422,19.7000897437435,-326.826937191194)) ;
#49518 = CARTESIAN_POINT('Ctrl Pts',(13.5530316879388,15.050171833497,-326.946031148539)) ;
#49519 = CARTESIAN_POINT('Ctrl Pts',(19.1016763997412,6.73188672450952,-327.065125105884)) ;
#49520 = CARTESIAN_POINT('Ctrl Pts',(19.9944298751515,-3.22724559333618,-327.184219063229)) ;
#49521 = CARTESIAN_POINT('Ctrl Pts',(16.0136901092232,-12.3997608540579,-327.303313020575)) ;
#49522 = CARTESIAN_POINT('Ctrl Pts',(8.12973274701934,-18.5499268358154,-327.422406977921)) ;
#49523 = CARTESIAN_POINT('Ctrl Pts',(-1.73578637232805,-20.1786864245842,
-327.541500935266)) ;
#49524 = CARTESIAN_POINT('Ctrl Pts',(-11.1782205021675,-16.8890416115595,
-327.660594892611)) ;
#49525 = CARTESIAN_POINT('Ctrl Pts',(-17.8960467083165,-9.48281879853313,
-327.779688849957)) ;
#49526 = CARTESIAN_POINT('Ctrl Pts',(-20.251844928459,0.234770410637488,-327.898782807302)) ;
#49527 = CARTESIAN_POINT('Ctrl Pts',(-17.6714069068199,9.89513608222032,-328.017876764648)) ;
#49528 = CARTESIAN_POINT('Ctrl Pts',(-10.7836951762985,17.1436360932194,-328.136970721993)) ;
#49529 = CARTESIAN_POINT('Ctrl Pts',(-1.26753812943136,20.2135025970884,-328.256064679339)) ;
#49530 = CARTESIAN_POINT('Ctrl Pts',(8.55757188811282,18.3564785166393,-328.375158636686)) ;
#49531 = CARTESIAN_POINT('Ctrl Pts',(16.2968375470331,12.0251996290154,-328.494252594031)) ;
#49532 = CARTESIAN_POINT('Ctrl Pts',(20.0638705323245,2.76286796900985,-328.613346551376)) ;
#49533 = CARTESIAN_POINT('Ctrl Pts',(18.94048463371,-7.17289216371329,-328.732440508722)) ;
#49534 = CARTESIAN_POINT('Ctrl Pts',(13.2004967901317,-15.3603132990765,-328.851534466067)) ;
#49535 = CARTESIAN_POINT('Ctrl Pts',(4.24298625194697,-19.8037725652929,-328.970628423413)) ;
#49536 = CARTESIAN_POINT('Ctrl Pts',(-5.7487205574529,-19.420209888268,-329.089722380758)) ;
#49537 = CARTESIAN_POINT('Ctrl Pts',(-14.3392195825834,-14.3031158114068,
-329.208816338104)) ;
#49538 = CARTESIAN_POINT('Ctrl Pts',(-19.4346407206152,-5.6997438725497,-329.327910295449)) ;
#49539 = CARTESIAN_POINT('Ctrl Pts',(-19.7930130509952,4.29289814870947,-329.447004252795)) ;
#49540 = CARTESIAN_POINT('Ctrl Pts',(-15.3269859895412,13.2391782459665,-329.56609821014)) ;
#49541 = CARTESIAN_POINT('Ctrl Pts',(-7.12512034221418,18.9585073320931,-329.685192167486)) ;
#49542 = CARTESIAN_POINT('Ctrl Pts',(2.81344027707881,20.0568415748685,-329.804286124832)) ;
#49543 = CARTESIAN_POINT('Ctrl Pts',(12.0662458005342,16.2664701897232,-329.923380082177)) ;
#49544 = CARTESIAN_POINT('Ctrl Pts',(18.377993853263,8.51126794793155,-330.042474039523)) ;
#49545 = CARTESIAN_POINT('Ctrl Pts',(20.2102428958927,-1.31849241221963,-330.161567996868)) ;
#49546 = CARTESIAN_POINT('Ctrl Pts',(17.1163958820726,-10.826880075083,-330.280661954214)) ;
#49547 = CARTESIAN_POINT('Ctrl Pts',(9.85055495953772,-17.696296424427,-330.399755911559)) ;
#49548 = CARTESIAN_POINT('Ctrl Pts',(0.183714692760428,-20.2523724305013,
-330.518849868905)) ;
#49549 = CARTESIAN_POINT('Ctrl Pts',(-9.52790466094728,-17.8720836201031,
-330.63794382625)) ;
#49550 = CARTESIAN_POINT('Ctrl Pts',(-16.9171682756223,-11.1356076478269,
-330.757037783596)) ;
#49551 = CARTESIAN_POINT('Ctrl Pts',(-20.1829982255898,-1.68491031746492,
-330.876131740941)) ;
#49552 = CARTESIAN_POINT('Ctrl Pts',(-18.5293728044092,8.17647134326807,-330.995225698287)) ;
#49553 = CARTESIAN_POINT('Ctrl Pts',(-12.3593508821832,16.0448990624167,-331.114319655634)) ;
#49554 = CARTESIAN_POINT('Ctrl Pts',(-3.17682931041687,20.0025022355838,-331.233413612979)) ;
#49555 = CARTESIAN_POINT('Ctrl Pts',(6.78002072532046,19.0846445897294,-331.352507570324)) ;
#49556 = CARTESIAN_POINT('Ctrl Pts',(15.0842912482982,13.515047084216,-331.47160152767)) ;
#49557 = CARTESIAN_POINT('Ctrl Pts',(19.711878219507,4.65125759460642,-331.590695485015)) ;
#49558 = CARTESIAN_POINT('Ctrl Pts',(19.5348418092689,-5.34624126269106,-331.709789442361)) ;
#49559 = CARTESIAN_POINT('Ctrl Pts',(14.5963333229299,-14.0406336636914,-331.828883399706)) ;
#49560 = CARTESIAN_POINT('Ctrl Pts',(6.10007739183751,-19.3127262696298,-331.947977357052)) ;
#49561 = CARTESIAN_POINT('Ctrl Pts',(-3.88302693285218,-19.8774858065804,
-332.067071314397)) ;
#49562 = CARTESIAN_POINT('Ctrl Pts',(-12.9196723871788,-15.5972563471924,
-332.186165271743)) ;
#49563 = CARTESIAN_POINT('Ctrl Pts',(-18.8072440018219,-7.51531191687963,
-332.305259229089)) ;
#49564 = CARTESIAN_POINT('Ctrl Pts',(-20.1106900823336,2.39843377319207,-332.424353186434)) ;
#49565 = CARTESIAN_POINT('Ctrl Pts',(-16.5123053626227,11.7275791092434,-332.543447143779)) ;
#49566 = CARTESIAN_POINT('Ctrl Pts',(-8.8891692953541,18.1982144561107,-332.662541101126)) ;
#49567 = CARTESIAN_POINT('Ctrl Pts',(0.900635526789087,20.2331706808385,-332.78163505847)) ;
#49568 = CARTESIAN_POINT('Ctrl Pts',(10.4709171527158,17.3364423724425,-332.900729015817)) ;
#49569 = CARTESIAN_POINT('Ctrl Pts',(17.4889907740626,10.2140854635555,-333.019822973162)) ;
#49570 = CARTESIAN_POINT('Ctrl Pts',(20.2442532591362,0.602121359868808,-333.138916930508)) ;
#49571 = CARTESIAN_POINT('Ctrl Pts',(18.0651299152368,-9.15660533700547,-333.258010887853)) ;
#49572 = CARTESIAN_POINT('Ctrl Pts',(11.4827658140091,-16.6834777373511,-333.3771048452)) ;
#49573 = CARTESIAN_POINT('Ctrl Pts',(2.10156313944477,-20.1438767997371,-333.496198802544)) ;
#49574 = CARTESIAN_POINT('Ctrl Pts',(-7.79187988507116,-18.6943560469111,
-333.615292759891)) ;
#49575 = CARTESIAN_POINT('Ctrl Pts',(-15.7861102691503,-12.6882253574836,
-333.734386717235)) ;
#49576 = CARTESIAN_POINT('Ctrl Pts',(-19.9325939465657,-3.5894343166286,-333.853480674581)) ;
#49577 = CARTESIAN_POINT('Ctrl Pts',(-19.2206564293034,6.38425458285745,-333.972574631926)) ;
#49578 = CARTESIAN_POINT('Ctrl Pts',(-13.8238271803337,14.8018290167238,-334.091668589273)) ;
#49579 = CARTESIAN_POINT('Ctrl Pts',(-5.05754310052052,19.6115679622625,-334.210762546618)) ;
#49580 = CARTESIAN_POINT('Ctrl Pts',(4.9414794105492,19.6411334038334,-334.329856503964)) ;
#49581 = CARTESIAN_POINT('Ctrl Pts',(13.7360531496411,14.8833189854379,-334.448950461308)) ;
#49582 = CARTESIAN_POINT('Ctrl Pts',(19.1825663235932,6.49780650627617,-334.568044418655)) ;
#49583 = CARTESIAN_POINT('Ctrl Pts',(19.9534719451772,-3.47149787340994,-334.687138376)) ;
#49584 = CARTESIAN_POINT('Ctrl Pts',(15.8608675155485,-12.5946505233876,-334.806232333347)) ;
#49585 = CARTESIAN_POINT('Ctrl Pts',(7.9022948576961,-18.6479509902325,-334.925326290692)) ;
#49586 = CARTESIAN_POINT('Ctrl Pts',(-1.98240326712582,-20.1559524071304,
-335.044420248037)) ;
#49587 = CARTESIAN_POINT('Ctrl Pts',(-11.3839053726409,-16.7510906695319,
-335.163514205383)) ;
#49588 = CARTESIAN_POINT('Ctrl Pts',(-18.0106654004898,-9.26327544573905,
-335.282608162728)) ;
#49589 = CARTESIAN_POINT('Ctrl Pts',(-20.2474599904878,0.482394118434052,
-335.401702120073)) ;
#49590 = CARTESIAN_POINT('Ctrl Pts',(-17.5490871346648,10.1104837121034,-335.520796077419)) ;
#49591 = CARTESIAN_POINT('Ctrl Pts',(-10.5732551026036,17.2742182655382,-335.639890034764)) ;
#49592 = CARTESIAN_POINT('Ctrl Pts',(-1.02027095358536,20.2274908809053,-335.75898399211)) ;
#49593 = CARTESIAN_POINT('Ctrl Pts',(8.78139663529907,18.2504633716488,-335.878077949457)) ;
#49594 = CARTESIAN_POINT('Ctrl Pts',(16.4426642515488,11.8250214573798,-335.997171906802)) ;
#49595 = CARTESIAN_POINT('Ctrl Pts',(20.0961550225722,2.51731870621567,-336.116265864147)) ;
#49596 = CARTESIAN_POINT('Ctrl Pts',(18.8513578045599,-7.40396171169045,-336.235359821493)) ;
#49597 = CARTESIAN_POINT('Ctrl Pts',(13.0116826444891,-15.5205816596335,-336.354453778838)) ;
#49598 = CARTESIAN_POINT('Ctrl Pts',(4.00050682485498,-19.8541755050778,-336.473547736184)) ;
#49599 = CARTESIAN_POINT('Ctrl Pts',(-5.9857627016793,-19.3484620977624,-336.592641693529)) ;
#49600 = CARTESIAN_POINT('Ctrl Pts',(-14.5130472119166,-14.126705214769,-336.711735650875)) ;
#49601 = CARTESIAN_POINT('Ctrl Pts',(-19.5028845970419,-5.46166937235563,
-336.83082960822)) ;
#49602 = CARTESIAN_POINT('Ctrl Pts',(-19.7390393400793,4.53460794668666,-336.949923565566)) ;
#49603 = CARTESIAN_POINT('Ctrl Pts',(-15.1639501701295,13.425607801955,-337.069017522911)) ;
#49604 = CARTESIAN_POINT('Ctrl Pts',(-6.89276161700482,19.0442170298797,-337.188111480257)) ;
#49605 = CARTESIAN_POINT('Ctrl Pts',(3.05848710651578,20.0209378308908,-337.307205437602)) ;
#49606 = CARTESIAN_POINT('Ctrl Pts',(12.2642505191642,16.1177094211354,-337.426299394949)) ;
#49607 = CARTESIAN_POINT('Ctrl Pts',(18.480698176803,8.28589881586294,-337.545393352293)) ;
#49608 = CARTESIAN_POINT('Ctrl Pts',(20.1926053493404,-1.56551575416202,-337.66448730964)) ;
#49609 = CARTESIAN_POINT('Ctrl Pts',(16.9827321936771,-11.0353933458052,-337.783581266985)) ;
#49610 = CARTESIAN_POINT('Ctrl Pts',(9.63341003308405,-17.8153811154403,-337.902675224331)) ;
#49611 = CARTESIAN_POINT('Ctrl Pts',(-0.0639122232836121,-20.2531993432151,
-338.021769181676)) ;
#49612 = CARTESIAN_POINT('Ctrl Pts',(-9.74580480841337,-17.7540434731756,
-338.140863139021)) ;
#49613 = CARTESIAN_POINT('Ctrl Pts',(-17.0519160995629,-10.9283209660436,
-338.259957096367)) ;
#49614 = CARTESIAN_POINT('Ctrl Pts',(-20.2028459632864,-1.43568353875935,
-338.379069512944)) ;
#49615 = CARTESIAN_POINT('Ctrl Pts',(-19.0176453076346,5.12386173724306,-338.458483943739)) ;
#49616 = CARTESIAN_POINT('Ctrl Pts',(-17.6759895201426,8.06450278382925,-338.49820038875)) ;
#49617 = CARTESIAN_POINT('Ctrl Pts',(1.53122046431516,-19.3652704049865,-338.)) ;
#49618 = CARTESIAN_POINT('Ctrl Pts',(1.12192133411244,-19.3892945386684,-338.)) ;
#49619 = CARTESIAN_POINT('Ctrl Pts',(0.712537519554564,-19.4002678090365,
-338.)) ;
#49620 = CARTESIAN_POINT('Ctrl Pts',(0.303666630142025,-19.3980968578391,
-338.)) ;
#49621 = CARTESIAN_POINT('Ctrl Pts',(0.181986669634313,-19.3974507828487,
-338.)) ;
#49622 = CARTESIAN_POINT('Ctrl Pts',(0.0603520673764698,-19.3956402363443,
-338.)) ;
#49623 = CARTESIAN_POINT('Ctrl Pts',(-0.061221567909213,-19.3926618778456,
-338.)) ;
#49624 = CARTESIAN_POINT('Ctrl Pts',(-0.466207908217332,-19.3827403639772,
-338.)) ;
#49625 = CARTESIAN_POINT('Ctrl Pts',(-0.870517665367189,-19.3598637558529,
-338.)) ;
#49626 = CARTESIAN_POINT('Ctrl Pts',(-1.2735764150429,-19.3242721999153,-338.)) ;
#49627 = CARTESIAN_POINT('Ctrl Pts',(-1.68065183836914,-19.2883259570616,
-338.)) ;
#49628 = CARTESIAN_POINT('Ctrl Pts',(-2.08645173638727,-19.2394100004437,
-338.)) ;
#49629 = CARTESIAN_POINT('Ctrl Pts',(-2.49038044442016,-19.1777188116874,
-338.)) ;
#49630 = CARTESIAN_POINT('Ctrl Pts',(-2.89439384831672,-19.1160146875086,
-338.)) ;
#49631 = CARTESIAN_POINT('Ctrl Pts',(-3.29653581874664,-19.0415298124728,
-338.)) ;
#49632 = CARTESIAN_POINT('Ctrl Pts',(-3.69619830300842,-18.9544080717603,
-338.)) ;
#49633 = CARTESIAN_POINT('Ctrl Pts',(-4.09281102360135,-18.8679511438087,
-338.)) ;
#49634 = CARTESIAN_POINT('Ctrl Pts',(-4.48698245887238,-18.7690492636138,
-338.)) ;
#49635 = CARTESIAN_POINT('Ctrl Pts',(-4.87809877604152,-18.6577959732304,
-338.)) ;
#49636 = CARTESIAN_POINT('Ctrl Pts',(-5.15629077763809,-18.578664077737,-338.)) ;
#49637 = CARTESIAN_POINT('Ctrl Pts',(-5.4329367601865,-18.4932824403319,-338.)) ;
#49638 = CARTESIAN_POINT('Ctrl Pts',(-5.70780760673927,-18.4016708993542,
-338.)) ;
#49639 = CARTESIAN_POINT('Ctrl Pts',(-5.75904326826443,-18.3845945961951,
-338.)) ;
#49640 = CARTESIAN_POINT('Ctrl Pts',(-5.81021723142297,-18.3673018061672,
-338.)) ;
#49641 = CARTESIAN_POINT('Ctrl Pts',(-5.8613279811968,-18.3497926149073,-338.)) ;
#49642 = CARTESIAN_POINT('Ctrl Pts',(-5.90598635521624,-18.3344938369492,
-338.)) ;
#49643 = CARTESIAN_POINT('Ctrl Pts',(-5.95058793173612,-18.3190327470415,
-338.)) ;
#49644 = CARTESIAN_POINT('Ctrl Pts',(-5.99512278417975,-18.3034128014496,
-338.)) ;
#49645 = CARTESIAN_POINT('Ctrl Pts',(-6.01150522446275,-18.2976669010627,
-338.)) ;
#49646 = CARTESIAN_POINT('Ctrl Pts',(-6.02787882113695,-18.2918994425318,
-338.)) ;
#49647 = CARTESIAN_POINT('Ctrl Pts',(-6.04424329331104,-18.2861105298845,
-338.)) ;
#49648 = CARTESIAN_POINT('Ctrl Pts',(-6.42829511386026,-18.1502526532877,
-338.)) ;
#49649 = CARTESIAN_POINT('Ctrl Pts',(-6.80747072006426,-18.0025302201036,
-338.)) ;
#49650 = CARTESIAN_POINT('Ctrl Pts',(-7.18119888215102,-17.8431638857732,
-338.)) ;
#49651 = CARTESIAN_POINT('Ctrl Pts',(-7.55462919821985,-17.6839245598753,
-338.)) ;
#49652 = CARTESIAN_POINT('Ctrl Pts',(-7.92262127604276,-17.5130596995448,
-338.)) ;
#49653 = CARTESIAN_POINT('Ctrl Pts',(-8.28459074029327,-17.3307396766341,
-338.)) ;
#49654 = CARTESIAN_POINT('Ctrl Pts',(-8.60540796776493,-17.1691475810581,
-338.)) ;
#49655 = CARTESIAN_POINT('Ctrl Pts',(-8.92149419227665,-16.998556156645,-338.)) ;
#49656 = CARTESIAN_POINT('Ctrl Pts',(-9.23242801516554,-16.819053016636,-338.)) ;
#49657 = CARTESIAN_POINT('Ctrl Pts',(-9.58379862825655,-16.6162055818645,
-338.)) ;
#49658 = CARTESIAN_POINT('Ctrl Pts',(-9.92859044196816,-16.4019782696566,
-338.)) ;
#49659 = CARTESIAN_POINT('Ctrl Pts',(-10.2663642689513,-16.1768116880322,
-338.)) ;
#49660 = CARTESIAN_POINT('Ctrl Pts',(-10.6170152476493,-15.9430609474202,
-338.)) ;
#49661 = CARTESIAN_POINT('Ctrl Pts',(-10.9601036420671,-15.6975207646042,
-338.)) ;
#49662 = CARTESIAN_POINT('Ctrl Pts',(-11.2950979866766,-15.4406404079358,
-338.)) ;
#49663 = CARTESIAN_POINT('Ctrl Pts',(-11.6300923312865,-15.183760051267,-338.)) ;
#49664 = CARTESIAN_POINT('Ctrl Pts',(-11.9569931202482,-14.9155390478906,
-338.)) ;
#49665 = CARTESIAN_POINT('Ctrl Pts',(-12.2752207699239,-14.6363892224392,
-338.)) ;
#49666 = CARTESIAN_POINT('Ctrl Pts',(-12.3029402979512,-14.6120736061868,
-338.)) ;
#49667 = CARTESIAN_POINT('Ctrl Pts',(-12.3305931560439,-14.5876757429795,
-338.)) ;
#49668 = CARTESIAN_POINT('Ctrl Pts',(-12.3581695198653,-14.5632043767021,
-338.)) ;
#49669 = CARTESIAN_POINT('Ctrl Pts',(-12.6595416244126,-14.2957656670909,
-338.)) ;
#49670 = CARTESIAN_POINT('Ctrl Pts',(-12.9520844173906,-14.0192854610996,
-338.)) ;
#49671 = CARTESIAN_POINT('Ctrl Pts',(-13.2354196355927,-13.7342473807588,
-338.)) ;
#49672 = CARTESIAN_POINT('Ctrl Pts',(-13.5205791579126,-13.4473740321199,
-338.)) ;
#49673 = CARTESIAN_POINT('Ctrl Pts',(-13.7964125715532,-13.1518318817186,
-338.)) ;
#49674 = CARTESIAN_POINT('Ctrl Pts',(-14.0625020156188,-12.8480723757908,
-338.)) ;
#49675 = CARTESIAN_POINT('Ctrl Pts',(-14.328094515029,-12.544880166561,-338.)) ;
#49676 = CARTESIAN_POINT('Ctrl Pts',(-14.5839797799945,-12.2335008504745,
-338.)) ;
#49677 = CARTESIAN_POINT('Ctrl Pts',(-14.8297043966001,-11.9143480443392,
-338.)) ;
#49678 = CARTESIAN_POINT('Ctrl Pts',(-15.0728958847685,-11.5984853239113,
-338.)) ;
#49679 = CARTESIAN_POINT('Ctrl Pts',(-15.3061354351909,-11.275008127149,-338.)) ;
#49680 = CARTESIAN_POINT('Ctrl Pts',(-15.5289414287006,-10.9442891626757,
-338.)) ;
#49681 = CARTESIAN_POINT('Ctrl Pts',(-15.6845001549643,-10.7133877400778,
-338.)) ;
#49682 = CARTESIAN_POINT('Ctrl Pts',(-15.8349721202972,-10.4789556881506,
-338.)) ;
#49683 = CARTESIAN_POINT('Ctrl Pts',(-15.9801798449266,-10.2411132100054,
-338.)) ;
#49684 = CARTESIAN_POINT('Ctrl Pts',(-16.1748344006451,-9.92227947004763,
-338.)) ;
#49685 = CARTESIAN_POINT('Ctrl Pts',(-16.3600303833031,-9.59731728203679,
-338.)) ;
#49686 = CARTESIAN_POINT('Ctrl Pts',(-16.5355799150942,-9.2666831201162,-338.)) ;
#49687 = CARTESIAN_POINT('Ctrl Pts',(-16.5779666097208,-9.18685101169948,
-338.)) ;
#49688 = CARTESIAN_POINT('Ctrl Pts',(-16.6197907574038,-9.10668819275675,
-338.)) ;
#49689 = CARTESIAN_POINT('Ctrl Pts',(-16.661049385152,-9.02620102002121,-338.)) ;
#49690 = CARTESIAN_POINT('Ctrl Pts',(-16.6936059345179,-8.96268982841101,
-338.)) ;
#49691 = CARTESIAN_POINT('Ctrl Pts',(-16.7258103578028,-8.8989766759393,-338.)) ;
#49692 = CARTESIAN_POINT('Ctrl Pts',(-16.7576611369262,-8.83506467784942,
-338.)) ;
#49693 = CARTESIAN_POINT('Ctrl Pts',(-16.779604249934,-8.79103347248394,-338.)) ;
#49694 = CARTESIAN_POINT('Ctrl Pts',(-16.8013802791104,-8.74690619927829,
-338.)) ;
#49695 = CARTESIAN_POINT('Ctrl Pts',(-16.8229776736961,-8.7027068234737,-338.)) ;
#49696 = CARTESIAN_POINT('Ctrl Pts',(-16.9064115593317,-8.53195818750261,
-338.)) ;
#49697 = CARTESIAN_POINT('Ctrl Pts',(-16.9872118844882,-8.36007011454329,
-338.)) ;
#49698 = CARTESIAN_POINT('Ctrl Pts',(-17.0653728977658,-8.18710624704896,
-338.)) ;
#49699 = CARTESIAN_POINT('Ctrl Pts',(-17.2299870027546,-7.82282882728421,
-338.)) ;
#49700 = CARTESIAN_POINT('Ctrl Pts',(-17.3828941511382,-7.45378725021279,
-338.)) ;
#49701 = CARTESIAN_POINT('Ctrl Pts',(-17.5239885713209,-7.08059343174374,
-338.)) ;
#49702 = CARTESIAN_POINT('Ctrl Pts',(-17.6659184550873,-6.70518981756066,
-338.)) ;
#49703 = CARTESIAN_POINT('Ctrl Pts',(-17.7958954921236,-6.32558411687078,
-338.)) ;
#49704 = CARTESIAN_POINT('Ctrl Pts',(-17.9137644956534,-5.9423765101345,-338.)) ;
#49705 = CARTESIAN_POINT('Ctrl Pts',(-18.0314668555706,-5.55971068366358,
-338.)) ;
#49706 = CARTESIAN_POINT('Ctrl Pts',(-18.1370955328315,-5.17345258238865,
-338.)) ;
#49707 = CARTESIAN_POINT('Ctrl Pts',(-18.2304463747966,-4.7841853991055,-338.)) ;
#49708 = CARTESIAN_POINT('Ctrl Pts',(-18.3232264444352,-4.39729830079178,
-338.)) ;
#49709 = CARTESIAN_POINT('Ctrl Pts',(-18.4038784618712,-4.00743827161781,
-338.)) ;
#49710 = CARTESIAN_POINT('Ctrl Pts',(-18.4721512104871,-3.61517165557224,
-338.)) ;
#49711 = CARTESIAN_POINT('Ctrl Pts',(-18.5393817124124,-3.22889335244342,
-338.)) ;
#49712 = CARTESIAN_POINT('Ctrl Pts',(-18.5946080455807,-2.84028088845193,
-338.)) ;
#49713 = CARTESIAN_POINT('Ctrl Pts',(-18.6375401222669,-2.44987658596576,
-338.)) ;
#49714 = CARTESIAN_POINT('Ctrl Pts',(-18.6620178572193,-2.22728746896645,
-338.)) ;
#49715 = CARTESIAN_POINT('Ctrl Pts',(-18.6824981590813,-2.00411594415889,
-338.)) ;
#49716 = CARTESIAN_POINT('Ctrl Pts',(-18.6989197228858,-1.78046367084787,
-338.)) ;
#49717 = CARTESIAN_POINT('Ctrl Pts',(-18.7019205354198,-1.73959432655047,
-338.)) ;
#49718 = CARTESIAN_POINT('Ctrl Pts',(-18.7047857659883,-1.69870898034511,
-338.)) ;
#49719 = CARTESIAN_POINT('Ctrl Pts',(-18.7075141594755,-1.65782261116247,
-338.)) ;
#49720 = CARTESIAN_POINT('Ctrl Pts',(-18.7147395803788,-1.54954599053089,
-338.)) ;
#49721 = CARTESIAN_POINT('Ctrl Pts',(-18.721007273306,-1.44123695536378,-338.)) ;
#49722 = CARTESIAN_POINT('Ctrl Pts',(-18.7263137442602,-1.33290715643541,
-338.)) ;
#49723 = CARTESIAN_POINT('Ctrl Pts',(-18.7457439791969,-0.936245521609726,
-338.)) ;
#49724 = CARTESIAN_POINT('Ctrl Pts',(-18.752290839866,-0.539305802993233,
-338.)) ;
#49725 = CARTESIAN_POINT('Ctrl Pts',(-18.746150022536,-0.142677068484718,
-338.)) ;
#49726 = CARTESIAN_POINT('Ctrl Pts',(-18.7399765659379,0.256059800969821,
-338.)) ;
#49727 = CARTESIAN_POINT('Ctrl Pts',(-18.7209801146579,0.654482919550263,
-338.)) ;
#49728 = CARTESIAN_POINT('Ctrl Pts',(-18.6893065939024,1.05199317238646,-338.)) ;
#49729 = CARTESIAN_POINT('Ctrl Pts',(-18.6576201367373,1.44966578025454,-338.)) ;
#49730 = CARTESIAN_POINT('Ctrl Pts',(-18.6132461326084,1.84642532793274,-338.)) ;
#49731 = CARTESIAN_POINT('Ctrl Pts',(-18.5562794787259,2.24166310101432,-338.)) ;
#49732 = CARTESIAN_POINT('Ctrl Pts',(-18.5221279800155,2.47860807456891,-338.)) ;
#49733 = CARTESIAN_POINT('Ctrl Pts',(-18.483449708919,2.71500591409569,-338.)) ;
#49734 = CARTESIAN_POINT('Ctrl Pts',(-18.4402565595206,2.95072268342921,-338.)) ;
#49735 = CARTESIAN_POINT('Ctrl Pts',(-18.429993187445,3.00673269755961,-338.)) ;
#49736 = CARTESIAN_POINT('Ctrl Pts',(-18.4194744473254,3.06270643984912,-338.)) ;
#49737 = CARTESIAN_POINT('Ctrl Pts',(-18.4087018356681,3.11863490845468,-338.)) ;
#49738 = CARTESIAN_POINT('Ctrl Pts',(-18.4018134016346,3.15439778368304,-338.)) ;
#49739 = CARTESIAN_POINT('Ctrl Pts',(-18.3948215986383,3.19013989341542,-338.)) ;
#49740 = CARTESIAN_POINT('Ctrl Pts',(-18.3877273514385,3.22585673647208,-338.)) ;
#49741 = CARTESIAN_POINT('Ctrl Pts',(-18.3101159279799,3.61660080741016,-338.)) ;
#49742 = CARTESIAN_POINT('Ctrl Pts',(-18.220212432157,4.00450434614193,-338.)) ;
#49743 = CARTESIAN_POINT('Ctrl Pts',(-18.118173080588,4.38897607361206,-338.)) ;
#49744 = CARTESIAN_POINT('Ctrl Pts',(-18.0163151528155,4.77276421852882,-338.)) ;
#49745 = CARTESIAN_POINT('Ctrl Pts',(-17.9023643369644,5.15313328585193,-338.)) ;
#49746 = CARTESIAN_POINT('Ctrl Pts',(-17.7764256451059,5.52948306809377,-338.)) ;
#49747 = CARTESIAN_POINT('Ctrl Pts',(-17.651889804069,5.90164063114181,-338.)) ;
#49748 = CARTESIAN_POINT('Ctrl Pts',(-17.5156314622654,6.26986843888553,-338.)) ;
#49749 = CARTESIAN_POINT('Ctrl Pts',(-17.3677056193957,6.63356670882829,-338.)) ;
#49750 = CARTESIAN_POINT('Ctrl Pts',(-17.2208939190367,6.99452568930165,-338.)) ;
#49751 = CARTESIAN_POINT('Ctrl Pts',(-17.0625896473109,7.35102357559316,-338.)) ;
#49752 = CARTESIAN_POINT('Ctrl Pts',(-16.8928031616867,7.70244771115104,-338.)) ;
#49753 = CARTESIAN_POINT('',(-15.1169529804711,-10.7789097737449,-318.249803151889)) ;
#49754 = CARTESIAN_POINT('Ctrl Pts',(-15.1172285295639,-10.7791107733297,
-318.25)) ;
#49755 = CARTESIAN_POINT('Ctrl Pts',(-14.8934395929579,-11.1089469203127,
-318.25)) ;
#49756 = CARTESIAN_POINT('Ctrl Pts',(-14.6593537074853,-11.431009438768,-318.25)) ;
#49757 = CARTESIAN_POINT('Ctrl Pts',(-14.4152963237418,-11.7447716872223,
-318.25)) ;
#49758 = CARTESIAN_POINT('Ctrl Pts',(-14.3474396575172,-11.8320087944987,
-318.25)) ;
#49759 = CARTESIAN_POINT('Ctrl Pts',(-14.2788118621464,-11.918604159466,-318.25)) ;
#49760 = CARTESIAN_POINT('Ctrl Pts',(-14.209419264857,-12.0045462090401,-318.25)) ;
#49761 = CARTESIAN_POINT('Ctrl Pts',(-13.9621513090759,-12.3107851414901,
-318.25)) ;
#49762 = CARTESIAN_POINT('Ctrl Pts',(-13.7051760626163,-12.6087308722331,
-318.25)) ;
#49763 = CARTESIAN_POINT('Ctrl Pts',(-13.4390527258754,-12.8980992743919,
-318.25)) ;
#49764 = CARTESIAN_POINT('Ctrl Pts',(-13.1707551578732,-13.1898318203108,
-318.25)) ;
#49765 = CARTESIAN_POINT('Ctrl Pts',(-12.8931590317108,-13.4728466860606,
-318.25)) ;
#49766 = CARTESIAN_POINT('Ctrl Pts',(-12.6067933865282,-13.7468220954629,
-318.25)) ;
#49767 = CARTESIAN_POINT('Ctrl Pts',(-12.3195148583575,-14.0216708899748,
-318.25)) ;
#49768 = CARTESIAN_POINT('Ctrl Pts',(-12.0234103896743,-14.2874228706985,
-318.25)) ;
#49769 = CARTESIAN_POINT('Ctrl Pts',(-11.7189760896812,-14.5437169207685,
-318.25)) ;
#49770 = CARTESIAN_POINT('Ctrl Pts',(-11.4152434420173,-14.7994202709167,
-318.25)) ;
#49771 = CARTESIAN_POINT('Ctrl Pts',(-11.1032188665144,-15.0457095764132,
-318.25)) ;
#49772 = CARTESIAN_POINT('Ctrl Pts',(-10.7833638518003,-15.2821849399938,
-318.25)) ;
#49773 = CARTESIAN_POINT('Ctrl Pts',(-10.629871777717,-15.3956647741556,-318.25)) ;
#49774 = CARTESIAN_POINT('Ctrl Pts',(-10.4745760517745,-15.5068839629755,
-318.25)) ;
#49775 = CARTESIAN_POINT('Ctrl Pts',(-10.3175255756812,-15.615794572014,-318.25)) ;
#49776 = CARTESIAN_POINT('Ctrl Pts',(-10.2483745954551,-15.6637490612928,
-318.25)) ;
#49777 = CARTESIAN_POINT('Ctrl Pts',(-10.1788833998896,-15.7112559453889,
-318.25)) ;
#49778 = CARTESIAN_POINT('Ctrl Pts',(-10.1090560916909,-15.7583109732571,
-318.25)) ;
#49779 = CARTESIAN_POINT('Ctrl Pts',(-10.0638091334537,-15.7888018647969,
-318.25)) ;
#49780 = CARTESIAN_POINT('Ctrl Pts',(-10.0184188268518,-15.8191044922151,
-318.25)) ;
#49781 = CARTESIAN_POINT('Ctrl Pts',(-9.9728937426656,-15.8492127503619,-318.25)) ;
#49782 = CARTESIAN_POINT('Ctrl Pts',(-9.92573156378842,-15.8804037098467,
-318.25)) ;
#49783 = CARTESIAN_POINT('Ctrl Pts',(-9.87843774940729,-15.9113774836762,
-318.25)) ;
#49784 = CARTESIAN_POINT('Ctrl Pts',(-9.8310174318769,-15.9421309678968,-318.25)) ;
#49785 = CARTESIAN_POINT('Ctrl Pts',(-9.49504077518283,-16.1600218076937,
-318.25)) ;
#49786 = CARTESIAN_POINT('Ctrl Pts',(-9.15264811101595,-16.3669028052293,
-318.25)) ;
#49787 = CARTESIAN_POINT('Ctrl Pts',(-8.80438953721077,-16.5624759763278,
-318.25)) ;
#49788 = CARTESIAN_POINT('Ctrl Pts',(-8.45495228619666,-16.7587110626145,
-318.25)) ;
#49789 = CARTESIAN_POINT('Ctrl Pts',(-8.09960891386764,-16.9435620090313,
-318.25)) ;
#49790 = CARTESIAN_POINT('Ctrl Pts',(-7.73887904347091,-17.1166898203253,
-318.25)) ;
#49791 = CARTESIAN_POINT('Ctrl Pts',(-7.4327189837679,-17.2636275302069,-318.25)) ;
#49792 = CARTESIAN_POINT('Ctrl Pts',(-7.12267810039724,-17.4021201630692,
-318.25)) ;
#49793 = CARTESIAN_POINT('Ctrl Pts',(-6.80905734728888,-17.5319362137542,
-318.25)) ;
#49794 = CARTESIAN_POINT('Ctrl Pts',(-6.44033603205845,-17.6845598665966,
-318.25)) ;
#49795 = CARTESIAN_POINT('Ctrl Pts',(-6.0666666021044,-17.8251916385922,-318.25)) ;
#49796 = CARTESIAN_POINT('Ctrl Pts',(-5.68866153394493,-17.9537870129653,
-318.25)) ;
#49797 = CARTESIAN_POINT('Ctrl Pts',(-5.31000037174938,-18.0826055871452,
-318.25)) ;
#49798 = CARTESIAN_POINT('Ctrl Pts',(-4.9269879640148,-18.1993460595037,-318.25)) ;
#49799 = CARTESIAN_POINT('Ctrl Pts',(-4.54022430962917,-18.303913654081,-318.25)) ;
#49800 = CARTESIAN_POINT('Ctrl Pts',(-4.25712592444706,-18.3804537240476,
-318.25)) ;
#49801 = CARTESIAN_POINT('Ctrl Pts',(-3.97201735027695,-18.4504708252309,
-318.25)) ;
#49802 = CARTESIAN_POINT('Ctrl Pts',(-3.68513114204395,-18.5139102951467,
-318.25)) ;
#49803 = CARTESIAN_POINT('Ctrl Pts',(-3.60185362345996,-18.5323255465016,
-318.25)) ;
#49804 = CARTESIAN_POINT('Ctrl Pts',(-3.51842630884418,-18.5501864512475,
-318.25)) ;
#49805 = CARTESIAN_POINT('Ctrl Pts',(-3.43485487456654,-18.5674914340203,
-318.25)) ;
#49806 = CARTESIAN_POINT('Ctrl Pts',(-3.37730934983001,-18.5794072797015,
-318.25)) ;
#49807 = CARTESIAN_POINT('Ctrl Pts',(-3.31969462818924,-18.5910597081359,
-318.25)) ;
#49808 = CARTESIAN_POINT('Ctrl Pts',(-3.26201522493554,-18.6024476502174,
-318.25)) ;
#49809 = CARTESIAN_POINT('Ctrl Pts',(-3.21756770865879,-18.611223152606,-318.25)) ;
#49810 = CARTESIAN_POINT('Ctrl Pts',(-3.17308968396432,-18.6198400188813,
-318.25)) ;
#49811 = CARTESIAN_POINT('Ctrl Pts',(-3.12859179875859,-18.6282963987947,
-318.25)) ;
#49812 = CARTESIAN_POINT('Ctrl Pts',(-2.73549464914775,-18.7030005970865,
-318.25)) ;
#49813 = CARTESIAN_POINT('Ctrl Pts',(-2.34060402666148,-18.7652327176257,
-318.25)) ;
#49814 = CARTESIAN_POINT('Ctrl Pts',(-1.94454526365388,-18.8150157087449,
-318.25)) ;
#49815 = CARTESIAN_POINT('Ctrl Pts',(-1.54434519916198,-18.8653192447789,
-318.25)) ;
#49816 = CARTESIAN_POINT('Ctrl Pts',(-1.14295191666762,-18.9029121077673,
-318.25)) ;
#49817 = CARTESIAN_POINT('Ctrl Pts',(-0.740991016366364,-18.9277686014751,
-318.25)) ;
#49818 = CARTESIAN_POINT('Ctrl Pts',(-0.338804046011407,-18.9526390749228,
-318.25)) ;
#49819 = CARTESIAN_POINT('Ctrl Pts',(0.063951739996451,-18.9647589382012,
-318.25)) ;
#49820 = CARTESIAN_POINT('Ctrl Pts',(0.466660972673863,-18.9640515178069,
-318.25)) ;
#49821 = CARTESIAN_POINT('Ctrl Pts',(0.866538636378975,-18.9633490714969,
-318.25)) ;
#49822 = CARTESIAN_POINT('Ctrl Pts',(1.26637094916322,-18.9499991231767,-318.25)) ;
#49823 = CARTESIAN_POINT('Ctrl Pts',(1.66555826598646,-18.923875599887,-318.25)) ;
#49824 = CARTESIAN_POINT('Ctrl Pts',(1.92227833398459,-18.907075385069,-318.25)) ;
#49825 = CARTESIAN_POINT('Ctrl Pts',(2.17873167516151,-18.8849911641002,-318.25)) ;
#49826 = CARTESIAN_POINT('Ctrl Pts',(2.43475782264655,-18.8575780223985,-318.25)) ;
#49827 = CARTESIAN_POINT('Ctrl Pts',(2.83508915706831,-18.8147138864268,-318.25)) ;
#49828 = CARTESIAN_POINT('Ctrl Pts',(3.23437686538619,-18.758823143256,-318.25)) ;
#49829 = CARTESIAN_POINT('Ctrl Pts',(3.63204670084311,-18.6900943991976,-318.25)) ;
#49830 = CARTESIAN_POINT('Ctrl Pts',(3.72453243208256,-18.6741102143672,-318.25)) ;
#49831 = CARTESIAN_POINT('Ctrl Pts',(3.81693059106408,-18.6574314297529,-318.25)) ;
#49832 = CARTESIAN_POINT('Ctrl Pts',(3.90923382524985,-18.6400600347302,-318.25)) ;
#49833 = CARTESIAN_POINT('Ctrl Pts',(3.96405242176188,-18.6297432186077,-318.25)) ;
#49834 = CARTESIAN_POINT('Ctrl Pts',(4.01883753596892,-18.6191821067855,-318.25)) ;
#49835 = CARTESIAN_POINT('Ctrl Pts',(4.07358761785632,-18.6083770923689,-318.25)) ;
#49836 = CARTESIAN_POINT('Ctrl Pts',(4.11408126063228,-18.6003856085411,-318.25)) ;
#49837 = CARTESIAN_POINT('Ctrl Pts',(4.15454833823327,-18.5922621474935,-318.25)) ;
#49838 = CARTESIAN_POINT('Ctrl Pts',(4.19498041797789,-18.5840086585812,-318.25)) ;
#49839 = CARTESIAN_POINT('Ctrl Pts',(4.5873287012649,-18.5039177449713,-318.25)) ;
#49840 = CARTESIAN_POINT('Ctrl Pts',(4.97661118933657,-18.41154179864,-318.25)) ;
#49841 = CARTESIAN_POINT('Ctrl Pts',(5.36229079546034,-18.3072214478284,-318.25)) ;
#49842 = CARTESIAN_POINT('Ctrl Pts',(5.75194592399491,-18.2018257798727,-318.25)) ;
#49843 = CARTESIAN_POINT('Ctrl Pts',(6.13792402250833,-18.0842380932291,-318.25)) ;
#49844 = CARTESIAN_POINT('Ctrl Pts',(6.51967037800299,-17.9547561950956,-318.25)) ;
#49845 = CARTESIAN_POINT('Ctrl Pts',(6.90358541881112,-17.8245387156349,-318.25)) ;
#49846 = CARTESIAN_POINT('Ctrl Pts',(7.28322103399168,-17.6822913566917,-318.25)) ;
#49847 = CARTESIAN_POINT('Ctrl Pts',(7.65800424636563,-17.5282651576925,-318.25)) ;
#49848 = CARTESIAN_POINT('Ctrl Pts',(8.03220348541031,-17.3744789566154,-318.25)) ;
#49849 = CARTESIAN_POINT('Ctrl Pts',(8.40156595799478,-17.2089503963534,-318.25)) ;
#49850 = CARTESIAN_POINT('Ctrl Pts',(8.76550470726295,-17.0318804289941,-318.25)) ;
#49851 = CARTESIAN_POINT('Ctrl Pts',(9.12717779683322,-16.8559127907754,-318.25)) ;
#49852 = CARTESIAN_POINT('Ctrl Pts',(9.48349498176718,-16.6685467769557,-318.25)) ;
#49853 = CARTESIAN_POINT('Ctrl Pts',(9.83385611329522,-16.4699344361079,-318.25)) ;
#49854 = CARTESIAN_POINT('Ctrl Pts',(10.0813465717466,-16.3296373116064,-318.25)) ;
#49855 = CARTESIAN_POINT('Ctrl Pts',(10.3258645793787,-16.1837275282184,-318.25)) ;
#49856 = CARTESIAN_POINT('Ctrl Pts',(10.5671892199504,-16.032245835092,-318.25)) ;
#49857 = CARTESIAN_POINT('Ctrl Pts',(10.6765018800387,-15.963629274466,-318.25)) ;
#49858 = CARTESIAN_POINT('Ctrl Pts',(10.7851592047769,-15.8938693215666,-318.25)) ;
#49859 = CARTESIAN_POINT('Ctrl Pts',(10.8931400466771,-15.8229690739819,-318.25)) ;
#49860 = CARTESIAN_POINT('Ctrl Pts',(10.9341643065962,-15.7960325347398,-318.25)) ;
#49861 = CARTESIAN_POINT('Ctrl Pts',(10.9750910749037,-15.7689312332667,-318.25)) ;
#49862 = CARTESIAN_POINT('Ctrl Pts',(11.0159020260381,-15.741676964968,-318.25)) ;
#49863 = CARTESIAN_POINT('Ctrl Pts',(11.1048166349595,-15.6822982310779,-318.25)) ;
#49864 = CARTESIAN_POINT('Ctrl Pts',(11.193201856226,-15.6221801352337,-318.25)) ;
#49865 = CARTESIAN_POINT('Ctrl Pts',(11.2810474222442,-15.5613272740523,-318.25)) ;
#49866 = CARTESIAN_POINT('Ctrl Pts',(11.6127958778286,-15.3315166685784,-318.25)) ;
#49867 = CARTESIAN_POINT('Ctrl Pts',(11.93684968069,-15.0912306318534,-318.25)) ;
#49868 = CARTESIAN_POINT('Ctrl Pts',(12.2528839901575,-14.8410069253261,-318.25)) ;
#49869 = CARTESIAN_POINT('Ctrl Pts',(12.5712207270902,-14.5889602460483,-318.25)) ;
#49870 = CARTESIAN_POINT('Ctrl Pts',(12.8814210852045,-14.326830220857,-318.25)) ;
#49871 = CARTESIAN_POINT('Ctrl Pts',(13.1831255705581,-14.0551207702151,-318.25)) ;
#49872 = CARTESIAN_POINT('Ctrl Pts',(13.4861015156718,-13.7822662665505,-318.25)) ;
#49873 = CARTESIAN_POINT('Ctrl Pts',(13.7805102252478,-13.4997510463041,-318.25)) ;
#49874 = CARTESIAN_POINT('Ctrl Pts',(14.0659540990013,-13.2080450727856,-318.25)) ;
#49875 = CARTESIAN_POINT('Ctrl Pts',(14.2780380061313,-12.9913084450785,-318.25)) ;
#49876 = CARTESIAN_POINT('Ctrl Pts',(14.4851722654754,-12.7694972480152,-318.25)) ;
#49877 = CARTESIAN_POINT('Ctrl Pts',(14.687179910341,-12.5427918149033,-318.25)) ;
#49878 = CARTESIAN_POINT('Ctrl Pts',(14.7184668118549,-12.5076797251448,-318.25)) ;
#49879 = CARTESIAN_POINT('Ctrl Pts',(14.7496291449813,-12.4724519303098,-318.25)) ;
#49880 = CARTESIAN_POINT('Ctrl Pts',(14.7806583427305,-12.4371182641492,-318.25)) ;
#49881 = CARTESIAN_POINT('Ctrl Pts',(15.0525159971116,-12.1275476564679,-318.25)) ;
#49882 = CARTESIAN_POINT('Ctrl Pts',(15.3143205432749,-11.8096706771766,-318.25)) ;
#49883 = CARTESIAN_POINT('Ctrl Pts',(15.5657126298465,-11.4840113666617,-318.25)) ;
#49884 = CARTESIAN_POINT('Ctrl Pts',(15.8161453061597,-11.1595948990998,-318.25)) ;
#49885 = CARTESIAN_POINT('Ctrl Pts',(16.0562445808496,-10.8274556378891,-318.25)) ;
#49886 = CARTESIAN_POINT('Ctrl Pts',(16.2856173638454,-10.4880756432578,-318.25)) ;
#49887 = CARTESIAN_POINT('Ctrl Pts',(16.5163082412145,-10.1467453960488,-318.25)) ;
#49888 = CARTESIAN_POINT('Ctrl Pts',(16.7361494174162,-9.79809056298881,-318.25)) ;
#49889 = CARTESIAN_POINT('Ctrl Pts',(16.9446986253785,-9.44256919289982,-318.25)) ;
#49890 = CARTESIAN_POINT('Ctrl Pts',(17.1532478333407,-9.08704782281084,-318.25)) ;
#49891 = CARTESIAN_POINT('Ctrl Pts',(17.3505054705389,-8.72465948814614,-318.25)) ;
#49892 = CARTESIAN_POINT('Ctrl Pts',(17.5359809117574,-8.35583619169791,-318.25)) ;
#49893 = CARTESIAN_POINT('Ctrl Pts',(-15.1166752930756,-10.7787117730376,
-318.249803151889)) ;
#49894 = CARTESIAN_POINT('Ctrl Pts',(-15.1223425749755,-10.7707636562237,
-318.249868767926)) ;
#49895 = CARTESIAN_POINT('Ctrl Pts',(-15.1280035883766,-10.7628110697536,
-318.249934383963)) ;
#49896 = CARTESIAN_POINT('Ctrl Pts',(-15.1336583262364,-10.7548540235205,
-318.25)) ;
#49897 = CARTESIAN_POINT('Ctrl Pts',(-15.8220589029561,11.2756047307133,-317.75179962416)) ;
#49898 = CARTESIAN_POINT('Ctrl Pts',(-13.9462169600666,13.9078331685254,-317.791516068309)) ;
#49899 = CARTESIAN_POINT('Ctrl Pts',(-8.85808512633525,18.2140200078628,-317.870930498241)) ;
#49900 = CARTESIAN_POINT('Ctrl Pts',(0.938245705209947,20.23155285505,-317.990042913955)) ;
#49901 = CARTESIAN_POINT('Ctrl Pts',(10.502550121817,17.3171363004613,-318.1091368713)) ;
#49902 = CARTESIAN_POINT('Ctrl Pts',(17.5078290499764,10.1819492314241,-318.228230828646)) ;
#49903 = CARTESIAN_POINT('Ctrl Pts',(20.2452775605918,0.564912754706648,-318.347324785991)) ;
#49904 = CARTESIAN_POINT('Ctrl Pts',(18.048297052031,-9.18978081702363,-318.466418743337)) ;
#49905 = CARTESIAN_POINT('Ctrl Pts',(11.4520790521312,-16.7045512834906,-318.585512700682)) ;
#49906 = CARTESIAN_POINT('Ctrl Pts',(2.06455022100158,-20.1477034639439,-318.704606658028)) ;
#49907 = CARTESIAN_POINT('Ctrl Pts',(-7.82622053472994,-18.68000717547,-318.823700615374)) ;
#49908 = CARTESIAN_POINT('Ctrl Pts',(-15.809397178503,-12.6591964182232,-318.942794572719)) ;
#49909 = CARTESIAN_POINT('Ctrl Pts',(-19.9391565068373,-3.55280184418553,
-319.061888530065)) ;
#49910 = CARTESIAN_POINT('Ctrl Pts',(-19.2088924586792,6.4195621534048,-319.18098248741)) ;
#49911 = CARTESIAN_POINT('Ctrl Pts',(-13.7966053168245,14.8272055077051,-319.300076444756)) ;
#49912 = CARTESIAN_POINT('Ctrl Pts',(-5.02149786345424,19.6208281495811,-319.419170402102)) ;
#49913 = CARTESIAN_POINT('Ctrl Pts',(4.97756197041771,19.6320201345031,-319.538264359447)) ;
#49914 = CARTESIAN_POINT('Ctrl Pts',(13.7633783186503,14.8580535757075,-319.657358316793)) ;
#49915 = CARTESIAN_POINT('Ctrl Pts',(19.1944737272763,6.46254719947798,-319.776452274138)) ;
#49916 = CARTESIAN_POINT('Ctrl Pts',(19.9470592755585,-3.50815687829998,-319.895546231484)) ;
#49917 = CARTESIAN_POINT('Ctrl Pts',(15.8376977971645,-12.623773869973,-320.014640188829)) ;
#49918 = CARTESIAN_POINT('Ctrl Pts',(7.86801554435696,-18.6624400785269,-320.133734146175)) ;
#49919 = CARTESIAN_POINT('Ctrl Pts',(-2.01943685201295,-20.152275630516,-320.252828103521)) ;
#49920 = CARTESIAN_POINT('Ctrl Pts',(-11.4146665670295,-16.7301442145837,
-320.371922060866)) ;
#49921 = CARTESIAN_POINT('Ctrl Pts',(-18.0276563934026,-9.23016485487467,
-320.491016018212)) ;
#49922 = CARTESIAN_POINT('Ctrl Pts',(-20.2465393536469,0.51959838559575,-320.610109975557)) ;
#49923 = CARTESIAN_POINT('Ctrl Pts',(-17.5304792666225,10.1427133926868,-320.729203932903)) ;
#49924 = CARTESIAN_POINT('Ctrl Pts',(-10.5414955324265,17.2936176152543,-320.848297890248)) ;
#49925 = CARTESIAN_POINT('Ctrl Pts',(-0.983100839741991,20.2293314526664,
-320.967391847594)) ;
#49926 = CARTESIAN_POINT('Ctrl Pts',(8.81491735450798,18.2342965402073,-321.086485804939)) ;
#49927 = CARTESIAN_POINT('Ctrl Pts',(16.4643651509713,11.7947877665687,-321.205579762285)) ;
#49928 = CARTESIAN_POINT('Ctrl Pts',(20.1007466691207,2.48038739450463,-321.324673719631)) ;
#49929 = CARTESIAN_POINT('Ctrl Pts',(18.8377210198965,-7.43858891588363,-321.443767676976)) ;
#49930 = CARTESIAN_POINT('Ctrl Pts',(12.9831412905652,-15.5444646261037,-321.562861634322)) ;
#49931 = CARTESIAN_POINT('Ctrl Pts',(3.96401764945386,-19.861492953899,-321.681955591667)) ;
#49932 = CARTESIAN_POINT('Ctrl Pts',(-6.02130574547807,-19.3374304239844,
-321.801049549013)) ;
#49933 = CARTESIAN_POINT('Ctrl Pts',(-14.5389807484402,-14.1000133716053,
-321.920143506359)) ;
#49934 = CARTESIAN_POINT('Ctrl Pts',(-19.5128875691681,-5.4258231629833,-322.039237463704)) ;
#49935 = CARTESIAN_POINT('Ctrl Pts',(-19.7306734961704,4.57087099691963,-322.15833142105)) ;
#49936 = CARTESIAN_POINT('Ctrl Pts',(-15.1392548331411,13.45344942311,-322.277425378395)) ;
#49937 = CARTESIAN_POINT('Ctrl Pts',(-6.85775565424215,19.0568498359428,-322.396519335741)) ;
#49938 = CARTESIAN_POINT('Ctrl Pts',(3.09527034689612,20.0152851531671,-322.515613293086)) ;
#49939 = CARTESIAN_POINT('Ctrl Pts',(12.2938472734718,16.095143910494,-322.634707250432)) ;
#49940 = CARTESIAN_POINT('Ctrl Pts',(18.4958905668593,8.25193131465147,-322.753801207777)) ;
#49941 = CARTESIAN_POINT('Ctrl Pts',(20.189698405024,-1.60262802831304,-322.872895165123)) ;
#49942 = CARTESIAN_POINT('Ctrl Pts',(16.9624177532472,-11.0665587355458,-322.991989122469)) ;
#49943 = CARTESIAN_POINT('Ctrl Pts',(9.60067421388661,-17.8330982423632,-323.111083079814)) ;
#49944 = CARTESIAN_POINT('Ctrl Pts',(-0.101162100603281,-20.2529529825249,
-323.23017703716)) ;
#49945 = CARTESIAN_POINT('Ctrl Pts',(-9.7783409071448,-17.7363014009861,-323.349270994505)) ;
#49946 = CARTESIAN_POINT('Ctrl Pts',(-17.0721220064229,-10.8965585613429,
-323.468364951851)) ;
#49947 = CARTESIAN_POINT('Ctrl Pts',(-20.2047006241534,-1.40086079654568,
-323.587458909197)) ;
#49948 = CARTESIAN_POINT('Ctrl Pts',(-18.4125340728579,8.43628634523557,-323.706552866542)) ;
#49949 = CARTESIAN_POINT('Ctrl Pts',(-12.1324495904037,16.2171515753931,-323.825646823888)) ;
#49950 = CARTESIAN_POINT('Ctrl Pts',(-2.89517095693271,20.0452069935208,-323.944740781233)) ;
#49951 = CARTESIAN_POINT('Ctrl Pts',(7.04778401636063,18.9873926262059,-324.063834738579)) ;
#49952 = CARTESIAN_POINT('Ctrl Pts',(15.2728941706411,13.3015428404137,-324.182928695924)) ;
#49953 = CARTESIAN_POINT('Ctrl Pts',(19.7753502166989,4.37354113846764,-324.30202265327)) ;
#49954 = CARTESIAN_POINT('Ctrl Pts',(19.4577120551217,-5.62047861511239,-324.421116610615)) ;
#49955 = CARTESIAN_POINT('Ctrl Pts',(14.3974016200832,-14.2445486019387,-324.54021056796)) ;
#49956 = CARTESIAN_POINT('Ctrl Pts',(5.8278318600006,-19.3966160475101,-324.659304525307)) ;
#49957 = CARTESIAN_POINT('Ctrl Pts',(-4.16222847464273,-19.820902916059,-324.778398482652)) ;
#49958 = CARTESIAN_POINT('Ctrl Pts',(-13.1377766443113,-15.4139924460587,
-324.897492439998)) ;
#49959 = CARTESIAN_POINT('Ctrl Pts',(-18.9110896873939,-7.25003621496531,
-325.016586397343)) ;
#49960 = CARTESIAN_POINT('Ctrl Pts',(-20.0749655845643,2.6810623009403,-325.135680354689)) ;
#49961 = CARTESIAN_POINT('Ctrl Pts',(-16.345718261549,11.9586718659317,-325.254774312035)) ;
#49962 = CARTESIAN_POINT('Ctrl Pts',(-8.63232395510391,18.3214443048877,-325.37386826938)) ;
#49963 = CARTESIAN_POINT('Ctrl Pts',(1.18513496908386,20.2185012646342,-325.492962226726)) ;
#49964 = CARTESIAN_POINT('Ctrl Pts',(10.7137260786869,17.1874492521093,-325.612056184072)) ;
#49965 = CARTESIAN_POINT('Ctrl Pts',(17.6309263179295,9.96708460156269,-325.731150141417)) ;
#49966 = CARTESIAN_POINT('Ctrl Pts',(20.2507196900847,0.31731737515523,-325.850244098763)) ;
#49967 = CARTESIAN_POINT('Ctrl Pts',(17.9345510889248,-9.40979359612691,-325.969338056107)) ;
#49968 = CARTESIAN_POINT('Ctrl Pts',(11.2469693460007,-16.8433375200132,-326.088432013454)) ;
#49969 = CARTESIAN_POINT('Ctrl Pts',(1.81802266116369,-20.171443475529,-326.207525970799)) ;
#49970 = CARTESIAN_POINT('Ctrl Pts',(-8.05405349558649,-18.5829104440933,
-326.326619928145)) ;
#49971 = CARTESIAN_POINT('Ctrl Pts',(-15.9630141486082,-12.4649315110151,
-326.44571388549)) ;
#49972 = CARTESIAN_POINT('Ctrl Pts',(-19.98110909301,-3.30871843712862,-326.564807842836)) ;
#49973 = CARTESIAN_POINT('Ctrl Pts',(-19.1289576374257,6.65397009224849,-326.683901800182)) ;
#49974 = CARTESIAN_POINT('Ctrl Pts',(-13.614265347121,14.9948030110817,-326.802995757527)) ;
#49975 = CARTESIAN_POINT('Ctrl Pts',(-4.78119736072094,19.6807644689122,-326.922089714873)) ;
#49976 = CARTESIAN_POINT('Ctrl Pts',(5.21725184277175,19.5696862900778,-327.041183672218)) ;
#49977 = CARTESIAN_POINT('Ctrl Pts',(13.944034799571,14.6886429526801,-327.160277629564)) ;
#49978 = CARTESIAN_POINT('Ctrl Pts',(19.2720632143789,6.22735238636345,-327.279371586909)) ;
#49979 = CARTESIAN_POINT('Ctrl Pts',(19.9026698768091,-3.75180890474398,-327.398465544254)) ;
#49980 = CARTESIAN_POINT('Ctrl Pts',(15.6821491135074,-12.8164947417256,-327.5175595016)) ;
#49981 = CARTESIAN_POINT('Ctrl Pts',(7.639221400292,-18.7572555210053,-327.636653458946)) ;
#49982 = CARTESIAN_POINT('Ctrl Pts',(-2.26570958562885,-20.1260750857328,
-327.755747416291)) ;
#49983 = CARTESIAN_POINT('Ctrl Pts',(-11.6183907489069,-16.5893138703406,
-327.874841373638)) ;
#49984 = CARTESIAN_POINT('Ctrl Pts',(-18.1391757719305,-9.00903105766491,
-327.993935330983)) ;
#49985 = CARTESIAN_POINT('Ctrl Pts',(-20.2386719120029,0.76713592098574,-328.113029288328)) ;
#49986 = CARTESIAN_POINT('Ctrl Pts',(-17.4051426348618,10.3563192372135,-328.232123245674)) ;
#49987 = CARTESIAN_POINT('Ctrl Pts',(-10.3292395803644,17.4212269365392,-328.351217203019)) ;
#49988 = CARTESIAN_POINT('Ctrl Pts',(-0.735661373466894,20.2398404298689,
-328.470311160365)) ;
#49989 = CARTESIAN_POINT('Ctrl Pts',(9.03722880951048,18.1251436884654,-328.589405117711)) ;
#49990 = CARTESIAN_POINT('Ctrl Pts',(16.6073618346899,11.5925782798587,-328.708499075056)) ;
#49991 = CARTESIAN_POINT('Ctrl Pts',(20.1295742058069,2.23440832791899,-328.827593032402)) ;
#49992 = CARTESIAN_POINT('Ctrl Pts',(18.7453529123693,-7.66838199841982,-328.946686989747)) ;
#49993 = CARTESIAN_POINT('Ctrl Pts',(12.7920915765111,-15.702061373626,-329.065780947093)) ;
#49994 = CARTESIAN_POINT('Ctrl Pts',(3.72085327256795,-19.9084803339427,-329.18487490444)) ;
#49995 = CARTESIAN_POINT('Ctrl Pts',(-6.25731528090481,-19.2623556129129,
-329.303968861784)) ;
#49996 = CARTESIAN_POINT('Ctrl Pts',(-14.7103098773889,-13.9211752950014,
-329.42306281913)) ;
#49997 = CARTESIAN_POINT('Ctrl Pts',(-19.5777760935643,-5.1868122689399,-329.542156776475)) ;
#49998 = CARTESIAN_POINT('Ctrl Pts',(-19.6733053218788,4.81179758459352,-329.661250733821)) ;
#49999 = CARTESIAN_POINT('Ctrl Pts',(-14.9736130250163,13.6375676445628,-329.780344691166)) ;
#50000 = CARTESIAN_POINT('Ctrl Pts',(-6.6242141683021,19.1392822471332,-329.899438648512)) ;
#50001 = CARTESIAN_POINT('Ctrl Pts',(3.33978751429805,19.975939468328,-330.018532605858)) ;
#50002 = CARTESIAN_POINT('Ctrl Pts',(12.4897408854399,15.9436103470178,-330.137626563203)) ;
#50003 = CARTESIAN_POINT('Ctrl Pts',(18.5954130156895,8.02514504908728,-330.256720520549)) ;
#50004 = CARTESIAN_POINT('Ctrl Pts',(20.1685918356652,-1.84938953422425,-330.375814477894)) ;
#50005 = CARTESIAN_POINT('Ctrl Pts',(16.8258267346502,-11.2731492041263,-330.49490843524)) ;
#50006 = CARTESIAN_POINT('Ctrl Pts',(9.38189178866938,-17.9491627868451,-330.614002392586)) ;
#50007 = CARTESIAN_POINT('Ctrl Pts',(-0.348809347122767,-20.2502017353488,
-330.733096349931)) ;
#50008 = CARTESIAN_POINT('Ctrl Pts',(-9.99449080461785,-17.6154049581431,
-330.852190307277)) ;
#50009 = CARTESIAN_POINT('Ctrl Pts',(-17.2040896285461,-10.6869845296003,
-330.971284264622)) ;
#50010 = CARTESIAN_POINT('Ctrl Pts',(-20.2203198467357,-1.15369128395224,
-331.090378221968)) ;
#50011 = CARTESIAN_POINT('Ctrl Pts',(-18.3079978268224,8.66080561241441,-331.209472179313)) ;
#50012 = CARTESIAN_POINT('Ctrl Pts',(-11.9332378064965,16.3642956993744,-331.328566136659)) ;
#50013 = CARTESIAN_POINT('Ctrl Pts',(-2.64984002253427,20.0791106909131,-331.447660094004)) ;
#50014 = CARTESIAN_POINT('Ctrl Pts',(7.27943651471512,18.8997921234915,-331.56675405135)) ;
#50015 = CARTESIAN_POINT('Ctrl Pts',(15.4344046632414,13.1137901071458,-331.685848008696)) ;
#50016 = CARTESIAN_POINT('Ctrl Pts',(19.8273517248913,4.13139950384977,-331.804941966041)) ;
#50017 = CARTESIAN_POINT('Ctrl Pts',(19.3875295989093,-5.85798893259291,-331.924035923387)) ;
#50018 = CARTESIAN_POINT('Ctrl Pts',(14.2221416500197,-14.4195362328246,-332.043129880732)) ;
#50019 = CARTESIAN_POINT('Ctrl Pts',(5.59021268738151,-19.4664290611504,-332.162223838078)) ;
#50020 = CARTESIAN_POINT('Ctrl Pts',(-4.4042889477316,-19.768524910773,-332.281317795423)) ;
#50021 = CARTESIAN_POINT('Ctrl Pts',(-13.3252779819004,-15.2521901702032,
-332.400411752769)) ;
#50022 = CARTESIAN_POINT('Ctrl Pts',(-18.998329836102,-7.01824776718787,-332.519505710115)) ;
#50023 = CARTESIAN_POINT('Ctrl Pts',(-20.0406804084418,2.92634021427114,-332.63859966746)) ;
#50024 = CARTESIAN_POINT('Ctrl Pts',(-16.1982645167102,12.1576545817708,-332.757693624806)) ;
#50025 = CARTESIAN_POINT('Ctrl Pts',(-8.4076423927164,18.4256312694888,-332.876787582151)) ;
#50026 = CARTESIAN_POINT('Ctrl Pts',(1.43227989298982,20.2024976819972,-332.995881539497)) ;
#50027 = CARTESIAN_POINT('Ctrl Pts',(10.9230946311552,17.0551558762091,-333.114975496841)) ;
#50028 = CARTESIAN_POINT('Ctrl Pts',(17.7514864749526,9.75074695664578,-333.234069454188)) ;
#50029 = CARTESIAN_POINT('Ctrl Pts',(20.2530858120576,0.0696661495647872,
-333.353163411534)) ;
#50030 = CARTESIAN_POINT('Ctrl Pts',(17.8181464512536,-9.62839526217338,-333.472257368879)) ;
#50031 = CARTESIAN_POINT('Ctrl Pts',(11.0401667114247,-16.9796070998983,-333.591351326225)) ;
#50032 = CARTESIAN_POINT('Ctrl Pts',(1.57122863033052,-20.1921662749243,-333.71044528357)) ;
#50033 = CARTESIAN_POINT('Ctrl Pts',(-8.28068471729155,-18.4830354351167,
-333.829539240916)) ;
#50034 = CARTESIAN_POINT('Ctrl Pts',(-16.1142428902293,-12.2688024826247,
-333.948633198262)) ;
#50035 = CARTESIAN_POINT('Ctrl Pts',(-20.0200744760529,-3.06414037802701,
-334.067727155607)) ;
#50036 = CARTESIAN_POINT('Ctrl Pts',(-19.0461621402262,6.88738310326793,-334.186821112953)) ;
#50037 = CARTESIAN_POINT('Ctrl Pts',(-13.4298897549544,15.1601582924693,-334.305915070298)) ;
#50038 = CARTESIAN_POINT('Ctrl Pts',(-4.54018184982169,19.7377579034077,-334.425009027644)) ;
#50039 = CARTESIAN_POINT('Ctrl Pts',(5.45616153817922,19.5044261528559,-334.544102984989)) ;
#50040 = CARTESIAN_POINT('Ctrl Pts',(14.1226062220899,14.5170359157374,-334.663196942335)) ;
#50041 = CARTESIAN_POINT('Ctrl Pts',(19.3467709108636,5.99122638576585,-334.78229089968)) ;
#50042 = CARTESIAN_POINT('Ctrl Pts',(19.8553044031172,-3.99489991643816,-334.901384857026)) ;
#50043 = CARTESIAN_POINT('Ctrl Pts',(15.5242554507918,-13.0072991424903,-335.020478814372)) ;
#50044 = CARTESIAN_POINT('Ctrl Pts',(7.40928495186548,-18.8492661603349,-335.139572771717)) ;
#50045 = CARTESIAN_POINT('Ctrl Pts',(-2.51164352439901,-20.0968650563489,
-335.258666729063)) ;
#50046 = CARTESIAN_POINT('Ctrl Pts',(-11.8203776137382,-16.4460028987553,
-335.377760686408)) ;
#50047 = CARTESIAN_POINT('Ctrl Pts',(-18.2479827700008,-8.78655012580679,
-335.496854643754)) ;
#50048 = CARTESIAN_POINT('Ctrl Pts',(-20.2277781489081,1.0145587461582,-335.6159486011)) ;
#50049 = CARTESIAN_POINT('Ctrl Pts',(-17.277203383498,10.5683764826849,-335.735042558445)) ;
#50050 = CARTESIAN_POINT('Ctrl Pts',(-10.115439080935,17.5462312370861,-335.854136515791)) ;
#50051 = CARTESIAN_POINT('Ctrl Pts',(-0.488111901202637,20.2473229031516,
-335.973230473135)) ;
#50052 = CARTESIAN_POINT('Ctrl Pts',(9.25818891017889,18.0132805702995,-336.092324430482)) ;
#50053 = CARTESIAN_POINT('Ctrl Pts',(16.7478751983631,11.3886353032719,-336.211418387827)) ;
#50054 = CARTESIAN_POINT('Ctrl Pts',(20.1553917224645,1.98809521454014,-336.330512345173)) ;
#50055 = CARTESIAN_POINT('Ctrl Pts',(18.6501818066376,-7.89702855606564,-336.449606302519)) ;
#50056 = CARTESIAN_POINT('Ctrl Pts',(12.5991289885161,-15.8573098746684,-336.568700259864)) ;
#50057 = CARTESIAN_POINT('Ctrl Pts',(3.47713261749939,-19.9524913709672,-336.68779421721)) ;
#50058 = CARTESIAN_POINT('Ctrl Pts',(-6.49238937166023,-19.1843992178428,
-336.806888174555)) ;
#50059 = CARTESIAN_POINT('Ctrl Pts',(-14.8794388899768,-13.7402581581745,
-336.925982131901)) ;
#50060 = CARTESIAN_POINT('Ctrl Pts',(-19.6397380740326,-4.94702040317705,
-337.045076089246)) ;
#50061 = CARTESIAN_POINT('Ctrl Pts',(-19.6129933917417,5.05199350895541,-337.164170046592)) ;
#50062 = CARTESIAN_POINT('Ctrl Pts',(-14.8057362800649,13.8196697192246,-337.283264003938)) ;
#50063 = CARTESIAN_POINT('Ctrl Pts',(-6.38967367544487,19.2188048600104,-337.402357961283)) ;
#50064 = CARTESIAN_POINT('Ctrl Pts',(3.58378767615178,19.933705979741,-337.521451918629)) ;
#50065 = CARTESIAN_POINT('Ctrl Pts',(12.6838030107157,15.7894873221202,-337.640545875974)) ;
#50066 = CARTESIAN_POINT('Ctrl Pts',(18.6920739072665,7.79758994659989,-337.75963983332)) ;
#50067 = CARTESIAN_POINT('Ctrl Pts',(20.1448670002182,-2.09864690139803,-337.878756758576)) ;
#50068 = CARTESIAN_POINT('Ctrl Pts',(17.8370731701076,-8.35261194983006,-337.958175698051)) ;
#50069 = CARTESIAN_POINT('Ctrl Pts',(16.0042781108101,-11.015438797673,-337.997896651744)) ;
#50070 = CARTESIAN_POINT('Ctrl Pts',(-15.5872995250709,11.1083032456097,-317.918234548891)) ;
#50071 = CARTESIAN_POINT('Ctrl Pts',(-13.7392903370854,13.7014760640297,-317.957950993041)) ;
#50072 = CARTESIAN_POINT('Ctrl Pts',(-8.72665352402181,17.943769970743,-318.037365422973)) ;
#50073 = CARTESIAN_POINT('Ctrl Pts',(0.924324509529332,19.9313677280047,-318.156477838686)) ;
#50074 = CARTESIAN_POINT('Ctrl Pts',(10.346718813899,17.0601937514806,-318.275571796032)) ;
#50075 = CARTESIAN_POINT('Ctrl Pts',(17.2480571023999,10.0308748306847,-318.394665753377)) ;
#50076 = CARTESIAN_POINT('Ctrl Pts',(19.9448887935932,0.556530876743228,-318.513759710723)) ;
#50077 = CARTESIAN_POINT('Ctrl Pts',(17.7805059248579,-9.05342768872738,-318.632853668069)) ;
#50078 = CARTESIAN_POINT('Ctrl Pts',(11.28215913398,-16.4566979483958,-318.751947625414)) ;
#50079 = CARTESIAN_POINT('Ctrl Pts',(2.03391751204327,-19.8487624500075,-318.871041582759)) ;
#50080 = CARTESIAN_POINT('Ctrl Pts',(-7.71009919583251,-18.4028430661526,
-318.990135540105)) ;
#50081 = CARTESIAN_POINT('Ctrl Pts',(-15.5748256686173,-12.471365928279,-319.109229497451)) ;
#50082 = CARTESIAN_POINT('Ctrl Pts',(-19.6433098028266,-3.50008724137647,
-319.228323454796)) ;
#50083 = CARTESIAN_POINT('Ctrl Pts',(-18.9238810280478,6.32431207080355,-319.347417412142)) ;
#50084 = CARTESIAN_POINT('Ctrl Pts',(-13.5918985526182,14.6072072405951,-319.466511369487)) ;
#50085 = CARTESIAN_POINT('Ctrl Pts',(-4.94699152254709,19.3297046340993,-319.585605326833)) ;
#50086 = CARTESIAN_POINT('Ctrl Pts',(4.90370752715424,19.3407305582428,-319.704699284178)) ;
#50087 = CARTESIAN_POINT('Ctrl Pts',(13.5591645591451,14.6375976012094,-319.823793241524)) ;
#50088 = CARTESIAN_POINT('Ctrl Pts',(18.9096762341886,6.36665932739958,-319.94288719887)) ;
#50089 = CARTESIAN_POINT('Ctrl Pts',(19.6510953144271,-3.45610469398413,-320.061981156216)) ;
#50090 = CARTESIAN_POINT('Ctrl Pts',(15.6027063776026,-12.4364689611457,-320.181075113561)) ;
#50091 = CARTESIAN_POINT('Ctrl Pts',(7.75127407311647,-18.3855366205428,-320.300169070907)) ;
#50092 = CARTESIAN_POINT('Ctrl Pts',(-1.9894735114664,-19.8532667771799,-320.419263028252)) ;
#50093 = CARTESIAN_POINT('Ctrl Pts',(-11.2453017556306,-16.481911145055,-320.538356985598)) ;
#50094 = CARTESIAN_POINT('Ctrl Pts',(-17.7601715214524,-9.09321252949154,
-320.657450942943)) ;
#50095 = CARTESIAN_POINT('Ctrl Pts',(-19.9461318648274,0.511888858378053,
-320.776544900289)) ;
#50096 = CARTESIAN_POINT('Ctrl Pts',(-17.2703712470592,9.99222115266052,-320.895638857634)) ;
#50097 = CARTESIAN_POINT('Ctrl Pts',(-10.3850863730149,17.0370240241393,-321.01473281498)) ;
#50098 = CARTESIAN_POINT('Ctrl Pts',(-0.968514107196489,19.9291792856197,
-321.133826772326)) ;
#50099 = CARTESIAN_POINT('Ctrl Pts',(8.68412625286022,17.9637456505785,-321.252920729671)) ;
#50100 = CARTESIAN_POINT('Ctrl Pts',(16.2200755712257,11.6197829169879,-321.372014687017)) ;
#50101 = CARTESIAN_POINT('Ctrl Pts',(19.8025023753778,2.44358471255154,-321.491108644362)) ;
#50102 = CARTESIAN_POINT('Ctrl Pts',(18.5582168356097,-7.32821905081441,-321.610202601708)) ;
#50103 = CARTESIAN_POINT('Ctrl Pts',(12.790504277199,-15.3138240459134,-321.729296559053)) ;
#50104 = CARTESIAN_POINT('Ctrl Pts',(3.9052016430782,-19.5667985807883,-321.848390516399)) ;
#50105 = CARTESIAN_POINT('Ctrl Pts',(-5.93196478173024,-19.0505118147137,
-321.967484473744)) ;
#50106 = CARTESIAN_POINT('Ctrl Pts',(-14.3232590085248,-13.890804798461,-322.08657843109)) ;
#50107 = CARTESIAN_POINT('Ctrl Pts',(-19.2233656191755,-5.34531765620506,
-322.205672388436)) ;
#50108 = CARTESIAN_POINT('Ctrl Pts',(-19.4379201532821,4.50305082015176,-322.324766345781)) ;
#50109 = CARTESIAN_POINT('Ctrl Pts',(-14.9146265424696,13.253834225344,-322.443860303127)) ;
#50110 = CARTESIAN_POINT('Ctrl Pts',(-6.75600388723424,18.7740943336799,-322.562954260472)) ;
#50111 = CARTESIAN_POINT('Ctrl Pts',(3.04934435550142,19.7183088923925,-322.682048217818)) ;
#50112 = CARTESIAN_POINT('Ctrl Pts',(12.1114376417395,15.8563326410773,-322.801142175163)) ;
#50113 = CARTESIAN_POINT('Ctrl Pts',(18.2214582828222,8.12949350338674,-322.920236132509)) ;
#50114 = CARTESIAN_POINT('Ctrl Pts',(19.890134292267,-1.57884907759523,-323.039330089855)) ;
#50115 = CARTESIAN_POINT('Ctrl Pts',(16.7107383312702,-10.902358964832,-323.1584240472)) ;
#50116 = CARTESIAN_POINT('Ctrl Pts',(9.45822446574986,-17.5685001218012,-323.277518004546)) ;
#50117 = CARTESIAN_POINT('Ctrl Pts',(-0.0996611106279288,-19.9524503316576,
-323.396611961891)) ;
#50118 = CARTESIAN_POINT('Ctrl Pts',(-9.63325503417527,-17.473139500982,-323.515705919237)) ;
#50119 = CARTESIAN_POINT('Ctrl Pts',(-16.8188148505092,-10.7348811636893,
-323.634799876582)) ;
#50120 = CARTESIAN_POINT('Ctrl Pts',(-19.9049139163692,-1.38007556175934,
-323.753893833928)) ;
#50121 = CARTESIAN_POINT('Ctrl Pts',(-18.1393385885821,8.31111317111102,-323.872987791274)) ;
#50122 = CARTESIAN_POINT('Ctrl Pts',(-11.9524346924985,15.9765300204956,-323.992081748619)) ;
#50123 = CARTESIAN_POINT('Ctrl Pts',(-2.85221393491113,19.7477867682365,-324.111175705965)) ;
#50124 = CARTESIAN_POINT('Ctrl Pts',(6.94321270858724,18.7056676934439,-324.23026966331)) ;
#50125 = CARTESIAN_POINT('Ctrl Pts',(15.046283009856,13.1041815525256,-324.349363620656)) ;
#50126 = CARTESIAN_POINT('Ctrl Pts',(19.4819339841588,4.30864883822279,-324.468457578002)) ;
#50127 = CARTESIAN_POINT('Ctrl Pts',(19.1690087703503,-5.53708491324378,-324.587551535347)) ;
#50128 = CARTESIAN_POINT('Ctrl Pts',(14.1837805567168,-14.033195491161,-324.706645492693)) ;
#50129 = CARTESIAN_POINT('Ctrl Pts',(5.74136155987941,-19.1088192731257,-324.825739450038)) ;
#50130 = CARTESIAN_POINT('Ctrl Pts',(-4.10047152042356,-19.5268107965543,
-324.944833407384)) ;
#50131 = CARTESIAN_POINT('Ctrl Pts',(-12.9428452329993,-15.1852877433674,
-325.06392736473)) ;
#50132 = CARTESIAN_POINT('Ctrl Pts',(-18.6304968974559,-7.14246399557781,
-325.183021322075)) ;
#50133 = CARTESIAN_POINT('Ctrl Pts',(-19.7771038169774,2.64128211040375,-325.30211527942)) ;
#50134 = CARTESIAN_POINT('Ctrl Pts',(-16.1031891018673,11.7812353903884,-325.421209236766)) ;
#50135 = CARTESIAN_POINT('Ctrl Pts',(-8.50424207816021,18.0496003626199,-325.540303194112)) ;
#50136 = CARTESIAN_POINT('Ctrl Pts',(1.1675505605212,19.9185097902143,-325.659397151457)) ;
#50137 = CARTESIAN_POINT('Ctrl Pts',(10.554761453129,16.9324309312569,-325.778491108803)) ;
#50138 = CARTESIAN_POINT('Ctrl Pts',(17.3693279179155,9.81919824905043,-325.897585066149)) ;
#50139 = CARTESIAN_POINT('Ctrl Pts',(19.9502501756347,0.312609187046404,-326.016679023494)) ;
#50140 = CARTESIAN_POINT('Ctrl Pts',(17.668447664452,-9.27017603407612,-326.13577298084)) ;
#50141 = CARTESIAN_POINT('Ctrl Pts',(11.0800927376556,-16.5934249478277,-326.254866938185)) ;
#50142 = CARTESIAN_POINT('Ctrl Pts',(1.7910477983134,-19.8721502198024,-326.373960895531)) ;
#50143 = CARTESIAN_POINT('Ctrl Pts',(-7.93455169119587,-18.3071870049437,
-326.493054852876)) ;
#50144 = CARTESIAN_POINT('Ctrl Pts',(-15.726163351017,-12.2799834214614,-326.612148810222)) ;
#50145 = CARTESIAN_POINT('Ctrl Pts',(-19.6846399186186,-3.25962541537577,
-326.731242767567)) ;
#50146 = CARTESIAN_POINT('Ctrl Pts',(-18.8451322375774,6.55524198809318,-326.850336724913)) ;
#50147 = CARTESIAN_POINT('Ctrl Pts',(-13.4122640473623,14.7723180204756,-326.969430682259)) ;
#50148 = CARTESIAN_POINT('Ctrl Pts',(-4.71025647212775,19.3887516498875,-327.088524639604)) ;
#50149 = CARTESIAN_POINT('Ctrl Pts',(5.13984100740629,19.2793215905752,-327.20761859695)) ;
#50150 = CARTESIAN_POINT('Ctrl Pts',(13.7371405543381,14.4707006037923,-327.326712554295)) ;
#50151 = CARTESIAN_POINT('Ctrl Pts',(18.9861144893412,6.13495421106516,-327.445806511641)) ;
#50152 = CARTESIAN_POINT('Ctrl Pts',(19.6073645422006,-3.69614153997029,-327.564900468986)) ;
#50153 = CARTESIAN_POINT('Ctrl Pts',(15.4494656433997,-12.6263303420928,-327.683994426332)) ;
#50154 = CARTESIAN_POINT('Ctrl Pts',(7.52587465607497,-18.4789452414169,-327.803088383677)) ;
#50155 = CARTESIAN_POINT('Ctrl Pts',(-2.23209217995158,-19.8274549822824,
-327.922182341023)) ;
#50156 = CARTESIAN_POINT('Ctrl Pts',(-11.4460031853812,-16.3431703672965,
-328.041276298369)) ;
#50157 = CARTESIAN_POINT('Ctrl Pts',(-17.8700362341696,-8.87535979911265,
-328.160370255714)) ;
#50158 = CARTESIAN_POINT('Ctrl Pts',(-19.9383811561395,0.755753562174654,
-328.27946421306)) ;
#50159 = CARTESIAN_POINT('Ctrl Pts',(-17.1468942942365,10.2026576261539,-328.398558170406)) ;
#50160 = CARTESIAN_POINT('Ctrl Pts',(-10.1759797629925,17.1627399455159,-328.517652127751)) ;
#50161 = CARTESIAN_POINT('Ctrl Pts',(-0.724746017416909,19.9395323361526,
-328.636746085097)) ;
#50162 = CARTESIAN_POINT('Ctrl Pts',(8.9031391675657,17.8562123513694,-328.755840042442)) ;
#50163 = CARTESIAN_POINT('Ctrl Pts',(16.3609505454551,11.4205737081554,-328.874933999788)) ;
#50164 = CARTESIAN_POINT('Ctrl Pts',(19.8309021842556,2.20125535381989,-328.994027957133)) ;
#50165 = CARTESIAN_POINT('Ctrl Pts',(18.4672192374198,-7.55460258460419,-329.113121914479)) ;
#50166 = CARTESIAN_POINT('Ctrl Pts',(12.6022892581927,-15.4690824558886,-329.232215871825)) ;
#50167 = CARTESIAN_POINT('Ctrl Pts',(3.66564521116278,-19.613088786831,-329.35130982917)) ;
#50168 = CARTESIAN_POINT('Ctrl Pts',(-6.16447253195624,-18.9765509241537,
-329.470403786516)) ;
#50169 = CARTESIAN_POINT('Ctrl Pts',(-14.4920460460825,-13.7146202270592,
-329.589497743861)) ;
#50170 = CARTESIAN_POINT('Ctrl Pts',(-19.2872913618179,-5.10985307994102,
-329.708591701207)) ;
#50171 = CARTESIAN_POINT('Ctrl Pts',(-19.3814031777496,4.74040266599305,-329.827685658552)) ;
#50172 = CARTESIAN_POINT('Ctrl Pts',(-14.7514424402645,13.435220597586,-329.946779615898)) ;
#50173 = CARTESIAN_POINT('Ctrl Pts',(-6.52592756687639,18.8553036561632,-330.065873573244)) ;
#50174 = CARTESIAN_POINT('Ctrl Pts',(3.29023350593959,19.6795469981051,-330.184967530589)) ;
#50175 = CARTESIAN_POINT('Ctrl Pts',(12.3044246874535,15.7070474528163,-330.304061487935)) ;
#50176 = CARTESIAN_POINT('Ctrl Pts',(18.3195040699664,7.90607217300219,-330.42315544528)) ;
#50177 = CARTESIAN_POINT('Ctrl Pts',(19.8693408910694,-1.82194926622977,-330.542249402626)) ;
#50178 = CARTESIAN_POINT('Ctrl Pts',(16.5761739782765,-11.1058841528331,-330.661343359971)) ;
#50179 = CARTESIAN_POINT('Ctrl Pts',(9.24268821894413,-17.6828425616933,-330.780437317317)) ;
#50180 = CARTESIAN_POINT('Ctrl Pts',(-0.343633897718047,-19.9497399060383,
-330.899531274662)) ;
#50181 = CARTESIAN_POINT('Ctrl Pts',(-9.84619781329718,-17.3540368558921,
-331.018625232008)) ;
#50182 = CARTESIAN_POINT('Ctrl Pts',(-16.9488244065513,-10.5284166810652,
-331.137719189353)) ;
#50183 = CARTESIAN_POINT('Ctrl Pts',(-19.9203013891524,-1.13657342023086,
-331.256813146699)) ;
#50184 = CARTESIAN_POINT('Ctrl Pts',(-18.0363533963149,8.53230113963843,-331.375907104045)) ;
#50185 = CARTESIAN_POINT('Ctrl Pts',(-11.7561787081332,16.1214908974534,-331.49500106139)) ;
#50186 = CARTESIAN_POINT('Ctrl Pts',(-2.61052309172258,19.7811874204209,-331.614095018736)) ;
#50187 = CARTESIAN_POINT('Ctrl Pts',(7.17142806916257,18.6193669608572,-331.733188976082)) ;
#50188 = CARTESIAN_POINT('Ctrl Pts',(15.205397094821,12.9192145954406,-331.852282933427)) ;
#50189 = CARTESIAN_POINT('Ctrl Pts',(19.5331639213574,4.07009997366421,-331.971376890773)) ;
#50190 = CARTESIAN_POINT('Ctrl Pts',(19.099867644464,-5.77107117770977,-332.090470848118)) ;
#50191 = CARTESIAN_POINT('Ctrl Pts',(14.0111210017947,-14.2055867477309,-332.209564805464)) ;
#50192 = CARTESIAN_POINT('Ctrl Pts',(5.50726805541008,-19.1775964380341,-332.328658762809)) ;
#50193 = CARTESIAN_POINT('Ctrl Pts',(-4.33894042768517,-19.4752099485278,
-332.447752720155)) ;
#50194 = CARTESIAN_POINT('Ctrl Pts',(-13.1275645244822,-15.0258862044737,
-332.5668466775)) ;
#50195 = CARTESIAN_POINT('Ctrl Pts',(-18.7164426227795,-6.91411470272545,
-332.685940634846)) ;
#50196 = CARTESIAN_POINT('Ctrl Pts',(-19.7433273462431,2.88292071922338,-332.805034592191)) ;
#50197 = CARTESIAN_POINT('Ctrl Pts',(-15.9579231980432,11.9772657054768,-332.924128549537)) ;
#50198 = CARTESIAN_POINT('Ctrl Pts',(-8.28289422247497,18.1522414559064,-333.043222506883)) ;
#50199 = CARTESIAN_POINT('Ctrl Pts',(1.41102847819622,19.9027436603086,-333.162316464228)) ;
#50200 = CARTESIAN_POINT('Ctrl Pts',(10.7610235052721,16.8021004548008,-333.281410421574)) ;
#50201 = CARTESIAN_POINT('Ctrl Pts',(17.4880992668176,9.60607050818238,-333.40050437892)) ;
#50202 = CARTESIAN_POINT('Ctrl Pts',(19.9525811903357,0.0686324799246863,
-333.519598336265)) ;
#50203 = CARTESIAN_POINT('Ctrl Pts',(17.5537701774943,-9.4855342037205,-333.638692293611)) ;
#50204 = CARTESIAN_POINT('Ctrl Pts',(10.8763585316662,-16.7276726314479,-333.757786250956)) ;
#50205 = CARTESIAN_POINT('Ctrl Pts',(1.54791556734456,-19.8925655452134,-333.876880208302)) ;
#50206 = CARTESIAN_POINT('Ctrl Pts',(-8.15782027818043,-18.2087938887545,
-333.995974165647)) ;
#50207 = CARTESIAN_POINT('Ctrl Pts',(-15.8751482402092,-12.0867644523099,
-334.115068122993)) ;
#50208 = CARTESIAN_POINT('Ctrl Pts',(-19.7230271538277,-3.01867627671687,
-334.234162080338)) ;
#50209 = CARTESIAN_POINT('Ctrl Pts',(-18.7635652163641,6.78519173977364,-334.353256037684)) ;
#50210 = CARTESIAN_POINT('Ctrl Pts',(-13.2306241231376,14.9352198472764,-334.472349995029)) ;
#50211 = CARTESIAN_POINT('Ctrl Pts',(-4.47281702245709,19.4448994458156,-334.591443952375)) ;
#50212 = CARTESIAN_POINT('Ctrl Pts',(5.37520588656649,19.2150297489026,-334.710537909721)) ;
#50213 = CARTESIAN_POINT('Ctrl Pts',(13.913062428128,14.3016397816933,-334.829631867067)) ;
#50214 = CARTESIAN_POINT('Ctrl Pts',(19.0597137123676,5.9023317237172,-334.948725824412)) ;
#50215 = CARTESIAN_POINT('Ctrl Pts',(19.5607018524639,-3.93562569524808,-335.067819781758)) ;
#50216 = CARTESIAN_POINT('Ctrl Pts',(15.2939147237023,-12.8143036876392,-335.186913739103)) ;
#50217 = CARTESIAN_POINT('Ctrl Pts',(7.29934988358244,-18.5695906753343,-335.306007696449)) ;
#50218 = CARTESIAN_POINT('Ctrl Pts',(-2.4743770804505,-19.7986783559321,-335.425101653794)) ;
#50219 = CARTESIAN_POINT('Ctrl Pts',(-11.6449930754812,-16.201985768438,-335.54419561114)) ;
#50220 = CARTESIAN_POINT('Ctrl Pts',(-17.9772288113016,-8.65617992215987,
-335.663289568485)) ;
#50221 = CARTESIAN_POINT('Ctrl Pts',(-19.9276490289647,0.999505257763509,
-335.782383525831)) ;
#50222 = CARTESIAN_POINT('Ctrl Pts',(-17.0208533381099,10.4115684778892,-335.901477483176)) ;
#50223 = CARTESIAN_POINT('Ctrl Pts',(-9.96535152278336,17.2858894980803,-336.020571440522)) ;
#50224 = CARTESIAN_POINT('Ctrl Pts',(-0.480869553859103,19.9469037884372,
-336.139665397868)) ;
#50225 = CARTESIAN_POINT('Ctrl Pts',(9.12082077862105,17.7460089992421,-336.258759355213)) ;
#50226 = CARTESIAN_POINT('Ctrl Pts',(16.4993790458345,11.2196567300561,-336.377853312559)) ;
#50227 = CARTESIAN_POINT('Ctrl Pts',(19.8563366341969,1.95859690470542,-336.496947269905)) ;
#50228 = CARTESIAN_POINT('Ctrl Pts',(18.3734602304366,-7.77985660503612,-336.61604122725)) ;
#50229 = CARTESIAN_POINT('Ctrl Pts',(12.4121897474615,-15.6220274614286,-336.735135184596)) ;
#50230 = CARTESIAN_POINT('Ctrl Pts',(3.42554075482743,-19.6564468112649,-336.854229141941)) ;
#50231 = CARTESIAN_POINT('Ctrl Pts',(-6.39605871714633,-18.8997512050206,
-336.973323099287)) ;
#50232 = CARTESIAN_POINT('Ctrl Pts',(-14.6586656114475,-13.536387443435,-337.092417056632)) ;
#50233 = CARTESIAN_POINT('Ctrl Pts',(-19.3483339830501,-4.87361911960462,
-337.211511013978)) ;
#50234 = CARTESIAN_POINT('Ctrl Pts',(-19.3219861242708,4.97703468971977,-337.330604971323)) ;
#50235 = CARTESIAN_POINT('Ctrl Pts',(-14.5860565620484,13.6146207375616,-337.449698928669)) ;
#50236 = CARTESIAN_POINT('Ctrl Pts',(-6.29486706233985,18.9336463543882,-337.568792886015)) ;
#50237 = CARTESIAN_POINT('Ctrl Pts',(3.53061332188562,19.637940147781,-337.68788684336)) ;
#50238 = CARTESIAN_POINT('Ctrl Pts',(12.4956074211102,15.5552112241988,-337.806980800706)) ;
#50239 = CARTESIAN_POINT('Ctrl Pts',(18.4147307581373,7.68189341329181,-337.926074758051)) ;
#50240 = CARTESIAN_POINT('Ctrl Pts',(19.8459680722369,-2.06750828385183,-338.045191683308)) ;
#50241 = CARTESIAN_POINT('Ctrl Pts',(17.572416071661,-8.22868029232043,-338.124610622782)) ;
#50242 = CARTESIAN_POINT('Ctrl Pts',(15.7668150602779,-10.8519975176768,-338.164331576474)) ;
#50243 = CARTESIAN_POINT('Ctrl Pts',(-15.3525401471856,10.941001760506,-318.084669473621)) ;
#50244 = CARTESIAN_POINT('Ctrl Pts',(-13.5323637141043,13.495118959534,-318.124385917771)) ;
#50245 = CARTESIAN_POINT('Ctrl Pts',(-8.59522192170838,17.6735199336233,-318.203800347703)) ;
#50246 = CARTESIAN_POINT('Ctrl Pts',(0.910403313848723,19.6311826009593,-318.322912763417)) ;
#50247 = CARTESIAN_POINT('Ctrl Pts',(10.1908875059808,16.8032512024997,-318.442006720762)) ;
#50248 = CARTESIAN_POINT('Ctrl Pts',(16.9882851548233,9.87980042994526,-318.561100678108)) ;
#50249 = CARTESIAN_POINT('Ctrl Pts',(19.6445000265946,0.54814899877979,-318.680194635453)) ;
#50250 = CARTESIAN_POINT('Ctrl Pts',(17.5127147976847,-8.91707456043111,-318.799288592799)) ;
#50251 = CARTESIAN_POINT('Ctrl Pts',(11.1122392158291,-16.2088446133011,-318.918382550144)) ;
#50252 = CARTESIAN_POINT('Ctrl Pts',(2.00328480308495,-19.5498214360711,-319.037476507491)) ;
#50253 = CARTESIAN_POINT('Ctrl Pts',(-7.59397785693506,-18.1256789568353,
-319.156570464836)) ;
#50254 = CARTESIAN_POINT('Ctrl Pts',(-15.3402541587318,-12.2835354383347,
-319.275664422181)) ;
#50255 = CARTESIAN_POINT('Ctrl Pts',(-19.347463098816,-3.44737263856742,-319.394758379528)) ;
#50256 = CARTESIAN_POINT('Ctrl Pts',(-18.6388695974165,6.22906198820229,-319.513852336872)) ;
#50257 = CARTESIAN_POINT('Ctrl Pts',(-13.3871917884119,14.3872089734848,-319.632946294218)) ;
#50258 = CARTESIAN_POINT('Ctrl Pts',(-4.8724851816399,19.0385811186175,-319.752040251563)) ;
#50259 = CARTESIAN_POINT('Ctrl Pts',(4.82985308389071,19.0494409819826,-319.871134208909)) ;
#50260 = CARTESIAN_POINT('Ctrl Pts',(13.35495079964,14.4171416267112,-319.990228166255)) ;
#50261 = CARTESIAN_POINT('Ctrl Pts',(18.6248787411007,6.27077145532118,-320.109322123601)) ;
#50262 = CARTESIAN_POINT('Ctrl Pts',(19.3551313532961,-3.40405250966826,-320.228416080946)) ;
#50263 = CARTESIAN_POINT('Ctrl Pts',(15.3677149580408,-12.2491640523184,-320.347510038291)) ;
#50264 = CARTESIAN_POINT('Ctrl Pts',(7.63453260187597,-18.1086331625589,-320.466603995637)) ;
#50265 = CARTESIAN_POINT('Ctrl Pts',(-1.95951017091986,-19.5542579238435,
-320.585697952983)) ;
#50266 = CARTESIAN_POINT('Ctrl Pts',(-11.0759369442315,-16.2336780755262,
-320.704791910328)) ;
#50267 = CARTESIAN_POINT('Ctrl Pts',(-17.4926866495024,-8.95626020410841,
-320.823885867674)) ;
#50268 = CARTESIAN_POINT('Ctrl Pts',(-19.6457243760081,0.50417933116037,-320.94297982502)) ;
#50269 = CARTESIAN_POINT('Ctrl Pts',(-17.0102632274958,9.84172891263414,-321.062073782365)) ;
#50270 = CARTESIAN_POINT('Ctrl Pts',(-10.2286772136034,16.7804304330243,-321.18116773971)) ;
#50271 = CARTESIAN_POINT('Ctrl Pts',(-0.953927374650981,19.629027118573,-321.300261697056)) ;
#50272 = CARTESIAN_POINT('Ctrl Pts',(8.55333515121244,17.6931947609498,-321.419355654403)) ;
#50273 = CARTESIAN_POINT('Ctrl Pts',(15.9757859914798,11.4447780674072,-321.538449611747)) ;
#50274 = CARTESIAN_POINT('Ctrl Pts',(19.5042580816349,2.40678203059845,-321.657543569093)) ;
#50275 = CARTESIAN_POINT('Ctrl Pts',(18.2787126513231,-7.21784918574521,-321.776637526438)) ;
#50276 = CARTESIAN_POINT('Ctrl Pts',(12.5978672638328,-15.0831834657231,-321.895731483785)) ;
#50277 = CARTESIAN_POINT('Ctrl Pts',(3.84638563670257,-19.2721042076775,-322.01482544113)) ;
#50278 = CARTESIAN_POINT('Ctrl Pts',(-5.84262381798243,-18.7635932054432,
-322.133919398475)) ;
#50279 = CARTESIAN_POINT('Ctrl Pts',(-14.1075372686095,-13.6815962253168,
-322.253013355821)) ;
#50280 = CARTESIAN_POINT('Ctrl Pts',(-18.9338436691828,-5.26481214942683,
-322.372107313166)) ;
#50281 = CARTESIAN_POINT('Ctrl Pts',(-19.1451668103936,4.4352306433839,-322.491201270511)) ;
#50282 = CARTESIAN_POINT('Ctrl Pts',(-14.6899982517982,13.054219027578,-322.610295227857)) ;
#50283 = CARTESIAN_POINT('Ctrl Pts',(-6.65425212022631,18.4913388314171,-322.729389185204)) ;
#50284 = CARTESIAN_POINT('Ctrl Pts',(3.00341836410673,19.4213326316182,-322.848483142548)) ;
#50285 = CARTESIAN_POINT('Ctrl Pts',(11.9290280100071,15.6175213716606,-322.967577099894)) ;
#50286 = CARTESIAN_POINT('Ctrl Pts',(17.947025998785,8.00705569212202,-323.08667105724)) ;
#50287 = CARTESIAN_POINT('Ctrl Pts',(19.5905701795099,-1.5550701268774,-323.205765014586)) ;
#50288 = CARTESIAN_POINT('Ctrl Pts',(16.4590589092933,-10.7381591941182,-323.324858971931)) ;
#50289 = CARTESIAN_POINT('Ctrl Pts',(9.3157747176131,-17.3039020012393,-323.443952929276)) ;
#50290 = CARTESIAN_POINT('Ctrl Pts',(-0.0981601206525683,-19.6519476807905,
-323.563046886622)) ;
#50291 = CARTESIAN_POINT('Ctrl Pts',(-9.48816916120576,-17.2099776009777,
-323.682140843967)) ;
#50292 = CARTESIAN_POINT('Ctrl Pts',(-16.5655076945953,-10.5732037660358,
-323.801234801313)) ;
#50293 = CARTESIAN_POINT('Ctrl Pts',(-19.6051272085852,-1.359290326973,-323.920328758658)) ;
#50294 = CARTESIAN_POINT('Ctrl Pts',(-17.8661431043062,8.18593999698645,-324.039422716004)) ;
#50295 = CARTESIAN_POINT('Ctrl Pts',(-11.7724197945931,15.7359084655981,-324.158516673351)) ;
#50296 = CARTESIAN_POINT('Ctrl Pts',(-2.80925691288954,19.4503665429521,-324.277610630695)) ;
#50297 = CARTESIAN_POINT('Ctrl Pts',(6.83864140081385,18.423942760682,-324.396704588041)) ;
#50298 = CARTESIAN_POINT('Ctrl Pts',(14.8196718490712,12.9068202646376,-324.515798545386)) ;
#50299 = CARTESIAN_POINT('Ctrl Pts',(19.1885177516185,4.24375653797794,-324.634892502732)) ;
#50300 = CARTESIAN_POINT('Ctrl Pts',(18.8803054855788,-5.45369121137518,-324.753986460077)) ;
#50301 = CARTESIAN_POINT('Ctrl Pts',(13.9701594933504,-13.8218423803834,-324.873080417423)) ;
#50302 = CARTESIAN_POINT('Ctrl Pts',(5.65489125975822,-18.8210224987411,-324.992174374769)) ;
#50303 = CARTESIAN_POINT('Ctrl Pts',(-4.03871456620437,-19.2327186770497,
-325.111268332114)) ;
#50304 = CARTESIAN_POINT('Ctrl Pts',(-12.7479138216875,-14.9565830406762,
-325.23036228946)) ;
#50305 = CARTESIAN_POINT('Ctrl Pts',(-18.3499041075179,-7.03489177619029,
-325.349456246805)) ;
#50306 = CARTESIAN_POINT('Ctrl Pts',(-19.4792420493903,2.60150191986722,-325.468550204151)) ;
#50307 = CARTESIAN_POINT('Ctrl Pts',(-15.8606599421856,11.6037989148451,-325.587644161497)) ;
#50308 = CARTESIAN_POINT('Ctrl Pts',(-8.37616020121653,17.7777564203519,-325.706738118843)) ;
#50309 = CARTESIAN_POINT('Ctrl Pts',(1.14996615195856,19.6185183157945,-325.825832076188)) ;
#50310 = CARTESIAN_POINT('Ctrl Pts',(10.3957968275708,16.6774126104045,-325.944926033533)) ;
#50311 = CARTESIAN_POINT('Ctrl Pts',(17.1077295179018,9.67131189653814,-326.064019990879)) ;
#50312 = CARTESIAN_POINT('Ctrl Pts',(19.6497806611846,0.307900998937585,-326.183113948225)) ;
#50313 = CARTESIAN_POINT('Ctrl Pts',(17.4023442399792,-9.13055847202533,-326.30220790557)) ;
#50314 = CARTESIAN_POINT('Ctrl Pts',(10.9132161293105,-16.3435123756421,-326.421301862916)) ;
#50315 = CARTESIAN_POINT('Ctrl Pts',(1.76407293546312,-19.572856964076,-326.540395820261)) ;
#50316 = CARTESIAN_POINT('Ctrl Pts',(-7.81504988680526,-18.0314635657939,
-326.659489777608)) ;
#50317 = CARTESIAN_POINT('Ctrl Pts',(-15.4893125534258,-12.0950353319077,
-326.778583734953)) ;
#50318 = CARTESIAN_POINT('Ctrl Pts',(-19.3881707442273,-3.21053239362289,
-326.897677692298)) ;
#50319 = CARTESIAN_POINT('Ctrl Pts',(-18.561306837729,6.45651388393782,-327.016771649644)) ;
#50320 = CARTESIAN_POINT('Ctrl Pts',(-13.2102627476037,14.5498330298696,-327.135865606989)) ;
#50321 = CARTESIAN_POINT('Ctrl Pts',(-4.63931558353454,19.0967388308628,-327.254959564336)) ;
#50322 = CARTESIAN_POINT('Ctrl Pts',(5.06243017204084,18.9889568910727,-327.37405352168)) ;
#50323 = CARTESIAN_POINT('Ctrl Pts',(13.5302463091053,14.2527582549047,-327.493147479025)) ;
#50324 = CARTESIAN_POINT('Ctrl Pts',(18.7001657643034,6.04255603576688,-327.612241436371)) ;
#50325 = CARTESIAN_POINT('Ctrl Pts',(19.3120592075919,-3.64047417519661,-327.731335393717)) ;
#50326 = CARTESIAN_POINT('Ctrl Pts',(15.2167821732917,-12.4361659424599,-327.850429351062)) ;
#50327 = CARTESIAN_POINT('Ctrl Pts',(7.41252791185793,-18.2006349618286,-327.969523308408)) ;
#50328 = CARTESIAN_POINT('Ctrl Pts',(-2.19847477427431,-19.5288348788321,
-328.088617265753)) ;
#50329 = CARTESIAN_POINT('Ctrl Pts',(-11.2736156218556,-16.0970268642526,
-328.2077112231)) ;
#50330 = CARTESIAN_POINT('Ctrl Pts',(-17.6008966964085,-8.74168854056036,
-328.326805180445)) ;
#50331 = CARTESIAN_POINT('Ctrl Pts',(-19.638090400276,0.744371203363559,-328.44589913779)) ;
#50332 = CARTESIAN_POINT('Ctrl Pts',(-16.8886459536112,10.0489960150942,-328.564993095137)) ;
#50333 = CARTESIAN_POINT('Ctrl Pts',(-10.0227199456207,16.9042529544926,-328.684087052482)) ;
#50334 = CARTESIAN_POINT('Ctrl Pts',(-0.713830661366919,19.6392242424365,
-328.803181009827)) ;
#50335 = CARTESIAN_POINT('Ctrl Pts',(8.76904952562091,17.5872810142733,-328.922274967172)) ;
#50336 = CARTESIAN_POINT('Ctrl Pts',(16.1145392562203,11.2485691364523,-329.041368924519)) ;
#50337 = CARTESIAN_POINT('Ctrl Pts',(19.5322301627044,2.1681023797208,-329.160462881865)) ;
#50338 = CARTESIAN_POINT('Ctrl Pts',(18.1890855624703,-7.44082317078855,-329.27955683921)) ;
#50339 = CARTESIAN_POINT('Ctrl Pts',(12.4124869398741,-15.2361035381512,-329.398650796555)) ;
#50340 = CARTESIAN_POINT('Ctrl Pts',(3.6104371497576,-19.3176972397194,-329.517744753901)) ;
#50341 = CARTESIAN_POINT('Ctrl Pts',(-6.07162978300767,-18.6907462353942,
-329.636838711246)) ;
#50342 = CARTESIAN_POINT('Ctrl Pts',(-14.2737822147762,-13.5080651591169,
-329.755932668592)) ;
#50343 = CARTESIAN_POINT('Ctrl Pts',(-18.9968066300715,-5.03289389094214,
-329.875026625937)) ;
#50344 = CARTESIAN_POINT('Ctrl Pts',(-19.0895010336205,4.66900774739259,-329.994120583283)) ;
#50345 = CARTESIAN_POINT('Ctrl Pts',(-14.5292718555126,13.2328735506094,-330.113214540628)) ;
#50346 = CARTESIAN_POINT('Ctrl Pts',(-6.42764096545065,18.5713250651932,-330.232308497974)) ;
#50347 = CARTESIAN_POINT('Ctrl Pts',(3.24067949758114,19.3831545278824,-330.351402455319)) ;
#50348 = CARTESIAN_POINT('Ctrl Pts',(12.119108489467,15.4704845586147,-330.470496412665)) ;
#50349 = CARTESIAN_POINT('Ctrl Pts',(18.0435951242435,7.78699929691711,-330.58959037001)) ;
#50350 = CARTESIAN_POINT('Ctrl Pts',(19.5700899464735,-1.79450899823529,-330.708684327357)) ;
#50351 = CARTESIAN_POINT('Ctrl Pts',(16.3265212219027,-10.9386191015399,-330.827778284703)) ;
#50352 = CARTESIAN_POINT('Ctrl Pts',(9.10348464921888,-17.4165223365414,-330.946872242047)) ;
#50353 = CARTESIAN_POINT('Ctrl Pts',(-0.338458448313333,-19.6492780767278,
-331.065966199393)) ;
#50354 = CARTESIAN_POINT('Ctrl Pts',(-9.69790482197649,-17.092668753641,-331.185060156739)) ;
#50355 = CARTESIAN_POINT('Ctrl Pts',(-16.6935591845564,-10.3698488325299,
-331.304154114084)) ;
#50356 = CARTESIAN_POINT('Ctrl Pts',(-19.6202829315688,-1.11945555650946,
-331.42324807143)) ;
#50357 = CARTESIAN_POINT('Ctrl Pts',(-17.7647089658075,8.40379666686245,-331.542342028775)) ;
#50358 = CARTESIAN_POINT('Ctrl Pts',(-11.5791196097698,15.8786860955325,-331.661435986121)) ;
#50359 = CARTESIAN_POINT('Ctrl Pts',(-2.5712061609109,19.4832641499289,-331.780529943466)) ;
#50360 = CARTESIAN_POINT('Ctrl Pts',(7.06341962361002,18.3389417982231,-331.899623900812)) ;
#50361 = CARTESIAN_POINT('Ctrl Pts',(14.9763895264006,12.7246390837355,-332.018717858158)) ;
#50362 = CARTESIAN_POINT('Ctrl Pts',(19.2389761178233,4.00880044347866,-332.137811815503)) ;
#50363 = CARTESIAN_POINT('Ctrl Pts',(18.812205690019,-5.68415342282663,-332.256905772849)) ;
#50364 = CARTESIAN_POINT('Ctrl Pts',(13.8001003535698,-13.9916372626369,-332.375999730194)) ;
#50365 = CARTESIAN_POINT('Ctrl Pts',(5.42432342343864,-18.8887638149177,-332.49509368754)) ;
#50366 = CARTESIAN_POINT('Ctrl Pts',(-4.27359190763872,-19.1818949862827,
-332.614187644887)) ;
#50367 = CARTESIAN_POINT('Ctrl Pts',(-12.9298510670639,-14.7995822387444,
-332.73328160223)) ;
#50368 = CARTESIAN_POINT('Ctrl Pts',(-18.4345554094567,-6.80998163826303,
-332.852375559577)) ;
#50369 = CARTESIAN_POINT('Ctrl Pts',(-19.4459742840444,2.8395012241756,-332.971469516922)) ;
#50370 = CARTESIAN_POINT('Ctrl Pts',(-15.7175818793762,11.796876829183,-333.090563474269)) ;
#50371 = CARTESIAN_POINT('Ctrl Pts',(-8.15814605223354,17.8788516423241,-333.209657431613)) ;
#50372 = CARTESIAN_POINT('Ctrl Pts',(1.38977706340263,19.6029896386202,-333.328751388959)) ;
#50373 = CARTESIAN_POINT('Ctrl Pts',(10.598952379389,16.5490450333925,-333.447845346304)) ;
#50374 = CARTESIAN_POINT('Ctrl Pts',(17.2247120586825,9.46139405971896,-333.56693930365)) ;
#50375 = CARTESIAN_POINT('Ctrl Pts',(19.6520765686137,0.0675988102845867,
-333.686033260995)) ;
#50376 = CARTESIAN_POINT('Ctrl Pts',(17.289393903735,-9.34267314526759,-333.805127218341)) ;
#50377 = CARTESIAN_POINT('Ctrl Pts',(10.7125503519078,-16.4757381629974,-333.924221175687)) ;
#50378 = CARTESIAN_POINT('Ctrl Pts',(1.5246025043586,-19.5929648155023,-334.043315133034)) ;
#50379 = CARTESIAN_POINT('Ctrl Pts',(-8.03495583906933,-17.9345523423925,
-334.162409090378)) ;
#50380 = CARTESIAN_POINT('Ctrl Pts',(-15.6360535901888,-11.9047264219953,
-334.281503047724)) ;
#50381 = CARTESIAN_POINT('Ctrl Pts',(-19.4259798316024,-2.97321217540674,
-334.40059700507)) ;
#50382 = CARTESIAN_POINT('Ctrl Pts',(-18.4809682925019,6.68300037627936,-334.519690962415)) ;
#50383 = CARTESIAN_POINT('Ctrl Pts',(-13.0313584913207,14.7102814020834,-334.63878491976)) ;
#50384 = CARTESIAN_POINT('Ctrl Pts',(-4.40545219509248,19.1520409882234,-334.757878877106)) ;
#50385 = CARTESIAN_POINT('Ctrl Pts',(5.29425023495375,18.9256333449493,-334.876972834452)) ;
#50386 = CARTESIAN_POINT('Ctrl Pts',(13.703518634166,14.086243647649,-334.996066791797)) ;
#50387 = CARTESIAN_POINT('Ctrl Pts',(18.7726565138715,5.81343706166854,-335.115160749142)) ;
#50388 = CARTESIAN_POINT('Ctrl Pts',(19.2660993018105,-3.876351474058,-335.234254706488)) ;
#50389 = CARTESIAN_POINT('Ctrl Pts',(15.0635739966129,-12.621308232788,-335.353348663833)) ;
#50390 = CARTESIAN_POINT('Ctrl Pts',(7.1894148152994,-18.2899151903336,-335.472442621179)) ;
#50391 = CARTESIAN_POINT('Ctrl Pts',(-2.43711063650199,-19.5004916555153,
-335.591536578526)) ;
#50392 = CARTESIAN_POINT('Ctrl Pts',(-11.4696085372243,-15.9579686381207,
-335.71063053587)) ;
#50393 = CARTESIAN_POINT('Ctrl Pts',(-17.7064748526026,-8.52580971851293,
-335.829724493216)) ;
#50394 = CARTESIAN_POINT('Ctrl Pts',(-19.6275199090212,0.984451769368805,
-335.948818450561)) ;
#50395 = CARTESIAN_POINT('Ctrl Pts',(-16.7645032927217,10.2547604730937,-336.067912407907)) ;
#50396 = CARTESIAN_POINT('Ctrl Pts',(-9.81526396463168,17.0255477590744,-336.187006365253)) ;
#50397 = CARTESIAN_POINT('Ctrl Pts',(-0.473627206515563,19.6464846737229,
-336.306100322598)) ;
#50398 = CARTESIAN_POINT('Ctrl Pts',(8.98345264706321,17.4787374281848,-336.425194279944)) ;
#50399 = CARTESIAN_POINT('Ctrl Pts',(16.2508828933058,11.0506781568403,-336.544288237289)) ;
#50400 = CARTESIAN_POINT('Ctrl Pts',(19.5572815459293,1.92909859487072,-336.663382194636)) ;
#50401 = CARTESIAN_POINT('Ctrl Pts',(18.0967386542354,-7.66268465400661,-336.78247615198)) ;
#50402 = CARTESIAN_POINT('Ctrl Pts',(12.2252505064069,-15.3867450481888,-336.901570109326)) ;
#50403 = CARTESIAN_POINT('Ctrl Pts',(3.37394889215548,-19.3604022515627,-337.020664066672)) ;
#50404 = CARTESIAN_POINT('Ctrl Pts',(-6.29972806263244,-18.6151031921984,
-337.139758024018)) ;
#50405 = CARTESIAN_POINT('Ctrl Pts',(-14.437892332918,-13.3325167286957,-337.258851981363)) ;
#50406 = CARTESIAN_POINT('Ctrl Pts',(-19.0569298920675,-4.80021783603219,
-337.377945938708)) ;
#50407 = CARTESIAN_POINT('Ctrl Pts',(-19.0309788568,4.90207587048415,-337.497039896054)) ;
#50408 = CARTESIAN_POINT('Ctrl Pts',(-14.366376844032,13.4095717558985,-337.616133853399)) ;
#50409 = CARTESIAN_POINT('Ctrl Pts',(-6.20006044923484,18.648487848766,-337.735227810745)) ;
#50410 = CARTESIAN_POINT('Ctrl Pts',(3.47743896761947,19.3421743158212,-337.85432176809)) ;
#50411 = CARTESIAN_POINT('Ctrl Pts',(12.3074118315047,15.3209351262774,-337.973415725436)) ;
#50412 = CARTESIAN_POINT('Ctrl Pts',(18.137387609008,7.56619687998373,-338.092509682783)) ;
#50413 = CARTESIAN_POINT('Ctrl Pts',(19.5470691442554,-2.03636966630564,-338.211626608038)) ;
#50414 = CARTESIAN_POINT('Ctrl Pts',(17.3077589732144,-8.1047486348108,-338.291045547513)) ;
#50415 = CARTESIAN_POINT('Ctrl Pts',(15.5293520097458,-10.6885562376806,-338.330766501206)) ;
#50416 = CARTESIAN_POINT('Ctrl Pts',(-15.1177807693004,10.7737002754024,-318.251104398353)) ;
#50417 = CARTESIAN_POINT('Ctrl Pts',(-13.325437091123,13.2887618550384,-318.290820842503)) ;
#50418 = CARTESIAN_POINT('Ctrl Pts',(-8.46379031939493,17.4032698965035,-318.370235272435)) ;
#50419 = CARTESIAN_POINT('Ctrl Pts',(0.89648211816811,19.3309974739139,-318.489347688148)) ;
#50420 = CARTESIAN_POINT('Ctrl Pts',(10.0350561980626,16.546308653519,-318.608441645494)) ;
#50421 = CARTESIAN_POINT('Ctrl Pts',(16.7285132072465,9.72872602920581,-318.727535602839)) ;
#50422 = CARTESIAN_POINT('Ctrl Pts',(19.344111259596,0.539767120816376,-318.846629560185)) ;
#50423 = CARTESIAN_POINT('Ctrl Pts',(17.2449236705115,-8.78072143213488,-318.96572351753)) ;
#50424 = CARTESIAN_POINT('Ctrl Pts',(10.942319297678,-15.9609912782063,-319.084817474876)) ;
#50425 = CARTESIAN_POINT('Ctrl Pts',(1.97265209412664,-19.2508804221347,-319.203911432221)) ;
#50426 = CARTESIAN_POINT('Ctrl Pts',(-7.47785651803763,-17.8485148475178,
-319.323005389567)) ;
#50427 = CARTESIAN_POINT('Ctrl Pts',(-15.1056826488461,-12.0957049483905,
-319.442099346912)) ;
#50428 = CARTESIAN_POINT('Ctrl Pts',(-19.0516163948054,-3.39465803575837,
-319.561193304259)) ;
#50429 = CARTESIAN_POINT('Ctrl Pts',(-18.3538581667854,6.13381190560104,-319.680287261603)) ;
#50430 = CARTESIAN_POINT('Ctrl Pts',(-13.1824850242055,14.1672107063747,-319.79938121895)) ;
#50431 = CARTESIAN_POINT('Ctrl Pts',(-4.79797884073275,18.7474576031358,-319.918475176295)) ;
#50432 = CARTESIAN_POINT('Ctrl Pts',(4.75599864062722,18.7581514057224,-320.037569133641)) ;
#50433 = CARTESIAN_POINT('Ctrl Pts',(13.1507370401348,14.1966856522131,-320.156663090986)) ;
#50434 = CARTESIAN_POINT('Ctrl Pts',(18.3400812480129,6.17488358324277,-320.275757048331)) ;
#50435 = CARTESIAN_POINT('Ctrl Pts',(19.0591673921649,-3.3520003253524,-320.394851005677)) ;
#50436 = CARTESIAN_POINT('Ctrl Pts',(15.132723538479,-12.0618591434911,-320.513944963023)) ;
#50437 = CARTESIAN_POINT('Ctrl Pts',(7.51779113063549,-17.8317297045749,-320.633038920368)) ;
#50438 = CARTESIAN_POINT('Ctrl Pts',(-1.92954683037332,-19.2552490705074,
-320.752132877714)) ;
#50439 = CARTESIAN_POINT('Ctrl Pts',(-10.9065721328326,-15.9854450059974,
-320.87122683506)) ;
#50440 = CARTESIAN_POINT('Ctrl Pts',(-17.2252017775524,-8.81930787872528,
-320.990320792405)) ;
#50441 = CARTESIAN_POINT('Ctrl Pts',(-19.3453168871886,0.496469803942675,
-321.109414749751)) ;
#50442 = CARTESIAN_POINT('Ctrl Pts',(-16.7501552079325,9.69123667260777,-321.228508707096)) ;
#50443 = CARTESIAN_POINT('Ctrl Pts',(-10.0722680541918,16.5238368419094,-321.347602664442)) ;
#50444 = CARTESIAN_POINT('Ctrl Pts',(-0.939340642105482,19.3288749515264,
-321.466696621787)) ;
#50445 = CARTESIAN_POINT('Ctrl Pts',(8.42254404956468,17.422643871321,-321.585790579133)) ;
#50446 = CARTESIAN_POINT('Ctrl Pts',(15.7314964117339,11.2697732178267,-321.704884536478)) ;
#50447 = CARTESIAN_POINT('Ctrl Pts',(19.2060137878919,2.36997934864535,-321.823978493824)) ;
#50448 = CARTESIAN_POINT('Ctrl Pts',(17.9992084670363,-7.10747932067599,-321.94307245117)) ;
#50449 = CARTESIAN_POINT('Ctrl Pts',(12.4052302504666,-14.8525428855328,-322.062166408515)) ;
#50450 = CARTESIAN_POINT('Ctrl Pts',(3.7875696303269,-18.9774098345666,-322.181260365861)) ;
#50451 = CARTESIAN_POINT('Ctrl Pts',(-5.75328285423461,-18.4766745961726,
-322.300354323206)) ;
#50452 = CARTESIAN_POINT('Ctrl Pts',(-13.8918155286942,-13.4723876521726,
-322.419448280552)) ;
#50453 = CARTESIAN_POINT('Ctrl Pts',(-18.6443217191903,-5.1843066426486,-322.538542237898)) ;
#50454 = CARTESIAN_POINT('Ctrl Pts',(-18.8524134675053,4.36741046661603,-322.657636195243)) ;
#50455 = CARTESIAN_POINT('Ctrl Pts',(-14.4653699611266,12.8546038298119,-322.776730152589)) ;
#50456 = CARTESIAN_POINT('Ctrl Pts',(-6.55250035321841,18.2085833291542,-322.895824109934)) ;
#50457 = CARTESIAN_POINT('Ctrl Pts',(2.95749237271203,19.1243563708438,-323.01491806728)) ;
#50458 = CARTESIAN_POINT('Ctrl Pts',(11.7466183782748,15.3787101022439,-323.134012024625)) ;
#50459 = CARTESIAN_POINT('Ctrl Pts',(17.6725937147479,7.8846178808573,-323.253105981971)) ;
#50460 = CARTESIAN_POINT('Ctrl Pts',(19.2910060667529,-1.53129117615959,-323.372199939316)) ;
#50461 = CARTESIAN_POINT('Ctrl Pts',(16.2073794873162,-10.5739594234043,-323.491293896662)) ;
#50462 = CARTESIAN_POINT('Ctrl Pts',(9.17332496947635,-17.0393038806773,-323.610387854007)) ;
#50463 = CARTESIAN_POINT('Ctrl Pts',(-0.0966591306772172,-19.3514450299231,
-323.729481811354)) ;
#50464 = CARTESIAN_POINT('Ctrl Pts',(-9.34308328823623,-16.9468157009735,
-323.848575768699)) ;
#50465 = CARTESIAN_POINT('Ctrl Pts',(-16.3122005386815,-10.4115263683823,
-323.967669726045)) ;
#50466 = CARTESIAN_POINT('Ctrl Pts',(-19.3053405008011,-1.33850509218666,
-324.08676368339)) ;
#50467 = CARTESIAN_POINT('Ctrl Pts',(-17.5929476200303,8.06076682286189,-324.205857640736)) ;
#50468 = CARTESIAN_POINT('Ctrl Pts',(-11.5924048966878,15.4952869107006,-324.324951598081)) ;
#50469 = CARTESIAN_POINT('Ctrl Pts',(-2.76629989086795,19.1529463176678,-324.444045555427)) ;
#50470 = CARTESIAN_POINT('Ctrl Pts',(6.73407009304045,18.14221782792,-324.563139512772)) ;
#50471 = CARTESIAN_POINT('Ctrl Pts',(14.5930606882862,12.7094589767493,-324.682233470118)) ;
#50472 = CARTESIAN_POINT('Ctrl Pts',(18.8951015190783,4.17886423773308,-324.801327427463)) ;
#50473 = CARTESIAN_POINT('Ctrl Pts',(18.5916022008074,-5.37029750950658,-324.920421384809)) ;
#50474 = CARTESIAN_POINT('Ctrl Pts',(13.756538429984,-13.6104892696057,-325.039515342155)) ;
#50475 = CARTESIAN_POINT('Ctrl Pts',(5.56842095963703,-18.5332257243567,-325.1586092995)) ;
#50476 = CARTESIAN_POINT('Ctrl Pts',(-3.9769576119852,-18.9386265575451,-325.277703256846)) ;
#50477 = CARTESIAN_POINT('Ctrl Pts',(-12.5529824103755,-14.7278783379849,
-325.396797214191)) ;
#50478 = CARTESIAN_POINT('Ctrl Pts',(-18.0693113175798,-6.92731955680278,
-325.515891171537)) ;
#50479 = CARTESIAN_POINT('Ctrl Pts',(-19.1813802818034,2.56172172933069,-325.634985128882)) ;
#50480 = CARTESIAN_POINT('Ctrl Pts',(-15.6181307825039,11.4263624393018,-325.754079086228)) ;
#50481 = CARTESIAN_POINT('Ctrl Pts',(-8.24807832427286,17.5059124780841,-325.873173043573)) ;
#50482 = CARTESIAN_POINT('Ctrl Pts',(1.13238174339593,19.3185268413744,-325.992267000919)) ;
#50483 = CARTESIAN_POINT('Ctrl Pts',(10.2368322020129,16.4223942895521,-326.111360958265)) ;
#50484 = CARTESIAN_POINT('Ctrl Pts',(16.8461311178881,9.52342554402588,-326.23045491561)) ;
#50485 = CARTESIAN_POINT('Ctrl Pts',(19.3493111467344,0.303192810828759,-326.349548872956)) ;
#50486 = CARTESIAN_POINT('Ctrl Pts',(17.1362408155064,-8.99094090997454,-326.468642830301)) ;
#50487 = CARTESIAN_POINT('Ctrl Pts',(10.7463395209654,-16.0935998034566,-326.587736787647)) ;
#50488 = CARTESIAN_POINT('Ctrl Pts',(1.73709807261283,-19.2735637083494,-326.706830744992)) ;
#50489 = CARTESIAN_POINT('Ctrl Pts',(-7.69554808241464,-17.7557401266443,
-326.825924702338)) ;
#50490 = CARTESIAN_POINT('Ctrl Pts',(-15.2524617558346,-11.9100872423539,
-326.945018659683)) ;
#50491 = CARTESIAN_POINT('Ctrl Pts',(-19.0917015698358,-3.16143937187002,
-327.064112617029)) ;
#50492 = CARTESIAN_POINT('Ctrl Pts',(-18.2774814378808,6.35778577978252,-327.183206574375)) ;
#50493 = CARTESIAN_POINT('Ctrl Pts',(-13.0082614478451,14.3273480392636,-327.302300531721)) ;
#50494 = CARTESIAN_POINT('Ctrl Pts',(-4.56837469494134,18.8047260118381,-327.421394489066)) ;
#50495 = CARTESIAN_POINT('Ctrl Pts',(4.98501933667539,18.6985921915703,-327.540488446412)) ;
#50496 = CARTESIAN_POINT('Ctrl Pts',(13.3233520638725,14.0348159060169,-327.659582403757)) ;
#50497 = CARTESIAN_POINT('Ctrl Pts',(18.4142170392658,5.95015786046861,-327.778676361102)) ;
#50498 = CARTESIAN_POINT('Ctrl Pts',(19.0167538729834,-3.58480681042292,-327.897770318448)) ;
#50499 = CARTESIAN_POINT('Ctrl Pts',(14.984098703184,-12.246001542827,-328.016864275794)) ;
#50500 = CARTESIAN_POINT('Ctrl Pts',(7.29918116764088,-17.9223246822402,-328.13595823314)) ;
#50501 = CARTESIAN_POINT('Ctrl Pts',(-2.16485736859702,-19.2302147753817,
-328.255052190485)) ;
#50502 = CARTESIAN_POINT('Ctrl Pts',(-11.1012280583299,-15.8508833612084,
-328.374146147831)) ;
#50503 = CARTESIAN_POINT('Ctrl Pts',(-17.3317571586476,-8.60801728200809,
-328.493240105176)) ;
#50504 = CARTESIAN_POINT('Ctrl Pts',(-19.3377996444125,0.732988844552469,
-328.612334062522)) ;
#50505 = CARTESIAN_POINT('Ctrl Pts',(-16.6303976129859,9.89533440403462,-328.731428019867)) ;
#50506 = CARTESIAN_POINT('Ctrl Pts',(-9.86946012824876,16.6457659634692,-328.850521977213)) ;
#50507 = CARTESIAN_POINT('Ctrl Pts',(-0.702915305316933,19.3389161487203,
-328.969615934558)) ;
#50508 = CARTESIAN_POINT('Ctrl Pts',(8.63495988367612,17.3183496771772,-329.088709891904)) ;
#50509 = CARTESIAN_POINT('Ctrl Pts',(15.8681279669855,11.076564564749,-329.20780384925)) ;
#50510 = CARTESIAN_POINT('Ctrl Pts',(19.2335581411531,2.13494940562169,-329.326897806595)) ;
#50511 = CARTESIAN_POINT('Ctrl Pts',(17.9109518875208,-7.32704375697291,-329.445991763941)) ;
#50512 = CARTESIAN_POINT('Ctrl Pts',(12.2226846215556,-15.0031246204138,-329.565085721286)) ;
#50513 = CARTESIAN_POINT('Ctrl Pts',(3.55522908835243,-19.0223056926077,-329.684179678632)) ;
#50514 = CARTESIAN_POINT('Ctrl Pts',(-5.97878703405911,-18.4049415466349,
-329.803273635977)) ;
#50515 = CARTESIAN_POINT('Ctrl Pts',(-14.0555183834698,-13.3015100911747,
-329.922367593323)) ;
#50516 = CARTESIAN_POINT('Ctrl Pts',(-18.706321898325,-4.95593470194325,-330.041461550668)) ;
#50517 = CARTESIAN_POINT('Ctrl Pts',(-18.7975988894914,4.59761282879211,-330.160555508015)) ;
#50518 = CARTESIAN_POINT('Ctrl Pts',(-14.3071012707609,13.0305265036326,-330.279649465359)) ;
#50519 = CARTESIAN_POINT('Ctrl Pts',(-6.3293543640249,18.2873464742231,-330.398743422706)) ;
#50520 = CARTESIAN_POINT('Ctrl Pts',(3.19112548922268,19.0867620576596,-330.517837380051)) ;
#50521 = CARTESIAN_POINT('Ctrl Pts',(11.9337922914806,15.2339216644132,-330.636931337396)) ;
#50522 = CARTESIAN_POINT('Ctrl Pts',(17.7676861785204,7.667926420832,-330.756025294742)) ;
#50523 = CARTESIAN_POINT('Ctrl Pts',(19.2708390018775,-1.76706873024081,-330.875119252087)) ;
#50524 = CARTESIAN_POINT('Ctrl Pts',(16.0768684655289,-10.7713540502466,-330.994213209433)) ;
#50525 = CARTESIAN_POINT('Ctrl Pts',(8.96428107949361,-17.1502021113896,-331.113307166779)) ;
#50526 = CARTESIAN_POINT('Ctrl Pts',(-0.333282998908613,-19.3488162474173,
-331.232401124124)) ;
#50527 = CARTESIAN_POINT('Ctrl Pts',(-9.54961183065582,-16.8313006513899,
-331.35149508147)) ;
#50528 = CARTESIAN_POINT('Ctrl Pts',(-16.4382939625616,-10.2112809839948,
-331.470589038815)) ;
#50529 = CARTESIAN_POINT('Ctrl Pts',(-19.3202644739853,-1.10233769278807,
-331.589682996161)) ;
#50530 = CARTESIAN_POINT('Ctrl Pts',(-17.4930645353,8.27529219408646,-331.708776953506)) ;
#50531 = CARTESIAN_POINT('Ctrl Pts',(-11.4020605114064,15.6358812936114,-331.827870910852)) ;
#50532 = CARTESIAN_POINT('Ctrl Pts',(-2.53188923009922,19.1853408794367,-331.946964868198)) ;
#50533 = CARTESIAN_POINT('Ctrl Pts',(6.95541117805748,18.0585166355887,-332.066058825544)) ;
#50534 = CARTESIAN_POINT('Ctrl Pts',(14.7473819579802,12.5300635720304,-332.185152782889)) ;
#50535 = CARTESIAN_POINT('Ctrl Pts',(18.9447883142893,3.9475009132931,-332.304246740235)) ;
#50536 = CARTESIAN_POINT('Ctrl Pts',(18.5245437355737,-5.59723566794349,-332.42334069758)) ;
#50537 = CARTESIAN_POINT('Ctrl Pts',(13.589079705345,-13.7776877775432,-332.542434654926)) ;
#50538 = CARTESIAN_POINT('Ctrl Pts',(5.3413787914672,-18.5999311918014,-332.661528612271)) ;
#50539 = CARTESIAN_POINT('Ctrl Pts',(-4.20824338759227,-18.8885800240374,
-332.780622569617)) ;
#50540 = CARTESIAN_POINT('Ctrl Pts',(-12.7321376096457,-14.5732782730149,
-332.899716526962)) ;
#50541 = CARTESIAN_POINT('Ctrl Pts',(-18.152668196134,-6.70584857380063,-333.018810484308)) ;
#50542 = CARTESIAN_POINT('Ctrl Pts',(-19.1486212218456,2.79608172912783,-333.137904441654)) ;
#50543 = CARTESIAN_POINT('Ctrl Pts',(-15.4772405607092,11.6164879528891,-333.256998398999)) ;
#50544 = CARTESIAN_POINT('Ctrl Pts',(-8.03339788199212,17.6054618287418,-333.376092356345)) ;
#50545 = CARTESIAN_POINT('Ctrl Pts',(1.36852564860903,19.3032356169317,-333.49518631369)) ;
#50546 = CARTESIAN_POINT('Ctrl Pts',(10.4368812535058,16.2959896119843,-333.614280271036)) ;
#50547 = CARTESIAN_POINT('Ctrl Pts',(16.9613248505475,9.31671761125554,-333.733374228381)) ;
#50548 = CARTESIAN_POINT('Ctrl Pts',(19.3515719468919,0.066565140644495,-333.852468185727)) ;
#50549 = CARTESIAN_POINT('Ctrl Pts',(17.0250176299756,-9.19981208681469,-333.971562143072)) ;
#50550 = CARTESIAN_POINT('Ctrl Pts',(10.5487421721494,-16.223803694547,-334.090656100418)) ;
#50551 = CARTESIAN_POINT('Ctrl Pts',(1.50128944137264,-19.2933640857914,-334.209750057763)) ;
#50552 = CARTESIAN_POINT('Ctrl Pts',(-7.91209139995821,-17.6603107960304,
-334.32884401511)) ;
#50553 = CARTESIAN_POINT('Ctrl Pts',(-15.3969589401686,-11.7226883916804,
-334.447937972455)) ;
#50554 = CARTESIAN_POINT('Ctrl Pts',(-19.1289325093771,-2.92774807409659,
-334.5670319298)) ;
#50555 = CARTESIAN_POINT('Ctrl Pts',(-18.1983713686398,6.58080901278506,-334.686125887146)) ;
#50556 = CARTESIAN_POINT('Ctrl Pts',(-12.832092859504,14.4853429568906,-334.805219844492)) ;
#50557 = CARTESIAN_POINT('Ctrl Pts',(-4.33808736772787,18.8591825306311,-334.924313801837)) ;
#50558 = CARTESIAN_POINT('Ctrl Pts',(5.21329458334102,18.6362369409961,-335.043407759183)) ;
#50559 = CARTESIAN_POINT('Ctrl Pts',(13.4939748402039,13.8708475136049,-335.162501716528)) ;
#50560 = CARTESIAN_POINT('Ctrl Pts',(18.4855993153755,5.72454239961989,-335.281595673874)) ;
#50561 = CARTESIAN_POINT('Ctrl Pts',(18.9714967511573,-3.81707725286791,-335.400689631219)) ;
#50562 = CARTESIAN_POINT('Ctrl Pts',(14.8332332695234,-12.4283127779369,-335.519783588565)) ;
#50563 = CARTESIAN_POINT('Ctrl Pts',(7.07947974701638,-18.010239705333,-335.63887754591)) ;
#50564 = CARTESIAN_POINT('Ctrl Pts',(-2.39984419255349,-19.2023049550986,
-335.757971503256)) ;
#50565 = CARTESIAN_POINT('Ctrl Pts',(-11.2942239989673,-15.7139515078035,
-335.877065460602)) ;
#50566 = CARTESIAN_POINT('Ctrl Pts',(-17.4357208939035,-8.39543951486601,
-335.996159417947)) ;
#50567 = CARTESIAN_POINT('Ctrl Pts',(-19.3273907890776,0.969398280974121,
-336.115253375293)) ;
#50568 = CARTESIAN_POINT('Ctrl Pts',(-16.5081532473335,10.097952468298,-336.234347332638)) ;
#50569 = CARTESIAN_POINT('Ctrl Pts',(-9.66517640648003,16.7652060200686,-336.353441289984)) ;
#50570 = CARTESIAN_POINT('Ctrl Pts',(-0.466384859172032,19.3460655590084,
-336.472535247329)) ;
#50571 = CARTESIAN_POINT('Ctrl Pts',(8.84608451550538,17.2114658571273,-336.591629204675)) ;
#50572 = CARTESIAN_POINT('Ctrl Pts',(16.0023867407771,10.8816995836245,-336.71072316202)) ;
#50573 = CARTESIAN_POINT('Ctrl Pts',(19.2582264576617,1.89960028503601,-336.829817119367)) ;
#50574 = CARTESIAN_POINT('Ctrl Pts',(17.8200170780343,-7.54551270297707,-336.948911076712)) ;
#50575 = CARTESIAN_POINT('Ctrl Pts',(12.0383112653523,-15.151462634949,-337.068005034058)) ;
#50576 = CARTESIAN_POINT('Ctrl Pts',(3.32235702948351,-19.0643576918605,-337.187098991403)) ;
#50577 = CARTESIAN_POINT('Ctrl Pts',(-6.20339740811853,-18.3304551793761,
-337.306192948749)) ;
#50578 = CARTESIAN_POINT('Ctrl Pts',(-14.2171190543885,-13.1286460139561,
-337.425286906094)) ;
#50579 = CARTESIAN_POINT('Ctrl Pts',(-18.7655258010849,-4.72681655245975,
-337.54438086344)) ;
#50580 = CARTESIAN_POINT('Ctrl Pts',(-18.7399715893291,4.82711705124851,-337.663474820785)) ;
#50581 = CARTESIAN_POINT('Ctrl Pts',(-14.1466971260155,13.2045227742355,-337.782568778131)) ;
#50582 = CARTESIAN_POINT('Ctrl Pts',(-6.10525383612982,18.3633293431438,-337.901662735476)) ;
#50583 = CARTESIAN_POINT('Ctrl Pts',(3.42426461335331,19.0464084838613,-338.020756692822)) ;
#50584 = CARTESIAN_POINT('Ctrl Pts',(12.1192162418993,15.086659028356,-338.139850650167)) ;
#50585 = CARTESIAN_POINT('Ctrl Pts',(17.8600444598788,7.45050034667566,-338.258944607513)) ;
#50586 = CARTESIAN_POINT('Ctrl Pts',(19.2481702162741,-2.00523104875944,-338.37806153277)) ;
#50587 = CARTESIAN_POINT('Ctrl Pts',(17.0431018747678,-7.98081697730116,-338.457480472244)) ;
#50588 = CARTESIAN_POINT('Ctrl Pts',(15.2918889592135,-10.5251149576845,-338.497201425936)) ;
#50589 = CARTESIAN_POINT('',(1.77633320448849,18.481120189533,-338.000196845114)) ;
#50590 = CARTESIAN_POINT('Ctrl Pts',(1.77636947923266,18.4814593181941,-338.)) ;
#50591 = CARTESIAN_POINT('Ctrl Pts',(2.17391040292432,18.45257048948,-338.)) ;
#50592 = CARTESIAN_POINT('Ctrl Pts',(2.56986764189956,18.4108774285079,-338.)) ;
#50593 = CARTESIAN_POINT('Ctrl Pts',(2.96362238619549,18.3563986629109,-338.)) ;
#50594 = CARTESIAN_POINT('Ctrl Pts',(3.07310029706004,18.3412516163535,-338.)) ;
#50595 = CARTESIAN_POINT('Ctrl Pts',(3.18240800731617,18.3251158806936,-338.)) ;
#50596 = CARTESIAN_POINT('Ctrl Pts',(3.29153233075946,18.3079911489261,-338.)) ;
#50597 = CARTESIAN_POINT('Ctrl Pts',(3.67850503528529,18.2472640483377,-338.)) ;
#50598 = CARTESIAN_POINT('Ctrl Pts',(4.06317162667884,18.1741041213075,-338.)) ;
#50599 = CARTESIAN_POINT('Ctrl Pts',(4.44501400222461,18.0888487936864,-338.)) ;
#50600 = CARTESIAN_POINT('Ctrl Pts',(4.8320753856327,18.0024281993121,-338.)) ;
#50601 = CARTESIAN_POINT('Ctrl Pts',(5.21623533761152,17.9035792153684,-338.)) ;
#50602 = CARTESIAN_POINT('Ctrl Pts',(5.59694970980476,17.7925998953498,-338.)) ;
#50603 = CARTESIAN_POINT('Ctrl Pts',(5.97863845099117,17.6813365440043,-338.)) ;
#50604 = CARTESIAN_POINT('Ctrl Pts',(6.35686448045023,17.557880499624,-338.)) ;
#50605 = CARTESIAN_POINT('Ctrl Pts',(6.7310670982975,17.4224810427333,-338.)) ;
#50606 = CARTESIAN_POINT('Ctrl Pts',(7.07320197655524,17.2986848037707,-338.)) ;
#50607 = CARTESIAN_POINT('Ctrl Pts',(7.4119736372984,17.1649037532658,-338.)) ;
#50608 = CARTESIAN_POINT('Ctrl Pts',(7.74693884571632,17.0212932123994,-338.)) ;
#50609 = CARTESIAN_POINT('Ctrl Pts',(7.91442144992528,16.9494879419662,-338.)) ;
#50610 = CARTESIAN_POINT('Ctrl Pts',(8.08095218795725,16.875224786464,-338.)) ;
#50611 = CARTESIAN_POINT('Ctrl Pts',(8.24647391943457,16.7985201662949,-338.)) ;
#50612 = CARTESIAN_POINT('Ctrl Pts',(8.34874712530054,16.7511256197335,-338.)) ;
#50613 = CARTESIAN_POINT('Ctrl Pts',(8.45063508783765,16.7027989309844,-338.)) ;
#50614 = CARTESIAN_POINT('Ctrl Pts',(8.5521240703735,16.653543605919,-338.)) ;
#50615 = CARTESIAN_POINT('Ctrl Pts',(8.61488761099822,16.6230827763937,-338.)) ;
#50616 = CARTESIAN_POINT('Ctrl Pts',(8.67750192033957,16.5922650996453,-338.)) ;
#50617 = CARTESIAN_POINT('Ctrl Pts',(8.73995271599396,16.5610968510217,-338.)) ;
#50618 = CARTESIAN_POINT('Ctrl Pts',(8.75802449680454,16.5520774982421,-338.)) ;
#50619 = CARTESIAN_POINT('Ctrl Pts',(8.77608157694232,16.5430292933114,-338.)) ;
#50620 = CARTESIAN_POINT('Ctrl Pts',(8.79412176922075,16.5339533427775,-338.)) ;
#50621 = CARTESIAN_POINT('Ctrl Pts',(9.15176790784609,16.3540229621748,-338.)) ;
#50622 = CARTESIAN_POINT('Ctrl Pts',(9.50314107696398,16.163010215128,-338.)) ;
#50623 = CARTESIAN_POINT('Ctrl Pts',(9.8477099058203,15.9612466705402,-338.)) ;
#50624 = CARTESIAN_POINT('Ctrl Pts',(10.1936378838504,15.7586872711566,-338.)) ;
#50625 = CARTESIAN_POINT('Ctrl Pts',(10.5327082667092,15.5452918979248,-338.)) ;
#50626 = CARTESIAN_POINT('Ctrl Pts',(10.8643692312143,15.3213455170803,-338.)) ;
#50627 = CARTESIAN_POINT('Ctrl Pts',(11.1757947544843,15.1110626490227,-338.)) ;
#50628 = CARTESIAN_POINT('Ctrl Pts',(11.4806876427794,14.891476392563,-338.)) ;
#50629 = CARTESIAN_POINT('Ctrl Pts',(11.7785734771352,14.662784696522,-338.)) ;
#50630 = CARTESIAN_POINT('Ctrl Pts',(12.0947284400047,14.4200674997583,-338.)) ;
#50631 = CARTESIAN_POINT('Ctrl Pts',(12.4029912449325,14.167093939552,-338.)) ;
#50632 = CARTESIAN_POINT('Ctrl Pts',(12.70301836703,13.9043703660326,-338.)) ;
#50633 = CARTESIAN_POINT('Ctrl Pts',(13.0148096585189,13.6313453084328,-338.)) ;
#50634 = CARTESIAN_POINT('Ctrl Pts',(13.3177074184112,13.3477904382868,-338.)) ;
#50635 = CARTESIAN_POINT('Ctrl Pts',(13.6112858760549,13.0542304304932,-338.)) ;
#50636 = CARTESIAN_POINT('Ctrl Pts',(13.9048643336986,12.7606704226996,-338.)) ;
#50637 = CARTESIAN_POINT('Ctrl Pts',(14.189123933801,12.4571047703764,-338.)) ;
#50638 = CARTESIAN_POINT('Ctrl Pts',(14.4635914006402,12.1440212322596,-338.)) ;
#50639 = CARTESIAN_POINT('Ctrl Pts',(14.4888948053455,12.1151577769191,-338.)) ;
#50640 = CARTESIAN_POINT('Ctrl Pts',(14.5141145397938,12.0862138269971,-338.)) ;
#50641 = CARTESIAN_POINT('Ctrl Pts',(14.5392407487137,12.0572008275875,-338.)) ;
#50642 = CARTESIAN_POINT('Ctrl Pts',(14.8011157482534,11.754816204771,-338.)) ;
#50643 = CARTESIAN_POINT('Ctrl Pts',(15.0531043329262,11.4446271310053,-338.)) ;
#50644 = CARTESIAN_POINT('Ctrl Pts',(15.294915138725,11.1271876030117,-338.)) ;
#50645 = CARTESIAN_POINT('Ctrl Pts',(15.539325453578,10.8063355437855,-338.)) ;
#50646 = CARTESIAN_POINT('Ctrl Pts',(15.7733383878772,10.4780759367288,-338.)) ;
#50647 = CARTESIAN_POINT('Ctrl Pts',(15.9966203086589,10.1429389926428,-338.)) ;
#50648 = CARTESIAN_POINT('Ctrl Pts',(16.2200615880048,9.80756285793146,-338.)) ;
#50649 = CARTESIAN_POINT('Ctrl Pts',(16.4327568885147,9.46529912697264,-338.)) ;
#50650 = CARTESIAN_POINT('Ctrl Pts',(16.6343335873533,9.11664365354599,-338.)) ;
#50651 = CARTESIAN_POINT('Ctrl Pts',(16.8345187990813,8.77039495431535,-338.)) ;
#50652 = CARTESIAN_POINT('Ctrl Pts',(17.0237386859317,8.41784199162096,-338.)) ;
#50653 = CARTESIAN_POINT('Ctrl Pts',(17.2015857010701,8.05944220770482,-338.)) ;
#50654 = CARTESIAN_POINT('Ctrl Pts',(17.3225387132176,7.81569601166157,-338.)) ;
#50655 = CARTESIAN_POINT('Ctrl Pts',(17.4382305466854,7.56924490433029,-338.)) ;
#50656 = CARTESIAN_POINT('Ctrl Pts',(17.54852052106,7.32022687050523,-338.)) ;
#50657 = CARTESIAN_POINT('Ctrl Pts',(17.7115647639123,6.95209770000015,-338.)) ;
#50658 = CARTESIAN_POINT('Ctrl Pts',(17.8628058244222,6.57835903075512,-338.)) ;
#50659 = CARTESIAN_POINT('Ctrl Pts',(18.0021199161755,6.19960247884217,-338.)) ;
#50660 = CARTESIAN_POINT('Ctrl Pts',(18.0345200794339,6.11151538038197,-338.)) ;
#50661 = CARTESIAN_POINT('Ctrl Pts',(18.0662749154496,6.02315682168231,-338.)) ;
#50662 = CARTESIAN_POINT('Ctrl Pts',(18.0973824707912,5.93453416492661,-338.)) ;
#50663 = CARTESIAN_POINT('Ctrl Pts',(18.1158571451719,5.8819014617672,-338.)) ;
#50664 = CARTESIAN_POINT('Ctrl Pts',(18.1341035121823,5.82917560727256,-338.)) ;
#50665 = CARTESIAN_POINT('Ctrl Pts',(18.1521211372521,5.77635814034836,-338.)) ;
#50666 = CARTESIAN_POINT('Ctrl Pts',(18.1654471331487,5.73729387162396,-338.)) ;
#50667 = CARTESIAN_POINT('Ctrl Pts',(18.1786455508356,5.69818662038403,-338.)) ;
#50668 = CARTESIAN_POINT('Ctrl Pts',(18.1917138621592,5.65904466423081,-338.)) ;
#50669 = CARTESIAN_POINT('Ctrl Pts',(18.3184406876075,5.27947490021735,-338.)) ;
#50670 = CARTESIAN_POINT('Ctrl Pts',(18.4330120738589,4.89642243179216,-338.)) ;
#50671 = CARTESIAN_POINT('Ctrl Pts',(18.5354544304136,4.51052141368157,-338.)) ;
#50672 = CARTESIAN_POINT('Ctrl Pts',(18.6389760269065,4.12055489176024,-338.)) ;
#50673 = CARTESIAN_POINT('Ctrl Pts',(18.7301118538657,3.72767899305814,-338.)) ;
#50674 = CARTESIAN_POINT('Ctrl Pts',(18.8088425322345,3.33252217319263,-338.)) ;
#50675 = CARTESIAN_POINT('Ctrl Pts',(18.8882582346412,2.93392715203159,-338.)) ;
#50676 = CARTESIAN_POINT('Ctrl Pts',(18.9550521478952,2.53301081531028,-338.)) ;
#50677 = CARTESIAN_POINT('Ctrl Pts',(19.0091546529916,2.13039965164354,-338.)) ;
#50678 = CARTESIAN_POINT('Ctrl Pts',(19.0630644990411,1.72922218652565,-338.)) ;
#50679 = CARTESIAN_POINT('Ctrl Pts',(19.1043732401407,1.32636138246208,-338.)) ;
#50680 = CARTESIAN_POINT('Ctrl Pts',(19.1329611487376,0.922426999182332,-338.)) ;
#50681 = CARTESIAN_POINT('Ctrl Pts',(19.1617023053855,0.516327289371959,-338.)) ;
#50682 = CARTESIAN_POINT('Ctrl Pts',(19.1775860460932,0.109141896139547,-338.)) ;
#50683 = CARTESIAN_POINT('Ctrl Pts',(19.1804373013571,-0.298511319337705,
-338.)) ;
#50684 = CARTESIAN_POINT('Ctrl Pts',(19.1832885566211,-0.706164534814958,
-338.)) ;
#50685 = CARTESIAN_POINT('Ctrl Pts',(19.1731074546459,-1.11428614840787,-338.)) ;
#50686 = CARTESIAN_POINT('Ctrl Pts',(19.1496635348269,-1.52225148885922,-338.)) ;
#50687 = CARTESIAN_POINT('Ctrl Pts',(19.1471568248662,-1.56587264054497,-338.)) ;
#50688 = CARTESIAN_POINT('Ctrl Pts',(19.144498328436,-1.60949310274768,-338.)) ;
#50689 = CARTESIAN_POINT('Ctrl Pts',(19.1416889329332,-1.65309486766109,-338.)) ;
#50690 = CARTESIAN_POINT('Ctrl Pts',(19.1344676969147,-1.76516831369235,-338.)) ;
#50691 = CARTESIAN_POINT('Ctrl Pts',(19.1262480834202,-1.87714443349572,-338.)) ;
#50692 = CARTESIAN_POINT('Ctrl Pts',(19.1170287633827,-1.98901025853755,-338.)) ;
#50693 = CARTESIAN_POINT('Ctrl Pts',(19.0838939307125,-2.39106327103881,-338.)) ;
#50694 = CARTESIAN_POINT('Ctrl Pts',(19.0378497220312,-2.79169132925915,-338.)) ;
#50695 = CARTESIAN_POINT('Ctrl Pts',(18.9791990932023,-3.19034486804637,-338.)) ;
#50696 = CARTESIAN_POINT('Ctrl Pts',(18.9201130494373,-3.59195796086731,-338.)) ;
#50697 = CARTESIAN_POINT('Ctrl Pts',(18.8482326076527,-3.99156762017486,-338.)) ;
#50698 = CARTESIAN_POINT('Ctrl Pts',(18.7638142657312,-4.38861097663487,-338.)) ;
#50699 = CARTESIAN_POINT('Ctrl Pts',(18.6790169160031,-4.78743691408631,-338.)) ;
#50700 = CARTESIAN_POINT('Ctrl Pts',(18.5815687026665,-5.18367398668219,-338.)) ;
#50701 = CARTESIAN_POINT('Ctrl Pts',(18.4716778745572,-5.57674284347594,-338.)) ;
#50702 = CARTESIAN_POINT('Ctrl Pts',(18.4042537522977,-5.81791240341871,-338.)) ;
#50703 = CARTESIAN_POINT('Ctrl Pts',(18.3321446001537,-6.057889081464,-338.)) ;
#50704 = CARTESIAN_POINT('Ctrl Pts',(18.2553892686054,-6.29653609375471,-338.)) ;
#50705 = CARTESIAN_POINT('Ctrl Pts',(18.2347050437555,-6.36084730657091,-338.)) ;
#50706 = CARTESIAN_POINT('Ctrl Pts',(18.2136824989532,-6.42506454969312,-338.)) ;
#50707 = CARTESIAN_POINT('Ctrl Pts',(18.1923252042675,-6.48917644953959,-338.)) ;
#50708 = CARTESIAN_POINT('Ctrl Pts',(18.1821231319009,-6.51980178160615,-338.)) ;
#50709 = CARTESIAN_POINT('Ctrl Pts',(18.1718451611425,-6.55040161889664,-338.)) ;
#50710 = CARTESIAN_POINT('Ctrl Pts',(18.1614925996888,-6.58097220724148,-338.)) ;
#50711 = CARTESIAN_POINT('Ctrl Pts',(18.1587181966591,-6.58916487852408,-338.)) ;
#50712 = CARTESIAN_POINT('Ctrl Pts',(18.1559384069493,-6.59735553787596,-338.)) ;
#50713 = CARTESIAN_POINT('Ctrl Pts',(18.153153236177,-6.60554417179179,-338.)) ;
#50714 = CARTESIAN_POINT('Ctrl Pts',(18.0211106344472,-6.99376041246909,-338.)) ;
#50715 = CARTESIAN_POINT('Ctrl Pts',(17.8769670753422,-7.37745629177543,-338.)) ;
#50716 = CARTESIAN_POINT('Ctrl Pts',(17.7209928606868,-7.75606376024863,-338.)) ;
#50717 = CARTESIAN_POINT('Ctrl Pts',(17.5648885109938,-8.1349871148908,-338.)) ;
#50718 = CARTESIAN_POINT('Ctrl Pts',(17.3969335821973,-8.50881409698665,-338.)) ;
#50719 = CARTESIAN_POINT('Ctrl Pts',(17.2173482215894,-8.87696303044654,-338.)) ;
#50720 = CARTESIAN_POINT('Ctrl Pts',(17.0381291457527,-9.24436108227884,-338.)) ;
#50721 = CARTESIAN_POINT('Ctrl Pts',(16.8473268445395,-9.60610474835268,-338.)) ;
#50722 = CARTESIAN_POINT('Ctrl Pts',(16.6451122658087,-9.96159584933572,-338.)) ;
#50723 = CARTESIAN_POINT('Ctrl Pts',(16.442897687078,-10.3170869503188,-338.)) ;
#50724 = CARTESIAN_POINT('Ctrl Pts',(16.2292706658994,-10.6663260229615,-338.)) ;
#50725 = CARTESIAN_POINT('Ctrl Pts',(16.0043568677508,-11.0086868540113,-338.)) ;
#50726 = CARTESIAN_POINT('Ctrl Pts',(1.74714810520642,18.4835595300519,-338.)) ;
#50727 = CARTESIAN_POINT('Ctrl Pts',(1.75686632367078,18.4826409208983,-338.000065615038)) ;
#50728 = CARTESIAN_POINT('Ctrl Pts',(1.76658381766053,18.4817146473289,-338.000131230076)) ;
#50729 = CARTESIAN_POINT('Ctrl Pts',(1.77630057508728,18.4807807104961,-338.000196845114)) ;
#50730 = CARTESIAN_POINT('Ctrl Pts',(17.5364361419604,8.35653984306081,-318.25)) ;
#50731 = CARTESIAN_POINT('Ctrl Pts',(17.3525924946923,8.7230155740616,-318.25)) ;
#50732 = CARTESIAN_POINT('Ctrl Pts',(17.1574041217987,9.08303922266712,-318.25)) ;
#50733 = CARTESIAN_POINT('Ctrl Pts',(16.9510889781351,9.43604656513547,-318.25)) ;
#50734 = CARTESIAN_POINT('Ctrl Pts',(16.8896859298515,9.54110781516859,-318.25)) ;
#50735 = CARTESIAN_POINT('Ctrl Pts',(16.8272969806292,9.64554747471652,-318.25)) ;
#50736 = CARTESIAN_POINT('Ctrl Pts',(16.7639270427763,9.74935035327283,-318.25)) ;
#50737 = CARTESIAN_POINT('Ctrl Pts',(16.5527990036617,10.0951878110104,-318.25)) ;
#50738 = CARTESIAN_POINT('Ctrl Pts',(16.330785425417,10.4339589343761,-318.25)) ;
#50739 = CARTESIAN_POINT('Ctrl Pts',(16.098381788604,10.765286099281,-318.25)) ;
#50740 = CARTESIAN_POINT('Ctrl Pts',(15.8636872847762,11.0998792478148,-318.25)) ;
#50741 = CARTESIAN_POINT('Ctrl Pts',(15.6183965352335,11.4268813867568,-318.25)) ;
#50742 = CARTESIAN_POINT('Ctrl Pts',(15.3629759208164,11.74587376911,-318.25)) ;
#50743 = CARTESIAN_POINT('Ctrl Pts',(15.1075497328084,12.0648731122681,-318.25)) ;
#50744 = CARTESIAN_POINT('Ctrl Pts',(14.841992826869,12.3758627364995,-318.25)) ;
#50745 = CARTESIAN_POINT('Ctrl Pts',(14.5667337092679,12.6783881128115,-318.25)) ;
#50746 = CARTESIAN_POINT('Ctrl Pts',(14.2937526021076,12.9784098264952,-318.25)) ;
#50747 = CARTESIAN_POINT('Ctrl Pts',(14.0112287706723,13.2701071365275,-318.25)) ;
#50748 = CARTESIAN_POINT('Ctrl Pts',(13.7195492816368,13.5529963066618,-318.25)) ;
#50749 = CARTESIAN_POINT('Ctrl Pts',(13.4708564703982,13.7941942846968,-318.25)) ;
#50750 = CARTESIAN_POINT('Ctrl Pts',(13.2155071586103,14.0289885024467,-318.25)) ;
#50751 = CARTESIAN_POINT('Ctrl Pts',(12.9537267975706,14.2570528823813,-318.25)) ;
#50752 = CARTESIAN_POINT('Ctrl Pts',(12.9229309771306,14.2838823575389,-318.25)) ;
#50753 = CARTESIAN_POINT('Ctrl Pts',(12.8920519586899,14.3106135816842,-318.25)) ;
#50754 = CARTESIAN_POINT('Ctrl Pts',(12.8610956304185,14.337241494279,-318.25)) ;
#50755 = CARTESIAN_POINT('Ctrl Pts',(12.5522537735751,14.6029000664955,-318.25)) ;
#50756 = CARTESIAN_POINT('Ctrl Pts',(12.2355521289726,14.8584249449322,-318.25)) ;
#50757 = CARTESIAN_POINT('Ctrl Pts',(11.9114691856933,15.1034336822037,-318.25)) ;
#50758 = CARTESIAN_POINT('Ctrl Pts',(11.5875586146252,15.3483121050028,-318.25)) ;
#50759 = CARTESIAN_POINT('Ctrl Pts',(11.2562741718227,15.5826859352766,-318.25)) ;
#50760 = CARTESIAN_POINT('Ctrl Pts',(10.9180574167217,15.8061361585003,-318.25)) ;
#50761 = CARTESIAN_POINT('Ctrl Pts',(10.6011819128877,16.015486821937,-318.25)) ;
#50762 = CARTESIAN_POINT('Ctrl Pts',(10.2782207486639,16.2152488449875,-318.25)) ;
#50763 = CARTESIAN_POINT('Ctrl Pts',(9.94951312127901,16.4050437026364,-318.25)) ;
#50764 = CARTESIAN_POINT('Ctrl Pts',(9.5981567850144,16.6079158609612,-318.25)) ;
#50765 = CARTESIAN_POINT('Ctrl Pts',(9.24023458672591,16.7994006724583,-318.25)) ;
#50766 = CARTESIAN_POINT('Ctrl Pts',(8.87634769728984,16.9793380940572,-318.25)) ;
#50767 = CARTESIAN_POINT('Ctrl Pts',(8.498588126862,17.1661353793137,-318.25)) ;
#50768 = CARTESIAN_POINT('Ctrl Pts',(8.11439989269635,17.3404885525691,-318.25)) ;
#50769 = CARTESIAN_POINT('Ctrl Pts',(7.72443780478856,17.5021619857,-318.25)) ;
#50770 = CARTESIAN_POINT('Ctrl Pts',(7.33447571688085,17.6638354188309,-318.25)) ;
#50771 = CARTESIAN_POINT('Ctrl Pts',(6.93873911864697,17.8128293033643,-318.25)) ;
#50772 = CARTESIAN_POINT('Ctrl Pts',(6.53787445191548,17.9488476178146,-318.25)) ;
#50773 = CARTESIAN_POINT('Ctrl Pts',(6.50295674792525,17.9606956244746,-318.25)) ;
#50774 = CARTESIAN_POINT('Ctrl Pts',(6.46800115095872,17.9724447698048,-318.25)) ;
#50775 = CARTESIAN_POINT('Ctrl Pts',(6.43302014559825,17.984090917627,-318.25)) ;
#50776 = CARTESIAN_POINT('Ctrl Pts',(6.05072538567341,18.1113674564188,-318.25)) ;
#50777 = CARTESIAN_POINT('Ctrl Pts',(5.66501511560512,18.2264768395085,-318.25)) ;
#50778 = CARTESIAN_POINT('Ctrl Pts',(5.27649729541834,18.3293332926791,-318.25)) ;
#50779 = CARTESIAN_POINT('Ctrl Pts',(4.88547792735887,18.432852007214,-318.25)) ;
#50780 = CARTESIAN_POINT('Ctrl Pts',(4.49161421006131,18.5239596743265,-318.25)) ;
#50781 = CARTESIAN_POINT('Ctrl Pts',(4.09550603735771,18.6025201392987,-318.25)) ;
#50782 = CARTESIAN_POINT('Ctrl Pts',(3.70013762588986,18.6809338868067,-318.25)) ;
#50783 = CARTESIAN_POINT('Ctrl Pts',(3.302532587526,18.7468473697804,-318.25)) ;
#50784 = CARTESIAN_POINT('Ctrl Pts',(2.90327583137912,18.8000747289629,-318.25)) ;
#50785 = CARTESIAN_POINT('Ctrl Pts',(2.50813492818765,18.852753378624,-318.25)) ;
#50786 = CARTESIAN_POINT('Ctrl Pts',(2.11137566179237,18.8930061594508,-318.25)) ;
#50787 = CARTESIAN_POINT('Ctrl Pts',(1.71356161645191,18.9206023316054,-318.25)) ;
#50788 = CARTESIAN_POINT('Ctrl Pts',(1.43581579041974,18.9398694281802,-318.25)) ;
#50789 = CARTESIAN_POINT('Ctrl Pts',(1.15755572908782,18.9529659484427,-318.25)) ;
#50790 = CARTESIAN_POINT('Ctrl Pts',(0.878974271023465,18.9597982921062,-318.25)) ;
#50791 = CARTESIAN_POINT('Ctrl Pts',(0.475814698531161,18.969685973683,-318.25)) ;
#50792 = CARTESIAN_POINT('Ctrl Pts',(0.0719811820807826,18.9664562374422,
-318.25)) ;
#50793 = CARTESIAN_POINT('Ctrl Pts',(-0.33191013715013,18.9501896976789,-318.25)) ;
#50794 = CARTESIAN_POINT('Ctrl Pts',(-0.481432201224366,18.9441677643396,
-318.25)) ;
#50795 = CARTESIAN_POINT('Ctrl Pts',(-0.630962043592318,18.9363586349412,
-318.25)) ;
#50796 = CARTESIAN_POINT('Ctrl Pts',(-0.780467810007441,18.9267646830662,
-318.25)) ;
#50797 = CARTESIAN_POINT('Ctrl Pts',(-0.819481615977578,18.9242611235988,
-318.25)) ;
#50798 = CARTESIAN_POINT('Ctrl Pts',(-0.858484587804893,18.9216366023749,
-318.25)) ;
#50799 = CARTESIAN_POINT('Ctrl Pts',(-0.897472407300964,18.9188916105698,
-318.25)) ;
#50800 = CARTESIAN_POINT('Ctrl Pts',(-1.29519018423448,18.8908897358177,-318.25)) ;
#50801 = CARTESIAN_POINT('Ctrl Pts',(-1.69145771369441,18.8503477102804,-318.25)) ;
#50802 = CARTESIAN_POINT('Ctrl Pts',(-2.08569795887412,18.79750147337,-318.25)) ;
#50803 = CARTESIAN_POINT('Ctrl Pts',(-2.48308103887955,18.7442339527479,-318.25)) ;
#50804 = CARTESIAN_POINT('Ctrl Pts',(-2.87840492618743,18.6784651799139,-318.25)) ;
#50805 = CARTESIAN_POINT('Ctrl Pts',(-3.27107831682424,18.6003836668584,-318.25)) ;
#50806 = CARTESIAN_POINT('Ctrl Pts',(-3.66482131669959,18.5220894663388,-318.25)) ;
#50807 = CARTESIAN_POINT('Ctrl Pts',(-4.05589991391592,18.4314152331644,-318.25)) ;
#50808 = CARTESIAN_POINT('Ctrl Pts',(-4.44370933874037,18.3284994600864,-318.25)) ;
#50809 = CARTESIAN_POINT('Ctrl Pts',(-4.82917214527218,18.2262064259627,-318.25)) ;
#50810 = CARTESIAN_POINT('Ctrl Pts',(-5.21140574505791,18.1118193654387,-318.25)) ;
#50811 = CARTESIAN_POINT('Ctrl Pts',(-5.58979976385578,17.9854258122364,-318.25)) ;
#50812 = CARTESIAN_POINT('Ctrl Pts',(-5.96503249356178,17.8600882127258,-318.25)) ;
#50813 = CARTESIAN_POINT('Ctrl Pts',(-6.33649001753982,17.7229437130915,-318.25)) ;
#50814 = CARTESIAN_POINT('Ctrl Pts',(-6.70355335341107,17.574032647774,-318.25)) ;
#50815 = CARTESIAN_POINT('Ctrl Pts',(-6.95903479026918,17.4703883738477,-318.25)) ;
#50816 = CARTESIAN_POINT('Ctrl Pts',(-7.21238703652132,17.3610430147345,-318.25)) ;
#50817 = CARTESIAN_POINT('Ctrl Pts',(-7.46339259575838,17.2459978119553,-318.25)) ;
#50818 = CARTESIAN_POINT('Ctrl Pts',(-7.54473144738717,17.2087171847536,-318.25)) ;
#50819 = CARTESIAN_POINT('Ctrl Pts',(-7.62582381093297,17.1708379407375,-318.25)) ;
#50820 = CARTESIAN_POINT('Ctrl Pts',(-7.70666209599477,17.132359899455,-318.25)) ;
#50821 = CARTESIAN_POINT('Ctrl Pts',(-7.75575752701837,17.1089910709319,-318.25)) ;
#50822 = CARTESIAN_POINT('Ctrl Pts',(-7.80476131161023,17.0854003626289,-318.25)) ;
#50823 = CARTESIAN_POINT('Ctrl Pts',(-7.85366455439646,17.0615912195305,-318.25)) ;
#50824 = CARTESIAN_POINT('Ctrl Pts',(-7.90459638592846,17.0367944331392,-318.25)) ;
#50825 = CARTESIAN_POINT('Ctrl Pts',(-7.95540854768636,17.011765894505,-318.25)) ;
#50826 = CARTESIAN_POINT('Ctrl Pts',(-8.00609533409681,16.9865079891405,-318.25)) ;
#50827 = CARTESIAN_POINT('Ctrl Pts',(-8.07389495885023,16.9527225269511,-318.25)) ;
#50828 = CARTESIAN_POINT('Ctrl Pts',(-8.14147310723852,16.9185252869047,-318.25)) ;
#50829 = CARTESIAN_POINT('Ctrl Pts',(-8.20882574575339,16.8839172080118,-318.25)) ;
#50830 = CARTESIAN_POINT('Ctrl Pts',(-8.56205988198051,16.7024134818954,-318.25)) ;
#50831 = CARTESIAN_POINT('Ctrl Pts',(-8.90909315514637,16.5096133834362,-318.25)) ;
#50832 = CARTESIAN_POINT('Ctrl Pts',(-9.24951326696572,16.305980925201,-318.25)) ;
#50833 = CARTESIAN_POINT('Ctrl Pts',(-9.59174277293422,16.1012661238089,-318.25)) ;
#50834 = CARTESIAN_POINT('Ctrl Pts',(-9.92728906249252,15.8856031573382,-318.25)) ;
#50835 = CARTESIAN_POINT('Ctrl Pts',(-10.2557062508469,15.6594179589091,-318.25)) ;
#50836 = CARTESIAN_POINT('Ctrl Pts',(-10.5842576024294,15.433140360516,-318.25)) ;
#50837 = CARTESIAN_POINT('Ctrl Pts',(-10.9056744444572,15.1963315518295,-318.25)) ;
#50838 = CARTESIAN_POINT('Ctrl Pts',(-11.2194770645759,14.9493780742992,-318.25)) ;
#50839 = CARTESIAN_POINT('Ctrl Pts',(-11.4076016762541,14.8013295110163,-318.25)) ;
#50840 = CARTESIAN_POINT('Ctrl Pts',(-11.5929890692767,14.6496342143967,-318.25)) ;
#50841 = CARTESIAN_POINT('Ctrl Pts',(-11.7755291988218,14.4943694532838,-318.25)) ;
#50842 = CARTESIAN_POINT('Ctrl Pts',(-11.8551661029436,14.4266319923482,-318.25)) ;
#50843 = CARTESIAN_POINT('Ctrl Pts',(-11.9342712318962,14.3582058144664,-318.25)) ;
#50844 = CARTESIAN_POINT('Ctrl Pts',(-12.0127749516453,14.2891508895264,-318.25)) ;
#50845 = CARTESIAN_POINT('Ctrl Pts',(-12.1830299567138,14.1393879657664,-318.25)) ;
#50846 = CARTESIAN_POINT('Ctrl Pts',(-12.3504882754301,13.9866429757157,-318.25)) ;
#50847 = CARTESIAN_POINT('Ctrl Pts',(-12.5150767471472,13.8309917767329,-318.25)) ;
#50848 = CARTESIAN_POINT('Ctrl Pts',(-12.8040613656493,13.5576992314641,-318.25)) ;
#50849 = CARTESIAN_POINT('Ctrl Pts',(-13.0841952993138,13.2754541823834,-318.25)) ;
#50850 = CARTESIAN_POINT('Ctrl Pts',(-13.3550247088023,12.9846635634382,-318.25)) ;
#50851 = CARTESIAN_POINT('Ctrl Pts',(-13.6247425545384,12.6950664349349,-318.25)) ;
#50852 = CARTESIAN_POINT('Ctrl Pts',(-13.8852324722817,12.3969933377131,-318.25)) ;
#50853 = CARTESIAN_POINT('Ctrl Pts',(-14.1360073231497,12.0908124329483,-318.25)) ;
#50854 = CARTESIAN_POINT('Ctrl Pts',(-14.3837323667058,11.7883551582001,-318.25)) ;
#50855 = CARTESIAN_POINT('Ctrl Pts',(-14.6219775075002,11.4779856734317,-318.25)) ;
#50856 = CARTESIAN_POINT('Ctrl Pts',(-14.850230230253,11.1600319202285,-318.25)) ;
#50857 = CARTESIAN_POINT('Ctrl Pts',(-14.94070771286,11.033997694532,-318.25)) ;
#50858 = CARTESIAN_POINT('Ctrl Pts',(-15.0296146205133,10.9067715134026,-318.25)) ;
#50859 = CARTESIAN_POINT('Ctrl Pts',(-15.1169169700217,10.7783728235744,-318.25)) ;
#50860 = CARTESIAN_POINT('Origin',(0.,17.5,-338.)) ;
#50861 = CARTESIAN_POINT('Ctrl Pts',(18.2156409023172,-9.03480205490196,1.0374236006889)) ;
#50862 = CARTESIAN_POINT('Ctrl Pts',(16.7221931315368,-12.045882967535,0.953894028032912)) ;
#50863 = CARTESIAN_POINT('Ctrl Pts',(12.216439346858,-17.3085987169493,0.786888023505637)) ;
#50864 = CARTESIAN_POINT('Ctrl Pts',(2.51163677899751,-21.0350137533098,0.536405587107078)) ;
#50865 = CARTESIAN_POINT('Ctrl Pts',(-7.79288106850021,-19.6988587020956,
0.285976291493228)) ;
#50866 = CARTESIAN_POINT('Ctrl Pts',(-16.2235226537376,-13.6228781814821,
0.0355469958793765)) ;
#50867 = CARTESIAN_POINT('Ctrl Pts',(-20.7497884505389,-4.26885360646641,
-0.214882299734473)) ;
#50868 = CARTESIAN_POINT('Ctrl Pts',(-20.2835223316277,6.11231092290265,-0.465311595348325)) ;
#50869 = CARTESIAN_POINT('Ctrl Pts',(-14.9364280746688,15.0227392151939,-0.715740890962176)) ;
#50870 = CARTESIAN_POINT('Ctrl Pts',(-5.99538406350538,20.3183546957665,-0.966170186576025)) ;
#50871 = CARTESIAN_POINT('Ctrl Pts',(4.38832445956057,20.7249313061308,-1.21659948218988)) ;
#50872 = CARTESIAN_POINT('Ctrl Pts',(13.7160834985439,16.1446296976496,-1.46702877780373)) ;
#50873 = CARTESIAN_POINT('Ctrl Pts',(19.7434615051254,7.67957554311442,-1.71745807341758)) ;
#50874 = CARTESIAN_POINT('Ctrl Pts',(21.0201216199593,-2.63335454319917,-1.96788736903143)) ;
#50875 = CARTESIAN_POINT('Ctrl Pts',(17.2388798197488,-12.3126410962928,-2.21831666464528)) ;
#50876 = CARTESIAN_POINT('Ctrl Pts',(9.30958190986166,-19.0292348637601,-2.46874596025913)) ;
#50877 = CARTESIAN_POINT('Ctrl Pts',(-0.859805955447589,-21.1669749936797,
-2.71917525587298)) ;
#50878 = CARTESIAN_POINT('Ctrl Pts',(-10.8223059286107,-18.2114742094664,
-2.96960455148683)) ;
#50879 = CARTESIAN_POINT('Ctrl Pts',(-18.1807202456265,-10.8738911034878,
-3.22003384710069)) ;
#50880 = CARTESIAN_POINT('Ctrl Pts',(-21.1644524458383,-0.919810017240595,
-3.47046314271453)) ;
#50881 = CARTESIAN_POINT('Ctrl Pts',(-19.0555506147577,9.25559764924098,-3.72089243832839)) ;
#50882 = CARTESIAN_POINT('Ctrl Pts',(-12.3614631148788,17.2039044119632,-3.97132173394223)) ;
#50883 = CARTESIAN_POINT('Ctrl Pts',(-2.69293497920678,21.0125723910915,-4.22175102955609)) ;
#50884 = CARTESIAN_POINT('Ctrl Pts',(7.62357269090942,19.7651520789397,-4.47218032516994)) ;
#50885 = CARTESIAN_POINT('Ctrl Pts',(16.1056806585396,13.7618003122057,-4.72260962078379)) ;
#50886 = CARTESIAN_POINT('Ctrl Pts',(20.7124066925322,4.44705591235964,-4.97303891639765)) ;
#50887 = CARTESIAN_POINT('Ctrl Pts',(20.3352709233352,-5.93774820719521,-5.22346821201149)) ;
#50888 = CARTESIAN_POINT('Ctrl Pts',(15.0650205323582,-14.8937991678264,-5.47389750762534)) ;
#50889 = CARTESIAN_POINT('Ctrl Pts',(6.16979398488841,-20.26607360782,-5.72432680323919)) ;
#50890 = CARTESIAN_POINT('Ctrl Pts',(-4.21002105290652,-20.7618838265611,
-5.97475609885304)) ;
#50891 = CARTESIAN_POINT('Ctrl Pts',(-13.5768121851455,-16.2619269516994,
-6.22518539446689)) ;
#50892 = CARTESIAN_POINT('Ctrl Pts',(-19.6767229072805,-7.84899184122399,
-6.47561469008074)) ;
#50893 = CARTESIAN_POINT('Ctrl Pts',(-21.041980183154,2.45258379368018,-6.7260439856946)) ;
#50894 = CARTESIAN_POINT('Ctrl Pts',(-17.3440730053068,12.1640136829898,-6.97647328130845)) ;
#50895 = CARTESIAN_POINT('Ctrl Pts',(-9.47279938765414,18.9485136370798,-7.2269025769223)) ;
#50896 = CARTESIAN_POINT('Ctrl Pts',(0.677838658600559,21.1735833539401,-7.47733187253615)) ;
#50897 = CARTESIAN_POINT('Ctrl Pts',(10.6653737757727,18.3038219920433,-7.72776116814999)) ;
#50898 = CARTESIAN_POINT('Ctrl Pts',(18.0865847676868,11.0297574195729,-7.97819046376386)) ;
#50899 = CARTESIAN_POINT('Ctrl Pts',(21.1557646157634,1.10168998169065,-8.22861975937769)) ;
#50900 = CARTESIAN_POINT('Ctrl Pts',(19.1344009664301,-9.09146836045887,-8.47904905499156)) ;
#50901 = CARTESIAN_POINT('Ctrl Pts',(12.5088784892037,-17.0970189283302,-8.7294783506054)) ;
#50902 = CARTESIAN_POINT('Ctrl Pts',(2.87344399935931,-20.9886497154031,-8.97990764621926)) ;
#50903 = CARTESIAN_POINT('Ctrl Pts',(-7.45340448245264,-19.8299485353416,
-9.2303369418331)) ;
#50904 = CARTESIAN_POINT('Ctrl Pts',(-15.9867994819242,-13.8997244439627,
-9.48076623744696)) ;
#50905 = CARTESIAN_POINT('Ctrl Pts',(-20.6734179821683,-4.62492013205691,
-9.7311955330608)) ;
#50906 = CARTESIAN_POINT('Ctrl Pts',(-20.3855562218433,5.76274195322095,-9.98162482867465)) ;
#50907 = CARTESIAN_POINT('Ctrl Pts',(-15.1924800884643,14.7637612434962,-10.2320541242885)) ;
#50908 = CARTESIAN_POINT('Ctrl Pts',(-6.34375821840344,20.2122940053766,-10.4824834199024)) ;
#50909 = CARTESIAN_POINT('Ctrl Pts',(4.0314117727417,20.7973031042956,-10.7329127155162)) ;
#50910 = CARTESIAN_POINT('Ctrl Pts',(13.4365351899228,16.3780224503238,-10.9833420111301)) ;
#50911 = CARTESIAN_POINT('Ctrl Pts',(19.6085319354347,8.0178284236062,-11.2337713067439)) ;
#50912 = CARTESIAN_POINT('Ctrl Pts',(21.0622834862866,-2.27163193247568,-11.4842006023578)) ;
#50913 = CARTESIAN_POINT('Ctrl Pts',(17.4479851609442,-12.0144875511529,-11.7346298979716)) ;
#50914 = CARTESIAN_POINT('Ctrl Pts',(9.63531683966331,-18.86639251931,-11.9850591935855)) ;
#50915 = CARTESIAN_POINT('Ctrl Pts',(-0.495821193039116,-21.1786274021194,
-12.2354884891993)) ;
#50916 = CARTESIAN_POINT('Ctrl Pts',(-10.5076537127573,-18.3948174969548,
-12.4859177848132)) ;
#50917 = CARTESIAN_POINT('Ctrl Pts',(-17.9911130324473,-11.1848088560703,
-12.736347080427)) ;
#50918 = CARTESIAN_POINT('Ctrl Pts',(-21.1455138131668,-1.28348855495878,
-12.9867763760408)) ;
#50919 = CARTESIAN_POINT('Ctrl Pts',(-19.2118376656181,8.92666739626179,-13.2372056716547)) ;
#50920 = CARTESIAN_POINT('Ctrl Pts',(-12.6553697127338,16.9888703192985,-13.4876349672685)) ;
#50921 = CARTESIAN_POINT('Ctrl Pts',(-3.05374072833861,20.963176402005,-13.7380642628824)) ;
#50922 = CARTESIAN_POINT('Ctrl Pts',(7.28268561683616,19.8932799580872,-13.9884935584963)) ;
#50923 = CARTESIAN_POINT('Ctrl Pts',(15.8667372036925,14.0366216667987,-14.2389228541101)) ;
#50924 = CARTESIAN_POINT('Ctrl Pts',(20.6329019226472,4.80244266260591,-14.489352149724)) ;
#50925 = CARTESIAN_POINT('Ctrl Pts',(20.4343354393096,-5.5873099472703,-14.7397814453378)) ;
#50926 = CARTESIAN_POINT('Ctrl Pts',(15.3188172257628,-14.6326325779113,-14.9902107409517)) ;
#50927 = CARTESIAN_POINT('Ctrl Pts',(6.51725377771559,-20.1570211160549,-15.2406400365655)) ;
#50928 = CARTESIAN_POINT('Ctrl Pts',(-3.85250465566884,-20.8311858922631,
-15.4910693321794)) ;
#50929 = CARTESIAN_POINT('Ctrl Pts',(-13.2952654995439,-16.4929079205848,
-15.7414986277932)) ;
#50930 = CARTESIAN_POINT('Ctrl Pts',(-19.5388923004895,-8.18607269478913,
-15.9919279234071)) ;
#50931 = CARTESIAN_POINT('Ctrl Pts',(-21.0810306877392,2.09051233114877,-16.2423572190209)) ;
#50932 = CARTESIAN_POINT('Ctrl Pts',(-17.5506083086661,11.8640736188016,-16.4927865146348)) ;
#50933 = CARTESIAN_POINT('Ctrl Pts',(-9.79712234498845,18.7828778935281,-16.7432158102486)) ;
#50934 = CARTESIAN_POINT('Ctrl Pts',(0.313766917516524,21.1821061131688,-16.9936451058625)) ;
#50935 = CARTESIAN_POINT('Ctrl Pts',(10.3491576970094,18.4844552986881,-17.2440744014763)) ;
#50936 = CARTESIAN_POINT('Ctrl Pts',(17.8943114275467,11.3390314025154,-17.4945036970902)) ;
#50937 = CARTESIAN_POINT('Ctrl Pts',(21.1337021366055,1.46519732713946,-17.744932992704)) ;
#50938 = CARTESIAN_POINT('Ctrl Pts',(19.2878523405992,-8.76121679329746,-17.9953622883179)) ;
#50939 = CARTESIAN_POINT('Ctrl Pts',(12.8009311760093,-16.879447212055,-18.2457915839317)) ;
#50940 = CARTESIAN_POINT('Ctrl Pts',(3.2338016054572,-20.9361923513427,-18.4962208795456)) ;
#50941 = CARTESIAN_POINT('Ctrl Pts',(-7.11140859808664,-19.9550670158388,
-18.7466501751594)) ;
#50942 = CARTESIAN_POINT('Ctrl Pts',(-15.7455421785189,-14.1726285052673,
-18.9970794707733)) ;
#50943 = CARTESIAN_POINT('Ctrl Pts',(-20.590783964988,-4.97932176306281,-19.2475087663871)) ;
#50944 = CARTESIAN_POINT('Ctrl Pts',(-20.4817574082174,5.41089053506673,-19.497938062001)) ;
#50945 = CARTESIAN_POINT('Ctrl Pts',(-15.4429055813031,14.5031102705227,-19.7484078957157)) ;
#50946 = CARTESIAN_POINT('Ctrl Pts',(-9.60564812754564,18.2335667456015,-19.9154012975592)) ;
#50947 = CARTESIAN_POINT('Ctrl Pts',(-6.41678291451902,19.2940954441978,-19.9989182675314)) ;
#50948 = CARTESIAN_POINT('Ctrl Pts',(18.753381758839,-9.30151691942753,0.690868146532775)) ;
#50949 = CARTESIAN_POINT('Ctrl Pts',(17.2158461688193,-12.4014874427912,0.607338573876783)) ;
#50950 = CARTESIAN_POINT('Ctrl Pts',(12.5770787881632,-17.8195629344126,0.440332569349508)) ;
#50951 = CARTESIAN_POINT('Ctrl Pts',(2.58578238386823,-21.6559848392743,0.18985013295095)) ;
#50952 = CARTESIAN_POINT('Ctrl Pts',(-8.0229333934785,-20.2803853806118,-0.0605791626629008)) ;
#50953 = CARTESIAN_POINT('Ctrl Pts',(-16.7024545241233,-14.0250368659274,
-0.311008458276752)) ;
#50954 = CARTESIAN_POINT('Ctrl Pts',(-21.3623394485453,-4.39487371232039,
-0.561437753890603)) ;
#50955 = CARTESIAN_POINT('Ctrl Pts',(-20.8823087663395,6.29275142063949,-0.811867049504453)) ;
#50956 = CARTESIAN_POINT('Ctrl Pts',(-15.3773638435128,15.4662229606302,-1.0622963451183)) ;
#50957 = CARTESIAN_POINT('Ctrl Pts',(-6.17237278318731,20.9181694108132,-1.31272564073215)) ;
#50958 = CARTESIAN_POINT('Ctrl Pts',(4.51787144427738,21.3367485005781,-1.563154936346)) ;
#50959 = CARTESIAN_POINT('Ctrl Pts',(14.1209936814018,16.621232582412,-1.81358423195985)) ;
#50960 = CARTESIAN_POINT('Ctrl Pts',(20.3263048954516,7.90628299482715,-2.0640135275737)) ;
#50961 = CARTESIAN_POINT('Ctrl Pts',(21.6406530777721,-2.71109335761582,-2.31444282318755)) ;
#50962 = CARTESIAN_POINT('Ctrl Pts',(17.7477858774307,-12.6761204931842,-2.5648721188014)) ;
#50963 = CARTESIAN_POINT('Ctrl Pts',(9.58440850404605,-19.5909936901154,-2.81530141441525)) ;
#50964 = CARTESIAN_POINT('Ctrl Pts',(-0.885188141745862,-21.7918416851191,
-3.0657307100291)) ;
#50965 = CARTESIAN_POINT('Ctrl Pts',(-11.1417893928927,-18.7490920617528,
-3.31616000564295)) ;
#50966 = CARTESIAN_POINT('Ctrl Pts',(-18.7174302153441,-11.1948974049994,
-3.56658930125681)) ;
#50967 = CARTESIAN_POINT('Ctrl Pts',(-21.789244669569,-0.946963573305998,
-3.81701859687065)) ;
#50968 = CARTESIAN_POINT('Ctrl Pts',(-19.6180863039507,9.52883058319122,-4.0674478924845)) ;
#50969 = CARTESIAN_POINT('Ctrl Pts',(-12.7263837783299,17.7117779665431,-4.31787718809835)) ;
#50970 = CARTESIAN_POINT('Ctrl Pts',(-2.77243265760535,21.6328809893946,-4.5683064837122)) ;
#50971 = CARTESIAN_POINT('Ctrl Pts',(7.84862689188701,20.3486357930296,-4.81873577932606)) ;
#50972 = CARTESIAN_POINT('Ctrl Pts',(16.5811337353011,14.1680600933934,-5.06916507493991)) ;
#50973 = CARTESIAN_POINT('Ctrl Pts',(21.3238541499783,4.57833669836856,-5.31959437055376)) ;
#50974 = CARTESIAN_POINT('Ctrl Pts',(20.9355850194769,-6.11303546850379,-5.57002366616761)) ;
#50975 = CARTESIAN_POINT('Ctrl Pts',(15.5097524574127,-15.333476495916,-5.82045296178146)) ;
#50976 = CARTESIAN_POINT('Ctrl Pts',(6.35193143038317,-20.8643449417053,-6.07088225739531)) ;
#50977 = CARTESIAN_POINT('Ctrl Pts',(-4.33430437288991,-21.3747918901187,
-6.32131155300916)) ;
#50978 = CARTESIAN_POINT('Ctrl Pts',(-13.9776109630983,-16.7419925488747,
-6.57174084862301)) ;
#50979 = CARTESIAN_POINT('Ctrl Pts',(-20.2575961187389,-8.08070060284082,
-6.82217014423686)) ;
#50980 = CARTESIAN_POINT('Ctrl Pts',(-21.6631569239166,2.52498610535163,-7.07259943985072)) ;
#50981 = CARTESIAN_POINT('Ctrl Pts',(-17.8560844532414,12.5231054751321,-7.32302873546457)) ;
#50982 = CARTESIAN_POINT('Ctrl Pts',(-9.75244429741565,19.5078895057446,-7.57345803107841)) ;
#50983 = CARTESIAN_POINT('Ctrl Pts',(0.697849019082179,21.7986451296659,-7.82388732669226)) ;
#50984 = CARTESIAN_POINT('Ctrl Pts',(10.9802244724935,18.8441660276118,-8.07431662230612)) ;
#50985 = CARTESIAN_POINT('Ctrl Pts',(18.6205157798695,11.3553650242592,-8.32474591791996)) ;
#50986 = CARTESIAN_POINT('Ctrl Pts',(21.7803003675309,1.13421278544775,-8.57517521353382)) ;
#50987 = CARTESIAN_POINT('Ctrl Pts',(19.6992643835285,-9.35985606141382,-8.82560450914767)) ;
#50988 = CARTESIAN_POINT('Ctrl Pts',(12.8781509770061,-17.6017371346119,-9.07603380476152)) ;
#50989 = CARTESIAN_POINT('Ctrl Pts',(2.95827045403466,-21.6082520964405,-9.32646310037537)) ;
#50990 = CARTESIAN_POINT('Ctrl Pts',(-7.67343517650784,-20.4153450946701,
-9.57689239598922)) ;
#50991 = CARTESIAN_POINT('Ctrl Pts',(-16.4587430875625,-14.310055860134,-9.82732169160307)) ;
#50992 = CARTESIAN_POINT('Ctrl Pts',(-21.283714460485,-4.76145161763541,-10.077750987217)) ;
#50993 = CARTESIAN_POINT('Ctrl Pts',(-20.9873547817838,5.93286288448311,-10.3281802828308)) ;
#50994 = CARTESIAN_POINT('Ctrl Pts',(-15.6409747255331,15.1995997439989,-10.5786095784447)) ;
#50995 = CARTESIAN_POINT('Ctrl Pts',(-6.53103123263476,20.8089777207072,-10.8290388740585)) ;
#50996 = CARTESIAN_POINT('Ctrl Pts',(4.15042239835139,21.4112567743653,-11.0794681696724)) ;
#50997 = CARTESIAN_POINT('Ctrl Pts',(13.8331928744073,16.8615152830932,-11.3298974652862)) ;
#50998 = CARTESIAN_POINT('Ctrl Pts',(20.187392092738,8.2545213814371,-11.5803267609001)) ;
#50999 = CARTESIAN_POINT('Ctrl Pts',(21.6840595974296,-2.33869239483448,-11.8307560565139)) ;
#51000 = CARTESIAN_POINT('Ctrl Pts',(17.9630641820635,-12.3691652076281,-12.0811853521278)) ;
#51001 = CARTESIAN_POINT('Ctrl Pts',(9.91975939965916,-19.423344104336,-12.3316146477416)) ;
#51002 = CARTESIAN_POINT('Ctrl Pts',(-0.510458246681989,-21.8038380823388,
-12.5820439433555)) ;
#51003 = CARTESIAN_POINT('Ctrl Pts',(-10.8178483821533,-18.937847795445,-12.8324732389693)) ;
#51004 = CARTESIAN_POINT('Ctrl Pts',(-18.5222256396692,-11.5149937080088,
-13.0829025345832)) ;
#51005 = CARTESIAN_POINT('Ctrl Pts',(-21.7697469527232,-1.32137820367226,
-13.333331830197)) ;
#51006 = CARTESIAN_POINT('Ctrl Pts',(-19.778987078426,9.19019003580505,-13.5837611258109)) ;
#51007 = CARTESIAN_POINT('Ctrl Pts',(-13.028966743188,17.4903958887708,-13.8341904214247)) ;
#51008 = CARTESIAN_POINT('Ctrl Pts',(-3.14388969227891,21.5820267896627,-14.0846197170386)) ;
#51009 = CARTESIAN_POINT('Ctrl Pts',(7.49767654811204,20.4805461136431,-14.3350490126524)) ;
#51010 = CARTESIAN_POINT('Ctrl Pts',(16.3351364711065,14.4509944027488,-14.5854783082663)) ;
#51011 = CARTESIAN_POINT('Ctrl Pts',(21.2420023332181,4.94421476080632,-14.8359076038801)) ;
#51012 = CARTESIAN_POINT('Ctrl Pts',(21.037574002285,-5.75225197993385,-15.086336899494)) ;
#51013 = CARTESIAN_POINT('Ctrl Pts',(15.7710414401101,-15.0646000512388,-15.3367661951078)) ;
#51014 = CARTESIAN_POINT('Ctrl Pts',(6.70964852503154,-20.7520731297612,-15.5871954907217)) ;
#51015 = CARTESIAN_POINT('Ctrl Pts',(-3.96623379451182,-21.4461398103899,
-15.8376247863355)) ;
#51016 = CARTESIAN_POINT('Ctrl Pts',(-13.6877527853741,-16.9797922679054,
-16.0880540819494)) ;
#51017 = CARTESIAN_POINT('Ctrl Pts',(-20.1156966378992,-8.4277323633153,-16.3384833775632)) ;
#51018 = CARTESIAN_POINT('Ctrl Pts',(-21.703360231848,2.15222599236713,-16.5889126731771)) ;
#51019 = CARTESIAN_POINT('Ctrl Pts',(-18.0687168503854,12.2143109310008,-16.8393419687909)) ;
#51020 = CARTESIAN_POINT('Ctrl Pts',(-10.0863415379608,19.3373640574009,-17.0897712644048)) ;
#51021 = CARTESIAN_POINT('Ctrl Pts',(0.323029577659986,21.8074194878293,-17.3402005600186)) ;
#51022 = CARTESIAN_POINT('Ctrl Pts',(10.6546734323115,19.030131779574,-17.5906298556325)) ;
#51023 = CARTESIAN_POINT('Ctrl Pts',(18.4225663709505,11.6737690321829,-17.8410591512463)) ;
#51024 = CARTESIAN_POINT('Ctrl Pts',(21.7575865856544,1.50845116980659,-18.0914884468602)) ;
#51025 = CARTESIAN_POINT('Ctrl Pts',(19.8572457697802,-9.01985519355281,-18.341917742474)) ;
#51026 = CARTESIAN_POINT('Ctrl Pts',(13.1788253018201,-17.3777425204716,-18.5923470380879)) ;
#51027 = CARTESIAN_POINT('Ctrl Pts',(3.32926611611954,-21.5542461474013,-18.8427763337017)) ;
#51028 = CARTESIAN_POINT('Ctrl Pts',(-7.32134328943889,-20.5441571766842,
-19.0932056293156)) ;
#51029 = CARTESIAN_POINT('Ctrl Pts',(-16.2103636680775,-14.5910162761098,
-19.3436349249294)) ;
#51030 = CARTESIAN_POINT('Ctrl Pts',(-21.1986410184491,-5.12631547929417,
-19.5940642205433)) ;
#51031 = CARTESIAN_POINT('Ctrl Pts',(-21.0863959071223,5.57062452007862,-19.8444935161572)) ;
#51032 = CARTESIAN_POINT('Ctrl Pts',(-15.8987929870226,14.9312541377039,-20.0949633498719)) ;
#51033 = CARTESIAN_POINT('Ctrl Pts',(-9.88921484250523,18.7718367879134,-20.2619567517154)) ;
#51034 = CARTESIAN_POINT('Ctrl Pts',(-6.60621167846272,19.863673174985,-20.3454737216875)) ;
#51035 = CARTESIAN_POINT('Ctrl Pts',(19.2911226153608,-9.5682317839531,0.344312692376646)) ;
#51036 = CARTESIAN_POINT('Ctrl Pts',(17.7094992061018,-12.7570919180474,0.260783119720654)) ;
#51037 = CARTESIAN_POINT('Ctrl Pts',(12.9377182294684,-18.330527151876,0.0937771151933803)) ;
#51038 = CARTESIAN_POINT('Ctrl Pts',(2.65992798873894,-22.276955925239,-0.156705321205179)) ;
#51039 = CARTESIAN_POINT('Ctrl Pts',(-8.2529857184568,-20.8619120591279,-0.407134616819029)) ;
#51040 = CARTESIAN_POINT('Ctrl Pts',(-17.181386394509,-14.4271955503726,-0.65756391243288)) ;
#51041 = CARTESIAN_POINT('Ctrl Pts',(-21.9748904465517,-4.52089381817433,
-0.907993208046731)) ;
#51042 = CARTESIAN_POINT('Ctrl Pts',(-21.4810952010514,6.47319191837629,-1.15842250366058)) ;
#51043 = CARTESIAN_POINT('Ctrl Pts',(-15.8182996123569,15.9097067060664,-1.40885179927444)) ;
#51044 = CARTESIAN_POINT('Ctrl Pts',(-6.34936150286924,21.5179841258598,-1.65928109488828)) ;
#51045 = CARTESIAN_POINT('Ctrl Pts',(4.64741842899419,21.9485656950253,-1.90971039050214)) ;
#51046 = CARTESIAN_POINT('Ctrl Pts',(14.5259038642597,17.0978354671745,-2.16013968611599)) ;
#51047 = CARTESIAN_POINT('Ctrl Pts',(20.9091482857778,8.13299044653988,-2.41056898172984)) ;
#51048 = CARTESIAN_POINT('Ctrl Pts',(22.261184535585,-2.78883217203244,-2.66099827734369)) ;
#51049 = CARTESIAN_POINT('Ctrl Pts',(18.2566919351126,-13.0395998900757,-2.91142757295754)) ;
#51050 = CARTESIAN_POINT('Ctrl Pts',(9.85923509823043,-20.1527525164705,-3.16185686857139)) ;
#51051 = CARTESIAN_POINT('Ctrl Pts',(-0.91057032804412,-22.4167083765583,
-3.41228616418524)) ;
#51052 = CARTESIAN_POINT('Ctrl Pts',(-11.461272857175,-19.2867099140392,-3.6627154597991)) ;
#51053 = CARTESIAN_POINT('Ctrl Pts',(-19.2541401850614,-11.5159037065109,
-3.91314475541294)) ;
#51054 = CARTESIAN_POINT('Ctrl Pts',(-22.4140368932999,-0.974117129371415,
-4.1635740510268)) ;
#51055 = CARTESIAN_POINT('Ctrl Pts',(-20.1806219931435,9.80206351714144,-4.41400334664064)) ;
#51056 = CARTESIAN_POINT('Ctrl Pts',(-13.0913044417807,18.2196515211228,-4.6644326422545)) ;
#51057 = CARTESIAN_POINT('Ctrl Pts',(-2.85193033600393,22.253189587698,-4.91486193786834)) ;
#51058 = CARTESIAN_POINT('Ctrl Pts',(8.07368109286461,20.9321195071196,-5.1652912334822)) ;
#51059 = CARTESIAN_POINT('Ctrl Pts',(17.0565868120627,14.5743198745811,-5.41572052909605)) ;
#51060 = CARTESIAN_POINT('Ctrl Pts',(21.9353016074241,4.70961748437752,-5.6661498247099)) ;
#51061 = CARTESIAN_POINT('Ctrl Pts',(21.5358991156188,-6.28832272981237,-5.91657912032376)) ;
#51062 = CARTESIAN_POINT('Ctrl Pts',(15.9544843824673,-15.7731538240056,-6.1670084159376)) ;
#51063 = CARTESIAN_POINT('Ctrl Pts',(6.53406887587788,-21.4626162755904,-6.41743771155145)) ;
#51064 = CARTESIAN_POINT('Ctrl Pts',(-4.45858769287325,-21.9876999536765,
-6.6678670071653)) ;
#51065 = CARTESIAN_POINT('Ctrl Pts',(-14.3784097410511,-17.2220581460501,
-6.91829630277916)) ;
#51066 = CARTESIAN_POINT('Ctrl Pts',(-20.8384693301974,-8.31240936445765,
-7.168725598393)) ;
#51067 = CARTESIAN_POINT('Ctrl Pts',(-22.2843336646794,2.59738841702309,-7.41915489400686)) ;
#51068 = CARTESIAN_POINT('Ctrl Pts',(-18.3680959011759,12.8821972672744,-7.6695841896207)) ;
#51069 = CARTESIAN_POINT('Ctrl Pts',(-10.0320892071771,20.0672653744092,-7.92001348523456)) ;
#51070 = CARTESIAN_POINT('Ctrl Pts',(0.717859379563796,22.4237069053915,-8.17044278084841)) ;
#51071 = CARTESIAN_POINT('Ctrl Pts',(11.2950751692142,19.3845100631803,-8.42087207646225)) ;
#51072 = CARTESIAN_POINT('Ctrl Pts',(19.1544467920521,11.6809726289455,-8.67130137207612)) ;
#51073 = CARTESIAN_POINT('Ctrl Pts',(22.4048361192983,1.16673558920485,-8.92173066768995)) ;
#51074 = CARTESIAN_POINT('Ctrl Pts',(20.2641278006269,-9.62824376236878,-9.17215996330381)) ;
#51075 = CARTESIAN_POINT('Ctrl Pts',(13.2474234648083,-18.1064553408938,-9.42258925891765)) ;
#51076 = CARTESIAN_POINT('Ctrl Pts',(3.04309690871005,-22.2278544774778,-9.67301855453152)) ;
#51077 = CARTESIAN_POINT('Ctrl Pts',(-7.89346587056307,-21.0007416539985,
-9.92344785014535)) ;
#51078 = CARTESIAN_POINT('Ctrl Pts',(-16.9306866932007,-14.7203872763052,
-10.1738771457592)) ;
#51079 = CARTESIAN_POINT('Ctrl Pts',(-21.8940109388016,-4.89798310321389,
-10.424306441373)) ;
#51080 = CARTESIAN_POINT('Ctrl Pts',(-21.5891533417242,6.10298381574526,-10.6747357369869)) ;
#51081 = CARTESIAN_POINT('Ctrl Pts',(-16.0894693626021,15.6354382445016,-10.9251650326007)) ;
#51082 = CARTESIAN_POINT('Ctrl Pts',(-6.71830424686603,21.4056614360378,-11.1755943282146)) ;
#51083 = CARTESIAN_POINT('Ctrl Pts',(4.26943302396105,22.0252104444349,-11.4260236238284)) ;
#51084 = CARTESIAN_POINT('Ctrl Pts',(14.2298505588917,17.3450081158625,-11.6764529194423)) ;
#51085 = CARTESIAN_POINT('Ctrl Pts',(20.7662522500413,8.49121433926803,-11.9268822150561)) ;
#51086 = CARTESIAN_POINT('Ctrl Pts',(22.3058357085726,-2.40575285719332,-12.17731151067)) ;
#51087 = CARTESIAN_POINT('Ctrl Pts',(18.4781432031829,-12.7238428641032,-12.4277408062838)) ;
#51088 = CARTESIAN_POINT('Ctrl Pts',(10.204201959655,-19.980295689362,-12.6781701018977)) ;
#51089 = CARTESIAN_POINT('Ctrl Pts',(-0.525095300324845,-22.4290487625584,
-12.9285993975115)) ;
#51090 = CARTESIAN_POINT('Ctrl Pts',(-11.1280430515494,-19.4808780939352,
-13.1790286931254)) ;
#51091 = CARTESIAN_POINT('Ctrl Pts',(-19.0533382468912,-11.8451785599472,
-13.4294579887392)) ;
#51092 = CARTESIAN_POINT('Ctrl Pts',(-22.3939800922797,-1.35926785238574,
-13.6798872843531)) ;
#51093 = CARTESIAN_POINT('Ctrl Pts',(-20.3461364912338,9.45371267534834,-13.9303165799669)) ;
#51094 = CARTESIAN_POINT('Ctrl Pts',(-13.4025637736422,17.991921458243,-14.1807458755808)) ;
#51095 = CARTESIAN_POINT('Ctrl Pts',(-3.23403865621921,22.2008771773204,-14.4311751711946)) ;
#51096 = CARTESIAN_POINT('Ctrl Pts',(7.71266747938792,21.067812269199,-14.6816044668085)) ;
#51097 = CARTESIAN_POINT('Ctrl Pts',(16.8035357385204,14.8653671386988,-14.9320337624223)) ;
#51098 = CARTESIAN_POINT('Ctrl Pts',(21.8511027437891,5.08598685900673,-15.1824630580362)) ;
#51099 = CARTESIAN_POINT('Ctrl Pts',(21.6408125652603,-5.91719401259742,-15.43289235365)) ;
#51100 = CARTESIAN_POINT('Ctrl Pts',(16.2232656544574,-15.4965675245663,-15.6833216492639)) ;
#51101 = CARTESIAN_POINT('Ctrl Pts',(6.90204327234747,-21.3471251434677,-15.9337509448777)) ;
#51102 = CARTESIAN_POINT('Ctrl Pts',(-4.0799629333548,-22.0610937285166,-16.1841802404916)) ;
#51103 = CARTESIAN_POINT('Ctrl Pts',(-14.0802400712044,-17.4666766152259,
-16.4346095361054)) ;
#51104 = CARTESIAN_POINT('Ctrl Pts',(-20.6925009753088,-8.6693920318415,-16.6850388317193)) ;
#51105 = CARTESIAN_POINT('Ctrl Pts',(-22.3256897759567,2.21393965358552,-16.9354681273331)) ;
#51106 = CARTESIAN_POINT('Ctrl Pts',(-18.5868253921046,12.5645482431999,-17.185897422947)) ;
#51107 = CARTESIAN_POINT('Ctrl Pts',(-10.3755607309332,19.8918502212737,-17.4363267185608)) ;
#51108 = CARTESIAN_POINT('Ctrl Pts',(0.332292237803433,22.4327328624897,-17.6867560141747)) ;
#51109 = CARTESIAN_POINT('Ctrl Pts',(10.9601891676135,19.5758082604597,-17.9371853097885)) ;
#51110 = CARTESIAN_POINT('Ctrl Pts',(18.9508213143542,12.0085066618505,-18.1876146054024)) ;
#51111 = CARTESIAN_POINT('Ctrl Pts',(22.3814710347033,1.5517050124737,-18.4380439010162)) ;
#51112 = CARTESIAN_POINT('Ctrl Pts',(20.4266391989612,-9.27849359380813,-18.6884731966301)) ;
#51113 = CARTESIAN_POINT('Ctrl Pts',(13.5567194276309,-17.8760378288881,-18.9389024922439)) ;
#51114 = CARTESIAN_POINT('Ctrl Pts',(3.42473062678186,-22.1722999434598,-19.1893317878578)) ;
#51115 = CARTESIAN_POINT('Ctrl Pts',(-7.53127798079115,-21.1332473375296,
-19.4397610834716)) ;
#51116 = CARTESIAN_POINT('Ctrl Pts',(-16.675185157636,-15.0094040469524,-19.6901903790855)) ;
#51117 = CARTESIAN_POINT('Ctrl Pts',(-21.8064980719103,-5.27330919552554,
-19.9406196746993)) ;
#51118 = CARTESIAN_POINT('Ctrl Pts',(-21.6910344060272,5.73035850509048,-20.1910489703132)) ;
#51119 = CARTESIAN_POINT('Ctrl Pts',(-16.3546803927421,15.3593980048849,-20.4415188040279)) ;
#51120 = CARTESIAN_POINT('Ctrl Pts',(-10.1727815574648,19.3101068302253,-20.6085122058714)) ;
#51121 = CARTESIAN_POINT('Ctrl Pts',(-6.79564044240643,20.4332509057722,-20.6920291758436)) ;
#51122 = CARTESIAN_POINT('Ctrl Pts',(19.8288634718826,-9.83494664847866,-0.00224276177948207)) ;
#51123 = CARTESIAN_POINT('Ctrl Pts',(18.2031522433843,-13.1126963933035,-0.0857723344354735)) ;
#51124 = CARTESIAN_POINT('Ctrl Pts',(13.2983576707735,-18.8414913693392,-0.252778338962747)) ;
#51125 = CARTESIAN_POINT('Ctrl Pts',(2.73407359360966,-22.8979270112036,-0.503260775361306)) ;
#51126 = CARTESIAN_POINT('Ctrl Pts',(-8.48303804343507,-21.443438737644,-0.753690070975157)) ;
#51127 = CARTESIAN_POINT('Ctrl Pts',(-17.6603182648948,-14.8293542348178,
-1.004119366589)) ;
#51128 = CARTESIAN_POINT('Ctrl Pts',(-22.5874414445579,-4.64691392402828,
-1.25454866220285)) ;
#51129 = CARTESIAN_POINT('Ctrl Pts',(-22.0798816357632,6.6536324161131,-1.5049779578167)) ;
#51130 = CARTESIAN_POINT('Ctrl Pts',(-16.2592353812007,16.3531904515028,-1.75540725343056)) ;
#51131 = CARTESIAN_POINT('Ctrl Pts',(-6.52635022255116,22.1177988409065,-2.0058365490444)) ;
#51132 = CARTESIAN_POINT('Ctrl Pts',(4.77696541371103,22.5603828894726,-2.25626584465826)) ;
#51133 = CARTESIAN_POINT('Ctrl Pts',(14.9308140471177,17.5744383519371,-2.5066951402721)) ;
#51134 = CARTESIAN_POINT('Ctrl Pts',(21.491991676104,8.35969789825263,-2.75712443588596)) ;
#51135 = CARTESIAN_POINT('Ctrl Pts',(22.8817159933979,-2.86657098644908,-3.0075537314998)) ;
#51136 = CARTESIAN_POINT('Ctrl Pts',(18.7655979927946,-13.4030792869672,-3.25798302711366)) ;
#51137 = CARTESIAN_POINT('Ctrl Pts',(10.1340616924148,-20.7145113428256,-3.5084123227275)) ;
#51138 = CARTESIAN_POINT('Ctrl Pts',(-0.935952514342351,-23.0415750679976,
-3.75884161834136)) ;
#51139 = CARTESIAN_POINT('Ctrl Pts',(-11.7807563214571,-19.8243277663255,
-4.0092709139552)) ;
#51140 = CARTESIAN_POINT('Ctrl Pts',(-19.7908501547789,-11.8369100080224,
-4.25970020956907)) ;
#51141 = CARTESIAN_POINT('Ctrl Pts',(-23.0388291170308,-1.00127068543683,
-4.51012950518291)) ;
#51142 = CARTESIAN_POINT('Ctrl Pts',(-20.7431576823363,10.0752964510917,-4.76055880079676)) ;
#51143 = CARTESIAN_POINT('Ctrl Pts',(-13.4562251052316,18.7275250757026,-5.01098809641061)) ;
#51144 = CARTESIAN_POINT('Ctrl Pts',(-2.93142801440251,22.8734981860013,-5.26141739202447)) ;
#51145 = CARTESIAN_POINT('Ctrl Pts',(8.29873529384221,21.5156032212096,-5.51184668763831)) ;
#51146 = CARTESIAN_POINT('Ctrl Pts',(17.5320398888242,14.9805796557688,-5.76227598325218)) ;
#51147 = CARTESIAN_POINT('Ctrl Pts',(22.5467490648702,4.84089827038645,-6.01270527886601)) ;
#51148 = CARTESIAN_POINT('Ctrl Pts',(22.1362132117605,-6.46360999112095,-6.26313457447988)) ;
#51149 = CARTESIAN_POINT('Ctrl Pts',(16.3992163075217,-16.2128311520952,-6.51356387009371)) ;
#51150 = CARTESIAN_POINT('Ctrl Pts',(6.71620632137261,-22.0608876094757,-6.76399316570757)) ;
#51151 = CARTESIAN_POINT('Ctrl Pts',(-4.58287101285661,-22.6006080172341,
-7.01442246132142)) ;
#51152 = CARTESIAN_POINT('Ctrl Pts',(-14.779208519004,-17.7021237432253,-7.26485175693527)) ;
#51153 = CARTESIAN_POINT('Ctrl Pts',(-21.4193425416559,-8.54411812607449,
-7.51528105254913)) ;
#51154 = CARTESIAN_POINT('Ctrl Pts',(-22.905510405442,2.66979072869455,-7.76571034816297)) ;
#51155 = CARTESIAN_POINT('Ctrl Pts',(-18.8801073491104,13.2412890594167,-8.01613964377683)) ;
#51156 = CARTESIAN_POINT('Ctrl Pts',(-10.3117341169386,20.626641243074,-8.26656893939068)) ;
#51157 = CARTESIAN_POINT('Ctrl Pts',(0.737869740045429,23.0487686811173,-8.51699823500452)) ;
#51158 = CARTESIAN_POINT('Ctrl Pts',(11.6099258659349,19.9248540987488,-8.76742753061838)) ;
#51159 = CARTESIAN_POINT('Ctrl Pts',(19.6883778042348,12.0065802336318,-9.01785682623222)) ;
#51160 = CARTESIAN_POINT('Ctrl Pts',(23.0293718710659,1.19925839296196,-9.26828612184608)) ;
#51161 = CARTESIAN_POINT('Ctrl Pts',(20.8289912177253,-9.89663146332373,-9.51871541745992)) ;
#51162 = CARTESIAN_POINT('Ctrl Pts',(13.6166959526106,-18.6111735471754,-9.76914471307378)) ;
#51163 = CARTESIAN_POINT('Ctrl Pts',(3.12792336338541,-22.8474568585153,-10.0195740086876)) ;
#51164 = CARTESIAN_POINT('Ctrl Pts',(-8.11349656461829,-21.5861382133269,
-10.2700033043015)) ;
#51165 = CARTESIAN_POINT('Ctrl Pts',(-17.4026302988391,-15.1307186924764,
-10.5204325999153)) ;
#51166 = CARTESIAN_POINT('Ctrl Pts',(-22.5043074171183,-5.03451458879237,
-10.7708618955292)) ;
#51167 = CARTESIAN_POINT('Ctrl Pts',(-22.1909519016647,6.27310474700741,-11.021291191143)) ;
#51168 = CARTESIAN_POINT('Ctrl Pts',(-16.5379639996709,16.0712767450043,-11.2717204867569)) ;
#51169 = CARTESIAN_POINT('Ctrl Pts',(-6.90557726109732,22.0023451513683,-11.5221497823707)) ;
#51170 = CARTESIAN_POINT('Ctrl Pts',(4.38844364957074,22.6391641145045,-11.7725790779846)) ;
#51171 = CARTESIAN_POINT('Ctrl Pts',(14.6265082433763,17.8285009486319,-12.0230083735984)) ;
#51172 = CARTESIAN_POINT('Ctrl Pts',(21.3451124073446,8.72790729709893,-12.2734376692123)) ;
#51173 = CARTESIAN_POINT('Ctrl Pts',(22.9276118197158,-2.47281331955212,-12.5238669648261)) ;
#51174 = CARTESIAN_POINT('Ctrl Pts',(18.9932222243021,-13.0785205205784,-12.77429626044)) ;
#51175 = CARTESIAN_POINT('Ctrl Pts',(10.4886445196508,-20.537247274388,-13.0247255560538)) ;
#51176 = CARTESIAN_POINT('Ctrl Pts',(-0.539732353967712,-23.054259442778,
-13.2751548516677)) ;
#51177 = CARTESIAN_POINT('Ctrl Pts',(-11.4382377209455,-20.0239083924253,
-13.5255841472815)) ;
#51178 = CARTESIAN_POINT('Ctrl Pts',(-19.5844508541132,-12.1753634118858,
-13.7760134428954)) ;
#51179 = CARTESIAN_POINT('Ctrl Pts',(-23.018213231836,-1.39715750109922,-14.0264427385092)) ;
#51180 = CARTESIAN_POINT('Ctrl Pts',(-20.9132859040416,9.7172353148916,-14.2768720341231)) ;
#51181 = CARTESIAN_POINT('Ctrl Pts',(-13.7761608040964,18.4934470277153,-14.5273013297369)) ;
#51182 = CARTESIAN_POINT('Ctrl Pts',(-3.32418762015953,22.8197275649781,-14.7777306253508)) ;
#51183 = CARTESIAN_POINT('Ctrl Pts',(7.92765841066382,21.655078424755,-15.0281599209646)) ;
#51184 = CARTESIAN_POINT('Ctrl Pts',(17.2719350059343,15.2797398746489,-15.2785892165785)) ;
#51185 = CARTESIAN_POINT('Ctrl Pts',(22.4602031543601,5.22775895720716,-15.5290185121924)) ;
#51186 = CARTESIAN_POINT('Ctrl Pts',(22.2440511282356,-6.08213604526099,-15.7794478078062)) ;
#51187 = CARTESIAN_POINT('Ctrl Pts',(16.6754898688048,-15.9285349978939,-16.0298771034201)) ;
#51188 = CARTESIAN_POINT('Ctrl Pts',(7.09443801966338,-21.942177157174,-16.2803063990339)) ;
#51189 = CARTESIAN_POINT('Ctrl Pts',(-4.19369207219777,-22.6760476466434,
-16.5307356946477)) ;
#51190 = CARTESIAN_POINT('Ctrl Pts',(-14.4727273570347,-17.9535609625466,
-16.7811649902616)) ;
#51191 = CARTESIAN_POINT('Ctrl Pts',(-21.2693053127184,-8.91105170036767,
-17.0315942858754)) ;
#51192 = CARTESIAN_POINT('Ctrl Pts',(-22.9480193200655,2.27565331480388,-17.2820235814893)) ;
#51193 = CARTESIAN_POINT('Ctrl Pts',(-19.1049339338239,12.9147855553991,-17.5324528771031)) ;
#51194 = CARTESIAN_POINT('Ctrl Pts',(-10.6647799239057,20.4463363851465,-17.782882172717)) ;
#51195 = CARTESIAN_POINT('Ctrl Pts',(0.341554897946883,23.0580462371502,-18.0333114683308)) ;
#51196 = CARTESIAN_POINT('Ctrl Pts',(11.2657049029156,20.1214847413455,-18.2837407639447)) ;
#51197 = CARTESIAN_POINT('Ctrl Pts',(19.479076257758,12.343244291518,-18.5341700595585)) ;
#51198 = CARTESIAN_POINT('Ctrl Pts',(23.0053554837523,1.59495885514083,-18.7845993551724)) ;
#51199 = CARTESIAN_POINT('Ctrl Pts',(20.9960326281422,-9.53713199406347,-19.0350286507863)) ;
#51200 = CARTESIAN_POINT('Ctrl Pts',(13.9346135534416,-18.3743331373046,-19.2854579464001)) ;
#51201 = CARTESIAN_POINT('Ctrl Pts',(3.52019513744419,-22.7903537395183,-19.535887242014)) ;
#51202 = CARTESIAN_POINT('Ctrl Pts',(-7.74121267214341,-21.722337498375,-19.7863165376278)) ;
#51203 = CARTESIAN_POINT('Ctrl Pts',(-17.1400066471944,-15.4277918177948,
-20.0367458332417)) ;
#51204 = CARTESIAN_POINT('Ctrl Pts',(-22.4143551253713,-5.42030291175687,
-20.2871751288555)) ;
#51205 = CARTESIAN_POINT('Ctrl Pts',(-22.295672904932,5.89009249010236,-20.5376044244694)) ;
#51206 = CARTESIAN_POINT('Ctrl Pts',(-16.8105677984616,15.7875418720662,-20.7880742581841)) ;
#51207 = CARTESIAN_POINT('Ctrl Pts',(-10.4563482724244,19.8483768725371,-20.9550676600276)) ;
#51208 = CARTESIAN_POINT('Ctrl Pts',(-6.98506920635011,21.0028286365594,-21.0385846299998)) ;
#51209 = CARTESIAN_POINT('Ctrl Pts',(-15.4058029086567,-15.8881929686655,
-20.)) ;
#51210 = CARTESIAN_POINT('Ctrl Pts',(-15.7163716256076,-15.5628634893299,
-20.)) ;
#51211 = CARTESIAN_POINT('Ctrl Pts',(-16.0164501429934,-15.2285241822995,
-20.)) ;
#51212 = CARTESIAN_POINT('Ctrl Pts',(-16.3055626420778,-14.8855558777442,
-20.)) ;
#51213 = CARTESIAN_POINT('Ctrl Pts',(-16.3389516192681,-14.8459472100662,
-20.)) ;
#51214 = CARTESIAN_POINT('Ctrl Pts',(-16.3721942998987,-14.8062234108858,
-20.)) ;
#51215 = CARTESIAN_POINT('Ctrl Pts',(-16.4052899206017,-14.7663850339305,
-20.)) ;
#51216 = CARTESIAN_POINT('Ctrl Pts',(-16.6898920554989,-14.4237993113638,
-20.)) ;
#51217 = CARTESIAN_POINT('Ctrl Pts',(-16.9636224828775,-14.072743433732,-20.)) ;
#51218 = CARTESIAN_POINT('Ctrl Pts',(-17.2262741595062,-13.7138211105957,
-20.)) ;
#51219 = CARTESIAN_POINT('Ctrl Pts',(-17.5044211527437,-13.3337239177371,
-20.)) ;
#51220 = CARTESIAN_POINT('Ctrl Pts',(-17.770144363433,-12.9448044622572,-20.)) ;
#51221 = CARTESIAN_POINT('Ctrl Pts',(-18.0231465801008,-12.5477434530078,
-20.)) ;
#51222 = CARTESIAN_POINT('Ctrl Pts',(-18.2640935768956,-12.1696018739219,
-20.)) ;
#51223 = CARTESIAN_POINT('Ctrl Pts',(-18.4935028088626,-11.784075385089,-20.)) ;
#51224 = CARTESIAN_POINT('Ctrl Pts',(-18.7110696989301,-11.3917284518891,
-20.)) ;
#51225 = CARTESIAN_POINT('Ctrl Pts',(-18.9276966497186,-11.0010765481736,
-20.)) ;
#51226 = CARTESIAN_POINT('Ctrl Pts',(-19.1325835442372,-10.6036625010867,
-20.)) ;
#51227 = CARTESIAN_POINT('Ctrl Pts',(-19.325380463851,-10.2000284326727,-20.)) ;
#51228 = CARTESIAN_POINT('Ctrl Pts',(-19.5159919112789,-9.80096980577254,
-20.)) ;
#51229 = CARTESIAN_POINT('Ctrl Pts',(-19.694786044292,-9.39583089087994,-20.)) ;
#51230 = CARTESIAN_POINT('Ctrl Pts',(-19.8613742887721,-8.98512816896795,
-20.)) ;
#51231 = CARTESIAN_POINT('Ctrl Pts',(-19.8901475315712,-8.91419129600486,
-20.)) ;
#51232 = CARTESIAN_POINT('Ctrl Pts',(-19.9185565173491,-8.84308843309169,
-20.)) ;
#51233 = CARTESIAN_POINT('Ctrl Pts',(-19.9465990851001,-8.77182223500242,
-20.)) ;
#51234 = CARTESIAN_POINT('Ctrl Pts',(-19.9623892760821,-8.73169371009773,
-20.)) ;
#51235 = CARTESIAN_POINT('Ctrl Pts',(-19.9780637277542,-8.69151219088789,
-20.)) ;
#51236 = CARTESIAN_POINT('Ctrl Pts',(-19.9936156884536,-8.65129482506473,
-20.)) ;
#51237 = CARTESIAN_POINT('Ctrl Pts',(-20.1540466428267,-8.2364204239466,-20.)) ;
#51238 = CARTESIAN_POINT('Ctrl Pts',(-20.3016056037318,-7.81733218163497,
-20.)) ;
#51239 = CARTESIAN_POINT('Ctrl Pts',(-20.4360702560848,-7.39460598547406,
-19.9999999999999)) ;
#51240 = CARTESIAN_POINT('Ctrl Pts',(-20.5702980837657,-6.97262431206373,
-19.9999999999999)) ;
#51241 = CARTESIAN_POINT('Ctrl Pts',(-20.6914778674514,-6.54701698129526,
-20.)) ;
#51242 = CARTESIAN_POINT('Ctrl Pts',(-20.7993404945017,-6.11833751408086,
-20.)) ;
#51243 = CARTESIAN_POINT('Ctrl Pts',(-20.8854364080905,-5.77616570373388,
-20.)) ;
#51244 = CARTESIAN_POINT('Ctrl Pts',(-20.963046773811,-5.43203610044039,-20.)) ;
#51245 = CARTESIAN_POINT('Ctrl Pts',(-21.0320115546805,-5.08622456252226,
-20.)) ;
#51246 = CARTESIAN_POINT('Ctrl Pts',(-21.1186694126574,-4.65169425934677,
-19.9999999999999)) ;
#51247 = CARTESIAN_POINT('Ctrl Pts',(-21.191678125955,-4.21450807110328,-20.)) ;
#51248 = CARTESIAN_POINT('Ctrl Pts',(-21.2510743901899,-3.77530376686837,
-20.)) ;
#51249 = CARTESIAN_POINT('Ctrl Pts',(-21.3104617875586,-3.33616502847145,
-20.)) ;
#51250 = CARTESIAN_POINT('Ctrl Pts',(-21.3562407539206,-2.89500822541275,
-19.9999999999999)) ;
#51251 = CARTESIAN_POINT('Ctrl Pts',(-21.3883959838031,-2.4524733104577,-20.)) ;
#51252 = CARTESIAN_POINT('Ctrl Pts',(-21.4203262144307,-2.01303493770006,
-20.)) ;
#51253 = CARTESIAN_POINT('Ctrl Pts',(-21.4388226045321,-1.57223714600192,
-20.)) ;
#51254 = CARTESIAN_POINT('Ctrl Pts',(-21.4438200461406,-1.13071700482763,
-20.)) ;
#51255 = CARTESIAN_POINT('Ctrl Pts',(-21.4458766248401,-0.949019850796634,
-20.)) ;
#51256 = CARTESIAN_POINT('Ctrl Pts',(-21.4456465214687,-0.767200531796367,
-20.)) ;
#51257 = CARTESIAN_POINT('Ctrl Pts',(-21.4431227621937,-0.585304284853741,
-20.)) ;
#51258 = CARTESIAN_POINT('Ctrl Pts',(-21.442338628647,-0.528789009941922,
-20.)) ;
#51259 = CARTESIAN_POINT('Ctrl Pts',(-21.4413329023764,-0.472260605289573,
-20.)) ;
#51260 = CARTESIAN_POINT('Ctrl Pts',(-21.4401061791021,-0.41575316401674,
-20.)) ;
#51261 = CARTESIAN_POINT('Ctrl Pts',(-21.430594871128,0.0223730931662136,
-20.)) ;
#51262 = CARTESIAN_POINT('Ctrl Pts',(-21.4078008345799,0.459551132058727,
-20.)) ;
#51263 = CARTESIAN_POINT('Ctrl Pts',(-21.3718229821551,0.895170021038482,
-20.)) ;
#51264 = CARTESIAN_POINT('Ctrl Pts',(-21.3356991982527,1.33255584450437,-20.)) ;
#51265 = CARTESIAN_POINT('Ctrl Pts',(-21.2862843980238,1.76837038828578,-20.)) ;
#51266 = CARTESIAN_POINT('Ctrl Pts',(-21.2236263779098,2.20199489548804,-20.)) ;
#51267 = CARTESIAN_POINT('Ctrl Pts',(-21.1611418379815,2.6344188339529,-20.)) ;
#51268 = CARTESIAN_POINT('Ctrl Pts',(-21.0854872263467,3.06466537747855,-20.)) ;
#51269 = CARTESIAN_POINT('Ctrl Pts',(-20.9966589676707,3.49211247687234,-20.)) ;
#51270 = CARTESIAN_POINT('Ctrl Pts',(-20.9087567138529,3.91510358335862,-20.)) ;
#51271 = CARTESIAN_POINT('Ctrl Pts',(-20.8079539088575,4.33535379125912,-20.)) ;
#51272 = CARTESIAN_POINT('Ctrl Pts',(-20.6941988108917,4.75224453494563,-20.)) ;
#51273 = CARTESIAN_POINT('Ctrl Pts',(-20.6335152012047,4.97463839354549,-20.)) ;
#51274 = CARTESIAN_POINT('Ctrl Pts',(-20.5691448457971,5.19607591101803,-20.)) ;
#51275 = CARTESIAN_POINT('Ctrl Pts',(-20.5010743690551,5.41646059911979,-20.)) ;
#51276 = CARTESIAN_POINT('Ctrl Pts',(-20.3720176703124,5.83429402208323,-20.)) ;
#51277 = CARTESIAN_POINT('Ctrl Pts',(-20.2296631034003,6.2483448872045,-20.)) ;
#51278 = CARTESIAN_POINT('Ctrl Pts',(-20.0742865758653,6.6580351300983,-20.)) ;
#51279 = CARTESIAN_POINT('Ctrl Pts',(-19.974727149743,6.92054920553505,-20.)) ;
#51280 = CARTESIAN_POINT('Ctrl Pts',(-19.8698203408578,7.18127234357877,-20.)) ;
#51281 = CARTESIAN_POINT('Ctrl Pts',(-19.7596300991819,7.44004522863576,-20.)) ;
#51282 = CARTESIAN_POINT('Ctrl Pts',(-19.743426557129,7.47809793876163,-20.)) ;
#51283 = CARTESIAN_POINT('Ctrl Pts',(-19.7271080968926,7.51610998653188,-20.)) ;
#51284 = CARTESIAN_POINT('Ctrl Pts',(-19.7106769746549,7.55407608714222,-20.)) ;
#51285 = CARTESIAN_POINT('Ctrl Pts',(-19.5393337799005,7.94998531822446,-20.)) ;
#51286 = CARTESIAN_POINT('Ctrl Pts',(-19.356105481169,8.34006611847233,-20.)) ;
#51287 = CARTESIAN_POINT('Ctrl Pts',(-19.1613930760502,8.72383375706302,-20.)) ;
#51288 = CARTESIAN_POINT('Ctrl Pts',(-18.9653863811575,9.11015237092336,-20.)) ;
#51289 = CARTESIAN_POINT('Ctrl Pts',(-18.7577421300927,9.4900740890982,-20.)) ;
#51290 = CARTESIAN_POINT('Ctrl Pts',(-18.5388203966269,9.86308441658966,-20.)) ;
#51291 = CARTESIAN_POINT('Ctrl Pts',(-18.319565318918,10.2366627134797,-20.)) ;
#51292 = CARTESIAN_POINT('Ctrl Pts',(-18.088998084385,10.6033090194613,-20.)) ;
#51293 = CARTESIAN_POINT('Ctrl Pts',(-17.8474358298871,10.9624794239074,-20.)) ;
#51294 = CARTESIAN_POINT('Ctrl Pts',(-17.6075749157737,11.3191201652846,-20.)) ;
#51295 = CARTESIAN_POINT('Ctrl Pts',(-17.3568729675726,11.668390348116,-20.)) ;
#51296 = CARTESIAN_POINT('Ctrl Pts',(-17.0956014939349,12.0097243781994,-20.)) ;
#51297 = CARTESIAN_POINT('Ctrl Pts',(-16.8365444490206,12.3481654025138,-20.)) ;
#51298 = CARTESIAN_POINT('Ctrl Pts',(-16.5670959558664,12.678804607708,-20.)) ;
#51299 = CARTESIAN_POINT('Ctrl Pts',(-16.2874872516987,13.0010522033732,-20.)) ;
#51300 = CARTESIAN_POINT('Ctrl Pts',(-16.0124316447049,13.3180523779271,-20.)) ;
#51301 = CARTESIAN_POINT('Ctrl Pts',(-15.7275436921894,13.6269323033859,-20.)) ;
#51302 = CARTESIAN_POINT('Ctrl Pts',(-15.4330159894672,13.927088326476,-20.)) ;
#51303 = CARTESIAN_POINT('Ctrl Pts',(-15.3371463552999,14.0247899954897,-20.)) ;
#51304 = CARTESIAN_POINT('Ctrl Pts',(-15.240255169351,14.1215669921431,-20.)) ;
#51305 = CARTESIAN_POINT('Ctrl Pts',(-15.1423485188742,14.2173974310379,-20.)) ;
#51306 = CARTESIAN_POINT('Ctrl Pts',(-15.0615994091814,14.2964341725109,-20.)) ;
#51307 = CARTESIAN_POINT('Ctrl Pts',(-14.980206607069,14.3747808968213,-20.)) ;
#51308 = CARTESIAN_POINT('Ctrl Pts',(-14.8981884568382,14.4524259180576,-20.)) ;
#51309 = CARTESIAN_POINT('Ctrl Pts',(-14.5873267664777,14.7467127616609,-20.)) ;
#51310 = CARTESIAN_POINT('Ctrl Pts',(-14.2674495159252,15.0309567608575,-20.)) ;
#51311 = CARTESIAN_POINT('Ctrl Pts',(-13.9391293443686,15.3048916258252,-20.)) ;
#51312 = CARTESIAN_POINT('Ctrl Pts',(-13.6095969492685,15.5798379129394,-20.)) ;
#51313 = CARTESIAN_POINT('Ctrl Pts',(-13.2715586942242,15.8443990772164,-20.)) ;
#51314 = CARTESIAN_POINT('Ctrl Pts',(-12.9255620668213,16.0982636774071,-20.)) ;
#51315 = CARTESIAN_POINT('Ctrl Pts',(-12.5802282517134,16.3516419590474,-20.)) ;
#51316 = CARTESIAN_POINT('Ctrl Pts',(-12.226966029585,16.5943648615532,-20.)) ;
#51317 = CARTESIAN_POINT('Ctrl Pts',(-11.8662957588071,16.8260769315832,-20.)) ;
#51318 = CARTESIAN_POINT('Ctrl Pts',(-11.6413560918667,16.9705890804392,-20.)) ;
#51319 = CARTESIAN_POINT('Ctrl Pts',(-11.413534500183,17.1108174721437,-20.)) ;
#51320 = CARTESIAN_POINT('Ctrl Pts',(-11.1829537686147,17.2466661897157,-20.)) ;
#51321 = CARTESIAN_POINT('Ctrl Pts',(-11.1400129309677,17.2719651714915,-20.)) ;
#51322 = CARTESIAN_POINT('Ctrl Pts',(-11.0969743505193,17.2971134233324,-20.)) ;
#51323 = CARTESIAN_POINT('Ctrl Pts',(-11.0538454480649,17.3221064554476,-20.)) ;
#51324 = CARTESIAN_POINT('Ctrl Pts',(-10.6847916114131,17.5359717259913,-20.)) ;
#51325 = CARTESIAN_POINT('Ctrl Pts',(-10.3095060771257,17.7382566945241,-20.)) ;
#51326 = CARTESIAN_POINT('Ctrl Pts',(-9.92853192271807,17.9286680256626,-20.)) ;
#51327 = CARTESIAN_POINT('Ctrl Pts',(-9.54864671752116,18.1185350987029,-20.)) ;
#51328 = CARTESIAN_POINT('Ctrl Pts',(-9.16310486846575,18.2965965356029,-20.)) ;
#51329 = CARTESIAN_POINT('Ctrl Pts',(-8.77242344642078,18.4625145294738,-20.)) ;
#51330 = CARTESIAN_POINT('Ctrl Pts',(-8.38645555043553,18.6264307419858,-20.)) ;
#51331 = CARTESIAN_POINT('Ctrl Pts',(-7.99547086428503,18.7784949003803,-20.)) ;
#51332 = CARTESIAN_POINT('Ctrl Pts',(-7.59995442243829,18.9183328108531,-20.)) ;
#51333 = CARTESIAN_POINT('Ctrl Pts',(-7.21155076956793,19.0556559395297,-20.)) ;
#51334 = CARTESIAN_POINT('Ctrl Pts',(-6.81877645105338,19.181188684393,-20.)) ;
#51335 = CARTESIAN_POINT('Ctrl Pts',(-6.42208446149232,19.2945281628512,-20.)) ;
#51336 = CARTESIAN_POINT('Ctrl Pts',(-17.8811317021246,13.0451252434097,1.03858668902498)) ;
#51337 = CARTESIAN_POINT('Ctrl Pts',(-15.7250931322991,16.0004653153199,0.955069732687912)) ;
#51338 = CARTESIAN_POINT('Ctrl Pts',(-9.92321314561447,20.8175865914447,0.788076344479562)) ;
#51339 = CARTESIAN_POINT('Ctrl Pts',(1.17400689041209,23.0306757905423,0.537606524399929)) ;
#51340 = CARTESIAN_POINT('Ctrl Pts',(11.9841056083277,19.7018876770169,0.287177228786078)) ;
#51341 = CARTESIAN_POINT('Ctrl Pts',(19.9119536450833,11.6323207154006,0.0367479331722268)) ;
#51342 = CARTESIAN_POINT('Ctrl Pts',(23.0478433418594,0.763795191132392,-0.213681362441623)) ;
#51343 = CARTESIAN_POINT('Ctrl Pts',(20.6382716461964,-10.2885336600105,-0.464110658055474)) ;
#51344 = CARTESIAN_POINT('Ctrl Pts',(13.2624942528171,-18.8652055910463,-0.714539953669324)) ;
#51345 = CARTESIAN_POINT('Ctrl Pts',(2.69556125327808,-22.9024975410042,-0.964969249283176)) ;
#51346 = CARTESIAN_POINT('Ctrl Pts',(-8.5200306184055,-21.4289412372532,-1.21539854489703)) ;
#51347 = CARTESIAN_POINT('Ctrl Pts',(-17.6854910820251,-14.799110286703,-1.46582784051088)) ;
#51348 = CARTESIAN_POINT('Ctrl Pts',(-22.5954447001295,-4.60828645213766,
-1.71625713612473)) ;
#51349 = CARTESIAN_POINT('Ctrl Pts',(-22.0684297685877,6.6913924216612,-1.96668643173858)) ;
#51350 = CARTESIAN_POINT('Ctrl Pts',(-16.2312671764708,16.3809748738999,-2.21711572735243)) ;
#51351 = CARTESIAN_POINT('Ctrl Pts',(-6.48850213627474,22.1289334562072,-2.46754502296629)) ;
#51352 = CARTESIAN_POINT('Ctrl Pts',(4.81553877248335,22.5521826978432,-2.71797431858013)) ;
#51353 = CARTESIAN_POINT('Ctrl Pts',(14.9608552830364,17.5488794369338,-2.96840361419398)) ;
#51354 = CARTESIAN_POINT('Ctrl Pts',(21.5062598770076,8.32292880280115,-3.21883290980783)) ;
#51355 = CARTESIAN_POINT('Ctrl Pts',(22.8767841945832,-2.90570204539006,-3.46926220542169)) ;
#51356 = CARTESIAN_POINT('Ctrl Pts',(18.742649695744,-13.4351569016615,-3.71969150103554)) ;
#51357 = CARTESIAN_POINT('Ctrl Pts',(10.0986203923039,-20.7318167341985,-3.97012079664939)) ;
#51358 = CARTESIAN_POINT('Ctrl Pts',(-0.975359688754453,-23.0399442779018,
-4.22055009226323)) ;
#51359 = CARTESIAN_POINT('Ctrl Pts',(-11.8146467124566,-19.804153147564,-4.47097938787709)) ;
#51360 = CARTESIAN_POINT('Ctrl Pts',(-19.8110692021406,-11.8030460448693,
-4.72140868349093)) ;
#51361 = CARTESIAN_POINT('Ctrl Pts',(-23.040511562476,-0.961865780905311,
-4.97183797910479)) ;
#51362 = CARTESIAN_POINT('Ctrl Pts',(-20.7258987482158,10.1107606012354,-5.22226727471864)) ;
#51363 = CARTESIAN_POINT('Ctrl Pts',(-13.4241776432584,18.7505150183207,-5.4726965703325)) ;
#51364 = CARTESIAN_POINT('Ctrl Pts',(-2.89230336512565,22.8784820321647,-5.72312586594633)) ;
#51365 = CARTESIAN_POINT('Ctrl Pts',(8.33552288439842,21.5013817485216,-5.9735551615602)) ;
#51366 = CARTESIAN_POINT('Ctrl Pts',(17.5576385113683,14.9505748637168,-6.22398445717404)) ;
#51367 = CARTESIAN_POINT('Ctrl Pts',(22.5549991282262,4.80232997384176,-6.47441375278789)) ;
#51368 = CARTESIAN_POINT('Ctrl Pts',(22.1251295677783,-6.50146140961283,-6.72484304840174)) ;
#51369 = CARTESIAN_POINT('Ctrl Pts',(16.3714659258583,-16.2408578064785,-6.9752723440156)) ;
#51370 = CARTESIAN_POINT('Ctrl Pts',(6.67846655556003,-22.0723456686872,-7.22570163962945)) ;
#51371 = CARTESIAN_POINT('Ctrl Pts',(-4.62151914279075,-22.5927404195368,
-7.4761309352433)) ;
#51372 = CARTESIAN_POINT('Ctrl Pts',(-14.8094654207873,-17.6768236061309,
-7.72656023085714)) ;
#51373 = CARTESIAN_POINT('Ctrl Pts',(-21.4339277374552,-8.50747322048703,
-7.97698952647101)) ;
#51374 = CARTESIAN_POINT('Ctrl Pts',(-22.9009143755295,2.70896283038824,-8.22741882208484)) ;
#51375 = CARTESIAN_POINT('Ctrl Pts',(-18.8574359996269,13.2735626857198,-8.47784811769871)) ;
#51376 = CARTESIAN_POINT('Ctrl Pts',(-10.2764426745271,20.6442506477933,-8.72827741331255)) ;
#51377 = CARTESIAN_POINT('Ctrl Pts',(0.777289376089591,23.0474766531517,-8.9787067089264)) ;
#51378 = CARTESIAN_POINT('Ctrl Pts',(11.6439884618892,19.9049715285189,-9.22913600454027)) ;
#51379 = CARTESIAN_POINT('Ctrl Pts',(19.7088871483584,11.9728913059891,-9.47956530015409)) ;
#51380 = CARTESIAN_POINT('Ctrl Pts',(23.0313929628866,1.15986940681171,-9.72999459576797)) ;
#51381 = CARTESIAN_POINT('Ctrl Pts',(20.8120377379817,-9.93224264930053,-9.98042389138181)) ;
#51382 = CARTESIAN_POINT('Ctrl Pts',(13.5848472823902,-18.6344380963283,-10.2308531869956)) ;
#51383 = CARTESIAN_POINT('Ctrl Pts',(3.08884299507603,-22.8527768072837,-10.4812824826094)) ;
#51384 = CARTESIAN_POINT('Ctrl Pts',(-8.15040503259386,-21.5722334647209,
-10.7317117782233)) ;
#51385 = CARTESIAN_POINT('Ctrl Pts',(-17.4284858751735,-15.1009350356404,
-10.9821410738372)) ;
#51386 = CARTESIAN_POINT('Ctrl Pts',(-22.5128886799735,-4.9960186283562,-11.232570369451)) ;
#51387 = CARTESIAN_POINT('Ctrl Pts',(-22.180194009962,6.3110500340433,-11.4829996650648)) ;
#51388 = CARTESIAN_POINT('Ctrl Pts',(-16.5104555393895,16.0995408858014,-11.7334289606787)) ;
#51389 = CARTESIAN_POINT('Ctrl Pts',(-6.86793737440163,22.014127170367,-11.9838582562926)) ;
#51390 = CARTESIAN_POINT('Ctrl Pts',(4.42715797589815,22.6316289981103,-12.2342875519064)) ;
#51391 = CARTESIAN_POINT('Ctrl Pts',(14.6569814886892,17.803461812023,-12.4847168475202)) ;
#51392 = CARTESIAN_POINT('Ctrl Pts',(21.3600120368117,8.69138910869525,-12.7351461431341)) ;
#51393 = CARTESIAN_POINT('Ctrl Pts',(22.9233526539321,-2.51202347828334,-12.985575438748)) ;
#51394 = CARTESIAN_POINT('Ctrl Pts',(18.9708291124514,-13.1109878208384,-13.2360047343618)) ;
#51395 = CARTESIAN_POINT('Ctrl Pts',(10.4535057383161,-20.5551593676385,-13.4864340299757)) ;
#51396 = CARTESIAN_POINT('Ctrl Pts',(-0.579161639218072,-23.0533062846188,
-13.7368633255895)) ;
#51397 = CARTESIAN_POINT('Ctrl Pts',(-11.4724699543666,-20.0043193332644,
-13.9872926212034)) ;
#51398 = CARTESIAN_POINT('Ctrl Pts',(-19.6052490058639,-12.14185201225,-14.2377219168172)) ;
#51399 = CARTESIAN_POINT('Ctrl Pts',(-23.0205728071453,-1.35778734095291,
-14.488151212431)) ;
#51400 = CARTESIAN_POINT('Ctrl Pts',(-20.8966391386554,9.75299090331169,-14.7385805080449)) ;
#51401 = CARTESIAN_POINT('Ctrl Pts',(-13.7445132737265,18.5169844682281,-14.9890098036587)) ;
#51402 = CARTESIAN_POINT('Ctrl Pts',(-3.28515442466593,22.8253832168429,-15.2394390992726)) ;
#51403 = CARTESIAN_POINT('Ctrl Pts',(7.96468503575488,21.6414914399017,-15.4898683948864)) ;
#51404 = CARTESIAN_POINT('Ctrl Pts',(17.2980456144141,15.2501795292886,-15.7402976905003)) ;
#51405 = CARTESIAN_POINT('Ctrl Pts',(22.4691150045175,5.18933822426017,-15.9907269861142)) ;
#51406 = CARTESIAN_POINT('Ctrl Pts',(22.2336197411977,-6.12017249021728,-16.241156281728)) ;
#51407 = CARTESIAN_POINT('Ctrl Pts',(16.6482254452527,-15.9570343549712,-16.4915855773418)) ;
#51408 = CARTESIAN_POINT('Ctrl Pts',(7.05690063010837,-21.9542826225338,-16.7420148729558)) ;
#51409 = CARTESIAN_POINT('Ctrl Pts',(-4.23246941534568,-22.6688448677897,
-16.9924441685695)) ;
#51410 = CARTESIAN_POINT('Ctrl Pts',(-14.5034153210617,-17.928786050549,-17.2428734641834)) ;
#51411 = CARTESIAN_POINT('Ctrl Pts',(-21.2845170458594,-8.87466023095568,
-17.4933027597973)) ;
#51412 = CARTESIAN_POINT('Ctrl Pts',(-22.9440997446774,2.31489334409071,-17.7437320554111)) ;
#51413 = CARTESIAN_POINT('Ctrl Pts',(-19.0828159826577,12.9474545088177,-17.994161351025)) ;
#51414 = CARTESIAN_POINT('Ctrl Pts',(-10.6298056821963,20.4645294829176,-18.2445906466388)) ;
#51415 = CARTESIAN_POINT('Ctrl Pts',(0.381009130946933,23.0574719658833,-18.4950199422527)) ;
#51416 = CARTESIAN_POINT('Ctrl Pts',(11.3000685139548,20.1021122617704,-18.7454492378665)) ;
#51417 = CARTESIAN_POINT('Ctrl Pts',(19.5002317951268,12.3100667393077,-18.9958785334804)) ;
#51418 = CARTESIAN_POINT('Ctrl Pts',(23.0079156563239,1.55530782188901,-19.2463078290942)) ;
#51419 = CARTESIAN_POINT('Ctrl Pts',(20.9799656776099,-9.57242705452063,-19.4967371247081)) ;
#51420 = CARTESIAN_POINT('Ctrl Pts',(13.9010937855928,-18.4013181476927,-19.7472203327695)) ;
#51421 = CARTESIAN_POINT('Ctrl Pts',(6.95138205173184,-21.3301728280204,-19.9142271089598)) ;
#51422 = CARTESIAN_POINT('Ctrl Pts',(3.33433033300097,-21.8813254712477,-19.9977574532787)) ;
#51423 = CARTESIAN_POINT('Ctrl Pts',(-17.3962108599074,12.6913527179767,0.692030669808437)) ;
#51424 = CARTESIAN_POINT('Ctrl Pts',(-15.2986421932486,15.5665465205911,0.60851371347137)) ;
#51425 = CARTESIAN_POINT('Ctrl Pts',(-9.65410417889847,20.2530316297668,0.441520325263021)) ;
#51426 = CARTESIAN_POINT('Ctrl Pts',(1.14216883790227,22.4061037619246,0.191050505183387)) ;
#51427 = CARTESIAN_POINT('Ctrl Pts',(11.6591070186625,19.167589505919,-0.0593787904304645)) ;
#51428 = CARTESIAN_POINT('Ctrl Pts',(19.3719586664313,11.3168622280845,-0.309808086044315)) ;
#51429 = CARTESIAN_POINT('Ctrl Pts',(22.4228057440828,0.743081725478456,-0.560237381658167)) ;
#51430 = CARTESIAN_POINT('Ctrl Pts',(20.0785795509029,-10.009517516586,-0.810666677272016)) ;
#51431 = CARTESIAN_POINT('Ctrl Pts',(12.9028268676587,-18.3535975152151,-1.06109597288587)) ;
#51432 = CARTESIAN_POINT('Ctrl Pts',(2.62245996109128,-22.281401595766,-1.31152526849971)) ;
#51433 = CARTESIAN_POINT('Ctrl Pts',(-8.28897474945834,-20.8478068657999,
-1.56195456411357)) ;
#51434 = CARTESIAN_POINT('Ctrl Pts',(-17.2058758443889,-14.3977712023632,
-1.81238385972742)) ;
#51435 = CARTESIAN_POINT('Ctrl Pts',(-21.9826757626381,-4.48331370517877,
-2.06281315534127)) ;
#51436 = CARTESIAN_POINT('Ctrl Pts',(-21.4699530206913,6.50992764064117,-2.31324245095512)) ;
#51437 = CARTESIAN_POINT('Ctrl Pts',(-15.7910892346836,15.936736988708,-2.56367174656897)) ;
#51438 = CARTESIAN_POINT('Ctrl Pts',(-6.31253956449433,21.5288159005788,-2.81410104218282)) ;
#51439 = CARTESIAN_POINT('Ctrl Pts',(4.68494552166555,21.9405869884746,-3.06453033779668)) ;
#51440 = CARTESIAN_POINT('Ctrl Pts',(14.5551298141459,17.0729689890782,-3.31495963341052)) ;
#51441 = CARTESIAN_POINT('Ctrl Pts',(20.9230286908485,8.09721816479448,-3.56538892902439)) ;
#51442 = CARTESIAN_POINT('Ctrl Pts',(22.2563855730833,-2.82690191648573,-3.81581822463822)) ;
#51443 = CARTESIAN_POINT('Ctrl Pts',(18.2343652299033,-13.0708070546494,-4.06624752025209)) ;
#51444 = CARTESIAN_POINT('Ctrl Pts',(9.82475453261194,-20.1695877769427,-4.31667681586593)) ;
#51445 = CARTESIAN_POINT('Ctrl Pts',(-0.948908776719674,-22.4151208959148,
-4.56710611147979)) ;
#51446 = CARTESIAN_POINT('Ctrl Pts',(-11.4942437016324,-19.2670816252636,
-4.81753540709363)) ;
#51447 = CARTESIAN_POINT('Ctrl Pts',(-19.2738101224156,-11.4829576341271,
-5.06796470270747)) ;
#51448 = CARTESIAN_POINT('Ctrl Pts',(-22.4156727962215,-0.93578081199245,
-5.31839399832132)) ;
#51449 = CARTESIAN_POINT('Ctrl Pts',(-20.1638302816266,9.83656550956651,-5.56882329393518)) ;
#51450 = CARTESIAN_POINT('Ctrl Pts',(-13.0601255442479,18.2420172517274,-5.81925258954903)) ;
#51451 = CARTESIAN_POINT('Ctrl Pts',(-2.81386659685344,22.2580373667766,-6.06968188516289)) ;
#51452 = CARTESIAN_POINT('Ctrl Pts',(8.10947070578031,20.9182828529922,-6.32011118077673)) ;
#51453 = CARTESIAN_POINT('Ctrl Pts',(17.081490524982,14.5451281909156,-6.57054047639058)) ;
#51454 = CARTESIAN_POINT('Ctrl Pts',(21.9433270396991,4.67209493423049,-6.82096977200444)) ;
#51455 = CARTESIAN_POINT('Ctrl Pts',(21.5251151703174,-6.32514739353649,-7.07139906761828)) ;
#51456 = CARTESIAN_POINT('Ctrl Pts',(15.9274859151215,-15.8004197750919,-7.32182836323213)) ;
#51457 = CARTESIAN_POINT('Ctrl Pts',(6.49735231286047,-21.4737627249635,-7.572257658846)) ;
#51458 = CARTESIAN_POINT('Ctrl Pts',(-4.49618753669457,-21.9800448197985,
-7.82268695445983)) ;
#51459 = CARTESIAN_POINT('Ctrl Pts',(-14.407845514158,-17.197443422952,-8.07311625007371)) ;
#51460 = CARTESIAN_POINT('Ctrl Pts',(-20.8526581364247,-8.27675789732166,
-8.32354554568752)) ;
#51461 = CARTESIAN_POINT('Ctrl Pts',(-22.2798613643712,2.63549809900938,-8.5739748413014)) ;
#51462 = CARTESIAN_POINT('Ctrl Pts',(-18.3460386284019,12.9135951342243,-8.82440413691524)) ;
#51463 = CARTESIAN_POINT('Ctrl Pts',(-9.99775442818221,20.0843964071426,-9.07483343252909)) ;
#51464 = CARTESIAN_POINT('Ctrl Pts',(0.756209959798816,22.4224489996561,-9.32526272814294)) ;
#51465 = CARTESIAN_POINT('Ctrl Pts',(11.3282135553694,19.3651658988355,-9.57569202375679)) ;
#51466 = CARTESIAN_POINT('Ctrl Pts',(19.1743991576454,11.6481968385139,-9.82612131937065)) ;
#51467 = CARTESIAN_POINT('Ctrl Pts',(22.4068014851743,1.12841475064213,-10.0765506149845)) ;
#51468 = CARTESIAN_POINT('Ctrl Pts',(20.2476332564153,-9.66288881024618,-10.3269799105984)) ;
#51469 = CARTESIAN_POINT('Ctrl Pts',(13.2164379615872,-18.1290882355676,-10.5774092062123)) ;
#51470 = CARTESIAN_POINT('Ctrl Pts',(3.00507624185253,-22.2330292453847,-10.8278385018261)) ;
#51471 = CARTESIAN_POINT('Ctrl Pts',(-7.92937309017233,-20.9872131318651,
-11.07826779744)) ;
#51472 = CARTESIAN_POINT('Ctrl Pts',(-16.955840396691,-14.69141072489,-11.3286970930538)) ;
#51473 = CARTESIAN_POINT('Ctrl Pts',(-21.902358590419,-4.8605309197842,-11.5791263886677)) ;
#51474 = CARTESIAN_POINT('Ctrl Pts',(-21.5786863124056,6.13989980995436,-11.8295556842815)) ;
#51475 = CARTESIAN_POINT('Ctrl Pts',(-16.0627062504226,15.6629352472039,-12.0799849798954)) ;
#51476 = CARTESIAN_POINT('Ctrl Pts',(-6.68168484680049,21.4171230620162,-12.3304142755092)) ;
#51477 = CARTESIAN_POINT('Ctrl Pts',(4.30709727671738,22.0178787737213,-12.5808435711231)) ;
#51478 = CARTESIAN_POINT('Ctrl Pts',(14.2594968145501,17.3206473101176,-12.8312728667369)) ;
#51479 = CARTESIAN_POINT('Ctrl Pts',(20.7807469657185,8.45568614554753,-13.0817021623508)) ;
#51480 = CARTESIAN_POINT('Ctrl Pts',(22.3016911360505,-2.44389957197528,-13.3321314579646)) ;
#51481 = CARTESIAN_POINT('Ctrl Pts',(18.4563566179797,-12.7554291592116,-13.5825607535785)) ;
#51482 = CARTESIAN_POINT('Ctrl Pts',(10.1700156946661,-19.9977212055294,-13.8329900491923)) ;
#51483 = CARTESIAN_POINT('Ctrl Pts',(-0.563455275966131,-22.4281205365546,
-14.0834193448062)) ;
#51484 = CARTESIAN_POINT('Ctrl Pts',(-11.1613464815765,-19.4618194769542,
-14.33384864042)) ;
#51485 = CARTESIAN_POINT('Ctrl Pts',(-19.0735715920305,-11.8125754764054,
-14.5842779360339)) ;
#51486 = CARTESIAN_POINT('Ctrl Pts',(-22.3962747627081,-1.32096532141325,
-14.8347072316477)) ;
#51487 = CARTESIAN_POINT('Ctrl Pts',(-20.3299403401995,9.4884982167326,-15.0851365272616)) ;
#51488 = CARTESIAN_POINT('Ctrl Pts',(-13.3717739491923,18.0148198483798,-15.3355658228754)) ;
#51489 = CARTESIAN_POINT('Ctrl Pts',(-3.19606387508772,22.2063785454482,-15.5859951184893)) ;
#51490 = CARTESIAN_POINT('Ctrl Pts',(7.74868965918299,21.0545928905987,-15.8364244141031)) ;
#51491 = CARTESIAN_POINT('Ctrl Pts',(16.8289375631012,14.8366078368198,-16.086853709717)) ;
#51492 = CARTESIAN_POINT('Ctrl Pts',(21.8597720192203,5.04860785527804,-16.3372830053308)) ;
#51493 = CARTESIAN_POINT('Ctrl Pts',(21.6306631839706,-5.95419870019608,-16.5877123009447)) ;
#51494 = CARTESIAN_POINT('Ctrl Pts',(16.1967399554739,-15.5242933703622,-16.8381415965585)) ;
#51495 = CARTESIAN_POINT('Ctrl Pts',(6.86552358227933,-21.3589014466138,-17.0885708921724)) ;
#51496 = CARTESIAN_POINT('Ctrl Pts',(-4.11768850171349,-22.0540853811699,
-17.3390001877862)) ;
#51497 = CARTESIAN_POINT('Ctrl Pts',(-14.1100952287054,-17.4425728635766,
-17.5894294834001)) ;
#51498 = CARTESIAN_POINT('Ctrl Pts',(-20.7072993336923,-8.63398711332103,
-17.8398587790139)) ;
#51499 = CARTESIAN_POINT('Ctrl Pts',(-22.3218755836205,2.25211543669878,-18.0902880746278)) ;
#51500 = CARTESIAN_POINT('Ctrl Pts',(-18.5653065010242,12.5963307293179,-18.3407173702416)) ;
#51501 = CARTESIAN_POINT('Ctrl Pts',(-10.3415345363939,19.9095491249766,-18.5911466658555)) ;
#51502 = CARTESIAN_POINT('Ctrl Pts',(0.370676492512795,22.4321732481425,-18.8415759614693)) ;
#51503 = CARTESIAN_POINT('Ctrl Pts',(10.9936204192713,19.5569603457334,-19.0920052570832)) ;
#51504 = CARTESIAN_POINT('Ctrl Pts',(18.9714023573123,11.9762283654051,-19.342434552697)) ;
#51505 = CARTESIAN_POINT('Ctrl Pts',(22.3839608628809,1.51312921756678,-19.5928638483109)) ;
#51506 = CARTESIAN_POINT('Ctrl Pts',(20.4110071354131,-9.31283110351108,-19.8432931439247)) ;
#51507 = CARTESIAN_POINT('Ctrl Pts',(13.5241081328644,-17.9022902985201,-20.0937763519862)) ;
#51508 = CARTESIAN_POINT('Ctrl Pts',(6.76286657657885,-20.7517169704882,-20.2607831281764)) ;
#51509 = CARTESIAN_POINT('Ctrl Pts',(3.24390617527739,-21.2879228302346,-20.3443134724953)) ;
#51510 = CARTESIAN_POINT('Ctrl Pts',(-16.9112900176904,12.3375801925435,0.345474650591894)) ;
#51511 = CARTESIAN_POINT('Ctrl Pts',(-14.872191254198,15.1326277258625,0.261957694254827)) ;
#51512 = CARTESIAN_POINT('Ctrl Pts',(-9.38499521218246,19.6884766680889,0.0949643060464787)) ;
#51513 = CARTESIAN_POINT('Ctrl Pts',(1.11033078539246,21.7815317333067,-0.155505514033156)) ;
#51514 = CARTESIAN_POINT('Ctrl Pts',(11.3341084289973,18.6332913348211,-0.405934809647006)) ;
#51515 = CARTESIAN_POINT('Ctrl Pts',(18.8319636877793,11.0014037407683,-0.656364105260858)) ;
#51516 = CARTESIAN_POINT('Ctrl Pts',(21.7977681463063,0.722368259824523,-0.906793400874708)) ;
#51517 = CARTESIAN_POINT('Ctrl Pts',(19.5188874556096,-9.73050137316158,-1.15722269648855)) ;
#51518 = CARTESIAN_POINT('Ctrl Pts',(12.5431594825004,-17.8419894393837,-1.4076519921024)) ;
#51519 = CARTESIAN_POINT('Ctrl Pts',(2.54935866890447,-21.6603056505278,-1.65808128771625)) ;
#51520 = CARTESIAN_POINT('Ctrl Pts',(-8.0579188805112,-20.2666724943465,-1.90851058333011)) ;
#51521 = CARTESIAN_POINT('Ctrl Pts',(-16.7262606067527,-13.9964321180233,
-2.15893987894396)) ;
#51522 = CARTESIAN_POINT('Ctrl Pts',(-21.3699068251464,-4.35834095821984,
-2.40936917455781)) ;
#51523 = CARTESIAN_POINT('Ctrl Pts',(-20.8714762727951,6.32846285962108,-2.65979847017166)) ;
#51524 = CARTESIAN_POINT('Ctrl Pts',(-15.3509112928965,15.4924991035161,-2.91022776578551)) ;
#51525 = CARTESIAN_POINT('Ctrl Pts',(-6.13657699271392,20.9286983449502,-3.16065706139936)) ;
#51526 = CARTESIAN_POINT('Ctrl Pts',(4.55435227084776,21.3289912791062,-3.41108635701321)) ;
#51527 = CARTESIAN_POINT('Ctrl Pts',(14.1494043452553,16.5970585412225,-3.66151565262706)) ;
#51528 = CARTESIAN_POINT('Ctrl Pts',(20.3397975046893,7.87150752678782,-3.91194494824091)) ;
#51529 = CARTESIAN_POINT('Ctrl Pts',(21.6359869515834,-2.74810178758143,-4.16237424385476)) ;
#51530 = CARTESIAN_POINT('Ctrl Pts',(17.7260807640627,-12.7064572076373,-4.41280353946861)) ;
#51531 = CARTESIAN_POINT('Ctrl Pts',(9.55088867291999,-19.607358819687,-4.66323283508247)) ;
#51532 = CARTESIAN_POINT('Ctrl Pts',(-0.922457864684889,-21.7902975139278,
-4.9136621306963)) ;
#51533 = CARTESIAN_POINT('Ctrl Pts',(-11.1738406908084,-18.7300101029632,
-5.16409142631018)) ;
#51534 = CARTESIAN_POINT('Ctrl Pts',(-18.7365510426908,-11.1628692233849,
-5.414520721924)) ;
#51535 = CARTESIAN_POINT('Ctrl Pts',(-21.790834029967,-0.90969584307959,-5.66495001753788)) ;
#51536 = CARTESIAN_POINT('Ctrl Pts',(-19.6017618150375,9.56237041789767,-5.91537931315171)) ;
#51537 = CARTESIAN_POINT('Ctrl Pts',(-12.6960734452374,17.7335194851344,-6.16580860876558)) ;
#51538 = CARTESIAN_POINT('Ctrl Pts',(-2.73542982858124,21.6375927013884,-6.41623790437941)) ;
#51539 = CARTESIAN_POINT('Ctrl Pts',(7.88341852716223,20.3351839574628,-6.66666719999328)) ;
#51540 = CARTESIAN_POINT('Ctrl Pts',(16.6053425385957,14.1396815181147,-6.91709649560712)) ;
#51541 = CARTESIAN_POINT('Ctrl Pts',(21.331654951172,4.54185989461926,-7.16752579122098)) ;
#51542 = CARTESIAN_POINT('Ctrl Pts',(20.9251007728565,-6.14883337746017,-7.41795508683483)) ;
#51543 = CARTESIAN_POINT('Ctrl Pts',(15.4835059043847,-15.3599817437055,-7.66838438244868)) ;
#51544 = CARTESIAN_POINT('Ctrl Pts',(6.31623807016093,-20.87517978124,-7.91881367806253)) ;
#51545 = CARTESIAN_POINT('Ctrl Pts',(-4.37085593059841,-21.36734922006,-8.16924297367638)) ;
#51546 = CARTESIAN_POINT('Ctrl Pts',(-14.0062256075287,-16.7180632397733,
-8.41967226929022)) ;
#51547 = CARTESIAN_POINT('Ctrl Pts',(-20.2713885353943,-8.04604257415629,
-8.67010156490409)) ;
#51548 = CARTESIAN_POINT('Ctrl Pts',(-21.6588083532127,2.56203336763053,-8.92053086051792)) ;
#51549 = CARTESIAN_POINT('Ctrl Pts',(-17.8346412571768,12.5536275827289,-9.17096015613178)) ;
#51550 = CARTESIAN_POINT('Ctrl Pts',(-9.71906618183729,19.5245421664919,-9.42138945174563)) ;
#51551 = CARTESIAN_POINT('Ctrl Pts',(0.735130543508015,21.7974213461604,-9.67181874735948)) ;
#51552 = CARTESIAN_POINT('Ctrl Pts',(11.0124386488497,18.8253602691521,-9.92224804297333)) ;
#51553 = CARTESIAN_POINT('Ctrl Pts',(18.6399111669323,11.3235023710388,-10.1726773385872)) ;
#51554 = CARTESIAN_POINT('Ctrl Pts',(21.7822100074621,1.09696009447255,-10.423106634201)) ;
#51555 = CARTESIAN_POINT('Ctrl Pts',(19.6832287748491,-9.39353497119186,-10.6735359298149)) ;
#51556 = CARTESIAN_POINT('Ctrl Pts',(12.8480286407844,-17.6237383748068,-10.9239652254287)) ;
#51557 = CARTESIAN_POINT('Ctrl Pts',(2.92130948862902,-21.6132816834856,-11.1743945210426)) ;
#51558 = CARTESIAN_POINT('Ctrl Pts',(-7.7083411477508,-20.4021927990092,-11.4248238166564)) ;
#51559 = CARTESIAN_POINT('Ctrl Pts',(-16.4831949182086,-14.2818864141397,
-11.6752531122703)) ;
#51560 = CARTESIAN_POINT('Ctrl Pts',(-21.2918285008646,-4.72504321121219,
-11.9256824078841)) ;
#51561 = CARTESIAN_POINT('Ctrl Pts',(-20.9771786148489,5.96874958586541,-12.176111703498)) ;
#51562 = CARTESIAN_POINT('Ctrl Pts',(-15.6149569614558,15.2263296086064,-12.4265409991118)) ;
#51563 = CARTESIAN_POINT('Ctrl Pts',(-6.49543231919935,20.8201189536655,-12.6769702947257)) ;
#51564 = CARTESIAN_POINT('Ctrl Pts',(4.1870365775366,21.4041285493321,-12.9273995903395)) ;
#51565 = CARTESIAN_POINT('Ctrl Pts',(13.8620121404112,16.8378328082122,-13.1778288859534)) ;
#51566 = CARTESIAN_POINT('Ctrl Pts',(20.2014818946252,8.2199831823998,-13.4282581815672)) ;
#51567 = CARTESIAN_POINT('Ctrl Pts',(21.6800296181687,-2.37577566566717,-13.6786874771811)) ;
#51568 = CARTESIAN_POINT('Ctrl Pts',(17.9418841235082,-12.3998704975848,-13.9291167727949)) ;
#51569 = CARTESIAN_POINT('Ctrl Pts',(9.88652565101624,-19.4402830434204,-14.1795460684088)) ;
#51570 = CARTESIAN_POINT('Ctrl Pts',(-0.547748912714191,-21.8029347884905,
-14.4299753640226)) ;
#51571 = CARTESIAN_POINT('Ctrl Pts',(-10.8502230087865,-18.919319620644,-14.6804046596365)) ;
#51572 = CARTESIAN_POINT('Ctrl Pts',(-18.5418941781971,-11.483298940561,-14.9308339552503)) ;
#51573 = CARTESIAN_POINT('Ctrl Pts',(-21.7719767182707,-1.28414330187359,
-15.1812632508642)) ;
#51574 = CARTESIAN_POINT('Ctrl Pts',(-19.7632415417438,9.22400553015349,-15.431692546478)) ;
#51575 = CARTESIAN_POINT('Ctrl Pts',(-12.9990346246578,17.5126552285315,-15.6821218420919)) ;
#51576 = CARTESIAN_POINT('Ctrl Pts',(-3.10697332550952,21.5873738740534,-15.9325511377058)) ;
#51577 = CARTESIAN_POINT('Ctrl Pts',(7.53269428261108,20.4676943412959,-16.1829804333196)) ;
#51578 = CARTESIAN_POINT('Ctrl Pts',(16.3598295117884,14.423036144351,-16.4334097289334)) ;
#51579 = CARTESIAN_POINT('Ctrl Pts',(21.2504290339233,4.90787748629594,-16.6838390245473)) ;
#51580 = CARTESIAN_POINT('Ctrl Pts',(21.0277066267436,-5.78822491017488,-16.9342683201612)) ;
#51581 = CARTESIAN_POINT('Ctrl Pts',(15.7452544656953,-15.0915523857532,-17.184697615775)) ;
#51582 = CARTESIAN_POINT('Ctrl Pts',(6.6741465344503,-20.7635202706937,-17.4351269113889)) ;
#51583 = CARTESIAN_POINT('Ctrl Pts',(-4.00290758808131,-21.4393258945502,
-17.6855562070027)) ;
#51584 = CARTESIAN_POINT('Ctrl Pts',(-13.7167751363492,-16.9563596766042,
-17.9359855026166)) ;
#51585 = CARTESIAN_POINT('Ctrl Pts',(-20.1300816215249,-8.39331399568637,
-18.1864147982304)) ;
#51586 = CARTESIAN_POINT('Ctrl Pts',(-21.6996514225636,2.18933752930682,-18.4368440938443)) ;
#51587 = CARTESIAN_POINT('Ctrl Pts',(-18.0477970193908,12.2452069498181,-18.6872733894581)) ;
#51588 = CARTESIAN_POINT('Ctrl Pts',(-10.0532633905914,19.3545687670357,-18.937702685072)) ;
#51589 = CARTESIAN_POINT('Ctrl Pts',(0.36034385407868,21.8068745304016,-19.1881319806858)) ;
#51590 = CARTESIAN_POINT('Ctrl Pts',(10.687172324588,19.0118084296965,-19.4385612762997)) ;
#51591 = CARTESIAN_POINT('Ctrl Pts',(18.4425729194978,11.6423899915026,-19.6889905719135)) ;
#51592 = CARTESIAN_POINT('Ctrl Pts',(21.7600060694379,1.47095061324456,-19.9394198675273)) ;
#51593 = CARTESIAN_POINT('Ctrl Pts',(19.842048593216,-9.05323515250154,-20.1898491631412)) ;
#51594 = CARTESIAN_POINT('Ctrl Pts',(13.1471224801359,-17.4032624493475,-20.4403323712028)) ;
#51595 = CARTESIAN_POINT('Ctrl Pts',(6.57435110142589,-20.1732611129558,-20.6073391473929)) ;
#51596 = CARTESIAN_POINT('Ctrl Pts',(3.1534820175538,-20.6945201892214,-20.6908694917118)) ;
#51597 = CARTESIAN_POINT('Ctrl Pts',(-16.4263691754732,11.9838076671105,-0.00108136862464728)) ;
#51598 = CARTESIAN_POINT('Ctrl Pts',(-14.4457403151475,14.6987089311338,-0.084598324961714)) ;
#51599 = CARTESIAN_POINT('Ctrl Pts',(-9.11588624546646,19.123921706411,-0.251591713170063)) ;
#51600 = CARTESIAN_POINT('Ctrl Pts',(1.07849273288265,21.1569597046888,-0.502061533249697)) ;
#51601 = CARTESIAN_POINT('Ctrl Pts',(11.0091098393319,18.0989931637232,-0.752490828863548)) ;
#51602 = CARTESIAN_POINT('Ctrl Pts',(18.2919687091274,10.6859452534523,-1.0029201244774)) ;
#51603 = CARTESIAN_POINT('Ctrl Pts',(21.1727305485295,0.701654794170591,-1.25334942009125)) ;
#51604 = CARTESIAN_POINT('Ctrl Pts',(18.9591953603162,-9.45148522973715,-1.5037787157051)) ;
#51605 = CARTESIAN_POINT('Ctrl Pts',(12.183492097342,-17.3303813635526,-1.75420801131895)) ;
#51606 = CARTESIAN_POINT('Ctrl Pts',(2.47625737671769,-21.0392097052897,-2.0046373069328)) ;
#51607 = CARTESIAN_POINT('Ctrl Pts',(-7.82686301156406,-19.685538122893,-2.25506660254666)) ;
#51608 = CARTESIAN_POINT('Ctrl Pts',(-16.2466453691165,-13.5950930336833,
-2.50549589816051)) ;
#51609 = CARTESIAN_POINT('Ctrl Pts',(-20.7571378876549,-4.23336821126094,
-2.75592519377435)) ;
#51610 = CARTESIAN_POINT('Ctrl Pts',(-20.2729995248988,6.14699807860102,-3.00635448938821)) ;
#51611 = CARTESIAN_POINT('Ctrl Pts',(-14.9107333511094,15.0482612183243,-3.25678378500206)) ;
#51612 = CARTESIAN_POINT('Ctrl Pts',(-5.96061442093349,20.3285807893217,-3.50721308061591)) ;
#51613 = CARTESIAN_POINT('Ctrl Pts',(4.42375902002995,20.7173955697377,-3.75764237622976)) ;
#51614 = CARTESIAN_POINT('Ctrl Pts',(13.7436788763648,16.1211480933668,-4.0080716718436)) ;
#51615 = CARTESIAN_POINT('Ctrl Pts',(19.75656631853,7.64579688878116,-4.25850096745746)) ;
#51616 = CARTESIAN_POINT('Ctrl Pts',(21.0155883300835,-2.66930165867712,-4.50893026307131)) ;
#51617 = CARTESIAN_POINT('Ctrl Pts',(17.217796298222,-12.3421073606251,-4.75935955868516)) ;
#51618 = CARTESIAN_POINT('Ctrl Pts',(9.27702281322807,-19.0451298624311,-5.00978885429902)) ;
#51619 = CARTESIAN_POINT('Ctrl Pts',(-0.896006952650112,-21.1654741319408,
-5.26021814991286)) ;
#51620 = CARTESIAN_POINT('Ctrl Pts',(-10.8534376799843,-18.1929385806628,
-5.51064744552672)) ;
#51621 = CARTESIAN_POINT('Ctrl Pts',(-18.1992919629658,-10.8427808126426,
-5.76107674114056)) ;
#51622 = CARTESIAN_POINT('Ctrl Pts',(-21.1659952637126,-0.883610874166736,
-6.01150603675442)) ;
#51623 = CARTESIAN_POINT('Ctrl Pts',(-19.0396933484483,9.28817532622884,-6.26193533236826)) ;
#51624 = CARTESIAN_POINT('Ctrl Pts',(-12.3320213462269,17.2250217185411,-6.51236462798212)) ;
#51625 = CARTESIAN_POINT('Ctrl Pts',(-2.65699306030903,21.0171480360003,-6.76279392359596)) ;
#51626 = CARTESIAN_POINT('Ctrl Pts',(7.65736634854412,19.7520850619333,-7.01322321920982)) ;
#51627 = CARTESIAN_POINT('Ctrl Pts',(16.1291945522093,13.7342348453136,-7.26365251482367)) ;
#51628 = CARTESIAN_POINT('Ctrl Pts',(20.719982862645,4.41162485500801,-7.51408181043751)) ;
#51629 = CARTESIAN_POINT('Ctrl Pts',(20.3250863753955,-5.97251936138383,-7.76451110605137)) ;
#51630 = CARTESIAN_POINT('Ctrl Pts',(15.0395258936478,-14.919543712319,-8.01494040166522)) ;
#51631 = CARTESIAN_POINT('Ctrl Pts',(6.13512382746137,-20.2765968375164,-8.26536969727907)) ;
#51632 = CARTESIAN_POINT('Ctrl Pts',(-4.24552432450223,-20.7546536203216,
-8.51579899289292)) ;
#51633 = CARTESIAN_POINT('Ctrl Pts',(-13.6046057008994,-16.2386830565945,
-8.76622828850679)) ;
#51634 = CARTESIAN_POINT('Ctrl Pts',(-19.6901189343637,-7.81532725099089,
-9.01665758412061)) ;
#51635 = CARTESIAN_POINT('Ctrl Pts',(-21.0377553420544,2.48856863625166,-9.26708687973448)) ;
#51636 = CARTESIAN_POINT('Ctrl Pts',(-17.3232438859519,12.1936600312335,-9.51751617534832)) ;
#51637 = CARTESIAN_POINT('Ctrl Pts',(-9.44037793549236,18.964687925841,-9.76794547096218)) ;
#51638 = CARTESIAN_POINT('Ctrl Pts',(0.714051127217217,21.1723936926648,-10.018374766576)) ;
#51639 = CARTESIAN_POINT('Ctrl Pts',(10.6966637423299,18.2855546394686,-10.2688040621899)) ;
#51640 = CARTESIAN_POINT('Ctrl Pts',(18.1054231762193,10.9988079035636,-10.5192333578037)) ;
#51641 = CARTESIAN_POINT('Ctrl Pts',(21.1576185297499,1.06550543830298,-10.7696626534176)) ;
#51642 = CARTESIAN_POINT('Ctrl Pts',(19.1188242932827,-9.12418113213751,-11.0200919490314)) ;
#51643 = CARTESIAN_POINT('Ctrl Pts',(12.4796193199814,-17.1183885140459,-11.2705212446453)) ;
#51644 = CARTESIAN_POINT('Ctrl Pts',(2.83754273540551,-20.9935341215866,-11.5209505402591)) ;
#51645 = CARTESIAN_POINT('Ctrl Pts',(-7.48730920532926,-19.8171724661533,
-11.771379835873)) ;
#51646 = CARTESIAN_POINT('Ctrl Pts',(-16.0105494397262,-13.8723621033893,
-12.0218091314868)) ;
#51647 = CARTESIAN_POINT('Ctrl Pts',(-20.6812984113101,-4.58955550264018,
-12.2722384271007)) ;
#51648 = CARTESIAN_POINT('Ctrl Pts',(-20.3756709172924,5.79759936177647,-12.5226677227145)) ;
#51649 = CARTESIAN_POINT('Ctrl Pts',(-15.1672076724889,14.789723970009,-12.7730970183284)) ;
#51650 = CARTESIAN_POINT('Ctrl Pts',(-6.30917979159822,20.2231148453148,-13.0235263139422)) ;
#51651 = CARTESIAN_POINT('Ctrl Pts',(4.06697587835583,20.7903783249431,-13.2739556095561)) ;
#51652 = CARTESIAN_POINT('Ctrl Pts',(13.4645274662721,16.3550183063067,-13.5243849051699)) ;
#51653 = CARTESIAN_POINT('Ctrl Pts',(19.622216823532,7.9842802192521,-13.7748142007838)) ;
#51654 = CARTESIAN_POINT('Ctrl Pts',(21.0583681002872,-2.30765175935909,-14.0252434963976)) ;
#51655 = CARTESIAN_POINT('Ctrl Pts',(17.4274116290366,-12.0443118359581,-14.2756727920115)) ;
#51656 = CARTESIAN_POINT('Ctrl Pts',(9.60303560736628,-18.8828448813113,-14.5261020876253)) ;
#51657 = CARTESIAN_POINT('Ctrl Pts',(-0.532042549462259,-21.1777490404263,
-14.7765313832392)) ;
#51658 = CARTESIAN_POINT('Ctrl Pts',(-10.5390995359964,-18.3768197643338,
-15.026960678853)) ;
#51659 = CARTESIAN_POINT('Ctrl Pts',(-18.0102167643638,-11.1540224047163,
-15.2773899744669)) ;
#51660 = CARTESIAN_POINT('Ctrl Pts',(-21.1476786738334,-1.24732128233393,
-15.5278192700807)) ;
#51661 = CARTESIAN_POINT('Ctrl Pts',(-19.1965427432879,8.95951284357439,-15.7782485656946)) ;
#51662 = CARTESIAN_POINT('Ctrl Pts',(-12.6262953001234,17.0104906086833,-16.0286778613084)) ;
#51663 = CARTESIAN_POINT('Ctrl Pts',(-3.01788277593133,20.9683692026586,-16.2791071569223)) ;
#51664 = CARTESIAN_POINT('Ctrl Pts',(7.31669890603918,19.8807957919929,-16.5295364525362)) ;
#51665 = CARTESIAN_POINT('Ctrl Pts',(15.8907214604756,14.0094644518822,-16.77996574815)) ;
#51666 = CARTESIAN_POINT('Ctrl Pts',(20.6410860486261,4.76714711731379,-17.0303950437638)) ;
#51667 = CARTESIAN_POINT('Ctrl Pts',(20.4247500695165,-5.62225112015366,-17.2808243393777)) ;
#51668 = CARTESIAN_POINT('Ctrl Pts',(15.2937689759164,-14.6588114011443,-17.5312536349915)) ;
#51669 = CARTESIAN_POINT('Ctrl Pts',(6.48276948662126,-20.1681390947737,-17.7816829306054)) ;
#51670 = CARTESIAN_POINT('Ctrl Pts',(-3.88812667444911,-20.8245664079305,
-18.0321122262192)) ;
#51671 = CARTESIAN_POINT('Ctrl Pts',(-13.3234550439929,-16.4701464896319,
-18.2825415218331)) ;
#51672 = CARTESIAN_POINT('Ctrl Pts',(-19.5528639093576,-8.15264087805174,
-18.5329708174469)) ;
#51673 = CARTESIAN_POINT('Ctrl Pts',(-21.0774272615067,2.12655962191487,-18.7834001130608)) ;
#51674 = CARTESIAN_POINT('Ctrl Pts',(-17.5302875377575,11.8940831703183,-19.0338294086746)) ;
#51675 = CARTESIAN_POINT('Ctrl Pts',(-9.76499224478906,18.7995884090949,-19.2842587042885)) ;
#51676 = CARTESIAN_POINT('Ctrl Pts',(0.350011215644548,21.1815758126608,-19.5346879999023)) ;
#51677 = CARTESIAN_POINT('Ctrl Pts',(10.3807242299048,18.4666565136597,-19.7851172955162)) ;
#51678 = CARTESIAN_POINT('Ctrl Pts',(17.9137434816832,11.3085516176001,-20.03554659113)) ;
#51679 = CARTESIAN_POINT('Ctrl Pts',(21.1360512759951,1.42877200892233,-20.2859758867439)) ;
#51680 = CARTESIAN_POINT('Ctrl Pts',(19.273090051019,-8.793639201492,-20.5364051823577)) ;
#51681 = CARTESIAN_POINT('Ctrl Pts',(12.7701368274074,-16.9042346001747,-20.7868883904192)) ;
#51682 = CARTESIAN_POINT('Ctrl Pts',(6.3858356262729,-19.5948052554236,-20.9538951666095)) ;
#51683 = CARTESIAN_POINT('Ctrl Pts',(3.06305785983022,-20.1011175482083,-21.0374255109284)) ;
#51684 = CARTESIAN_POINT('',(16.4193236035816,11.9978307730923,-20.0002857096829)) ;
#51685 = CARTESIAN_POINT('Ctrl Pts',(16.4197292796609,11.9981151325406,-19.9999999999999)) ;
#51686 = CARTESIAN_POINT('Ctrl Pts',(16.6862133039597,11.6651737505463,-20.)) ;
#51687 = CARTESIAN_POINT('Ctrl Pts',(16.9417323578455,11.3243161017761,-20.)) ;
#51688 = CARTESIAN_POINT('Ctrl Pts',(17.1858733884563,10.9760266131827,-20.)) ;
#51689 = CARTESIAN_POINT('Ctrl Pts',(17.2064494004021,10.9466730520056,-20.)) ;
#51690 = CARTESIAN_POINT('Ctrl Pts',(17.2269445780442,10.9172666767459,-20.)) ;
#51691 = CARTESIAN_POINT('Ctrl Pts',(17.247358664803,10.8878077633562,-20.)) ;
#51692 = CARTESIAN_POINT('Ctrl Pts',(17.4900365983564,10.5376070264538,-20.)) ;
#51693 = CARTESIAN_POINT('Ctrl Pts',(17.7212580268335,10.1799851561655,-20.)) ;
#51694 = CARTESIAN_POINT('Ctrl Pts',(17.9409219607083,9.81560429891178,-20.)) ;
#51695 = CARTESIAN_POINT('Ctrl Pts',(18.1595616319545,9.45292249934163,-20.)) ;
#51696 = CARTESIAN_POINT('Ctrl Pts',(18.3667515113989,9.08354407349083,-20.)) ;
#51697 = CARTESIAN_POINT('Ctrl Pts',(18.5623524443059,8.70808474634139,-20.)) ;
#51698 = CARTESIAN_POINT('Ctrl Pts',(18.7589822028964,8.33065057074363,-20.)) ;
#51699 = CARTESIAN_POINT('Ctrl Pts',(18.9439010327212,7.94707088429373,-20.)) ;
#51700 = CARTESIAN_POINT('Ctrl Pts',(19.1169242226168,7.55794089715604,-20.)) ;
#51701 = CARTESIAN_POINT('Ctrl Pts',(19.2899858008947,7.16872457436191,-20.)) ;
#51702 = CARTESIAN_POINT('Ctrl Pts',(19.451146684296,6.77395498478179,-20.)) ;
#51703 = CARTESIAN_POINT('Ctrl Pts',(19.6001752754721,6.37420488768944,-20.)) ;
#51704 = CARTESIAN_POINT('Ctrl Pts',(19.7492082704025,5.9744429780903,-20.)) ;
#51705 = CARTESIAN_POINT('Ctrl Pts',(19.8861084889852,5.56969975867407,-20.)) ;
#51706 = CARTESIAN_POINT('Ctrl Pts',(20.010594127929,5.16053277403186,-20.)) ;
#51707 = CARTESIAN_POINT('Ctrl Pts',(20.029874433682,5.09716109007805,-20.)) ;
#51708 = CARTESIAN_POINT('Ctrl Pts',(20.0488574581927,5.03368115903446,-20.)) ;
#51709 = CARTESIAN_POINT('Ctrl Pts',(20.0675400518462,4.97010181780182,-20.)) ;
#51710 = CARTESIAN_POINT('Ctrl Pts',(20.0825290409452,4.91909230218903,-20.)) ;
#51711 = CARTESIAN_POINT('Ctrl Pts',(20.0973224475511,4.86802621134112,-20.)) ;
#51712 = CARTESIAN_POINT('Ctrl Pts',(20.1119161689802,4.81691812032873,-20.)) ;
#51713 = CARTESIAN_POINT('Ctrl Pts',(20.2302152409695,4.40262764841097,-20.)) ;
#51714 = CARTESIAN_POINT('Ctrl Pts',(20.3354841370377,3.98528158528001,-20.)) ;
#51715 = CARTESIAN_POINT('Ctrl Pts',(20.427602726343,3.56551255586273,-20.)) ;
#51716 = CARTESIAN_POINT('Ctrl Pts',(20.5202217737677,3.14346302236244,-20.)) ;
#51717 = CARTESIAN_POINT('Ctrl Pts',(20.5995474842104,2.71896362856786,-20.)) ;
#51718 = CARTESIAN_POINT('Ctrl Pts',(20.6654124192146,2.29263066822524,-20.)) ;
#51719 = CARTESIAN_POINT('Ctrl Pts',(20.7109932711171,1.99759326288532,-20.)) ;
#51720 = CARTESIAN_POINT('Ctrl Pts',(20.7501266438824,1.70167717908982,-20.)) ;
#51721 = CARTESIAN_POINT('Ctrl Pts',(20.7827435110061,1.40508115597038,-20.)) ;
#51722 = CARTESIAN_POINT('Ctrl Pts',(20.8295945595039,0.979048986458191,-20.)) ;
#51723 = CARTESIAN_POINT('Ctrl Pts',(20.8630027249507,0.551614161017511,-20.)) ;
#51724 = CARTESIAN_POINT('Ctrl Pts',(20.8831226202743,0.123380410496852,-20.)) ;
#51725 = CARTESIAN_POINT('Ctrl Pts',(20.9033298789958,-0.306712790829077,
-20.)) ;
#51726 = CARTESIAN_POINT('Ctrl Pts',(20.9101332115589,-0.737612398604347,
-20.)) ;
#51727 = CARTESIAN_POINT('Ctrl Pts',(20.9036368555828,-1.16871241502824,-20.)) ;
#51728 = CARTESIAN_POINT('Ctrl Pts',(20.8971421869036,-1.59970046194614,-20.)) ;
#51729 = CARTESIAN_POINT('Ctrl Pts',(20.8773546977867,-2.03088935474534,-20.)) ;
#51730 = CARTESIAN_POINT('Ctrl Pts',(20.8443266935953,-2.4616711459039,-20.)) ;
#51731 = CARTESIAN_POINT('Ctrl Pts',(20.8299804328112,-2.64878835350629,-20.)) ;
#51732 = CARTESIAN_POINT('Ctrl Pts',(20.8131353688933,-2.83582867226119,-20.)) ;
#51733 = CARTESIAN_POINT('Ctrl Pts',(20.7937927667325,-3.02274173750564,-20.)) ;
#51734 = CARTESIAN_POINT('Ctrl Pts',(20.7887912971327,-3.07107236054491,-20.)) ;
#51735 = CARTESIAN_POINT('Ctrl Pts',(20.7836229540371,-3.11939285262655,-20.)) ;
#51736 = CARTESIAN_POINT('Ctrl Pts',(20.7782901354159,-3.16768221580796,-20.)) ;
#51737 = CARTESIAN_POINT('Ctrl Pts',(20.7307766888087,-3.59792262753397,-20.)) ;
#51738 = CARTESIAN_POINT('Ctrl Pts',(20.670167860427,-4.02611636531182,-20.)) ;
#51739 = CARTESIAN_POINT('Ctrl Pts',(20.5966777225206,-4.45165660389502,-20.)) ;
#51740 = CARTESIAN_POINT('Ctrl Pts',(20.5223305323676,-4.88215955214073,-20.)) ;
#51741 = CARTESIAN_POINT('Ctrl Pts',(20.4347998671604,-5.30994727220065,-20.)) ;
#51742 = CARTESIAN_POINT('Ctrl Pts',(20.3342547042927,-5.73439911854882,-20.)) ;
#51743 = CARTESIAN_POINT('Ctrl Pts',(20.2335254061709,-6.15962829268022,-20.)) ;
#51744 = CARTESIAN_POINT('Ctrl Pts',(20.1197338520914,-6.58150991347884,-20.)) ;
#51745 = CARTESIAN_POINT('Ctrl Pts',(19.9929976115934,-6.99941944689774,-20.)) ;
#51746 = CARTESIAN_POINT('Ctrl Pts',(19.8668278005729,-7.41546119350469,-20.)) ;
#51747 = CARTESIAN_POINT('Ctrl Pts',(19.7278286613732,-7.82756681794848,-20.)) ;
#51748 = CARTESIAN_POINT('Ctrl Pts',(19.5760654853802,-8.23511151272187,-20.)) ;
#51749 = CARTESIAN_POINT('Ctrl Pts',(19.5021725166428,-8.43354362375884,-20.)) ;
#51750 = CARTESIAN_POINT('Ctrl Pts',(19.4252528423934,-8.63089430266909,-20.)) ;
#51751 = CARTESIAN_POINT('Ctrl Pts',(19.3453097129688,-8.82709009854958,-20.)) ;
#51752 = CARTESIAN_POINT('Ctrl Pts',(19.180732696096,-9.2309937115481,-20.)) ;
#51753 = CARTESIAN_POINT('Ctrl Pts',(19.0033447592909,-9.6300043076582,-20.)) ;
#51754 = CARTESIAN_POINT('Ctrl Pts',(18.8135117710249,-10.023630445027,-20.)) ;
#51755 = CARTESIAN_POINT('Ctrl Pts',(18.6803892841659,-10.2996651362462,-20.)) ;
#51756 = CARTESIAN_POINT('Ctrl Pts',(18.5411457110759,-10.5730515120463,-20.0000000000001)) ;
#51757 = CARTESIAN_POINT('Ctrl Pts',(18.3958940868607,-10.843612277219,-20.)) ;
#51758 = CARTESIAN_POINT('Ctrl Pts',(18.376401160023,-10.8799218278293,-20.)) ;
#51759 = CARTESIAN_POINT('Ctrl Pts',(18.3567991230378,-10.9161820673089,-20.)) ;
#51760 = CARTESIAN_POINT('Ctrl Pts',(18.3370964703204,-10.9523775690894,-20.)) ;
#51761 = CARTESIAN_POINT('Ctrl Pts',(18.1288264545511,-11.3349878619637,-20.)) ;
#51762 = CARTESIAN_POINT('Ctrl Pts',(17.9091288638351,-11.7107205413323,-20.)) ;
#51763 = CARTESIAN_POINT('Ctrl Pts',(17.6785011392334,-12.0791488707737,-20.)) ;
#51764 = CARTESIAN_POINT('Ctrl Pts',(17.4454005262735,-12.4515276451508,-20.)) ;
#51765 = CARTESIAN_POINT('Ctrl Pts',(17.2011339150899,-12.8164450377157,-20.)) ;
#51766 = CARTESIAN_POINT('Ctrl Pts',(16.9461630841213,-13.1734471994973,-20.)) ;
#51767 = CARTESIAN_POINT('Ctrl Pts',(16.6895009605379,-13.5328174561601,-20.)) ;
#51768 = CARTESIAN_POINT('Ctrl Pts',(16.4219918820727,-13.8841675923275,-20.)) ;
#51769 = CARTESIAN_POINT('Ctrl Pts',(16.1440582308894,-14.227014410769,-20.)) ;
#51770 = CARTESIAN_POINT('Ctrl Pts',(15.8659290427536,-14.5701024350588,-20.)) ;
#51771 = CARTESIAN_POINT('Ctrl Pts',(15.5773603059104,-14.9046756305149,-20.)) ;
#51772 = CARTESIAN_POINT('Ctrl Pts',(15.2787310149449,-15.2302226371145,-20.)) ;
#51773 = CARTESIAN_POINT('Ctrl Pts',(14.9815081945709,-15.5542363972954,-20.)) ;
#51774 = CARTESIAN_POINT('Ctrl Pts',(14.6743190319459,-15.8693092199902,-20.)) ;
#51775 = CARTESIAN_POINT('Ctrl Pts',(14.3574981339932,-16.1749034673177,-20.)) ;
#51776 = CARTESIAN_POINT('Ctrl Pts',(14.0446734403697,-16.4766431171044,-20.)) ;
#51777 = CARTESIAN_POINT('Ctrl Pts',(13.722458104397,-16.7691421598843,-20.)) ;
#51778 = CARTESIAN_POINT('Ctrl Pts',(13.3911412031311,-17.051844554609,-20.)) ;
#51779 = CARTESIAN_POINT('Ctrl Pts',(13.2887762376605,-17.1391893920256,-20.)) ;
#51780 = CARTESIAN_POINT('Ctrl Pts',(13.1855422289172,-17.2255987530988,-20.)) ;
#51781 = CARTESIAN_POINT('Ctrl Pts',(13.0814471333101,-17.3110553987592,-20.)) ;
#51782 = CARTESIAN_POINT('Ctrl Pts',(13.048030312067,-17.3384888665457,-20.)) ;
#51783 = CARTESIAN_POINT('Ctrl Pts',(13.0145317665027,-17.3658183827095,-20.)) ;
#51784 = CARTESIAN_POINT('Ctrl Pts',(12.9809537152124,-17.3930425047458,-20.)) ;
#51785 = CARTESIAN_POINT('Ctrl Pts',(12.6331656762335,-17.6750190832576,-20.)) ;
#51786 = CARTESIAN_POINT('Ctrl Pts',(12.2767956567509,-17.9457381705363,-20.)) ;
#51787 = CARTESIAN_POINT('Ctrl Pts',(11.9125033775857,-18.2050396015228,-20.)) ;
#51788 = CARTESIAN_POINT('Ctrl Pts',(11.5503007497329,-18.4628536291067,-20.)) ;
#51789 = CARTESIAN_POINT('Ctrl Pts',(11.1802659791631,-18.7093808135623,-20.)) ;
#51790 = CARTESIAN_POINT('Ctrl Pts',(10.8030080891504,-18.9444265203506,-20.)) ;
#51791 = CARTESIAN_POINT('Ctrl Pts',(10.4239904271859,-19.1805686305624,-20.)) ;
#51792 = CARTESIAN_POINT('Ctrl Pts',(10.037681655143,-19.4051221766271,-20.)) ;
#51793 = CARTESIAN_POINT('Ctrl Pts',(9.64466654416206,-19.6178484363144,-20.)) ;
#51794 = CARTESIAN_POINT('Ctrl Pts',(9.39842589258477,-19.75113046881,-20.)) ;
#51795 = CARTESIAN_POINT('Ctrl Pts',(9.14955200279447,-19.8797687995387,-20.)) ;
#51796 = CARTESIAN_POINT('Ctrl Pts',(8.89818338640667,-20.0036957576717,-19.9999999999999)) ;
#51797 = CARTESIAN_POINT('Ctrl Pts',(8.81183420772632,-20.0462666688893,-19.9999999999999)) ;
#51798 = CARTESIAN_POINT('Ctrl Pts',(8.72519061167969,-20.088281560275,-19.9999999999999)) ;
#51799 = CARTESIAN_POINT('Ctrl Pts',(8.63825811992194,-20.1297374908914,-20.)) ;
#51800 = CARTESIAN_POINT('Ctrl Pts',(8.56437314507967,-20.1649713870874,-20.)) ;
#51801 = CARTESIAN_POINT('Ctrl Pts',(8.49027196637771,-20.1998049273805,-20.)) ;
#51802 = CARTESIAN_POINT('Ctrl Pts',(8.41599661777268,-20.2342185484354,-20.)) ;
#51803 = CARTESIAN_POINT('Ctrl Pts',(8.00723515078845,-20.4236079285037,-20.)) ;
#51804 = CARTESIAN_POINT('Ctrl Pts',(7.59304737752386,-20.600359290717,-20.)) ;
#51805 = CARTESIAN_POINT('Ctrl Pts',(7.17405350980231,-20.7642755093381,-20.)) ;
#51806 = CARTESIAN_POINT('Ctrl Pts',(6.7543491679915,-20.9284696752876,-20.)) ;
#51807 = CARTESIAN_POINT('Ctrl Pts',(6.32982193923238,-21.0797853877173,-20.)) ;
#51808 = CARTESIAN_POINT('Ctrl Pts',(5.90106642836833,-21.2179806890933,-20.)) ;
#51809 = CARTESIAN_POINT('Ctrl Pts',(5.4746446821956,-21.355423777829,-20.)) ;
#51810 = CARTESIAN_POINT('Ctrl Pts',(5.04404006112706,-21.4798891022081,-20.)) ;
#51811 = CARTESIAN_POINT('Ctrl Pts',(4.6098164331882,-21.591091970763,-20.)) ;
#51812 = CARTESIAN_POINT('Ctrl Pts',(4.18999697364085,-21.6986059915877,-20.)) ;
#51813 = CARTESIAN_POINT('Ctrl Pts',(3.76679413188183,-21.7937228229268,-20.)) ;
#51814 = CARTESIAN_POINT('Ctrl Pts',(3.34070509846234,-21.8761405304411,-20.)) ;
#51815 = CARTESIAN_POINT('Ctrl Pts',(16.4056275812262,12.0157134421436,-20.)) ;
#51816 = CARTESIAN_POINT('Ctrl Pts',(16.4100629678363,12.0096575969161,-20.000095236561)) ;
#51817 = CARTESIAN_POINT('Ctrl Pts',(16.414495001335,12.0035992958223,-20.0001904731219)) ;
#51818 = CARTESIAN_POINT('Ctrl Pts',(16.4189236790046,11.9975385425771,-20.0002857096829)) ;
#51819 = CARTESIAN_POINT('Origin',(0.,20.065,-20.)) ;
#51820 = CARTESIAN_POINT('',(-2.45725380248917E-15,-20.065,-20.)) ;
#51821 = CARTESIAN_POINT('Origin',(0.,0.,-20.)) ;
#51822 = CARTESIAN_POINT('Origin',(5.00000000000251,14.8,-258.5)) ;
#51823 = CARTESIAN_POINT('',(5.00000000000251,14.8,-303.5)) ;
#51824 = CARTESIAN_POINT('',(5.00000000000251,14.8,-303.5)) ;
#51825 = CARTESIAN_POINT('',(5.00000000000251,14.8,-258.5)) ;
#51826 = CARTESIAN_POINT('',(5.00000000000251,14.8,-258.5)) ;
#51827 = CARTESIAN_POINT('',(5.00000000000251,14.8,-258.5)) ;
#51828 = CARTESIAN_POINT('Origin',(0.,14.8,-258.5)) ;
#51829 = CARTESIAN_POINT('',(-5.00000000000251,14.8,-258.5)) ;
#51830 = CARTESIAN_POINT('Origin',(0.,14.8,-258.5)) ;
#51831 = CARTESIAN_POINT('',(-5.00000000000251,14.8,-258.5)) ;
#51832 = CARTESIAN_POINT('Origin',(-5.00000000000251,14.8,-303.5)) ;
#51833 = CARTESIAN_POINT('',(-5.00000000000251,14.8,-303.5)) ;
#51834 = CARTESIAN_POINT('',(-5.00000000000251,14.8,-303.5)) ;
#51835 = CARTESIAN_POINT('',(-5.00000000000251,14.8,-303.5)) ;
#51836 = CARTESIAN_POINT('Origin',(0.,14.8,-303.5)) ;
#51837 = CARTESIAN_POINT('Origin',(0.,14.8,-303.5)) ;
#51838 = CARTESIAN_POINT('Origin',(0.,14.8,-281.)) ;
#51839 = CARTESIAN_POINT('Origin',(0.,0.,-22.)) ;
#51840 = CARTESIAN_POINT('',(-2.45725380248917E-15,-20.065,-24.)) ;
#51841 = CARTESIAN_POINT('Origin',(0.,0.,-24.)) ;
#51842 = CARTESIAN_POINT('',(-2.45725380248916E-15,-20.065,-22.)) ;
#51843 = CARTESIAN_POINT('Origin',(0.,23.,-24.)) ;
#51844 = CARTESIAN_POINT('',(-2.81668763803891E-15,-23.,-24.)) ;
#51845 = CARTESIAN_POINT('Origin',(0.,0.,-24.)) ;
#51846 = CARTESIAN_POINT('Origin',(0.,0.,-29.)) ;
#51847 = CARTESIAN_POINT('',(-2.81668763803891E-15,-23.,-29.)) ;
#51848 = CARTESIAN_POINT('Origin',(0.,0.,-42.87)) ;
#51849 = CARTESIAN_POINT('',(-2.45725380248916E-15,-20.065,-42.87)) ;
#51850 = CARTESIAN_POINT('Origin',(0.,0.,-72.)) ;
#51851 = CARTESIAN_POINT('',(-2.75545529808154E-15,-22.5,-88.)) ;
#51852 = CARTESIAN_POINT('Origin',(0.,0.,-88.)) ;
#51853 = CARTESIAN_POINT('',(-2.75545529808154E-15,-22.5,-72.)) ;
#51854 = CARTESIAN_POINT('Origin',(0.,22.25,-88.)) ;
#51855 = CARTESIAN_POINT('',(-2.72483912810286E-15,-22.25,-88.)) ;
#51856 = CARTESIAN_POINT('Origin',(0.,0.,-88.)) ;
#51857 = CARTESIAN_POINT('Origin',(0.,0.,-146.)) ;
#51858 = CARTESIAN_POINT('',(-2.72483912810286E-15,-22.25,-204.)) ;
#51859 = CARTESIAN_POINT('Origin',(0.,0.,-204.)) ;
#51860 = CARTESIAN_POINT('',(-2.72483912810286E-15,-22.25,-146.)) ;
#51861 = CARTESIAN_POINT('Origin',(0.,22.5,-204.)) ;
#51862 = CARTESIAN_POINT('Origin',(0.,0.,-317.125)) ;
#51863 = CARTESIAN_POINT('',(-2.20436423846523E-15,-18.,-318.25)) ;
#51864 = CARTESIAN_POINT('Origin',(0.,0.,-318.25)) ;
#51865 = CARTESIAN_POINT('',(-2.20436423846524E-15,-18.,-317.125)) ;
#51866 = CARTESIAN_POINT('Origin',(0.,19.5,-318.25)) ;
#51867 = CARTESIAN_POINT('',(0.,0.,0.)) ;
#51868 = CARTESIAN_POINT('Origin',(5.,5.,8.)) ;
#51869 = CARTESIAN_POINT('',(2.82055052822966,9.5,0.)) ;
#51870 = CARTESIAN_POINT('',(2.82055052822966,0.5,0.)) ;
#51871 = CARTESIAN_POINT('Origin',(5.,5.,0.)) ;
#51872 = CARTESIAN_POINT('',(5.,0.,0.500000000000001)) ;
#51873 = CARTESIAN_POINT('Origin',(5.,5.,-4.5)) ;
#51874 = CARTESIAN_POINT('',(5.,0.,7.5)) ;
#51875 = CARTESIAN_POINT('',(5.,-8.67361737988404E-16,8.)) ;
#51876 = CARTESIAN_POINT('',(2.82055052822966,0.5,8.)) ;
#51877 = CARTESIAN_POINT('Origin',(5.,5.,12.5)) ;
#51878 = CARTESIAN_POINT('',(2.82055052822966,9.5,8.)) ;
#51879 = CARTESIAN_POINT('Origin',(5.,5.,8.)) ;
#51880 = CARTESIAN_POINT('',(5.,10.,7.5)) ;
#51881 = CARTESIAN_POINT('Origin',(5.,5.,12.5)) ;
#51882 = CARTESIAN_POINT('',(5.,10.,0.5)) ;
#51883 = CARTESIAN_POINT('',(5.,10.,8.)) ;
#51884 = CARTESIAN_POINT('Origin',(5.,5.,-4.5)) ;
#51885 = CARTESIAN_POINT('Origin',(5.,0.,8.)) ;
#51886 = CARTESIAN_POINT('',(50.,0.,0.500000000000001)) ;
#51887 = CARTESIAN_POINT('',(55.,0.,0.500000000000001)) ;
#51888 = CARTESIAN_POINT('',(50.,8.67361737988404E-16,7.5)) ;
#51889 = CARTESIAN_POINT('',(50.,0.,8.)) ;
#51890 = CARTESIAN_POINT('',(55.,0.,7.5)) ;
#51891 = CARTESIAN_POINT('Origin',(50.,5.00000000000001,8.)) ;
#51892 = CARTESIAN_POINT('',(50.,10.,7.5)) ;
#51893 = CARTESIAN_POINT('',(50.,10.,0.5)) ;
#51894 = CARTESIAN_POINT('',(50.,10.,8.)) ;
#51895 = CARTESIAN_POINT('',(52.1794494717703,9.5,8.)) ;
#51896 = CARTESIAN_POINT('Origin',(50.,5.00000000000001,12.5)) ;
#51897 = CARTESIAN_POINT('',(52.1794494717703,0.5,8.)) ;
#51898 = CARTESIAN_POINT('Origin',(50.,5.00000000000001,8.)) ;
#51899 = CARTESIAN_POINT('Origin',(50.,4.99999999999999,12.5)) ;
#51900 = CARTESIAN_POINT('',(52.1794494717703,0.5,0.)) ;
#51901 = CARTESIAN_POINT('Origin',(50.,4.99999999999999,-4.49999999999999)) ;
#51902 = CARTESIAN_POINT('',(52.1794494717703,9.5,0.)) ;
#51903 = CARTESIAN_POINT('Origin',(50.,5.00000000000001,0.)) ;
#51904 = CARTESIAN_POINT('Origin',(50.,5.00000000000001,-4.49999999999998)) ;
#51905 = CARTESIAN_POINT('Origin',(50.,10.,8.)) ;
#51906 = CARTESIAN_POINT('',(55.,10.,7.5)) ;
#51907 = CARTESIAN_POINT('',(55.,10.,0.5)) ;
#51908 = CARTESIAN_POINT('Origin',(5.,5.,8.)) ;
#51909 = CARTESIAN_POINT('',(5.,9.5,8.)) ;
#51910 = CARTESIAN_POINT('',(5.,0.5,8.)) ;
#51911 = CARTESIAN_POINT('Origin',(5.,5.,0.)) ;
#51912 = CARTESIAN_POINT('',(5.,9.5,0.)) ;
#51913 = CARTESIAN_POINT('',(5.,0.5,0.)) ;
#51914 = CARTESIAN_POINT('Origin',(55.,0.,0.5)) ;
#51915 = CARTESIAN_POINT('Origin',(55.,9.5,0.)) ;
#51916 = CARTESIAN_POINT('Origin',(55.,0.5,8.)) ;
#51917 = CARTESIAN_POINT('Origin',(55.,10.,7.5)) ;
#51918 = CARTESIAN_POINT('',(0.,0.,0.)) ;
#51919 = CARTESIAN_POINT('Origin',(0.,0.,0.1)) ;
#51920 = CARTESIAN_POINT('',(-27.,3.30654635769785E-15,0.2)) ;
#51921 = CARTESIAN_POINT('Origin',(0.,0.,0.2)) ;
#51922 = CARTESIAN_POINT('',(-26.8,-3.28205342171491E-15,0.)) ;
#51923 = CARTESIAN_POINT('',(-26.9,-3.29429988970638E-15,0.1)) ;
#51924 = CARTESIAN_POINT('Origin',(0.,0.,0.)) ;
#51925 = CARTESIAN_POINT('Origin',(0.,0.,0.)) ;
#51926 = CARTESIAN_POINT('',(-22.7,2.77994823406449E-15,0.)) ;
#51927 = CARTESIAN_POINT('Origin',(0.,0.,0.)) ;
#51928 = CARTESIAN_POINT('Origin',(0.,0.,0.)) ;
#51929 = CARTESIAN_POINT('',(-27.,-3.30654635769785E-15,12.8)) ;
#51930 = CARTESIAN_POINT('Origin',(0.,0.,12.8)) ;
#51931 = CARTESIAN_POINT('',(-27.,-3.30654635769785E-15,0.)) ;
#51932 = CARTESIAN_POINT('Origin',(0.,0.,0.1)) ;
#51933 = CARTESIAN_POINT('',(-22.5,-2.75545529808154E-15,0.2)) ;
#51934 = CARTESIAN_POINT('Origin',(0.,0.,0.2)) ;
#51935 = CARTESIAN_POINT('',(-22.6,2.76770176607302E-15,0.1)) ;
#51936 = CARTESIAN_POINT('Origin',(0.,0.,0.)) ;
#51937 = CARTESIAN_POINT('',(-22.5,2.75545529808154E-15,12.8)) ;
#51938 = CARTESIAN_POINT('',(-22.5,-2.75545529808154E-15,0.)) ;
#51939 = CARTESIAN_POINT('Origin',(0.,0.,12.8)) ;
#51940 = CARTESIAN_POINT('Origin',(0.,0.,12.9)) ;
#51941 = CARTESIAN_POINT('',(-26.8,3.28205342171491E-15,13.)) ;
#51942 = CARTESIAN_POINT('',(-26.9,3.29429988970638E-15,12.9)) ;
#51943 = CARTESIAN_POINT('Origin',(0.,0.,13.)) ;
#51944 = CARTESIAN_POINT('Origin',(0.,0.,13.)) ;
#51945 = CARTESIAN_POINT('',(-22.7,-2.77994823406449E-15,13.)) ;
#51946 = CARTESIAN_POINT('Origin',(0.,0.,13.)) ;
#51947 = CARTESIAN_POINT('Origin',(0.,0.,12.9)) ;
#51948 = CARTESIAN_POINT('',(-22.6,-2.76770176607302E-15,12.9)) ;
#51949 = CARTESIAN_POINT('',(0.,0.,0.)) ;
#51950 = CARTESIAN_POINT('Origin',(0.,24.5,5.)) ;
#51951 = CARTESIAN_POINT('',(0.,19.3649167310371,5.)) ;
#51952 = CARTESIAN_POINT('',(45.,19.3649167310371,5.)) ;
#51953 = CARTESIAN_POINT('',(45.,19.3649167310371,5.)) ;
#51954 = CARTESIAN_POINT('',(0.,24.5,5.)) ;
#51955 = CARTESIAN_POINT('',(0.,12.25,5.)) ;
#51956 = CARTESIAN_POINT('',(45.,24.5,5.)) ;
#51957 = CARTESIAN_POINT('',(0.,24.5,5.)) ;
#51958 = CARTESIAN_POINT('',(45.,31.,5.)) ;
#51959 = CARTESIAN_POINT('Origin',(0.,24.5,-5.)) ;
#51960 = CARTESIAN_POINT('',(0.,24.5,-5.)) ;
#51961 = CARTESIAN_POINT('',(0.,24.5,-2.5)) ;
#51962 = CARTESIAN_POINT('',(45.,24.5,-5.)) ;
#51963 = CARTESIAN_POINT('',(0.,24.5,-5.)) ;
#51964 = CARTESIAN_POINT('',(45.,24.5,-2.5)) ;
#51965 = CARTESIAN_POINT('Origin',(0.,14.5,-5.)) ;
#51966 = CARTESIAN_POINT('',(45.,19.3649167310371,-5.)) ;
#51967 = CARTESIAN_POINT('',(0.,19.3649167310371,-5.)) ;
#51968 = CARTESIAN_POINT('',(45.,19.3649167310371,-5.)) ;
#51969 = CARTESIAN_POINT('',(45.,26.,-5.)) ;
#51970 = CARTESIAN_POINT('',(0.,7.25,-5.)) ;
#51971 = CARTESIAN_POINT('Origin',(0.,0.,0.)) ;
#51972 = CARTESIAN_POINT('',(0.,-4.89858719658941E-15,40.)) ;
#51973 = CARTESIAN_POINT('Origin',(0.,0.,0.)) ;
#51974 = CARTESIAN_POINT('Origin',(0.,0.,0.)) ;
#51975 = CARTESIAN_POINT('Origin',(45.,0.,0.)) ;
#51976 = CARTESIAN_POINT('',(30.5,46.5121833407376,7.8801919949714)) ;
#51977 = CARTESIAN_POINT('',(2.5,46.5121833407376,7.8801919949714)) ;
#51978 = CARTESIAN_POINT('',(30.5,46.5121833407376,7.8801919949714)) ;
#51979 = CARTESIAN_POINT('',(30.5,46.670828298707,6.87854715129665)) ;
#51980 = CARTESIAN_POINT('Origin',(30.5,0.,0.)) ;
#51981 = CARTESIAN_POINT('',(2.5,46.6708282987069,6.87854715129677)) ;
#51982 = CARTESIAN_POINT('',(30.5,46.6708282987069,6.87854715129677)) ;
#51983 = CARTESIAN_POINT('Origin',(2.49999999999999,0.,0.)) ;
#51984 = CARTESIAN_POINT('Origin',(45.,0.,0.)) ;
#51985 = CARTESIAN_POINT('',(30.5,45.6961566547982,11.7192957117799)) ;
#51986 = CARTESIAN_POINT('',(30.5,45.4336803742586,12.6988705265355)) ;
#51987 = CARTESIAN_POINT('Origin',(30.5,0.,0.)) ;
#51988 = CARTESIAN_POINT('',(2.5,45.6961566547981,11.71929571178)) ;
#51989 = CARTESIAN_POINT('',(30.5,45.6961566547981,11.71929571178)) ;
#51990 = CARTESIAN_POINT('',(2.5,45.4336803742586,12.6988705265355)) ;
#51991 = CARTESIAN_POINT('Origin',(2.49999999999999,0.,0.)) ;
#51992 = CARTESIAN_POINT('',(30.5,45.4336803742586,12.6988705265355)) ;
#51993 = CARTESIAN_POINT('Origin',(45.,0.,0.)) ;
#51994 = CARTESIAN_POINT('',(30.5,44.2208283560439,16.4316452160247)) ;
#51995 = CARTESIAN_POINT('',(30.5,43.8573964979903,17.3784175752014)) ;
#51996 = CARTESIAN_POINT('Origin',(30.5,0.,0.)) ;
#51997 = CARTESIAN_POINT('',(2.5,44.2208283560438,16.4316452160248)) ;
#51998 = CARTESIAN_POINT('',(30.5,44.2208283560438,16.4316452160248)) ;
#51999 = CARTESIAN_POINT('',(2.5,43.8573964979903,17.3784175752014)) ;
#52000 = CARTESIAN_POINT('Origin',(2.49999999999999,0.,0.)) ;
#52001 = CARTESIAN_POINT('',(30.5,43.8573964979903,17.3784175752014)) ;
#52002 = CARTESIAN_POINT('Origin',(45.,0.,0.)) ;
#52003 = CARTESIAN_POINT('',(30.5,42.2610074080175,20.9639661767398)) ;
#52004 = CARTESIAN_POINT('',(30.5,41.8006018079398,21.8675630442457)) ;
#52005 = CARTESIAN_POINT('Origin',(30.5,0.,0.)) ;
#52006 = CARTESIAN_POINT('',(2.5,42.2610074080174,20.9639661767399)) ;
#52007 = CARTESIAN_POINT('',(30.5,42.2610074080174,20.9639661767399)) ;
#52008 = CARTESIAN_POINT('',(2.5,41.8006018079398,21.8675630442457)) ;
#52009 = CARTESIAN_POINT('Origin',(2.49999999999999,0.,0.)) ;
#52010 = CARTESIAN_POINT('',(30.5,41.8006018079398,21.8675630442457)) ;
#52011 = CARTESIAN_POINT('Origin',(45.,0.,0.)) ;
#52012 = CARTESIAN_POINT('',(30.5,29.2924107235056,36.9788493466935)) ;
#52013 = CARTESIAN_POINT('',(2.5,29.2924107235056,36.9788493466935)) ;
#52014 = CARTESIAN_POINT('',(30.5,29.2924107235056,36.9788493466935)) ;
#52015 = CARTESIAN_POINT('',(30.5,30.0805381247129,36.3406363610723)) ;
#52016 = CARTESIAN_POINT('Origin',(30.5,0.,0.)) ;
#52017 = CARTESIAN_POINT('',(2.5,30.0805381247128,36.3406363610724)) ;
#52018 = CARTESIAN_POINT('',(30.5,30.0805381247128,36.3406363610724)) ;
#52019 = CARTESIAN_POINT('Origin',(2.49999999999999,0.,0.)) ;
#52020 = CARTESIAN_POINT('Origin',(45.,0.,0.)) ;
#52021 = CARTESIAN_POINT('',(30.5,32.9972861282627,33.7143846624785)) ;
#52022 = CARTESIAN_POINT('',(2.5,32.9972861282627,33.7143846624785)) ;
#52023 = CARTESIAN_POINT('',(30.5,32.9972861282627,33.7143846624785)) ;
#52024 = CARTESIAN_POINT('',(30.5,33.7143846624786,32.9972861282625)) ;
#52025 = CARTESIAN_POINT('Origin',(30.5,0.,0.)) ;
#52026 = CARTESIAN_POINT('',(2.5,33.7143846624785,32.9972861282626)) ;
#52027 = CARTESIAN_POINT('',(30.5,33.7143846624785,32.9972861282626)) ;
#52028 = CARTESIAN_POINT('Origin',(2.49999999999999,0.,0.)) ;
#52029 = CARTESIAN_POINT('Origin',(45.,0.,0.)) ;
#52030 = CARTESIAN_POINT('',(30.5,36.3406363610724,30.0805381247128)) ;
#52031 = CARTESIAN_POINT('',(2.5,36.3406363610724,30.0805381247128)) ;
#52032 = CARTESIAN_POINT('',(30.5,36.3406363610724,30.0805381247128)) ;
#52033 = CARTESIAN_POINT('',(30.5,36.9788493466936,29.2924107235055)) ;
#52034 = CARTESIAN_POINT('Origin',(30.5,0.,0.)) ;
#52035 = CARTESIAN_POINT('',(2.5,36.9788493466935,29.2924107235055)) ;
#52036 = CARTESIAN_POINT('',(30.5,36.9788493466935,29.2924107235055)) ;
#52037 = CARTESIAN_POINT('Origin',(2.49999999999999,0.,0.)) ;
#52038 = CARTESIAN_POINT('Origin',(45.,0.,0.)) ;
#52039 = CARTESIAN_POINT('',(30.5,39.8381660191445,25.2666015370306)) ;
#52040 = CARTESIAN_POINT('',(30.5,39.2858309771432,26.1171229164955)) ;
#52041 = CARTESIAN_POINT('Origin',(30.5,0.,0.)) ;
#52042 = CARTESIAN_POINT('',(2.5,39.8381660191444,25.2666015370307)) ;
#52043 = CARTESIAN_POINT('',(30.5,39.8381660191444,25.2666015370307)) ;
#52044 = CARTESIAN_POINT('',(2.5,39.2858309771432,26.1171229164955)) ;
#52045 = CARTESIAN_POINT('Origin',(2.49999999999999,0.,0.)) ;
#52046 = CARTESIAN_POINT('',(30.5,39.2858309771432,26.1171229164955)) ;
#52047 = CARTESIAN_POINT('Origin',(45.,0.,0.)) ;
#52048 = CARTESIAN_POINT('',(30.5,26.1171229164956,39.2858309771432)) ;
#52049 = CARTESIAN_POINT('',(30.5,25.2666015370307,39.8381660191445)) ;
#52050 = CARTESIAN_POINT('Origin',(30.5,0.,0.)) ;
#52051 = CARTESIAN_POINT('',(2.5,26.1171229164954,39.2858309771432)) ;
#52052 = CARTESIAN_POINT('',(30.5,26.1171229164954,39.2858309771432)) ;
#52053 = CARTESIAN_POINT('',(2.5,25.2666015370307,39.8381660191445)) ;
#52054 = CARTESIAN_POINT('Origin',(2.49999999999999,0.,0.)) ;
#52055 = CARTESIAN_POINT('',(30.5,25.2666015370307,39.8381660191445)) ;
#52056 = CARTESIAN_POINT('Origin',(45.,0.,0.)) ;
#52057 = CARTESIAN_POINT('',(30.5,21.8675630442458,41.8006018079397)) ;
#52058 = CARTESIAN_POINT('',(30.5,20.9639661767399,42.2610074080174)) ;
#52059 = CARTESIAN_POINT('Origin',(30.5,0.,0.)) ;
#52060 = CARTESIAN_POINT('',(2.5,21.8675630442456,41.8006018079398)) ;
#52061 = CARTESIAN_POINT('',(30.5,21.8675630442456,41.8006018079398)) ;
#52062 = CARTESIAN_POINT('',(2.5,20.9639661767399,42.2610074080174)) ;
#52063 = CARTESIAN_POINT('Origin',(2.49999999999999,0.,0.)) ;
#52064 = CARTESIAN_POINT('',(30.5,20.9639661767399,42.2610074080174)) ;
#52065 = CARTESIAN_POINT('Origin',(45.,0.,0.)) ;
#52066 = CARTESIAN_POINT('',(30.5,17.3784175752015,43.8573964979902)) ;
#52067 = CARTESIAN_POINT('',(30.5,16.4316452160248,44.2208283560438)) ;
#52068 = CARTESIAN_POINT('Origin',(30.5,0.,0.)) ;
#52069 = CARTESIAN_POINT('',(2.5,17.3784175752014,43.8573964979902)) ;
#52070 = CARTESIAN_POINT('',(30.5,17.3784175752014,43.8573964979902)) ;
#52071 = CARTESIAN_POINT('',(2.5,16.4316452160248,44.2208283560438)) ;
#52072 = CARTESIAN_POINT('Origin',(2.49999999999999,0.,0.)) ;
#52073 = CARTESIAN_POINT('',(30.5,16.4316452160248,44.2208283560438)) ;
#52074 = CARTESIAN_POINT('Origin',(45.,0.,0.)) ;
#52075 = CARTESIAN_POINT('',(30.5,12.6988705265356,45.4336803742585)) ;
#52076 = CARTESIAN_POINT('',(30.5,11.7192957117801,45.6961566547981)) ;
#52077 = CARTESIAN_POINT('Origin',(30.5,0.,0.)) ;
#52078 = CARTESIAN_POINT('',(2.5,12.6988705265355,45.4336803742585)) ;
#52079 = CARTESIAN_POINT('',(30.5,12.6988705265355,45.4336803742585)) ;
#52080 = CARTESIAN_POINT('',(2.5,11.7192957117801,45.6961566547981)) ;
#52081 = CARTESIAN_POINT('Origin',(2.49999999999999,0.,0.)) ;
#52082 = CARTESIAN_POINT('',(30.5,11.7192957117801,45.6961566547981)) ;
#52083 = CARTESIAN_POINT('Origin',(45.,0.,0.)) ;
#52084 = CARTESIAN_POINT('',(30.5,7.88019199497154,46.5121833407376)) ;
#52085 = CARTESIAN_POINT('',(30.5,6.87854715129677,46.670828298707)) ;
#52086 = CARTESIAN_POINT('Origin',(30.5,0.,0.)) ;
#52087 = CARTESIAN_POINT('',(2.5,7.8801919949714,46.5121833407375)) ;
#52088 = CARTESIAN_POINT('',(30.5,7.8801919949714,46.5121833407375)) ;
#52089 = CARTESIAN_POINT('',(2.5,6.87854715129677,46.670828298707)) ;
#52090 = CARTESIAN_POINT('Origin',(2.49999999999999,0.,0.)) ;
#52091 = CARTESIAN_POINT('',(30.5,6.87854715129677,46.670828298707)) ;
#52092 = CARTESIAN_POINT('Origin',(45.,0.,0.)) ;
#52093 = CARTESIAN_POINT('',(30.5,2.97517643087433,47.0810890932354)) ;
#52094 = CARTESIAN_POINT('',(30.5,1.96243578879535,47.1341645812764)) ;
#52095 = CARTESIAN_POINT('Origin',(30.5,0.,0.)) ;
#52096 = CARTESIAN_POINT('',(2.5,2.9751764308742,47.0810890932354)) ;
#52097 = CARTESIAN_POINT('',(30.5,2.9751764308742,47.0810890932354)) ;
#52098 = CARTESIAN_POINT('',(2.5,1.96243578879535,47.1341645812764)) ;
#52099 = CARTESIAN_POINT('Origin',(2.49999999999999,0.,0.)) ;
#52100 = CARTESIAN_POINT('',(30.5,1.96243578879535,47.1341645812764)) ;
#52101 = CARTESIAN_POINT('Origin',(45.,0.,0.)) ;
#52102 = CARTESIAN_POINT('',(30.5,-1.96243578879522,47.1341645812764)) ;
#52103 = CARTESIAN_POINT('',(30.5,-2.97517643087417,47.0810890932354)) ;
#52104 = CARTESIAN_POINT('Origin',(30.5,0.,0.)) ;
#52105 = CARTESIAN_POINT('',(2.5,-1.96243578879535,47.1341645812764)) ;
#52106 = CARTESIAN_POINT('',(30.5,-1.96243578879535,47.1341645812764)) ;
#52107 = CARTESIAN_POINT('',(2.5,-2.97517643087417,47.0810890932354)) ;
#52108 = CARTESIAN_POINT('Origin',(2.49999999999999,0.,0.)) ;
#52109 = CARTESIAN_POINT('',(30.5,-2.97517643087417,47.0810890932354)) ;
#52110 = CARTESIAN_POINT('Origin',(45.,0.,0.)) ;
#52111 = CARTESIAN_POINT('',(30.5,-6.87854715129661,46.670828298707)) ;
#52112 = CARTESIAN_POINT('',(30.5,-7.88019199497139,46.5121833407376)) ;
#52113 = CARTESIAN_POINT('Origin',(30.5,0.,0.)) ;
#52114 = CARTESIAN_POINT('',(2.5,-6.87854715129673,46.6708282987069)) ;
#52115 = CARTESIAN_POINT('',(30.5,-6.87854715129673,46.6708282987069)) ;
#52116 = CARTESIAN_POINT('',(2.5,-7.88019199497139,46.5121833407376)) ;
#52117 = CARTESIAN_POINT('Origin',(2.49999999999999,0.,0.)) ;
#52118 = CARTESIAN_POINT('',(30.5,-7.88019199497139,46.5121833407376)) ;
#52119 = CARTESIAN_POINT('Origin',(45.,0.,0.)) ;
#52120 = CARTESIAN_POINT('',(30.5,-11.7192957117799,45.6961566547982)) ;
#52121 = CARTESIAN_POINT('',(30.5,-12.6988705265355,45.4336803742586)) ;
#52122 = CARTESIAN_POINT('Origin',(30.5,0.,0.)) ;
#52123 = CARTESIAN_POINT('',(2.5,-11.71929571178,45.6961566547981)) ;
#52124 = CARTESIAN_POINT('',(30.5,-11.71929571178,45.6961566547981)) ;
#52125 = CARTESIAN_POINT('',(2.5,-12.6988705265355,45.4336803742586)) ;
#52126 = CARTESIAN_POINT('Origin',(2.49999999999999,0.,0.)) ;
#52127 = CARTESIAN_POINT('',(30.5,-12.6988705265355,45.4336803742586)) ;
#52128 = CARTESIAN_POINT('Origin',(45.,0.,0.)) ;
#52129 = CARTESIAN_POINT('',(30.5,-16.4316452160246,44.2208283560439)) ;
#52130 = CARTESIAN_POINT('',(30.5,-17.3784175752014,43.8573964979903)) ;
#52131 = CARTESIAN_POINT('Origin',(30.5,0.,0.)) ;
#52132 = CARTESIAN_POINT('',(2.5,-16.4316452160247,44.2208283560438)) ;
#52133 = CARTESIAN_POINT('',(30.5,-16.4316452160247,44.2208283560438)) ;
#52134 = CARTESIAN_POINT('',(2.5,-17.3784175752014,43.8573964979903)) ;
#52135 = CARTESIAN_POINT('Origin',(2.49999999999999,0.,0.)) ;
#52136 = CARTESIAN_POINT('',(30.5,-17.3784175752014,43.8573964979903)) ;
#52137 = CARTESIAN_POINT('Origin',(45.,0.,0.)) ;
#52138 = CARTESIAN_POINT('',(30.5,-20.9639661767398,42.2610074080175)) ;
#52139 = CARTESIAN_POINT('',(30.5,-21.8675630442457,41.8006018079398)) ;
#52140 = CARTESIAN_POINT('Origin',(30.5,0.,0.)) ;
#52141 = CARTESIAN_POINT('',(2.5,-20.9639661767399,42.2610074080174)) ;
#52142 = CARTESIAN_POINT('',(30.5,-20.9639661767399,42.2610074080174)) ;
#52143 = CARTESIAN_POINT('',(2.5,-21.8675630442457,41.8006018079398)) ;
#52144 = CARTESIAN_POINT('Origin',(2.49999999999999,0.,0.)) ;
#52145 = CARTESIAN_POINT('',(30.5,-21.8675630442457,41.8006018079398)) ;
#52146 = CARTESIAN_POINT('Origin',(45.,0.,0.)) ;
#52147 = CARTESIAN_POINT('',(30.5,-25.2666015370306,39.8381660191445)) ;
#52148 = CARTESIAN_POINT('',(30.5,-26.1171229164955,39.2858309771432)) ;
#52149 = CARTESIAN_POINT('Origin',(30.5,0.,0.)) ;
#52150 = CARTESIAN_POINT('',(2.5,-25.2666015370307,39.8381660191444)) ;
#52151 = CARTESIAN_POINT('',(30.5,-25.2666015370307,39.8381660191444)) ;
#52152 = CARTESIAN_POINT('',(2.5,-26.1171229164955,39.2858309771432)) ;
#52153 = CARTESIAN_POINT('Origin',(2.49999999999999,0.,0.)) ;
#52154 = CARTESIAN_POINT('',(30.5,-26.1171229164955,39.2858309771432)) ;
#52155 = CARTESIAN_POINT('Origin',(45.,0.,0.)) ;
#52156 = CARTESIAN_POINT('',(30.5,-33.7143846624785,32.9972861282626)) ;
#52157 = CARTESIAN_POINT('',(2.5,-33.7143846624785,32.9972861282626)) ;
#52158 = CARTESIAN_POINT('',(30.5,-33.7143846624785,32.9972861282626)) ;
#52159 = CARTESIAN_POINT('',(30.5,-32.9972861282625,33.7143846624786)) ;
#52160 = CARTESIAN_POINT('Origin',(30.5,0.,0.)) ;
#52161 = CARTESIAN_POINT('',(2.5,-32.9972861282626,33.7143846624785)) ;
#52162 = CARTESIAN_POINT('',(30.5,-32.9972861282626,33.7143846624785)) ;
#52163 = CARTESIAN_POINT('Origin',(2.49999999999999,0.,0.)) ;
#52164 = CARTESIAN_POINT('Origin',(45.,0.,0.)) ;
#52165 = CARTESIAN_POINT('',(30.5,-29.2924107235054,36.9788493466936)) ;
#52166 = CARTESIAN_POINT('',(30.5,-30.0805381247128,36.3406363610724)) ;
#52167 = CARTESIAN_POINT('Origin',(30.5,0.,0.)) ;
#52168 = CARTESIAN_POINT('',(2.5,-29.2924107235055,36.9788493466935)) ;
#52169 = CARTESIAN_POINT('',(30.5,-29.2924107235055,36.9788493466935)) ;
#52170 = CARTESIAN_POINT('',(2.5,-30.0805381247128,36.3406363610724)) ;
#52171 = CARTESIAN_POINT('Origin',(2.49999999999999,0.,0.)) ;
#52172 = CARTESIAN_POINT('',(30.5,-30.0805381247128,36.3406363610724)) ;
#52173 = CARTESIAN_POINT('Origin',(45.,0.,0.)) ;
#52174 = CARTESIAN_POINT('',(30.5,-36.3406363610723,30.0805381247129)) ;
#52175 = CARTESIAN_POINT('',(30.5,-36.9788493466935,29.2924107235056)) ;
#52176 = CARTESIAN_POINT('Origin',(30.5,0.,0.)) ;
#52177 = CARTESIAN_POINT('',(2.5,-36.3406363610724,30.0805381247128)) ;
#52178 = CARTESIAN_POINT('',(30.5,-36.3406363610724,30.0805381247128)) ;
#52179 = CARTESIAN_POINT('',(2.5,-36.9788493466935,29.2924107235056)) ;
#52180 = CARTESIAN_POINT('Origin',(2.49999999999999,0.,0.)) ;
#52181 = CARTESIAN_POINT('',(30.5,-36.9788493466935,29.2924107235056)) ;
#52182 = CARTESIAN_POINT('Origin',(45.,0.,0.)) ;
#52183 = CARTESIAN_POINT('',(30.5,-39.2858309771431,26.1171229164956)) ;
#52184 = CARTESIAN_POINT('',(30.5,-39.8381660191444,25.2666015370307)) ;
#52185 = CARTESIAN_POINT('Origin',(30.5,0.,0.)) ;
#52186 = CARTESIAN_POINT('',(2.5,-39.2858309771432,26.1171229164955)) ;
#52187 = CARTESIAN_POINT('',(30.5,-39.2858309771432,26.1171229164955)) ;
#52188 = CARTESIAN_POINT('',(2.5,-39.8381660191444,25.2666015370307)) ;
#52189 = CARTESIAN_POINT('Origin',(2.49999999999999,0.,0.)) ;
#52190 = CARTESIAN_POINT('',(30.5,-39.8381660191444,25.2666015370307)) ;
#52191 = CARTESIAN_POINT('Origin',(45.,0.,0.)) ;
#52192 = CARTESIAN_POINT('',(30.5,-41.8006018079397,21.8675630442458)) ;
#52193 = CARTESIAN_POINT('',(30.5,-42.2610074080174,20.9639661767399)) ;
#52194 = CARTESIAN_POINT('Origin',(30.5,0.,0.)) ;
#52195 = CARTESIAN_POINT('',(2.5,-41.8006018079397,21.8675630442457)) ;
#52196 = CARTESIAN_POINT('',(30.5,-41.8006018079397,21.8675630442457)) ;
#52197 = CARTESIAN_POINT('',(2.5,-42.2610074080174,20.9639661767399)) ;
#52198 = CARTESIAN_POINT('Origin',(2.49999999999999,0.,0.)) ;
#52199 = CARTESIAN_POINT('',(30.5,-42.2610074080174,20.9639661767399)) ;
#52200 = CARTESIAN_POINT('Origin',(45.,0.,0.)) ;
#52201 = CARTESIAN_POINT('',(30.5,-43.8573964979902,17.3784175752015)) ;
#52202 = CARTESIAN_POINT('',(30.5,-44.2208283560438,16.4316452160248)) ;
#52203 = CARTESIAN_POINT('Origin',(30.5,0.,0.)) ;
#52204 = CARTESIAN_POINT('',(2.5,-43.8573964979902,17.3784175752014)) ;
#52205 = CARTESIAN_POINT('',(30.5,-43.8573964979902,17.3784175752014)) ;
#52206 = CARTESIAN_POINT('',(2.5,-44.2208283560438,16.4316452160248)) ;
#52207 = CARTESIAN_POINT('Origin',(2.49999999999999,0.,0.)) ;
#52208 = CARTESIAN_POINT('',(30.5,-44.2208283560438,16.4316452160248)) ;
#52209 = CARTESIAN_POINT('Origin',(45.,0.,0.)) ;
#52210 = CARTESIAN_POINT('',(30.5,-45.4336803742585,12.6988705265356)) ;
#52211 = CARTESIAN_POINT('',(30.5,-45.6961566547981,11.7192957117801)) ;
#52212 = CARTESIAN_POINT('Origin',(30.5,0.,0.)) ;
#52213 = CARTESIAN_POINT('',(2.5,-45.4336803742585,12.6988705265355)) ;
#52214 = CARTESIAN_POINT('',(30.5,-45.4336803742585,12.6988705265355)) ;
#52215 = CARTESIAN_POINT('',(2.5,-45.6961566547981,11.7192957117801)) ;
#52216 = CARTESIAN_POINT('Origin',(2.49999999999999,0.,0.)) ;
#52217 = CARTESIAN_POINT('',(30.5,-45.6961566547981,11.7192957117801)) ;
#52218 = CARTESIAN_POINT('Origin',(45.,0.,0.)) ;
#52219 = CARTESIAN_POINT('',(30.5,-46.5121833407376,7.88019199497153)) ;
#52220 = CARTESIAN_POINT('',(30.5,-46.670828298707,6.87854715129678)) ;
#52221 = CARTESIAN_POINT('Origin',(30.5,0.,0.)) ;
#52222 = CARTESIAN_POINT('',(2.5,-46.5121833407376,7.88019199497139)) ;
#52223 = CARTESIAN_POINT('',(30.5,-46.5121833407376,7.88019199497139)) ;
#52224 = CARTESIAN_POINT('',(2.5,-46.670828298707,6.87854715129678)) ;
#52225 = CARTESIAN_POINT('Origin',(2.49999999999999,0.,0.)) ;
#52226 = CARTESIAN_POINT('',(30.5,-46.670828298707,6.87854715129678)) ;
#52227 = CARTESIAN_POINT('Origin',(45.,0.,0.)) ;
#52228 = CARTESIAN_POINT('',(30.5,-47.0810890932354,2.97517643087434)) ;
#52229 = CARTESIAN_POINT('',(30.5,-47.1341645812764,1.96243578879536)) ;
#52230 = CARTESIAN_POINT('Origin',(30.5,0.,0.)) ;
#52231 = CARTESIAN_POINT('',(2.5,-47.0810890932354,2.97517643087421)) ;
#52232 = CARTESIAN_POINT('',(30.5,-47.0810890932354,2.97517643087421)) ;
#52233 = CARTESIAN_POINT('',(2.5,-47.1341645812764,1.96243578879536)) ;
#52234 = CARTESIAN_POINT('Origin',(2.49999999999999,0.,0.)) ;
#52235 = CARTESIAN_POINT('',(30.5,-47.1341645812764,1.96243578879536)) ;
#52236 = CARTESIAN_POINT('Origin',(45.,0.,0.)) ;
#52237 = CARTESIAN_POINT('',(30.5,-47.1341645812764,-1.96243578879522)) ;
#52238 = CARTESIAN_POINT('',(30.5,-47.0810890932354,-2.97517643087418)) ;
#52239 = CARTESIAN_POINT('Origin',(30.5,0.,0.)) ;
#52240 = CARTESIAN_POINT('',(2.5,-47.1341645812764,-1.96243578879534)) ;
#52241 = CARTESIAN_POINT('',(30.5,-47.1341645812764,-1.96243578879534)) ;
#52242 = CARTESIAN_POINT('',(2.5,-47.0810890932354,-2.97517643087418)) ;
#52243 = CARTESIAN_POINT('Origin',(2.49999999999999,0.,0.)) ;
#52244 = CARTESIAN_POINT('',(30.5,-47.0810890932354,-2.97517643087418)) ;
#52245 = CARTESIAN_POINT('Origin',(45.,0.,0.)) ;
#52246 = CARTESIAN_POINT('',(30.5,-46.670828298707,-6.87854715129663)) ;
#52247 = CARTESIAN_POINT('',(30.5,-46.5121833407376,-7.88019199497139)) ;
#52248 = CARTESIAN_POINT('Origin',(30.5,0.,0.)) ;
#52249 = CARTESIAN_POINT('',(2.5,-46.6708282987069,-6.87854715129675)) ;
#52250 = CARTESIAN_POINT('',(30.5,-46.6708282987069,-6.87854715129675)) ;
#52251 = CARTESIAN_POINT('',(2.5,-46.5121833407376,-7.88019199497139)) ;
#52252 = CARTESIAN_POINT('Origin',(2.49999999999999,0.,0.)) ;
#52253 = CARTESIAN_POINT('',(30.5,-46.5121833407376,-7.88019199497139)) ;
#52254 = CARTESIAN_POINT('Origin',(45.,0.,0.)) ;
#52255 = CARTESIAN_POINT('',(30.5,-45.6961566547982,-11.7192957117799)) ;
#52256 = CARTESIAN_POINT('',(30.5,-45.4336803742586,-12.6988705265355)) ;
#52257 = CARTESIAN_POINT('Origin',(30.5,0.,0.)) ;
#52258 = CARTESIAN_POINT('',(2.5,-45.6961566547981,-11.71929571178)) ;
#52259 = CARTESIAN_POINT('',(30.5,-45.6961566547981,-11.71929571178)) ;
#52260 = CARTESIAN_POINT('',(2.5,-45.4336803742586,-12.6988705265355)) ;
#52261 = CARTESIAN_POINT('Origin',(2.49999999999999,0.,0.)) ;
#52262 = CARTESIAN_POINT('',(30.5,-45.4336803742586,-12.6988705265355)) ;
#52263 = CARTESIAN_POINT('Origin',(45.,0.,0.)) ;
#52264 = CARTESIAN_POINT('',(30.5,-20.9639661767399,-42.2610074080174)) ;
#52265 = CARTESIAN_POINT('',(2.5,-20.9639661767399,-42.2610074080174)) ;
#52266 = CARTESIAN_POINT('',(30.5,-20.9639661767399,-42.2610074080174)) ;
#52267 = CARTESIAN_POINT('',(30.5,-21.8675630442458,-41.8006018079397)) ;
#52268 = CARTESIAN_POINT('Origin',(30.5,0.,0.)) ;
#52269 = CARTESIAN_POINT('',(2.5,-21.8675630442457,-41.8006018079397)) ;
#52270 = CARTESIAN_POINT('',(30.5,-21.8675630442457,-41.8006018079397)) ;
#52271 = CARTESIAN_POINT('Origin',(2.49999999999999,0.,0.)) ;
#52272 = CARTESIAN_POINT('Origin',(45.,0.,0.)) ;
#52273 = CARTESIAN_POINT('',(30.5,-25.2666015370308,-39.8381660191444)) ;
#52274 = CARTESIAN_POINT('',(2.5,-25.2666015370308,-39.8381660191444)) ;
#52275 = CARTESIAN_POINT('',(30.5,-25.2666015370308,-39.8381660191444)) ;
#52276 = CARTESIAN_POINT('',(30.5,-26.1171229164956,-39.2858309771431)) ;
#52277 = CARTESIAN_POINT('Origin',(30.5,0.,0.)) ;
#52278 = CARTESIAN_POINT('',(2.5,-26.1171229164955,-39.2858309771432)) ;
#52279 = CARTESIAN_POINT('',(30.5,-26.1171229164955,-39.2858309771432)) ;
#52280 = CARTESIAN_POINT('Origin',(2.49999999999999,0.,0.)) ;
#52281 = CARTESIAN_POINT('Origin',(45.,0.,0.)) ;
#52282 = CARTESIAN_POINT('',(30.5,-29.2924107235056,-36.9788493466935)) ;
#52283 = CARTESIAN_POINT('',(2.5,-29.2924107235056,-36.9788493466935)) ;
#52284 = CARTESIAN_POINT('',(30.5,-29.2924107235056,-36.9788493466935)) ;
#52285 = CARTESIAN_POINT('',(30.5,-30.0805381247129,-36.3406363610723)) ;
#52286 = CARTESIAN_POINT('Origin',(30.5,0.,0.)) ;
#52287 = CARTESIAN_POINT('',(2.5,-30.0805381247128,-36.3406363610724)) ;
#52288 = CARTESIAN_POINT('',(30.5,-30.0805381247128,-36.3406363610724)) ;
#52289 = CARTESIAN_POINT('Origin',(2.49999999999999,0.,0.)) ;
#52290 = CARTESIAN_POINT('Origin',(45.,0.,0.)) ;
#52291 = CARTESIAN_POINT('',(30.5,-32.9972861282627,-33.7143846624785)) ;
#52292 = CARTESIAN_POINT('',(2.5,-32.9972861282627,-33.7143846624785)) ;
#52293 = CARTESIAN_POINT('',(30.5,-32.9972861282627,-33.7143846624785)) ;
#52294 = CARTESIAN_POINT('',(30.5,-33.7143846624786,-32.9972861282625)) ;
#52295 = CARTESIAN_POINT('Origin',(30.5,0.,0.)) ;
#52296 = CARTESIAN_POINT('',(2.5,-33.7143846624785,-32.9972861282626)) ;
#52297 = CARTESIAN_POINT('',(30.5,-33.7143846624785,-32.9972861282626)) ;
#52298 = CARTESIAN_POINT('Origin',(2.49999999999999,0.,0.)) ;
#52299 = CARTESIAN_POINT('Origin',(45.,0.,0.)) ;
#52300 = CARTESIAN_POINT('',(30.5,-36.3406363610724,-30.0805381247128)) ;
#52301 = CARTESIAN_POINT('',(2.5,-36.3406363610724,-30.0805381247128)) ;
#52302 = CARTESIAN_POINT('',(30.5,-36.3406363610724,-30.0805381247128)) ;
#52303 = CARTESIAN_POINT('',(30.5,-36.9788493466936,-29.2924107235055)) ;
#52304 = CARTESIAN_POINT('Origin',(30.5,0.,0.)) ;
#52305 = CARTESIAN_POINT('',(2.5,-36.9788493466935,-29.2924107235055)) ;
#52306 = CARTESIAN_POINT('',(30.5,-36.9788493466935,-29.2924107235055)) ;
#52307 = CARTESIAN_POINT('Origin',(2.49999999999999,0.,0.)) ;
#52308 = CARTESIAN_POINT('Origin',(45.,0.,0.)) ;
#52309 = CARTESIAN_POINT('',(30.5,-39.2858309771432,-26.1171229164955)) ;
#52310 = CARTESIAN_POINT('',(2.5,-39.2858309771432,-26.1171229164955)) ;
#52311 = CARTESIAN_POINT('',(30.5,-39.2858309771432,-26.1171229164955)) ;
#52312 = CARTESIAN_POINT('',(30.5,-39.8381660191445,-25.2666015370306)) ;
#52313 = CARTESIAN_POINT('Origin',(30.5,0.,0.)) ;
#52314 = CARTESIAN_POINT('',(2.5,-39.8381660191444,-25.2666015370307)) ;
#52315 = CARTESIAN_POINT('',(30.5,-39.8381660191444,-25.2666015370307)) ;
#52316 = CARTESIAN_POINT('Origin',(2.49999999999999,0.,0.)) ;
#52317 = CARTESIAN_POINT('Origin',(45.,0.,0.)) ;
#52318 = CARTESIAN_POINT('',(30.5,-41.8006018079398,-21.8675630442457)) ;
#52319 = CARTESIAN_POINT('',(2.5,-41.8006018079398,-21.8675630442457)) ;
#52320 = CARTESIAN_POINT('',(30.5,-41.8006018079398,-21.8675630442457)) ;
#52321 = CARTESIAN_POINT('',(30.5,-42.2610074080175,-20.9639661767398)) ;
#52322 = CARTESIAN_POINT('Origin',(30.5,0.,0.)) ;
#52323 = CARTESIAN_POINT('',(2.5,-42.2610074080174,-20.9639661767399)) ;
#52324 = CARTESIAN_POINT('',(30.5,-42.2610074080174,-20.9639661767399)) ;
#52325 = CARTESIAN_POINT('Origin',(2.49999999999999,0.,0.)) ;
#52326 = CARTESIAN_POINT('Origin',(45.,0.,0.)) ;
#52327 = CARTESIAN_POINT('',(30.5,-44.2208283560439,-16.4316452160247)) ;
#52328 = CARTESIAN_POINT('',(30.5,-43.8573964979903,-17.3784175752014)) ;
#52329 = CARTESIAN_POINT('Origin',(30.5,0.,0.)) ;
#52330 = CARTESIAN_POINT('',(2.5,-44.2208283560438,-16.4316452160248)) ;
#52331 = CARTESIAN_POINT('',(30.5,-44.2208283560438,-16.4316452160248)) ;
#52332 = CARTESIAN_POINT('',(2.5,-43.8573964979903,-17.3784175752014)) ;
#52333 = CARTESIAN_POINT('Origin',(2.49999999999999,0.,0.)) ;
#52334 = CARTESIAN_POINT('',(30.5,-43.8573964979903,-17.3784175752014)) ;
#52335 = CARTESIAN_POINT('Origin',(45.,0.,0.)) ;
#52336 = CARTESIAN_POINT('',(30.5,-17.3784175752015,-43.8573964979902)) ;
#52337 = CARTESIAN_POINT('',(30.5,-16.4316452160248,-44.2208283560438)) ;
#52338 = CARTESIAN_POINT('Origin',(30.5,0.,0.)) ;
#52339 = CARTESIAN_POINT('',(2.5,-17.3784175752014,-43.8573964979902)) ;
#52340 = CARTESIAN_POINT('',(30.5,-17.3784175752014,-43.8573964979902)) ;
#52341 = CARTESIAN_POINT('',(2.5,-16.4316452160248,-44.2208283560438)) ;
#52342 = CARTESIAN_POINT('Origin',(2.49999999999999,0.,0.)) ;
#52343 = CARTESIAN_POINT('',(30.5,-16.4316452160248,-44.2208283560438)) ;
#52344 = CARTESIAN_POINT('Origin',(45.,0.,0.)) ;
#52345 = CARTESIAN_POINT('',(30.5,-12.6988705265356,-45.4336803742585)) ;
#52346 = CARTESIAN_POINT('',(30.5,-11.7192957117801,-45.6961566547981)) ;
#52347 = CARTESIAN_POINT('Origin',(30.5,0.,0.)) ;
#52348 = CARTESIAN_POINT('',(2.5,-12.6988705265355,-45.4336803742585)) ;
#52349 = CARTESIAN_POINT('',(30.5,-12.6988705265355,-45.4336803742585)) ;
#52350 = CARTESIAN_POINT('',(2.5,-11.7192957117801,-45.6961566547981)) ;
#52351 = CARTESIAN_POINT('Origin',(2.49999999999999,0.,0.)) ;
#52352 = CARTESIAN_POINT('',(30.5,-11.7192957117801,-45.6961566547981)) ;
#52353 = CARTESIAN_POINT('Origin',(45.,0.,0.)) ;
#52354 = CARTESIAN_POINT('',(30.5,-7.88019199497155,-46.5121833407376)) ;
#52355 = CARTESIAN_POINT('',(30.5,-6.87854715129677,-46.670828298707)) ;
#52356 = CARTESIAN_POINT('Origin',(30.5,0.,0.)) ;
#52357 = CARTESIAN_POINT('',(2.5,-7.88019199497142,-46.5121833407375)) ;
#52358 = CARTESIAN_POINT('',(30.5,-7.88019199497142,-46.5121833407375)) ;
#52359 = CARTESIAN_POINT('',(2.5,-6.87854715129677,-46.670828298707)) ;
#52360 = CARTESIAN_POINT('Origin',(2.49999999999999,0.,0.)) ;
#52361 = CARTESIAN_POINT('',(30.5,-6.87854715129677,-46.670828298707)) ;
#52362 = CARTESIAN_POINT('Origin',(45.,0.,0.)) ;
#52363 = CARTESIAN_POINT('',(30.5,-2.97517643087433,-47.0810890932354)) ;
#52364 = CARTESIAN_POINT('',(30.5,-1.96243578879536,-47.1341645812764)) ;
#52365 = CARTESIAN_POINT('Origin',(30.5,0.,0.)) ;
#52366 = CARTESIAN_POINT('',(2.5,-2.97517643087419,-47.0810890932354)) ;
#52367 = CARTESIAN_POINT('',(30.5,-2.97517643087419,-47.0810890932354)) ;
#52368 = CARTESIAN_POINT('',(2.5,-1.96243578879536,-47.1341645812764)) ;
#52369 = CARTESIAN_POINT('Origin',(2.49999999999999,0.,0.)) ;
#52370 = CARTESIAN_POINT('',(30.5,-1.96243578879536,-47.1341645812764)) ;
#52371 = CARTESIAN_POINT('Origin',(45.,0.,0.)) ;
#52372 = CARTESIAN_POINT('',(30.5,1.96243578879521,-47.1341645812764)) ;
#52373 = CARTESIAN_POINT('',(30.5,2.9751764308742,-47.0810890932354)) ;
#52374 = CARTESIAN_POINT('Origin',(30.5,0.,0.)) ;
#52375 = CARTESIAN_POINT('',(2.5,1.96243578879534,-47.1341645812764)) ;
#52376 = CARTESIAN_POINT('',(30.5,1.96243578879534,-47.1341645812764)) ;
#52377 = CARTESIAN_POINT('',(2.5,2.9751764308742,-47.0810890932354)) ;
#52378 = CARTESIAN_POINT('Origin',(2.49999999999999,0.,0.)) ;
#52379 = CARTESIAN_POINT('',(30.5,2.9751764308742,-47.0810890932354)) ;
#52380 = CARTESIAN_POINT('Origin',(45.,0.,0.)) ;
#52381 = CARTESIAN_POINT('',(30.5,6.87854715129665,-46.670828298707)) ;
#52382 = CARTESIAN_POINT('',(30.5,7.88019199497141,-46.5121833407376)) ;
#52383 = CARTESIAN_POINT('Origin',(30.5,0.,0.)) ;
#52384 = CARTESIAN_POINT('',(2.5,6.87854715129677,-46.6708282987069)) ;
#52385 = CARTESIAN_POINT('',(30.5,6.87854715129677,-46.6708282987069)) ;
#52386 = CARTESIAN_POINT('',(2.5,7.88019199497141,-46.5121833407376)) ;
#52387 = CARTESIAN_POINT('Origin',(2.49999999999999,0.,0.)) ;
#52388 = CARTESIAN_POINT('',(30.5,7.88019199497141,-46.5121833407376)) ;
#52389 = CARTESIAN_POINT('Origin',(45.,0.,0.)) ;
#52390 = CARTESIAN_POINT('',(30.5,11.7192957117799,-45.6961566547982)) ;
#52391 = CARTESIAN_POINT('',(30.5,12.6988705265355,-45.4336803742586)) ;
#52392 = CARTESIAN_POINT('Origin',(30.5,0.,0.)) ;
#52393 = CARTESIAN_POINT('',(2.5,11.71929571178,-45.6961566547981)) ;
#52394 = CARTESIAN_POINT('',(30.5,11.71929571178,-45.6961566547981)) ;
#52395 = CARTESIAN_POINT('',(2.5,12.6988705265355,-45.4336803742586)) ;
#52396 = CARTESIAN_POINT('Origin',(2.49999999999999,0.,0.)) ;
#52397 = CARTESIAN_POINT('',(30.5,12.6988705265355,-45.4336803742586)) ;
#52398 = CARTESIAN_POINT('Origin',(45.,0.,0.)) ;
#52399 = CARTESIAN_POINT('',(30.5,16.4316452160247,-44.2208283560439)) ;
#52400 = CARTESIAN_POINT('',(30.5,17.3784175752014,-43.8573964979903)) ;
#52401 = CARTESIAN_POINT('Origin',(30.5,0.,0.)) ;
#52402 = CARTESIAN_POINT('',(2.5,16.4316452160248,-44.2208283560438)) ;
#52403 = CARTESIAN_POINT('',(30.5,16.4316452160248,-44.2208283560438)) ;
#52404 = CARTESIAN_POINT('',(2.5,17.3784175752014,-43.8573964979903)) ;
#52405 = CARTESIAN_POINT('Origin',(2.49999999999999,0.,0.)) ;
#52406 = CARTESIAN_POINT('',(30.5,17.3784175752014,-43.8573964979903)) ;
#52407 = CARTESIAN_POINT('Origin',(45.,0.,0.)) ;
#52408 = CARTESIAN_POINT('',(30.5,20.9639661767398,-42.2610074080175)) ;
#52409 = CARTESIAN_POINT('',(30.5,21.8675630442457,-41.8006018079398)) ;
#52410 = CARTESIAN_POINT('Origin',(30.5,0.,0.)) ;
#52411 = CARTESIAN_POINT('',(2.5,20.9639661767399,-42.2610074080174)) ;
#52412 = CARTESIAN_POINT('',(30.5,20.9639661767399,-42.2610074080174)) ;
#52413 = CARTESIAN_POINT('',(2.5,21.8675630442457,-41.8006018079398)) ;
#52414 = CARTESIAN_POINT('Origin',(2.49999999999999,0.,0.)) ;
#52415 = CARTESIAN_POINT('',(30.5,21.8675630442457,-41.8006018079398)) ;
#52416 = CARTESIAN_POINT('Origin',(45.,0.,0.)) ;
#52417 = CARTESIAN_POINT('',(30.5,25.2666015370306,-39.8381660191445)) ;
#52418 = CARTESIAN_POINT('',(30.5,26.1171229164955,-39.2858309771432)) ;
#52419 = CARTESIAN_POINT('Origin',(30.5,0.,0.)) ;
#52420 = CARTESIAN_POINT('',(2.5,25.2666015370307,-39.8381660191444)) ;
#52421 = CARTESIAN_POINT('',(30.5,25.2666015370307,-39.8381660191444)) ;
#52422 = CARTESIAN_POINT('',(2.5,26.1171229164955,-39.2858309771432)) ;
#52423 = CARTESIAN_POINT('Origin',(2.49999999999999,0.,0.)) ;
#52424 = CARTESIAN_POINT('',(30.5,26.1171229164955,-39.2858309771432)) ;
#52425 = CARTESIAN_POINT('Origin',(45.,0.,0.)) ;
#52426 = CARTESIAN_POINT('',(30.5,33.7143846624785,-32.9972861282626)) ;
#52427 = CARTESIAN_POINT('',(2.5,33.7143846624785,-32.9972861282626)) ;
#52428 = CARTESIAN_POINT('',(30.5,33.7143846624785,-32.9972861282626)) ;
#52429 = CARTESIAN_POINT('',(30.5,32.9972861282625,-33.7143846624786)) ;
#52430 = CARTESIAN_POINT('Origin',(30.5,0.,0.)) ;
#52431 = CARTESIAN_POINT('',(2.5,32.9972861282626,-33.7143846624785)) ;
#52432 = CARTESIAN_POINT('',(30.5,32.9972861282626,-33.7143846624785)) ;
#52433 = CARTESIAN_POINT('Origin',(2.49999999999999,0.,0.)) ;
#52434 = CARTESIAN_POINT('Origin',(45.,0.,0.)) ;
#52435 = CARTESIAN_POINT('',(30.5,29.2924107235055,-36.9788493466936)) ;
#52436 = CARTESIAN_POINT('',(30.5,30.0805381247128,-36.3406363610724)) ;
#52437 = CARTESIAN_POINT('Origin',(30.5,0.,0.)) ;
#52438 = CARTESIAN_POINT('',(2.5,29.2924107235055,-36.9788493466935)) ;
#52439 = CARTESIAN_POINT('',(30.5,29.2924107235055,-36.9788493466935)) ;
#52440 = CARTESIAN_POINT('',(2.5,30.0805381247128,-36.3406363610724)) ;
#52441 = CARTESIAN_POINT('Origin',(2.49999999999999,0.,0.)) ;
#52442 = CARTESIAN_POINT('',(30.5,30.0805381247128,-36.3406363610724)) ;
#52443 = CARTESIAN_POINT('Origin',(45.,0.,0.)) ;
#52444 = CARTESIAN_POINT('',(30.5,36.3406363610723,-30.0805381247129)) ;
#52445 = CARTESIAN_POINT('',(30.5,36.9788493466935,-29.2924107235056)) ;
#52446 = CARTESIAN_POINT('Origin',(30.5,0.,0.)) ;
#52447 = CARTESIAN_POINT('',(2.5,36.3406363610724,-30.0805381247128)) ;
#52448 = CARTESIAN_POINT('',(30.5,36.3406363610724,-30.0805381247128)) ;
#52449 = CARTESIAN_POINT('',(2.5,36.9788493466935,-29.2924107235056)) ;
#52450 = CARTESIAN_POINT('Origin',(2.49999999999999,0.,0.)) ;
#52451 = CARTESIAN_POINT('',(30.5,36.9788493466935,-29.2924107235056)) ;
#52452 = CARTESIAN_POINT('Origin',(45.,0.,0.)) ;
#52453 = CARTESIAN_POINT('',(30.5,39.2858309771432,-26.1171229164956)) ;
#52454 = CARTESIAN_POINT('',(30.5,39.8381660191444,-25.2666015370307)) ;
#52455 = CARTESIAN_POINT('Origin',(30.5,0.,0.)) ;
#52456 = CARTESIAN_POINT('',(2.5,39.2858309771432,-26.1171229164954)) ;
#52457 = CARTESIAN_POINT('',(30.5,39.2858309771432,-26.1171229164954)) ;
#52458 = CARTESIAN_POINT('',(2.5,39.8381660191444,-25.2666015370307)) ;
#52459 = CARTESIAN_POINT('Origin',(2.49999999999999,0.,0.)) ;
#52460 = CARTESIAN_POINT('',(30.5,39.8381660191444,-25.2666015370307)) ;
#52461 = CARTESIAN_POINT('Origin',(45.,0.,0.)) ;
#52462 = CARTESIAN_POINT('',(30.5,41.8006018079397,-21.8675630442458)) ;
#52463 = CARTESIAN_POINT('',(30.5,42.2610074080174,-20.9639661767399)) ;
#52464 = CARTESIAN_POINT('Origin',(30.5,0.,0.)) ;
#52465 = CARTESIAN_POINT('',(2.5,41.8006018079397,-21.8675630442457)) ;
#52466 = CARTESIAN_POINT('',(30.5,41.8006018079397,-21.8675630442457)) ;
#52467 = CARTESIAN_POINT('',(2.5,42.2610074080174,-20.9639661767399)) ;
#52468 = CARTESIAN_POINT('Origin',(2.49999999999999,0.,0.)) ;
#52469 = CARTESIAN_POINT('',(30.5,42.2610074080174,-20.9639661767399)) ;
#52470 = CARTESIAN_POINT('Origin',(45.,0.,0.)) ;
#52471 = CARTESIAN_POINT('',(30.5,43.8573964979902,-17.3784175752015)) ;
#52472 = CARTESIAN_POINT('',(30.5,44.2208283560438,-16.4316452160248)) ;
#52473 = CARTESIAN_POINT('Origin',(30.5,0.,0.)) ;
#52474 = CARTESIAN_POINT('',(2.5,43.8573964979902,-17.3784175752014)) ;
#52475 = CARTESIAN_POINT('',(30.5,43.8573964979902,-17.3784175752014)) ;
#52476 = CARTESIAN_POINT('',(2.5,44.2208283560438,-16.4316452160248)) ;
#52477 = CARTESIAN_POINT('Origin',(2.49999999999999,0.,0.)) ;
#52478 = CARTESIAN_POINT('',(30.5,44.2208283560438,-16.4316452160248)) ;
#52479 = CARTESIAN_POINT('Origin',(45.,0.,0.)) ;
#52480 = CARTESIAN_POINT('',(30.5,45.4336803742585,-12.6988705265356)) ;
#52481 = CARTESIAN_POINT('',(30.5,45.6961566547981,-11.7192957117801)) ;
#52482 = CARTESIAN_POINT('Origin',(30.5,0.,0.)) ;
#52483 = CARTESIAN_POINT('',(2.5,45.4336803742585,-12.6988705265355)) ;
#52484 = CARTESIAN_POINT('',(30.5,45.4336803742585,-12.6988705265355)) ;
#52485 = CARTESIAN_POINT('',(2.5,45.6961566547981,-11.7192957117801)) ;
#52486 = CARTESIAN_POINT('Origin',(2.49999999999999,0.,0.)) ;
#52487 = CARTESIAN_POINT('',(30.5,45.6961566547981,-11.7192957117801)) ;
#52488 = CARTESIAN_POINT('Origin',(45.,0.,0.)) ;
#52489 = CARTESIAN_POINT('',(30.5,46.5121833407376,-7.88019199497153)) ;
#52490 = CARTESIAN_POINT('',(30.5,46.670828298707,-6.87854715129677)) ;
#52491 = CARTESIAN_POINT('Origin',(30.5,0.,0.)) ;
#52492 = CARTESIAN_POINT('',(2.5,46.5121833407376,-7.88019199497139)) ;
#52493 = CARTESIAN_POINT('',(30.5,46.5121833407376,-7.88019199497139)) ;
#52494 = CARTESIAN_POINT('',(2.5,46.670828298707,-6.87854715129677)) ;
#52495 = CARTESIAN_POINT('Origin',(2.49999999999999,0.,0.)) ;
#52496 = CARTESIAN_POINT('',(30.5,46.670828298707,-6.87854715129677)) ;
#52497 = CARTESIAN_POINT('Origin',(45.,0.,0.)) ;
#52498 = CARTESIAN_POINT('',(30.5,47.0810890932354,2.9751764308742)) ;
#52499 = CARTESIAN_POINT('',(2.5,47.0810890932354,2.9751764308742)) ;
#52500 = CARTESIAN_POINT('',(30.5,47.0810890932354,2.9751764308742)) ;
#52501 = CARTESIAN_POINT('',(30.5,47.1341645812764,1.96243578879522)) ;
#52502 = CARTESIAN_POINT('Origin',(30.5,0.,0.)) ;
#52503 = CARTESIAN_POINT('',(2.5,47.1341645812764,1.96243578879535)) ;
#52504 = CARTESIAN_POINT('',(30.5,47.1341645812764,1.96243578879535)) ;
#52505 = CARTESIAN_POINT('Origin',(2.49999999999999,0.,0.)) ;
#52506 = CARTESIAN_POINT('Origin',(45.,0.,0.)) ;
#52507 = CARTESIAN_POINT('',(30.5,47.0810890932354,-2.97517643087433)) ;
#52508 = CARTESIAN_POINT('',(30.5,47.1341645812764,-1.96243578879535)) ;
#52509 = CARTESIAN_POINT('Origin',(30.5,0.,0.)) ;
#52510 = CARTESIAN_POINT('',(2.5,47.0810890932354,-2.9751764308742)) ;
#52511 = CARTESIAN_POINT('',(30.5,47.0810890932354,-2.9751764308742)) ;
#52512 = CARTESIAN_POINT('',(2.5,47.1341645812764,-1.96243578879535)) ;
#52513 = CARTESIAN_POINT('Origin',(2.49999999999999,0.,0.)) ;
#52514 = CARTESIAN_POINT('',(30.5,47.1341645812764,-1.96243578879535)) ;
#52515 = CARTESIAN_POINT('Origin',(45.,0.,0.)) ;
#52516 = CARTESIAN_POINT('',(1.5,-4.89858719658941E-15,40.)) ;
#52517 = CARTESIAN_POINT('Origin',(1.5,0.,0.)) ;
#52518 = CARTESIAN_POINT('',(45.,-4.89858719658941E-15,40.)) ;
#52519 = CARTESIAN_POINT('Origin',(1.5,40.,0.)) ;
#52520 = CARTESIAN_POINT('',(1.5,0.,-47.0433475024125)) ;
#52521 = CARTESIAN_POINT('Origin',(1.5,0.,0.)) ;
#52522 = CARTESIAN_POINT('Origin',(1.5,0.,0.)) ;
#52523 = CARTESIAN_POINT('',(0.91109230130857,-6.03030546426507E-15,-49.2411809548974)) ;
#52524 = CARTESIAN_POINT('',(1.5,-5.76114849400061E-15,-47.0433475024125)) ;
#52525 = CARTESIAN_POINT('',(0.911092301308557,-6.03030546426507E-15,49.2411809548974)) ;
#52526 = CARTESIAN_POINT('Origin',(0.911092301308557,0.,0.)) ;
#52527 = CARTESIAN_POINT('Origin',(0.911092301308557,0.,0.)) ;
#52528 = CARTESIAN_POINT('Origin',(0.911092301308557,0.,0.)) ;
#52529 = CARTESIAN_POINT('',(1.87701812759763,0.,-49.5)) ;
#52530 = CARTESIAN_POINT('',(1.87701812759764,-6.06200165577939E-15,49.5)) ;
#52531 = CARTESIAN_POINT('Origin',(1.87701812759763,0.,0.)) ;
#52532 = CARTESIAN_POINT('Origin',(1.87701812759763,0.,0.)) ;
#52533 = CARTESIAN_POINT('',(0.911092301308557,-6.03030546426507E-15,49.2411809548974)) ;
#52534 = CARTESIAN_POINT('Origin',(1.87701812759763,0.,0.)) ;
#52535 = CARTESIAN_POINT('',(2.49999999999999,-5.77727127497764E-15,-47.175)) ;
#52536 = CARTESIAN_POINT('',(1.87701812759763,-6.0620016557794E-15,-49.5)) ;
#52537 = CARTESIAN_POINT('Origin',(2.49999999999999,0.,0.)) ;
#52538 = CARTESIAN_POINT('Origin',(2.49999999999999,0.,0.)) ;
#52539 = CARTESIAN_POINT('Origin',(2.49999999999999,0.,0.)) ;
#52540 = CARTESIAN_POINT('Origin',(2.49999999999999,0.,0.)) ;
#52541 = CARTESIAN_POINT('Origin',(2.49999999999999,0.,0.)) ;
#52542 = CARTESIAN_POINT('Origin',(2.49999999999999,0.,0.)) ;
#52543 = CARTESIAN_POINT('Origin',(2.49999999999999,0.,0.)) ;
#52544 = CARTESIAN_POINT('Origin',(2.49999999999999,0.,0.)) ;
#52545 = CARTESIAN_POINT('Origin',(2.49999999999999,0.,0.)) ;
#52546 = CARTESIAN_POINT('Origin',(2.49999999999999,0.,0.)) ;
#52547 = CARTESIAN_POINT('Origin',(2.49999999999999,0.,0.)) ;
#52548 = CARTESIAN_POINT('Origin',(2.49999999999999,0.,0.)) ;
#52549 = CARTESIAN_POINT('Origin',(2.49999999999999,0.,0.)) ;
#52550 = CARTESIAN_POINT('Origin',(2.49999999999999,0.,0.)) ;
#52551 = CARTESIAN_POINT('Origin',(2.49999999999999,0.,0.)) ;
#52552 = CARTESIAN_POINT('Origin',(2.49999999999999,0.,0.)) ;
#52553 = CARTESIAN_POINT('Origin',(2.49999999999999,0.,0.)) ;
#52554 = CARTESIAN_POINT('Origin',(2.49999999999999,0.,0.)) ;
#52555 = CARTESIAN_POINT('Origin',(2.49999999999999,0.,0.)) ;
#52556 = CARTESIAN_POINT('Origin',(2.49999999999999,0.,0.)) ;
#52557 = CARTESIAN_POINT('Origin',(2.49999999999999,0.,0.)) ;
#52558 = CARTESIAN_POINT('Origin',(2.49999999999999,0.,0.)) ;
#52559 = CARTESIAN_POINT('Origin',(2.49999999999999,0.,0.)) ;
#52560 = CARTESIAN_POINT('Origin',(2.49999999999999,0.,0.)) ;
#52561 = CARTESIAN_POINT('Origin',(2.49999999999999,0.,0.)) ;
#52562 = CARTESIAN_POINT('Origin',(2.49999999999999,0.,0.)) ;
#52563 = CARTESIAN_POINT('Origin',(2.49999999999999,0.,0.)) ;
#52564 = CARTESIAN_POINT('Origin',(2.49999999999999,0.,0.)) ;
#52565 = CARTESIAN_POINT('Origin',(2.49999999999999,0.,0.)) ;
#52566 = CARTESIAN_POINT('Origin',(2.49999999999999,0.,0.)) ;
#52567 = CARTESIAN_POINT('Origin',(2.49999999999999,0.,0.)) ;
#52568 = CARTESIAN_POINT('Origin',(2.49999999999999,0.,0.)) ;
#52569 = CARTESIAN_POINT('Origin',(2.49999999999999,0.,0.)) ;
#52570 = CARTESIAN_POINT('Origin',(2.49999999999999,0.,0.)) ;
#52571 = CARTESIAN_POINT('Origin',(2.49999999999999,0.,0.)) ;
#52572 = CARTESIAN_POINT('Origin',(2.49999999999999,0.,0.)) ;
#52573 = CARTESIAN_POINT('Origin',(2.49999999999999,0.,0.)) ;
#52574 = CARTESIAN_POINT('Origin',(2.49999999999999,0.,0.)) ;
#52575 = CARTESIAN_POINT('Origin',(2.49999999999999,0.,0.)) ;
#52576 = CARTESIAN_POINT('Origin',(2.49999999999999,0.,0.)) ;
#52577 = CARTESIAN_POINT('Origin',(2.49999999999999,0.,0.)) ;
#52578 = CARTESIAN_POINT('Origin',(2.49999999999999,0.,0.)) ;
#52579 = CARTESIAN_POINT('Origin',(2.49999999999999,0.,0.)) ;
#52580 = CARTESIAN_POINT('Origin',(2.49999999999999,0.,0.)) ;
#52581 = CARTESIAN_POINT('Origin',(2.49999999999999,0.,0.)) ;
#52582 = CARTESIAN_POINT('Origin',(2.49999999999999,0.,0.)) ;
#52583 = CARTESIAN_POINT('Origin',(2.49999999999999,0.,0.)) ;
#52584 = CARTESIAN_POINT('Origin',(2.49999999999999,0.,0.)) ;
#52585 = CARTESIAN_POINT('Origin',(2.49999999999999,0.,0.)) ;
#52586 = CARTESIAN_POINT('Origin',(2.49999999999999,0.,0.)) ;
#52587 = CARTESIAN_POINT('Origin',(2.49999999999999,0.,0.)) ;
#52588 = CARTESIAN_POINT('Origin',(2.49999999999999,0.,0.)) ;
#52589 = CARTESIAN_POINT('Origin',(2.49999999999999,0.,0.)) ;
#52590 = CARTESIAN_POINT('Origin',(2.49999999999999,0.,0.)) ;
#52591 = CARTESIAN_POINT('Origin',(2.49999999999999,0.,0.)) ;
#52592 = CARTESIAN_POINT('Origin',(2.49999999999999,0.,0.)) ;
#52593 = CARTESIAN_POINT('Origin',(2.49999999999999,0.,0.)) ;
#52594 = CARTESIAN_POINT('Origin',(2.49999999999999,0.,0.)) ;
#52595 = CARTESIAN_POINT('Origin',(2.49999999999999,0.,0.)) ;
#52596 = CARTESIAN_POINT('Origin',(2.49999999999999,0.,0.)) ;
#52597 = CARTESIAN_POINT('Origin',(2.49999999999999,0.,0.)) ;
#52598 = CARTESIAN_POINT('Origin',(30.5,0.,0.)) ;
#52599 = CARTESIAN_POINT('',(31.1229818724024,0.,-49.5)) ;
#52600 = CARTESIAN_POINT('',(31.1229818724024,-6.0620016557794E-15,49.5)) ;
#52601 = CARTESIAN_POINT('Origin',(31.1229818724024,0.,0.)) ;
#52602 = CARTESIAN_POINT('Origin',(31.1229818724024,0.,0.)) ;
#52603 = CARTESIAN_POINT('',(30.5,-5.77727127497764E-15,47.175)) ;
#52604 = CARTESIAN_POINT('',(30.5,-5.77727127497764E-15,47.175)) ;
#52605 = CARTESIAN_POINT('Origin',(30.5,0.,0.)) ;
#52606 = CARTESIAN_POINT('Origin',(30.5,0.,0.)) ;
#52607 = CARTESIAN_POINT('Origin',(30.5,0.,0.)) ;
#52608 = CARTESIAN_POINT('Origin',(30.5,0.,0.)) ;
#52609 = CARTESIAN_POINT('Origin',(30.5,0.,0.)) ;
#52610 = CARTESIAN_POINT('Origin',(30.5,0.,0.)) ;
#52611 = CARTESIAN_POINT('Origin',(30.5,0.,0.)) ;
#52612 = CARTESIAN_POINT('Origin',(30.5,0.,0.)) ;
#52613 = CARTESIAN_POINT('Origin',(30.5,0.,0.)) ;
#52614 = CARTESIAN_POINT('Origin',(30.5,0.,0.)) ;
#52615 = CARTESIAN_POINT('Origin',(30.5,0.,0.)) ;
#52616 = CARTESIAN_POINT('Origin',(30.5,0.,0.)) ;
#52617 = CARTESIAN_POINT('Origin',(30.5,0.,0.)) ;
#52618 = CARTESIAN_POINT('Origin',(30.5,0.,0.)) ;
#52619 = CARTESIAN_POINT('Origin',(30.5,0.,0.)) ;
#52620 = CARTESIAN_POINT('Origin',(30.5,0.,0.)) ;
#52621 = CARTESIAN_POINT('Origin',(30.5,0.,0.)) ;
#52622 = CARTESIAN_POINT('Origin',(30.5,0.,0.)) ;
#52623 = CARTESIAN_POINT('Origin',(30.5,0.,0.)) ;
#52624 = CARTESIAN_POINT('Origin',(30.5,0.,0.)) ;
#52625 = CARTESIAN_POINT('Origin',(30.5,0.,0.)) ;
#52626 = CARTESIAN_POINT('Origin',(30.5,0.,0.)) ;
#52627 = CARTESIAN_POINT('Origin',(30.5,0.,0.)) ;
#52628 = CARTESIAN_POINT('Origin',(30.5,0.,0.)) ;
#52629 = CARTESIAN_POINT('Origin',(30.5,0.,0.)) ;
#52630 = CARTESIAN_POINT('Origin',(30.5,0.,0.)) ;
#52631 = CARTESIAN_POINT('Origin',(30.5,0.,0.)) ;
#52632 = CARTESIAN_POINT('Origin',(30.5,0.,0.)) ;
#52633 = CARTESIAN_POINT('Origin',(30.5,0.,0.)) ;
#52634 = CARTESIAN_POINT('Origin',(30.5,0.,0.)) ;
#52635 = CARTESIAN_POINT('Origin',(30.5,0.,0.)) ;
#52636 = CARTESIAN_POINT('Origin',(30.5,0.,0.)) ;
#52637 = CARTESIAN_POINT('Origin',(30.5,0.,0.)) ;
#52638 = CARTESIAN_POINT('Origin',(30.5,0.,0.)) ;
#52639 = CARTESIAN_POINT('Origin',(30.5,0.,0.)) ;
#52640 = CARTESIAN_POINT('Origin',(30.5,0.,0.)) ;
#52641 = CARTESIAN_POINT('Origin',(30.5,0.,0.)) ;
#52642 = CARTESIAN_POINT('Origin',(30.5,0.,0.)) ;
#52643 = CARTESIAN_POINT('Origin',(30.5,0.,0.)) ;
#52644 = CARTESIAN_POINT('Origin',(30.5,0.,0.)) ;
#52645 = CARTESIAN_POINT('Origin',(30.5,0.,0.)) ;
#52646 = CARTESIAN_POINT('Origin',(30.5,0.,0.)) ;
#52647 = CARTESIAN_POINT('Origin',(30.5,0.,0.)) ;
#52648 = CARTESIAN_POINT('Origin',(30.5,0.,0.)) ;
#52649 = CARTESIAN_POINT('Origin',(30.5,0.,0.)) ;
#52650 = CARTESIAN_POINT('Origin',(30.5,0.,0.)) ;
#52651 = CARTESIAN_POINT('Origin',(30.5,0.,0.)) ;
#52652 = CARTESIAN_POINT('Origin',(30.5,0.,0.)) ;
#52653 = CARTESIAN_POINT('Origin',(30.5,0.,0.)) ;
#52654 = CARTESIAN_POINT('Origin',(30.5,0.,0.)) ;
#52655 = CARTESIAN_POINT('Origin',(30.5,0.,0.)) ;
#52656 = CARTESIAN_POINT('Origin',(30.5,0.,0.)) ;
#52657 = CARTESIAN_POINT('Origin',(30.5,0.,0.)) ;
#52658 = CARTESIAN_POINT('Origin',(30.5,0.,0.)) ;
#52659 = CARTESIAN_POINT('Origin',(30.5,0.,0.)) ;
#52660 = CARTESIAN_POINT('Origin',(30.5,0.,0.)) ;
#52661 = CARTESIAN_POINT('Origin',(30.5,0.,0.)) ;
#52662 = CARTESIAN_POINT('Origin',(30.5,0.,0.)) ;
#52663 = CARTESIAN_POINT('Origin',(30.5,0.,0.)) ;
#52664 = CARTESIAN_POINT('Origin',(30.5,0.,0.)) ;
#52665 = CARTESIAN_POINT('Origin',(30.5,0.,0.)) ;
#52666 = CARTESIAN_POINT('Origin',(31.1229818724024,0.,0.)) ;
#52667 = CARTESIAN_POINT('',(32.0889076986914,-6.03030546426508E-15,-49.2411809548975)) ;
#52668 = CARTESIAN_POINT('',(31.1229818724024,-6.0620016557794E-15,-49.5)) ;
#52669 = CARTESIAN_POINT('',(32.0889076986914,-6.03030546426508E-15,49.2411809548975)) ;
#52670 = CARTESIAN_POINT('Origin',(32.0889076986914,0.,0.)) ;
#52671 = CARTESIAN_POINT('Origin',(32.0889076986914,0.,0.)) ;
#52672 = CARTESIAN_POINT('Origin',(32.0889076986914,0.,0.)) ;
#52673 = CARTESIAN_POINT('',(31.5,-5.76114849400062E-15,47.0433475024126)) ;
#52674 = CARTESIAN_POINT('Origin',(31.5,0.,0.)) ;
#52675 = CARTESIAN_POINT('',(32.0889076986914,-6.03030546426508E-15,49.2411809548975)) ;
#52676 = CARTESIAN_POINT('Origin',(31.5,47.0433475024126,0.)) ;
#52677 = CARTESIAN_POINT('',(31.5,-4.89858719658941E-15,40.)) ;
#52678 = CARTESIAN_POINT('Origin',(31.5,0.,0.)) ;
#52679 = CARTESIAN_POINT('Origin',(45.,0.,0.)) ;
#52680 = CARTESIAN_POINT('',(33.,-4.89858719658941E-15,40.)) ;
#52681 = CARTESIAN_POINT('Origin',(33.,0.,0.)) ;
#52682 = CARTESIAN_POINT('',(45.,-4.89858719658941E-15,40.)) ;
#52683 = CARTESIAN_POINT('Origin',(33.,40.,0.)) ;
#52684 = CARTESIAN_POINT('',(33.,-4.59242549680258E-15,37.5)) ;
#52685 = CARTESIAN_POINT('Origin',(33.,0.,0.)) ;
#52686 = CARTESIAN_POINT('Origin',(45.,0.,0.)) ;
#52687 = CARTESIAN_POINT('',(45.,-4.59242549680258E-15,37.5)) ;
#52688 = CARTESIAN_POINT('Origin',(45.,0.,0.)) ;
#52689 = CARTESIAN_POINT('',(45.,-4.59242549680258E-15,37.5)) ;
#52690 = CARTESIAN_POINT('Origin',(45.,37.5,0.)) ;
#52691 = CARTESIAN_POINT('Origin',(45.,0.,0.)) ;
#52692 = CARTESIAN_POINT('Origin',(2.5,-2.84494650060196E-12,-7.9580439460436E-14)) ;
#52693 = CARTESIAN_POINT('',(2.5,46.5975179480543,-1.39998000660682)) ;
#52694 = CARTESIAN_POINT('Origin',(2.5,46.5946320137324,-1.93997229486941)) ;
#52695 = CARTESIAN_POINT('',(2.5,46.5975179480543,1.39998000660682)) ;
#52696 = CARTESIAN_POINT('Origin',(2.5,46.5946320137324,1.93997229486942)) ;
#52697 = CARTESIAN_POINT('Origin',(2.5,46.6049999999905,0.)) ;
#52698 = CARTESIAN_POINT('Origin',(30.5,-2.84494650060196E-12,-7.9580439460436E-14)) ;
#52699 = CARTESIAN_POINT('',(30.5,46.5975179480543,-1.39998000660682)) ;
#52700 = CARTESIAN_POINT('Origin',(30.5,46.5946320137324,-1.93997229486941)) ;
#52701 = CARTESIAN_POINT('',(30.5,46.5975179480543,1.39998000660682)) ;
#52702 = CARTESIAN_POINT('Origin',(30.5,46.6049999999905,0.)) ;
#52703 = CARTESIAN_POINT('Origin',(30.5,46.5946320137324,1.93997229486942)) ;
#52704 = CARTESIAN_POINT('Origin',(30.5,46.5946320137324,1.93997229486942)) ;
#52705 = CARTESIAN_POINT('',(30.5,46.5975179480543,1.39998000660682)) ;
#52706 = CARTESIAN_POINT('Origin',(30.5,46.6049999999905,0.)) ;
#52707 = CARTESIAN_POINT('',(30.5,46.5975179480543,-1.39998000660682)) ;
#52708 = CARTESIAN_POINT('Origin',(30.5,46.5946320137324,-1.93997229486941)) ;
#52709 = CARTESIAN_POINT('Origin',(2.5,-2.82104316495704E-12,-3.76522375273045E-13)) ;
#52710 = CARTESIAN_POINT('',(2.5,46.19591411046,6.26307771284532)) ;
#52711 = CARTESIAN_POINT('Origin',(2.5,46.1365994215198,6.79981020457273)) ;
#52712 = CARTESIAN_POINT('',(2.5,46.4885896278522,3.47845617354872)) ;
#52713 = CARTESIAN_POINT('Origin',(2.5,46.3496929336289,4.871549030588)) ;
#52714 = CARTESIAN_POINT('Origin',(2.5,46.5421640670489,2.94112035726179)) ;
#52715 = CARTESIAN_POINT('Origin',(30.5,-2.82104316495704E-12,-3.76522375273045E-13)) ;
#52716 = CARTESIAN_POINT('',(30.5,46.4885896278522,3.47845617354872)) ;
#52717 = CARTESIAN_POINT('Origin',(30.5,46.5421640670489,2.94112035726179)) ;
#52718 = CARTESIAN_POINT('',(30.5,46.19591411046,6.26307771284532)) ;
#52719 = CARTESIAN_POINT('Origin',(30.5,46.3496929336289,4.871549030588)) ;
#52720 = CARTESIAN_POINT('Origin',(30.5,46.1365994215198,6.79981020457273)) ;
#52721 = CARTESIAN_POINT('Origin',(30.5,46.1365994215198,6.79981020457273)) ;
#52722 = CARTESIAN_POINT('',(30.5,46.19591411046,6.26307771284532)) ;
#52723 = CARTESIAN_POINT('Origin',(30.5,46.3496929336289,4.871549030588)) ;
#52724 = CARTESIAN_POINT('',(30.5,46.4885896278522,3.47845617354872)) ;
#52725 = CARTESIAN_POINT('Origin',(30.5,46.5421640670489,2.94112035726179)) ;
#52726 = CARTESIAN_POINT('Origin',(2.5,-2.83768000704297E-12,2.18233396300179E-13)) ;
#52727 = CARTESIAN_POINT('',(2.5,46.4885896278521,-3.47845617354871)) ;
#52728 = CARTESIAN_POINT('Origin',(2.5,46.5421640670489,-2.94112035726178)) ;
#52729 = CARTESIAN_POINT('',(2.5,46.1959141104601,-6.26307771284532)) ;
#52730 = CARTESIAN_POINT('Origin',(2.5,46.3496929336289,-4.871549030588)) ;
#52731 = CARTESIAN_POINT('Origin',(2.5,46.1365994215199,-6.79981020457273)) ;
#52732 = CARTESIAN_POINT('Origin',(30.5,-2.83768000704297E-12,2.18233396300179E-13)) ;
#52733 = CARTESIAN_POINT('',(30.5,46.1959141104601,-6.26307771284532)) ;
#52734 = CARTESIAN_POINT('Origin',(30.5,46.1365994215199,-6.79981020457273)) ;
#52735 = CARTESIAN_POINT('',(30.5,46.4885896278521,-3.47845617354871)) ;
#52736 = CARTESIAN_POINT('Origin',(30.5,46.3496929336289,-4.871549030588)) ;
#52737 = CARTESIAN_POINT('Origin',(30.5,46.5421640670489,-2.94112035726178)) ;
#52738 = CARTESIAN_POINT('Origin',(30.5,46.5421640670489,-2.94112035726178)) ;
#52739 = CARTESIAN_POINT('',(30.5,46.4885896278521,-3.47845617354871)) ;
#52740 = CARTESIAN_POINT('Origin',(30.5,46.3496929336289,-4.871549030588)) ;
#52741 = CARTESIAN_POINT('',(30.5,46.1959141104601,-6.26307771284532)) ;
#52742 = CARTESIAN_POINT('Origin',(30.5,46.1365994215199,-6.79981020457273)) ;
#52743 = CARTESIAN_POINT('Origin',(2.5,-2.79932329750409E-12,5.13656221302654E-13)) ;
#52744 = CARTESIAN_POINT('',(2.5,45.8703225913244,-8.3187816599531)) ;
#52745 = CARTESIAN_POINT('Origin',(2.5,45.9797704312728,-7.78998947928981)) ;
#52746 = CARTESIAN_POINT('',(2.5,45.2881781707551,-11.0575558290286)) ;
#52747 = CARTESIAN_POINT('Origin',(2.5,45.5865689321897,-9.6897243505597)) ;
#52748 = CARTESIAN_POINT('Origin',(2.5,45.1730845913411,-11.585147970723)) ;
#52749 = CARTESIAN_POINT('Origin',(30.5,-2.79932329750409E-12,5.13656221302654E-13)) ;
#52750 = CARTESIAN_POINT('',(30.5,45.2881781707551,-11.0575558290286)) ;
#52751 = CARTESIAN_POINT('Origin',(30.5,45.1730845913411,-11.585147970723)) ;
#52752 = CARTESIAN_POINT('',(30.5,45.8703225913244,-8.3187816599531)) ;
#52753 = CARTESIAN_POINT('Origin',(30.5,45.5865689321897,-9.6897243505597)) ;
#52754 = CARTESIAN_POINT('Origin',(30.5,45.9797704312728,-7.78998947928981)) ;
#52755 = CARTESIAN_POINT('Origin',(30.5,45.9797704312728,-7.78998947928981)) ;
#52756 = CARTESIAN_POINT('',(30.5,45.8703225913244,-8.3187816599531)) ;
#52757 = CARTESIAN_POINT('Origin',(30.5,45.5865689321897,-9.6897243505597)) ;
#52758 = CARTESIAN_POINT('',(30.5,45.2881781707551,-11.0575558290286)) ;
#52759 = CARTESIAN_POINT('Origin',(30.5,45.1730845913411,-11.585147970723)) ;
#52760 = CARTESIAN_POINT('Origin',(2.5,-2.73029661612169E-12,8.03451321255064E-13)) ;
#52761 = CARTESIAN_POINT('',(2.5,44.7494907015041,-13.0679648336741)) ;
#52762 = CARTESIAN_POINT('Origin',(2.5,44.9136128087662,-12.5535098464227)) ;
#52763 = CARTESIAN_POINT('',(2.5,43.8842554738508,-15.7308850496068)) ;
#52764 = CARTESIAN_POINT('Origin',(2.5,44.3239889419266,-14.4017370228415)) ;
#52765 = CARTESIAN_POINT('Origin',(2.5,43.7146439933038,-16.2435564313579)) ;
#52766 = CARTESIAN_POINT('Origin',(30.5,-2.73029661612169E-12,8.03451321255064E-13)) ;
#52767 = CARTESIAN_POINT('',(30.5,43.8842554738508,-15.7308850496068)) ;
#52768 = CARTESIAN_POINT('Origin',(30.5,43.7146439933038,-16.2435564313579)) ;
#52769 = CARTESIAN_POINT('',(30.5,44.7494907015041,-13.0679648336741)) ;
#52770 = CARTESIAN_POINT('Origin',(30.5,44.3239889419266,-14.4017370228415)) ;
#52771 = CARTESIAN_POINT('Origin',(30.5,44.9136128087662,-12.5535098464227)) ;
#52772 = CARTESIAN_POINT('Origin',(30.5,44.9136128087662,-12.5535098464227)) ;
#52773 = CARTESIAN_POINT('',(30.5,44.7494907015041,-13.0679648336741)) ;
#52774 = CARTESIAN_POINT('Origin',(30.5,44.3239889419266,-14.4017370228415)) ;
#52775 = CARTESIAN_POINT('',(30.5,43.8842554738508,-15.7308850496068)) ;
#52776 = CARTESIAN_POINT('Origin',(30.5,43.7146439933038,-16.2435564313579)) ;
#52777 = CARTESIAN_POINT('Origin',(2.5,-2.63135623366177E-12,1.0844436403988E-12)) ;
#52778 = CARTESIAN_POINT('',(2.5,43.1383740271251,-17.6739726500298)) ;
#52779 = CARTESIAN_POINT('Origin',(2.5,43.355372245549,-17.1794913326873)) ;
#52780 = CARTESIAN_POINT('',(2.5,41.9995276906041,-20.2318634016821)) ;
#52781 = CARTESIAN_POINT('Origin',(2.5,42.5757860534247,-18.9559612505438)) ;
#52782 = CARTESIAN_POINT('Origin',(2.5,41.7772566077985,-20.7239970885482)) ;
#52783 = CARTESIAN_POINT('Origin',(30.5,-2.63135623366177E-12,1.0844436403988E-12)) ;
#52784 = CARTESIAN_POINT('',(30.5,41.9995276906041,-20.2318634016821)) ;
#52785 = CARTESIAN_POINT('Origin',(30.5,41.7772566077985,-20.7239970885482)) ;
#52786 = CARTESIAN_POINT('',(30.5,43.1383740271251,-17.6739726500298)) ;
#52787 = CARTESIAN_POINT('Origin',(30.5,42.5757860534247,-18.9559612505438)) ;
#52788 = CARTESIAN_POINT('Origin',(30.5,43.355372245549,-17.1794913326873)) ;
#52789 = CARTESIAN_POINT('Origin',(30.5,43.355372245549,-17.1794913326873)) ;
#52790 = CARTESIAN_POINT('',(30.5,43.1383740271251,-17.6739726500298)) ;
#52791 = CARTESIAN_POINT('Origin',(30.5,42.5757860534247,-18.9559612505438)) ;
#52792 = CARTESIAN_POINT('',(30.5,41.9995276906041,-20.2318634016821)) ;
#52793 = CARTESIAN_POINT('Origin',(30.5,41.7772566077985,-20.7239970885482)) ;
#52794 = CARTESIAN_POINT('Origin',(2.5,-2.50358616165916E-12,1.35355456808391E-12)) ;
#52795 = CARTESIAN_POINT('',(2.5,41.0546242996198,-22.0863407235153)) ;
#52796 = CARTESIAN_POINT('Origin',(2.5,41.3221211513146,-21.6172507168713)) ;
#52797 = CARTESIAN_POINT('',(2.5,39.654644293013,-24.511177224539)) ;
#52798 = CARTESIAN_POINT('Origin',(2.5,40.3611139433656,-23.3024999999953)) ;
#52799 = CARTESIAN_POINT('Origin',(2.5,39.3821488564453,-24.9773812968611)) ;
#52800 = CARTESIAN_POINT('Origin',(30.5,-2.50358616165916E-12,1.35355456808391E-12)) ;
#52801 = CARTESIAN_POINT('',(30.5,39.654644293013,-24.511177224539)) ;
#52802 = CARTESIAN_POINT('Origin',(30.5,39.3821488564453,-24.9773812968611)) ;
#52803 = CARTESIAN_POINT('',(30.5,41.0546242996198,-22.0863407235153)) ;
#52804 = CARTESIAN_POINT('Origin',(30.5,40.3611139433656,-23.3024999999953)) ;
#52805 = CARTESIAN_POINT('Origin',(30.5,41.3221211513146,-21.6172507168713)) ;
#52806 = CARTESIAN_POINT('Origin',(30.5,41.3221211513146,-21.6172507168713)) ;
#52807 = CARTESIAN_POINT('',(30.5,41.0546242996198,-22.0863407235153)) ;
#52808 = CARTESIAN_POINT('Origin',(30.5,40.3611139433656,-23.3024999999953)) ;
#52809 = CARTESIAN_POINT('',(30.5,39.654644293013,-24.511177224539)) ;
#52810 = CARTESIAN_POINT('Origin',(30.5,39.3821488564453,-24.9773812968611)) ;
#52811 = CARTESIAN_POINT('Origin',(2.5,-2.34838627576032E-12,1.60783566867159E-12)) ;
#52812 = CARTESIAN_POINT('',(2.5,38.5210715170554,-26.2567262261701)) ;
#52813 = CARTESIAN_POINT('Origin',(2.5,38.8361362505367,-25.8181669785007)) ;
#52814 = CARTESIAN_POINT('',(2.5,36.8752963142798,-28.5219414604302)) ;
#52815 = CARTESIAN_POINT('Origin',(2.5,37.7042370228368,-27.3937316830851)) ;
#52816 = CARTESIAN_POINT('Origin',(2.5,36.5555620409763,-28.9571080888326)) ;
#52817 = CARTESIAN_POINT('Origin',(30.5,-2.34838627576032E-12,1.60783566867159E-12)) ;
#52818 = CARTESIAN_POINT('',(30.5,36.8752963142798,-28.5219414604302)) ;
#52819 = CARTESIAN_POINT('Origin',(30.5,36.5555620409763,-28.9571080888326)) ;
#52820 = CARTESIAN_POINT('',(30.5,38.5210715170554,-26.2567262261701)) ;
#52821 = CARTESIAN_POINT('Origin',(30.5,37.7042370228368,-27.3937316830851)) ;
#52822 = CARTESIAN_POINT('Origin',(30.5,38.8361362505367,-25.8181669785007)) ;
#52823 = CARTESIAN_POINT('Origin',(30.5,38.8361362505367,-25.8181669785007)) ;
#52824 = CARTESIAN_POINT('',(30.5,38.5210715170554,-26.2567262261701)) ;
#52825 = CARTESIAN_POINT('Origin',(30.5,37.7042370228368,-27.3937316830851)) ;
#52826 = CARTESIAN_POINT('',(30.5,36.8752963142798,-28.5219414604302)) ;
#52827 = CARTESIAN_POINT('Origin',(30.5,36.5555620409763,-28.9571080888326)) ;
#52828 = CARTESIAN_POINT('Origin',(2.5,-1.96278056880054E-12,2.0609575629719E-12)) ;
#52829 = CARTESIAN_POINT('',(2.5,32.220213337081,-33.6919348724754)) ;
#52830 = CARTESIAN_POINT('Origin',(2.5,32.6195747449183,-33.3284648380432)) ;
#52831 = CARTESIAN_POINT('',(2.5,30.1394375417177,-35.5654738138977)) ;
#52832 = CARTESIAN_POINT('Origin',(2.5,31.1848319093482,-34.6342645913669)) ;
#52833 = CARTESIAN_POINT('Origin',(2.5,29.736213999915,-35.924654514014)) ;
#52834 = CARTESIAN_POINT('Origin',(30.5,-1.96278056880054E-12,2.0609575629719E-12)) ;
#52835 = CARTESIAN_POINT('',(30.5,30.1394375417177,-35.5654738138977)) ;
#52836 = CARTESIAN_POINT('Origin',(30.5,29.736213999915,-35.924654514014)) ;
#52837 = CARTESIAN_POINT('',(30.5,32.220213337081,-33.6919348724754)) ;
#52838 = CARTESIAN_POINT('Origin',(30.5,31.1848319093482,-34.6342645913669)) ;
#52839 = CARTESIAN_POINT('Origin',(30.5,32.6195747449183,-33.3284648380432)) ;
#52840 = CARTESIAN_POINT('Origin',(30.5,32.6195747449183,-33.3284648380432)) ;
#52841 = CARTESIAN_POINT('',(30.5,32.220213337081,-33.6919348724754)) ;
#52842 = CARTESIAN_POINT('Origin',(30.5,31.1848319093482,-34.6342645913669)) ;
#52843 = CARTESIAN_POINT('',(30.5,30.1394375417177,-35.5654738138977)) ;
#52844 = CARTESIAN_POINT('Origin',(30.5,29.736213999915,-35.924654514014)) ;
#52845 = CARTESIAN_POINT('Origin',(2.5,-2.16745697839284E-12,1.84450098521206E-12)) ;
#52846 = CARTESIAN_POINT('',(2.5,35.5654738138977,-30.1394375417177)) ;
#52847 = CARTESIAN_POINT('Origin',(2.5,35.9246545140139,-29.7362139999149)) ;
#52848 = CARTESIAN_POINT('',(2.5,33.6919348724755,-32.220213337081)) ;
#52849 = CARTESIAN_POINT('Origin',(2.5,34.6342645913669,-31.1848319093482)) ;
#52850 = CARTESIAN_POINT('Origin',(2.5,33.3284648380432,-32.6195747449184)) ;
#52851 = CARTESIAN_POINT('Origin',(30.5,-2.16745697839284E-12,1.84450098521206E-12)) ;
#52852 = CARTESIAN_POINT('',(30.5,33.6919348724755,-32.220213337081)) ;
#52853 = CARTESIAN_POINT('Origin',(30.5,33.3284648380432,-32.6195747449184)) ;
#52854 = CARTESIAN_POINT('',(30.5,35.5654738138977,-30.1394375417177)) ;
#52855 = CARTESIAN_POINT('Origin',(30.5,34.6342645913669,-31.1848319093482)) ;
#52856 = CARTESIAN_POINT('Origin',(30.5,35.9246545140139,-29.7362139999149)) ;
#52857 = CARTESIAN_POINT('Origin',(30.5,35.9246545140139,-29.7362139999149)) ;
#52858 = CARTESIAN_POINT('',(30.5,35.5654738138977,-30.1394375417177)) ;
#52859 = CARTESIAN_POINT('Origin',(30.5,34.6342645913669,-31.1848319093482)) ;
#52860 = CARTESIAN_POINT('',(30.5,33.6919348724755,-32.220213337081)) ;
#52861 = CARTESIAN_POINT('Origin',(30.5,33.3284648380432,-32.6195747449184)) ;
#52862 = CARTESIAN_POINT('Origin',(2.5,-1.73659952455823E-12,2.25483385838873E-12)) ;
#52863 = CARTESIAN_POINT('',(2.5,28.5219414604302,-36.8752963142797)) ;
#52864 = CARTESIAN_POINT('Origin',(2.5,28.9571080888326,-36.5555620409762)) ;
#52865 = CARTESIAN_POINT('',(2.5,26.2567262261701,-38.5210715170554)) ;
#52866 = CARTESIAN_POINT('Origin',(2.5,27.3937316830851,-37.7042370228368)) ;
#52867 = CARTESIAN_POINT('Origin',(2.5,25.8181669785007,-38.8361362505368)) ;
#52868 = CARTESIAN_POINT('Origin',(30.5,-1.73659952455823E-12,2.25483385838873E-12)) ;
#52869 = CARTESIAN_POINT('',(30.5,26.2567262261701,-38.5210715170554)) ;
#52870 = CARTESIAN_POINT('Origin',(30.5,25.8181669785007,-38.8361362505368)) ;
#52871 = CARTESIAN_POINT('',(30.5,28.5219414604302,-36.8752963142797)) ;
#52872 = CARTESIAN_POINT('Origin',(30.5,27.3937316830851,-37.7042370228368)) ;
#52873 = CARTESIAN_POINT('Origin',(30.5,28.9571080888326,-36.5555620409762)) ;
#52874 = CARTESIAN_POINT('Origin',(30.5,28.9571080888326,-36.5555620409762)) ;
#52875 = CARTESIAN_POINT('',(30.5,28.5219414604302,-36.8752963142797)) ;
#52876 = CARTESIAN_POINT('Origin',(30.5,27.3937316830851,-37.7042370228368)) ;
#52877 = CARTESIAN_POINT('',(30.5,26.2567262261701,-38.5210715170554)) ;
#52878 = CARTESIAN_POINT('Origin',(30.5,25.8181669785007,-38.8361362505368)) ;
#52879 = CARTESIAN_POINT('Origin',(2.5,-1.49139193251805E-12,2.42400572219872E-12)) ;
#52880 = CARTESIAN_POINT('',(2.5,24.511177224539,-39.6546442930129)) ;
#52881 = CARTESIAN_POINT('Origin',(2.5,24.9773812968611,-39.3821488564452)) ;
#52882 = CARTESIAN_POINT('',(2.5,22.0863407235154,-41.0546242996198)) ;
#52883 = CARTESIAN_POINT('Origin',(2.5,23.3024999999953,-40.3611139433656)) ;
#52884 = CARTESIAN_POINT('Origin',(2.5,21.6172507168713,-41.3221211513147)) ;
#52885 = CARTESIAN_POINT('Origin',(30.5,-1.49139193251805E-12,2.42400572219872E-12)) ;
#52886 = CARTESIAN_POINT('',(30.5,22.0863407235154,-41.0546242996198)) ;
#52887 = CARTESIAN_POINT('Origin',(30.5,21.6172507168713,-41.3221211513147)) ;
#52888 = CARTESIAN_POINT('',(30.5,24.511177224539,-39.6546442930129)) ;
#52889 = CARTESIAN_POINT('Origin',(30.5,23.3024999999953,-40.3611139433656)) ;
#52890 = CARTESIAN_POINT('Origin',(30.5,24.9773812968611,-39.3821488564452)) ;
#52891 = CARTESIAN_POINT('Origin',(30.5,24.9773812968611,-39.3821488564452)) ;
#52892 = CARTESIAN_POINT('',(30.5,24.511177224539,-39.6546442930129)) ;
#52893 = CARTESIAN_POINT('Origin',(30.5,23.3024999999953,-40.3611139433656)) ;
#52894 = CARTESIAN_POINT('',(30.5,22.0863407235154,-41.0546242996198)) ;
#52895 = CARTESIAN_POINT('Origin',(30.5,21.6172507168713,-41.3221211513147)) ;
#52896 = CARTESIAN_POINT('Origin',(2.5,-1.22984433837137E-12,2.5666196720605E-12)) ;
#52897 = CARTESIAN_POINT('',(2.5,20.2318634016821,-41.9995276906041)) ;
#52898 = CARTESIAN_POINT('Origin',(2.5,20.7239970885482,-41.7772566077985)) ;
#52899 = CARTESIAN_POINT('',(2.5,17.6739726500299,-43.1383740271251)) ;
#52900 = CARTESIAN_POINT('Origin',(2.5,18.9559612505438,-42.5757860534247)) ;
#52901 = CARTESIAN_POINT('Origin',(2.5,17.1794913326873,-43.355372245549)) ;
#52902 = CARTESIAN_POINT('Origin',(30.5,-1.22984433837137E-12,2.5666196720605E-12)) ;
#52903 = CARTESIAN_POINT('',(30.5,17.6739726500299,-43.1383740271251)) ;
#52904 = CARTESIAN_POINT('Origin',(30.5,17.1794913326873,-43.355372245549)) ;
#52905 = CARTESIAN_POINT('',(30.5,20.2318634016821,-41.9995276906041)) ;
#52906 = CARTESIAN_POINT('Origin',(30.5,18.9559612505438,-42.5757860534247)) ;
#52907 = CARTESIAN_POINT('Origin',(30.5,20.7239970885482,-41.7772566077985)) ;
#52908 = CARTESIAN_POINT('Origin',(30.5,20.7239970885482,-41.7772566077985)) ;
#52909 = CARTESIAN_POINT('',(30.5,20.2318634016821,-41.9995276906041)) ;
#52910 = CARTESIAN_POINT('Origin',(30.5,18.9559612505438,-42.5757860534247)) ;
#52911 = CARTESIAN_POINT('',(30.5,17.6739726500299,-43.1383740271251)) ;
#52912 = CARTESIAN_POINT('Origin',(30.5,17.1794913326873,-43.355372245549)) ;
#52913 = CARTESIAN_POINT('Origin',(2.5,-9.54822312292023E-13,2.68111319969549E-12)) ;
#52914 = CARTESIAN_POINT('',(2.5,15.7308850496068,-43.8842554738508)) ;
#52915 = CARTESIAN_POINT('Origin',(2.5,16.2435564313579,-43.7146439933037)) ;
#52916 = CARTESIAN_POINT('',(2.5,13.0679648336741,-44.7494907015041)) ;
#52917 = CARTESIAN_POINT('Origin',(2.5,14.4017370228415,-44.3239889419266)) ;
#52918 = CARTESIAN_POINT('Origin',(2.5,12.5535098464227,-44.9136128087662)) ;
#52919 = CARTESIAN_POINT('Origin',(30.5,-9.54822312292023E-13,2.68111319969549E-12)) ;
#52920 = CARTESIAN_POINT('',(30.5,13.0679648336741,-44.7494907015041)) ;
#52921 = CARTESIAN_POINT('Origin',(30.5,12.5535098464227,-44.9136128087662)) ;
#52922 = CARTESIAN_POINT('',(30.5,15.7308850496068,-43.8842554738508)) ;
#52923 = CARTESIAN_POINT('Origin',(30.5,14.4017370228415,-44.3239889419266)) ;
#52924 = CARTESIAN_POINT('Origin',(30.5,16.2435564313579,-43.7146439933037)) ;
#52925 = CARTESIAN_POINT('Origin',(30.5,16.2435564313579,-43.7146439933037)) ;
#52926 = CARTESIAN_POINT('',(30.5,15.7308850496068,-43.8842554738508)) ;
#52927 = CARTESIAN_POINT('Origin',(30.5,14.4017370228415,-44.3239889419266)) ;
#52928 = CARTESIAN_POINT('',(30.5,13.0679648336741,-44.7494907015041)) ;
#52929 = CARTESIAN_POINT('Origin',(30.5,12.5535098464227,-44.9136128087662)) ;
#52930 = CARTESIAN_POINT('Origin',(2.5,-6.69339053149789E-13,2.76623189005561E-12)) ;
#52931 = CARTESIAN_POINT('',(2.5,11.0575558290286,-45.2881781707551)) ;
#52932 = CARTESIAN_POINT('Origin',(2.5,11.585147970723,-45.173084591341)) ;
#52933 = CARTESIAN_POINT('',(2.5,8.31878165995311,-45.8703225913245)) ;
#52934 = CARTESIAN_POINT('Origin',(2.5,9.68972435055971,-45.5865689321897)) ;
#52935 = CARTESIAN_POINT('Origin',(2.5,7.78998947928984,-45.9797704312729)) ;
#52936 = CARTESIAN_POINT('Origin',(30.5,-6.69339053149789E-13,2.76623189005561E-12)) ;
#52937 = CARTESIAN_POINT('',(30.5,8.31878165995311,-45.8703225913245)) ;
#52938 = CARTESIAN_POINT('Origin',(30.5,7.78998947928984,-45.9797704312729)) ;
#52939 = CARTESIAN_POINT('',(30.5,11.0575558290286,-45.2881781707551)) ;
#52940 = CARTESIAN_POINT('Origin',(30.5,9.68972435055971,-45.5865689321897)) ;
#52941 = CARTESIAN_POINT('Origin',(30.5,11.585147970723,-45.173084591341)) ;
#52942 = CARTESIAN_POINT('Origin',(30.5,11.585147970723,-45.173084591341)) ;
#52943 = CARTESIAN_POINT('',(30.5,11.0575558290286,-45.2881781707551)) ;
#52944 = CARTESIAN_POINT('Origin',(30.5,9.68972435055971,-45.5865689321897)) ;
#52945 = CARTESIAN_POINT('',(30.5,8.31878165995311,-45.8703225913245)) ;
#52946 = CARTESIAN_POINT('Origin',(30.5,7.78998947928984,-45.9797704312729)) ;
#52947 = CARTESIAN_POINT('Origin',(2.5,-3.76522375273045E-13,2.82104316495704E-12)) ;
#52948 = CARTESIAN_POINT('',(2.5,6.26307771284532,-46.19591411046)) ;
#52949 = CARTESIAN_POINT('Origin',(2.5,6.79981020457273,-46.1365994215198)) ;
#52950 = CARTESIAN_POINT('',(2.5,3.47845617354872,-46.4885896278522)) ;
#52951 = CARTESIAN_POINT('Origin',(2.5,4.871549030588,-46.3496929336289)) ;
#52952 = CARTESIAN_POINT('Origin',(2.5,2.94112035726179,-46.5421640670489)) ;
#52953 = CARTESIAN_POINT('Origin',(30.5,-3.76522375273045E-13,2.82104316495704E-12)) ;
#52954 = CARTESIAN_POINT('',(30.5,3.47845617354872,-46.4885896278522)) ;
#52955 = CARTESIAN_POINT('Origin',(30.5,2.94112035726179,-46.5421640670489)) ;
#52956 = CARTESIAN_POINT('',(30.5,6.26307771284532,-46.19591411046)) ;
#52957 = CARTESIAN_POINT('Origin',(30.5,4.871549030588,-46.3496929336289)) ;
#52958 = CARTESIAN_POINT('Origin',(30.5,6.79981020457273,-46.1365994215198)) ;
#52959 = CARTESIAN_POINT('Origin',(30.5,6.79981020457273,-46.1365994215198)) ;
#52960 = CARTESIAN_POINT('',(30.5,6.26307771284532,-46.19591411046)) ;
#52961 = CARTESIAN_POINT('Origin',(30.5,4.871549030588,-46.3496929336289)) ;
#52962 = CARTESIAN_POINT('',(30.5,3.47845617354872,-46.4885896278522)) ;
#52963 = CARTESIAN_POINT('Origin',(30.5,2.94112035726179,-46.5421640670489)) ;
#52964 = CARTESIAN_POINT('Origin',(2.5,-7.95804394604355E-14,2.84494650060196E-12)) ;
#52965 = CARTESIAN_POINT('',(2.5,1.39998000660681,-46.5975179480543)) ;
#52966 = CARTESIAN_POINT('Origin',(2.5,1.93997229486942,-46.5946320137324)) ;
#52967 = CARTESIAN_POINT('',(2.5,-1.39998000660683,-46.5975179480543)) ;
#52968 = CARTESIAN_POINT('Origin',(2.5,-8.56119961113762E-15,-46.6049999999905)) ;
#52969 = CARTESIAN_POINT('Origin',(2.5,-1.93997229486942,-46.5946320137324)) ;
#52970 = CARTESIAN_POINT('Origin',(30.5,-7.95804394604355E-14,2.84494650060196E-12)) ;
#52971 = CARTESIAN_POINT('',(30.5,-1.39998000660683,-46.5975179480543)) ;
#52972 = CARTESIAN_POINT('Origin',(30.5,-1.93997229486942,-46.5946320137324)) ;
#52973 = CARTESIAN_POINT('',(30.5,1.39998000660681,-46.5975179480543)) ;
#52974 = CARTESIAN_POINT('Origin',(30.5,-8.56119961113762E-15,-46.6049999999905)) ;
#52975 = CARTESIAN_POINT('Origin',(30.5,1.93997229486942,-46.5946320137324)) ;
#52976 = CARTESIAN_POINT('Origin',(30.5,1.93997229486942,-46.5946320137324)) ;
#52977 = CARTESIAN_POINT('',(30.5,1.39998000660681,-46.5975179480543)) ;
#52978 = CARTESIAN_POINT('Origin',(30.5,-8.56119961113762E-15,-46.6049999999905)) ;
#52979 = CARTESIAN_POINT('',(30.5,-1.39998000660683,-46.5975179480543)) ;
#52980 = CARTESIAN_POINT('Origin',(30.5,-1.93997229486942,-46.5946320137324)) ;
#52981 = CARTESIAN_POINT('Origin',(2.5,2.18233396300178E-13,2.83768000704297E-12)) ;
#52982 = CARTESIAN_POINT('',(2.5,-3.47845617354871,-46.4885896278521)) ;
#52983 = CARTESIAN_POINT('Origin',(2.5,-2.94112035726177,-46.5421640670489)) ;
#52984 = CARTESIAN_POINT('',(2.5,-6.26307771284532,-46.1959141104601)) ;
#52985 = CARTESIAN_POINT('Origin',(2.5,-4.87154903058799,-46.349692933629)) ;
#52986 = CARTESIAN_POINT('Origin',(2.5,-6.79981020457272,-46.1365994215199)) ;
#52987 = CARTESIAN_POINT('Origin',(30.5,2.18233396300178E-13,2.83768000704297E-12)) ;
#52988 = CARTESIAN_POINT('',(30.5,-6.26307771284532,-46.1959141104601)) ;
#52989 = CARTESIAN_POINT('Origin',(30.5,-6.79981020457272,-46.1365994215199)) ;
#52990 = CARTESIAN_POINT('',(30.5,-3.47845617354871,-46.4885896278521)) ;
#52991 = CARTESIAN_POINT('Origin',(30.5,-4.87154903058799,-46.349692933629)) ;
#52992 = CARTESIAN_POINT('Origin',(30.5,-2.94112035726177,-46.5421640670489)) ;
#52993 = CARTESIAN_POINT('Origin',(30.5,-2.94112035726177,-46.5421640670489)) ;
#52994 = CARTESIAN_POINT('',(30.5,-3.47845617354871,-46.4885896278521)) ;
#52995 = CARTESIAN_POINT('Origin',(30.5,-4.87154903058799,-46.349692933629)) ;
#52996 = CARTESIAN_POINT('',(30.5,-6.26307771284532,-46.1959141104601)) ;
#52997 = CARTESIAN_POINT('Origin',(30.5,-6.79981020457272,-46.1365994215199)) ;
#52998 = CARTESIAN_POINT('Origin',(2.5,5.13656221302656E-13,2.79932329750409E-12)) ;
#52999 = CARTESIAN_POINT('',(2.5,-8.31878165995312,-45.8703225913244)) ;
#53000 = CARTESIAN_POINT('Origin',(2.5,-7.78998947928983,-45.9797704312728)) ;
#53001 = CARTESIAN_POINT('',(2.5,-11.0575558290286,-45.2881781707551)) ;
#53002 = CARTESIAN_POINT('Origin',(2.5,-9.68972435055972,-45.5865689321897)) ;
#53003 = CARTESIAN_POINT('Origin',(2.5,-11.585147970723,-45.173084591341)) ;
#53004 = CARTESIAN_POINT('Origin',(30.5,5.13656221302656E-13,2.79932329750409E-12)) ;
#53005 = CARTESIAN_POINT('',(30.5,-11.0575558290286,-45.2881781707551)) ;
#53006 = CARTESIAN_POINT('Origin',(30.5,-11.585147970723,-45.173084591341)) ;
#53007 = CARTESIAN_POINT('',(30.5,-8.31878165995312,-45.8703225913244)) ;
#53008 = CARTESIAN_POINT('Origin',(30.5,-9.68972435055972,-45.5865689321897)) ;
#53009 = CARTESIAN_POINT('Origin',(30.5,-7.78998947928983,-45.9797704312728)) ;
#53010 = CARTESIAN_POINT('Origin',(30.5,-7.78998947928983,-45.9797704312728)) ;
#53011 = CARTESIAN_POINT('',(30.5,-8.31878165995312,-45.8703225913244)) ;
#53012 = CARTESIAN_POINT('Origin',(30.5,-9.68972435055972,-45.5865689321897)) ;
#53013 = CARTESIAN_POINT('',(30.5,-11.0575558290286,-45.2881781707551)) ;
#53014 = CARTESIAN_POINT('Origin',(30.5,-11.585147970723,-45.173084591341)) ;
#53015 = CARTESIAN_POINT('Origin',(2.5,8.03451321255064E-13,2.73029661612169E-12)) ;
#53016 = CARTESIAN_POINT('',(2.5,-13.0679648336741,-44.7494907015041)) ;
#53017 = CARTESIAN_POINT('Origin',(2.5,-12.5535098464227,-44.9136128087662)) ;
#53018 = CARTESIAN_POINT('',(2.5,-15.7308850496068,-43.8842554738508)) ;
#53019 = CARTESIAN_POINT('Origin',(2.5,-14.4017370228415,-44.3239889419266)) ;
#53020 = CARTESIAN_POINT('Origin',(2.5,-16.2435564313579,-43.7146439933038)) ;
#53021 = CARTESIAN_POINT('Origin',(30.5,8.03451321255064E-13,2.73029661612169E-12)) ;
#53022 = CARTESIAN_POINT('',(30.5,-15.7308850496068,-43.8842554738508)) ;
#53023 = CARTESIAN_POINT('Origin',(30.5,-16.2435564313579,-43.7146439933038)) ;
#53024 = CARTESIAN_POINT('',(30.5,-13.0679648336741,-44.7494907015041)) ;
#53025 = CARTESIAN_POINT('Origin',(30.5,-14.4017370228415,-44.3239889419266)) ;
#53026 = CARTESIAN_POINT('Origin',(30.5,-12.5535098464227,-44.9136128087662)) ;
#53027 = CARTESIAN_POINT('Origin',(30.5,-12.5535098464227,-44.9136128087662)) ;
#53028 = CARTESIAN_POINT('',(30.5,-13.0679648336741,-44.7494907015041)) ;
#53029 = CARTESIAN_POINT('Origin',(30.5,-14.4017370228415,-44.3239889419266)) ;
#53030 = CARTESIAN_POINT('',(30.5,-15.7308850496068,-43.8842554738508)) ;
#53031 = CARTESIAN_POINT('Origin',(30.5,-16.2435564313579,-43.7146439933038)) ;
#53032 = CARTESIAN_POINT('Origin',(2.5,2.5666196720605E-12,1.22984433837137E-12)) ;
#53033 = CARTESIAN_POINT('',(2.5,-41.9995276906041,-20.2318634016821)) ;
#53034 = CARTESIAN_POINT('Origin',(2.5,-41.7772566077985,-20.7239970885482)) ;
#53035 = CARTESIAN_POINT('',(2.5,-43.1383740271251,-17.6739726500298)) ;
#53036 = CARTESIAN_POINT('Origin',(2.5,-42.5757860534248,-18.9559612505438)) ;
#53037 = CARTESIAN_POINT('Origin',(2.5,-43.355372245549,-17.1794913326873)) ;
#53038 = CARTESIAN_POINT('Origin',(30.5,2.5666196720605E-12,1.22984433837137E-12)) ;
#53039 = CARTESIAN_POINT('',(30.5,-43.1383740271251,-17.6739726500298)) ;
#53040 = CARTESIAN_POINT('Origin',(30.5,-43.355372245549,-17.1794913326873)) ;
#53041 = CARTESIAN_POINT('',(30.5,-41.9995276906041,-20.2318634016821)) ;
#53042 = CARTESIAN_POINT('Origin',(30.5,-42.5757860534248,-18.9559612505438)) ;
#53043 = CARTESIAN_POINT('Origin',(30.5,-41.7772566077985,-20.7239970885482)) ;
#53044 = CARTESIAN_POINT('Origin',(30.5,-41.7772566077985,-20.7239970885482)) ;
#53045 = CARTESIAN_POINT('',(30.5,-41.9995276906041,-20.2318634016821)) ;
#53046 = CARTESIAN_POINT('Origin',(30.5,-42.5757860534248,-18.9559612505438)) ;
#53047 = CARTESIAN_POINT('',(30.5,-43.1383740271251,-17.6739726500298)) ;
#53048 = CARTESIAN_POINT('Origin',(30.5,-43.355372245549,-17.1794913326873)) ;
#53049 = CARTESIAN_POINT('Origin',(2.5,2.42400572219872E-12,1.49139193251805E-12)) ;
#53050 = CARTESIAN_POINT('',(2.5,-39.654644293013,-24.5111772245389)) ;
#53051 = CARTESIAN_POINT('Origin',(2.5,-39.3821488564452,-24.9773812968611)) ;
#53052 = CARTESIAN_POINT('',(2.5,-41.0546242996198,-22.0863407235153)) ;
#53053 = CARTESIAN_POINT('Origin',(2.5,-40.3611139433656,-23.3024999999952)) ;
#53054 = CARTESIAN_POINT('Origin',(2.5,-41.3221211513147,-21.6172507168713)) ;
#53055 = CARTESIAN_POINT('Origin',(30.5,2.42400572219872E-12,1.49139193251805E-12)) ;
#53056 = CARTESIAN_POINT('',(30.5,-41.0546242996198,-22.0863407235153)) ;
#53057 = CARTESIAN_POINT('Origin',(30.5,-41.3221211513147,-21.6172507168713)) ;
#53058 = CARTESIAN_POINT('',(30.5,-39.654644293013,-24.5111772245389)) ;
#53059 = CARTESIAN_POINT('Origin',(30.5,-40.3611139433656,-23.3024999999952)) ;
#53060 = CARTESIAN_POINT('Origin',(30.5,-39.3821488564452,-24.9773812968611)) ;
#53061 = CARTESIAN_POINT('Origin',(30.5,-39.3821488564452,-24.9773812968611)) ;
#53062 = CARTESIAN_POINT('',(30.5,-39.654644293013,-24.5111772245389)) ;
#53063 = CARTESIAN_POINT('Origin',(30.5,-40.3611139433656,-23.3024999999952)) ;
#53064 = CARTESIAN_POINT('',(30.5,-41.0546242996198,-22.0863407235153)) ;
#53065 = CARTESIAN_POINT('Origin',(30.5,-41.3221211513147,-21.6172507168713)) ;
#53066 = CARTESIAN_POINT('Origin',(2.5,2.25483385838873E-12,1.73659952455823E-12)) ;
#53067 = CARTESIAN_POINT('',(2.5,-36.8752963142797,-28.5219414604302)) ;
#53068 = CARTESIAN_POINT('Origin',(2.5,-36.5555620409762,-28.9571080888326)) ;
#53069 = CARTESIAN_POINT('',(2.5,-38.5210715170554,-26.2567262261701)) ;
#53070 = CARTESIAN_POINT('Origin',(2.5,-37.7042370228368,-27.3937316830851)) ;
#53071 = CARTESIAN_POINT('Origin',(2.5,-38.8361362505368,-25.8181669785007)) ;
#53072 = CARTESIAN_POINT('Origin',(30.5,2.25483385838873E-12,1.73659952455823E-12)) ;
#53073 = CARTESIAN_POINT('',(30.5,-38.5210715170554,-26.2567262261701)) ;
#53074 = CARTESIAN_POINT('Origin',(30.5,-38.8361362505368,-25.8181669785007)) ;
#53075 = CARTESIAN_POINT('',(30.5,-36.8752963142797,-28.5219414604302)) ;
#53076 = CARTESIAN_POINT('Origin',(30.5,-37.7042370228368,-27.3937316830851)) ;
#53077 = CARTESIAN_POINT('Origin',(30.5,-36.5555620409762,-28.9571080888326)) ;
#53078 = CARTESIAN_POINT('Origin',(30.5,-36.5555620409762,-28.9571080888326)) ;
#53079 = CARTESIAN_POINT('',(30.5,-36.8752963142797,-28.5219414604302)) ;
#53080 = CARTESIAN_POINT('Origin',(30.5,-37.7042370228368,-27.3937316830851)) ;
#53081 = CARTESIAN_POINT('',(30.5,-38.5210715170554,-26.2567262261701)) ;
#53082 = CARTESIAN_POINT('Origin',(30.5,-38.8361362505368,-25.8181669785007)) ;
#53083 = CARTESIAN_POINT('Origin',(2.5,2.0609575629719E-12,1.96278056880054E-12)) ;
#53084 = CARTESIAN_POINT('',(2.5,-33.6919348724754,-32.220213337081)) ;
#53085 = CARTESIAN_POINT('Origin',(2.5,-33.3284648380432,-32.6195747449183)) ;
#53086 = CARTESIAN_POINT('',(2.5,-35.5654738138977,-30.1394375417177)) ;
#53087 = CARTESIAN_POINT('Origin',(2.5,-34.6342645913669,-31.1848319093482)) ;
#53088 = CARTESIAN_POINT('Origin',(2.5,-35.924654514014,-29.7362139999149)) ;
#53089 = CARTESIAN_POINT('Origin',(30.5,2.0609575629719E-12,1.96278056880054E-12)) ;
#53090 = CARTESIAN_POINT('',(30.5,-35.5654738138977,-30.1394375417177)) ;
#53091 = CARTESIAN_POINT('Origin',(30.5,-35.924654514014,-29.7362139999149)) ;
#53092 = CARTESIAN_POINT('',(30.5,-33.6919348724754,-32.220213337081)) ;
#53093 = CARTESIAN_POINT('Origin',(30.5,-34.6342645913669,-31.1848319093482)) ;
#53094 = CARTESIAN_POINT('Origin',(30.5,-33.3284648380432,-32.6195747449183)) ;
#53095 = CARTESIAN_POINT('Origin',(30.5,-33.3284648380432,-32.6195747449183)) ;
#53096 = CARTESIAN_POINT('',(30.5,-33.6919348724754,-32.220213337081)) ;
#53097 = CARTESIAN_POINT('Origin',(30.5,-34.6342645913669,-31.1848319093482)) ;
#53098 = CARTESIAN_POINT('',(30.5,-35.5654738138977,-30.1394375417177)) ;
#53099 = CARTESIAN_POINT('Origin',(30.5,-35.924654514014,-29.7362139999149)) ;
#53100 = CARTESIAN_POINT('Origin',(2.5,1.84450098521206E-12,2.16745697839284E-12)) ;
#53101 = CARTESIAN_POINT('',(2.5,-30.1394375417177,-35.5654738138976)) ;
#53102 = CARTESIAN_POINT('Origin',(2.5,-29.7362139999149,-35.9246545140139)) ;
#53103 = CARTESIAN_POINT('',(2.5,-32.220213337081,-33.6919348724755)) ;
#53104 = CARTESIAN_POINT('Origin',(2.5,-31.1848319093483,-34.6342645913669)) ;
#53105 = CARTESIAN_POINT('Origin',(2.5,-32.6195747449184,-33.3284648380432)) ;
#53106 = CARTESIAN_POINT('Origin',(30.5,1.84450098521206E-12,2.16745697839284E-12)) ;
#53107 = CARTESIAN_POINT('',(30.5,-32.220213337081,-33.6919348724755)) ;
#53108 = CARTESIAN_POINT('Origin',(30.5,-32.6195747449184,-33.3284648380432)) ;
#53109 = CARTESIAN_POINT('',(30.5,-30.1394375417177,-35.5654738138976)) ;
#53110 = CARTESIAN_POINT('Origin',(30.5,-31.1848319093483,-34.6342645913669)) ;
#53111 = CARTESIAN_POINT('Origin',(30.5,-29.7362139999149,-35.9246545140139)) ;
#53112 = CARTESIAN_POINT('Origin',(30.5,-29.7362139999149,-35.9246545140139)) ;
#53113 = CARTESIAN_POINT('',(30.5,-30.1394375417177,-35.5654738138976)) ;
#53114 = CARTESIAN_POINT('Origin',(30.5,-31.1848319093483,-34.6342645913669)) ;
#53115 = CARTESIAN_POINT('',(30.5,-32.220213337081,-33.6919348724755)) ;
#53116 = CARTESIAN_POINT('Origin',(30.5,-32.6195747449184,-33.3284648380432)) ;
#53117 = CARTESIAN_POINT('Origin',(2.5,1.60783566867159E-12,2.34838627576032E-12)) ;
#53118 = CARTESIAN_POINT('',(2.5,-26.2567262261701,-38.5210715170554)) ;
#53119 = CARTESIAN_POINT('Origin',(2.5,-25.8181669785007,-38.8361362505367)) ;
#53120 = CARTESIAN_POINT('',(2.5,-28.5219414604302,-36.8752963142798)) ;
#53121 = CARTESIAN_POINT('Origin',(2.5,-27.3937316830851,-37.7042370228368)) ;
#53122 = CARTESIAN_POINT('Origin',(2.5,-28.9571080888326,-36.5555620409763)) ;
#53123 = CARTESIAN_POINT('Origin',(30.5,1.60783566867159E-12,2.34838627576032E-12)) ;
#53124 = CARTESIAN_POINT('',(30.5,-28.5219414604302,-36.8752963142798)) ;
#53125 = CARTESIAN_POINT('Origin',(30.5,-28.9571080888326,-36.5555620409763)) ;
#53126 = CARTESIAN_POINT('',(30.5,-26.2567262261701,-38.5210715170554)) ;
#53127 = CARTESIAN_POINT('Origin',(30.5,-27.3937316830851,-37.7042370228368)) ;
#53128 = CARTESIAN_POINT('Origin',(30.5,-25.8181669785007,-38.8361362505367)) ;
#53129 = CARTESIAN_POINT('Origin',(30.5,-25.8181669785007,-38.8361362505367)) ;
#53130 = CARTESIAN_POINT('',(30.5,-26.2567262261701,-38.5210715170554)) ;
#53131 = CARTESIAN_POINT('Origin',(30.5,-27.3937316830851,-37.7042370228368)) ;
#53132 = CARTESIAN_POINT('',(30.5,-28.5219414604302,-36.8752963142798)) ;
#53133 = CARTESIAN_POINT('Origin',(30.5,-28.9571080888326,-36.5555620409763)) ;
#53134 = CARTESIAN_POINT('Origin',(2.5,1.35355456808392E-12,2.50358616165916E-12)) ;
#53135 = CARTESIAN_POINT('',(2.5,-22.0863407235154,-41.0546242996198)) ;
#53136 = CARTESIAN_POINT('Origin',(2.5,-21.6172507168713,-41.3221211513146)) ;
#53137 = CARTESIAN_POINT('',(2.5,-24.511177224539,-39.654644293013)) ;
#53138 = CARTESIAN_POINT('Origin',(2.5,-23.3024999999953,-40.3611139433655)) ;
#53139 = CARTESIAN_POINT('Origin',(2.5,-24.9773812968612,-39.3821488564453)) ;
#53140 = CARTESIAN_POINT('Origin',(30.5,1.35355456808392E-12,2.50358616165916E-12)) ;
#53141 = CARTESIAN_POINT('',(30.5,-24.511177224539,-39.654644293013)) ;
#53142 = CARTESIAN_POINT('Origin',(30.5,-24.9773812968612,-39.3821488564453)) ;
#53143 = CARTESIAN_POINT('',(30.5,-22.0863407235154,-41.0546242996198)) ;
#53144 = CARTESIAN_POINT('Origin',(30.5,-23.3024999999953,-40.3611139433655)) ;
#53145 = CARTESIAN_POINT('Origin',(30.5,-21.6172507168713,-41.3221211513146)) ;
#53146 = CARTESIAN_POINT('Origin',(30.5,-21.6172507168713,-41.3221211513146)) ;
#53147 = CARTESIAN_POINT('',(30.5,-22.0863407235154,-41.0546242996198)) ;
#53148 = CARTESIAN_POINT('Origin',(30.5,-23.3024999999953,-40.3611139433655)) ;
#53149 = CARTESIAN_POINT('',(30.5,-24.511177224539,-39.654644293013)) ;
#53150 = CARTESIAN_POINT('Origin',(30.5,-24.9773812968612,-39.3821488564453)) ;
#53151 = CARTESIAN_POINT('Origin',(2.5,1.0844436403988E-12,2.63135623366177E-12)) ;
#53152 = CARTESIAN_POINT('',(2.5,-17.6739726500298,-43.1383740271251)) ;
#53153 = CARTESIAN_POINT('Origin',(2.5,-17.1794913326873,-43.355372245549)) ;
#53154 = CARTESIAN_POINT('',(2.5,-20.2318634016821,-41.9995276906041)) ;
#53155 = CARTESIAN_POINT('Origin',(2.5,-18.9559612505438,-42.5757860534248)) ;
#53156 = CARTESIAN_POINT('Origin',(2.5,-20.7239970885482,-41.7772566077985)) ;
#53157 = CARTESIAN_POINT('Origin',(30.5,1.0844436403988E-12,2.63135623366177E-12)) ;
#53158 = CARTESIAN_POINT('',(30.5,-20.2318634016821,-41.9995276906041)) ;
#53159 = CARTESIAN_POINT('Origin',(30.5,-20.7239970885482,-41.7772566077985)) ;
#53160 = CARTESIAN_POINT('',(30.5,-17.6739726500298,-43.1383740271251)) ;
#53161 = CARTESIAN_POINT('Origin',(30.5,-18.9559612505438,-42.5757860534248)) ;
#53162 = CARTESIAN_POINT('Origin',(30.5,-17.1794913326873,-43.355372245549)) ;
#53163 = CARTESIAN_POINT('Origin',(30.5,-17.1794913326873,-43.355372245549)) ;
#53164 = CARTESIAN_POINT('',(30.5,-17.6739726500298,-43.1383740271251)) ;
#53165 = CARTESIAN_POINT('Origin',(30.5,-18.9559612505438,-42.5757860534248)) ;
#53166 = CARTESIAN_POINT('',(30.5,-20.2318634016821,-41.9995276906041)) ;
#53167 = CARTESIAN_POINT('Origin',(30.5,-20.7239970885482,-41.7772566077985)) ;
#53168 = CARTESIAN_POINT('Origin',(2.5,2.68111319969549E-12,9.54822312292024E-13)) ;
#53169 = CARTESIAN_POINT('',(2.5,-43.8842554738508,-15.7308850496068)) ;
#53170 = CARTESIAN_POINT('Origin',(2.5,-43.7146439933037,-16.2435564313579)) ;
#53171 = CARTESIAN_POINT('',(2.5,-44.7494907015041,-13.0679648336741)) ;
#53172 = CARTESIAN_POINT('Origin',(2.5,-44.3239889419266,-14.4017370228415)) ;
#53173 = CARTESIAN_POINT('Origin',(2.5,-44.9136128087662,-12.5535098464227)) ;
#53174 = CARTESIAN_POINT('Origin',(30.5,2.68111319969549E-12,9.54822312292024E-13)) ;
#53175 = CARTESIAN_POINT('',(30.5,-44.7494907015041,-13.0679648336741)) ;
#53176 = CARTESIAN_POINT('Origin',(30.5,-44.9136128087662,-12.5535098464227)) ;
#53177 = CARTESIAN_POINT('',(30.5,-43.8842554738508,-15.7308850496068)) ;
#53178 = CARTESIAN_POINT('Origin',(30.5,-44.3239889419266,-14.4017370228415)) ;
#53179 = CARTESIAN_POINT('Origin',(30.5,-43.7146439933037,-16.2435564313579)) ;
#53180 = CARTESIAN_POINT('Origin',(30.5,-43.7146439933037,-16.2435564313579)) ;
#53181 = CARTESIAN_POINT('',(30.5,-43.8842554738508,-15.7308850496068)) ;
#53182 = CARTESIAN_POINT('Origin',(30.5,-44.3239889419266,-14.4017370228415)) ;
#53183 = CARTESIAN_POINT('',(30.5,-44.7494907015041,-13.0679648336741)) ;
#53184 = CARTESIAN_POINT('Origin',(30.5,-44.9136128087662,-12.5535098464227)) ;
#53185 = CARTESIAN_POINT('Origin',(2.5,2.76623189005561E-12,6.69339053149788E-13)) ;
#53186 = CARTESIAN_POINT('',(2.5,-45.2881781707551,-11.0575558290286)) ;
#53187 = CARTESIAN_POINT('Origin',(2.5,-45.173084591341,-11.585147970723)) ;
#53188 = CARTESIAN_POINT('',(2.5,-45.8703225913245,-8.31878165995309)) ;
#53189 = CARTESIAN_POINT('Origin',(2.5,-45.5865689321897,-9.68972435055969)) ;
#53190 = CARTESIAN_POINT('Origin',(2.5,-45.9797704312729,-7.78998947928983)) ;
#53191 = CARTESIAN_POINT('Origin',(30.5,2.76623189005561E-12,6.69339053149788E-13)) ;
#53192 = CARTESIAN_POINT('',(30.5,-45.8703225913245,-8.31878165995309)) ;
#53193 = CARTESIAN_POINT('Origin',(30.5,-45.9797704312729,-7.78998947928983)) ;
#53194 = CARTESIAN_POINT('',(30.5,-45.2881781707551,-11.0575558290286)) ;
#53195 = CARTESIAN_POINT('Origin',(30.5,-45.5865689321897,-9.68972435055969)) ;
#53196 = CARTESIAN_POINT('Origin',(30.5,-45.173084591341,-11.585147970723)) ;
#53197 = CARTESIAN_POINT('Origin',(30.5,-45.173084591341,-11.585147970723)) ;
#53198 = CARTESIAN_POINT('',(30.5,-45.2881781707551,-11.0575558290286)) ;
#53199 = CARTESIAN_POINT('Origin',(30.5,-45.5865689321897,-9.68972435055969)) ;
#53200 = CARTESIAN_POINT('',(30.5,-45.8703225913245,-8.31878165995309)) ;
#53201 = CARTESIAN_POINT('Origin',(30.5,-45.9797704312729,-7.78998947928983)) ;
#53202 = CARTESIAN_POINT('Origin',(2.5,2.82104316495704E-12,3.76522375273043E-13)) ;
#53203 = CARTESIAN_POINT('',(2.5,-46.1959141104601,-6.2630777128453)) ;
#53204 = CARTESIAN_POINT('Origin',(2.5,-46.1365994215198,-6.79981020457271)) ;
#53205 = CARTESIAN_POINT('',(2.5,-46.4885896278522,-3.4784561735487)) ;
#53206 = CARTESIAN_POINT('Origin',(2.5,-46.349692933629,-4.87154903058798)) ;
#53207 = CARTESIAN_POINT('Origin',(2.5,-46.5421640670489,-2.94112035726177)) ;
#53208 = CARTESIAN_POINT('Origin',(30.5,2.82104316495704E-12,3.76522375273043E-13)) ;
#53209 = CARTESIAN_POINT('',(30.5,-46.4885896278522,-3.4784561735487)) ;
#53210 = CARTESIAN_POINT('Origin',(30.5,-46.5421640670489,-2.94112035726177)) ;
#53211 = CARTESIAN_POINT('',(30.5,-46.1959141104601,-6.2630777128453)) ;
#53212 = CARTESIAN_POINT('Origin',(30.5,-46.349692933629,-4.87154903058798)) ;
#53213 = CARTESIAN_POINT('Origin',(30.5,-46.1365994215198,-6.79981020457271)) ;
#53214 = CARTESIAN_POINT('Origin',(30.5,-46.1365994215198,-6.79981020457271)) ;
#53215 = CARTESIAN_POINT('',(30.5,-46.1959141104601,-6.2630777128453)) ;
#53216 = CARTESIAN_POINT('Origin',(30.5,-46.349692933629,-4.87154903058798)) ;
#53217 = CARTESIAN_POINT('',(30.5,-46.4885896278522,-3.4784561735487)) ;
#53218 = CARTESIAN_POINT('Origin',(30.5,-46.5421640670489,-2.94112035726177)) ;
#53219 = CARTESIAN_POINT('Origin',(2.5,2.84494650060196E-12,7.95804394604357E-14)) ;
#53220 = CARTESIAN_POINT('',(2.5,-46.5975179480543,-1.39998000660681)) ;
#53221 = CARTESIAN_POINT('Origin',(2.5,-46.5946320137324,-1.93997229486942)) ;
#53222 = CARTESIAN_POINT('',(2.5,-46.5975179480543,1.39998000660682)) ;
#53223 = CARTESIAN_POINT('Origin',(2.5,-46.6049999999905,5.70746640742508E-15)) ;
#53224 = CARTESIAN_POINT('Origin',(2.5,-46.5946320137324,1.93997229486942)) ;
#53225 = CARTESIAN_POINT('Origin',(30.5,2.84494650060196E-12,7.95804394604357E-14)) ;
#53226 = CARTESIAN_POINT('',(30.5,-46.5975179480543,1.39998000660682)) ;
#53227 = CARTESIAN_POINT('Origin',(30.5,-46.5946320137324,1.93997229486942)) ;
#53228 = CARTESIAN_POINT('',(30.5,-46.5975179480543,-1.39998000660681)) ;
#53229 = CARTESIAN_POINT('Origin',(30.5,-46.6049999999905,5.70746640742508E-15)) ;
#53230 = CARTESIAN_POINT('Origin',(30.5,-46.5946320137324,-1.93997229486942)) ;
#53231 = CARTESIAN_POINT('Origin',(30.5,-46.5946320137324,-1.93997229486942)) ;
#53232 = CARTESIAN_POINT('',(30.5,-46.5975179480543,-1.39998000660681)) ;
#53233 = CARTESIAN_POINT('Origin',(30.5,-46.6049999999905,5.70746640742508E-15)) ;
#53234 = CARTESIAN_POINT('',(30.5,-46.5975179480543,1.39998000660682)) ;
#53235 = CARTESIAN_POINT('Origin',(30.5,-46.5946320137324,1.93997229486942)) ;
#53236 = CARTESIAN_POINT('Origin',(2.5,2.83768000704297E-12,-2.18233396300179E-13)) ;
#53237 = CARTESIAN_POINT('',(2.5,-46.4885896278521,3.47845617354873)) ;
#53238 = CARTESIAN_POINT('Origin',(2.5,-46.5421640670489,2.94112035726179)) ;
#53239 = CARTESIAN_POINT('',(2.5,-46.1959141104601,6.26307771284533)) ;
#53240 = CARTESIAN_POINT('Origin',(2.5,-46.3496929336289,4.87154903058801)) ;
#53241 = CARTESIAN_POINT('Origin',(2.5,-46.1365994215199,6.79981020457274)) ;
#53242 = CARTESIAN_POINT('Origin',(30.5,2.83768000704297E-12,-2.18233396300179E-13)) ;
#53243 = CARTESIAN_POINT('',(30.5,-46.1959141104601,6.26307771284533)) ;
#53244 = CARTESIAN_POINT('Origin',(30.5,-46.1365994215199,6.79981020457274)) ;
#53245 = CARTESIAN_POINT('',(30.5,-46.4885896278521,3.47845617354873)) ;
#53246 = CARTESIAN_POINT('Origin',(30.5,-46.3496929336289,4.87154903058801)) ;
#53247 = CARTESIAN_POINT('Origin',(30.5,-46.5421640670489,2.94112035726179)) ;
#53248 = CARTESIAN_POINT('Origin',(30.5,-46.5421640670489,2.94112035726179)) ;
#53249 = CARTESIAN_POINT('',(30.5,-46.4885896278521,3.47845617354873)) ;
#53250 = CARTESIAN_POINT('Origin',(30.5,-46.3496929336289,4.87154903058801)) ;
#53251 = CARTESIAN_POINT('',(30.5,-46.1959141104601,6.26307771284533)) ;
#53252 = CARTESIAN_POINT('Origin',(30.5,-46.1365994215199,6.79981020457274)) ;
#53253 = CARTESIAN_POINT('Origin',(2.5,2.79932329750409E-12,-5.13656221302654E-13)) ;
#53254 = CARTESIAN_POINT('',(2.5,-45.8703225913244,8.3187816599531)) ;
#53255 = CARTESIAN_POINT('Origin',(2.5,-45.9797704312728,7.78998947928981)) ;
#53256 = CARTESIAN_POINT('',(2.5,-45.2881781707551,11.0575558290286)) ;
#53257 = CARTESIAN_POINT('Origin',(2.5,-45.5865689321897,9.6897243505597)) ;
#53258 = CARTESIAN_POINT('Origin',(2.5,-45.1730845913411,11.585147970723)) ;
#53259 = CARTESIAN_POINT('Origin',(30.5,2.79932329750409E-12,-5.13656221302654E-13)) ;
#53260 = CARTESIAN_POINT('',(30.5,-45.2881781707551,11.0575558290286)) ;
#53261 = CARTESIAN_POINT('Origin',(30.5,-45.1730845913411,11.585147970723)) ;
#53262 = CARTESIAN_POINT('',(30.5,-45.8703225913244,8.3187816599531)) ;
#53263 = CARTESIAN_POINT('Origin',(30.5,-45.5865689321897,9.6897243505597)) ;
#53264 = CARTESIAN_POINT('Origin',(30.5,-45.9797704312728,7.78998947928981)) ;
#53265 = CARTESIAN_POINT('Origin',(30.5,-45.9797704312728,7.78998947928981)) ;
#53266 = CARTESIAN_POINT('',(30.5,-45.8703225913244,8.3187816599531)) ;
#53267 = CARTESIAN_POINT('Origin',(30.5,-45.5865689321897,9.6897243505597)) ;
#53268 = CARTESIAN_POINT('',(30.5,-45.2881781707551,11.0575558290286)) ;
#53269 = CARTESIAN_POINT('Origin',(30.5,-45.1730845913411,11.585147970723)) ;
#53270 = CARTESIAN_POINT('Origin',(2.5,2.73029661612169E-12,-8.03451321255064E-13)) ;
#53271 = CARTESIAN_POINT('',(2.5,-44.7494907015041,13.0679648336741)) ;
#53272 = CARTESIAN_POINT('Origin',(2.5,-44.9136128087662,12.5535098464227)) ;
#53273 = CARTESIAN_POINT('',(2.5,-43.8842554738508,15.7308850496068)) ;
#53274 = CARTESIAN_POINT('Origin',(2.5,-44.3239889419266,14.4017370228415)) ;
#53275 = CARTESIAN_POINT('Origin',(2.5,-43.7146439933038,16.2435564313579)) ;
#53276 = CARTESIAN_POINT('Origin',(30.5,2.73029661612169E-12,-8.03451321255064E-13)) ;
#53277 = CARTESIAN_POINT('',(30.5,-43.8842554738508,15.7308850496068)) ;
#53278 = CARTESIAN_POINT('Origin',(30.5,-43.7146439933038,16.2435564313579)) ;
#53279 = CARTESIAN_POINT('',(30.5,-44.7494907015041,13.0679648336741)) ;
#53280 = CARTESIAN_POINT('Origin',(30.5,-44.3239889419266,14.4017370228415)) ;
#53281 = CARTESIAN_POINT('Origin',(30.5,-44.9136128087662,12.5535098464227)) ;
#53282 = CARTESIAN_POINT('Origin',(30.5,-44.9136128087662,12.5535098464227)) ;
#53283 = CARTESIAN_POINT('',(30.5,-44.7494907015041,13.0679648336741)) ;
#53284 = CARTESIAN_POINT('Origin',(30.5,-44.3239889419266,14.4017370228415)) ;
#53285 = CARTESIAN_POINT('',(30.5,-43.8842554738508,15.7308850496068)) ;
#53286 = CARTESIAN_POINT('Origin',(30.5,-43.7146439933038,16.2435564313579)) ;
#53287 = CARTESIAN_POINT('Origin',(2.5,2.63135623366177E-12,-1.08444364039881E-12)) ;
#53288 = CARTESIAN_POINT('',(2.5,-43.1383740271251,17.6739726500298)) ;
#53289 = CARTESIAN_POINT('Origin',(2.5,-43.355372245549,17.1794913326873)) ;
#53290 = CARTESIAN_POINT('',(2.5,-41.9995276906041,20.2318634016821)) ;
#53291 = CARTESIAN_POINT('Origin',(2.5,-42.5757860534247,18.9559612505438)) ;
#53292 = CARTESIAN_POINT('Origin',(2.5,-41.7772566077985,20.7239970885482)) ;
#53293 = CARTESIAN_POINT('Origin',(30.5,2.63135623366177E-12,-1.08444364039881E-12)) ;
#53294 = CARTESIAN_POINT('',(30.5,-41.9995276906041,20.2318634016821)) ;
#53295 = CARTESIAN_POINT('Origin',(30.5,-41.7772566077985,20.7239970885482)) ;
#53296 = CARTESIAN_POINT('',(30.5,-43.1383740271251,17.6739726500298)) ;
#53297 = CARTESIAN_POINT('Origin',(30.5,-42.5757860534247,18.9559612505438)) ;
#53298 = CARTESIAN_POINT('Origin',(30.5,-43.355372245549,17.1794913326873)) ;
#53299 = CARTESIAN_POINT('Origin',(30.5,-43.355372245549,17.1794913326873)) ;
#53300 = CARTESIAN_POINT('',(30.5,-43.1383740271251,17.6739726500298)) ;
#53301 = CARTESIAN_POINT('Origin',(30.5,-42.5757860534247,18.9559612505438)) ;
#53302 = CARTESIAN_POINT('',(30.5,-41.9995276906041,20.2318634016821)) ;
#53303 = CARTESIAN_POINT('Origin',(30.5,-41.7772566077985,20.7239970885482)) ;
#53304 = CARTESIAN_POINT('Origin',(2.5,2.50358616165916E-12,-1.35355456808391E-12)) ;
#53305 = CARTESIAN_POINT('',(2.5,-41.0546242996198,22.0863407235153)) ;
#53306 = CARTESIAN_POINT('Origin',(2.5,-41.3221211513146,21.6172507168713)) ;
#53307 = CARTESIAN_POINT('',(2.5,-39.654644293013,24.511177224539)) ;
#53308 = CARTESIAN_POINT('Origin',(2.5,-40.3611139433656,23.3024999999953)) ;
#53309 = CARTESIAN_POINT('Origin',(2.5,-39.3821488564453,24.9773812968611)) ;
#53310 = CARTESIAN_POINT('Origin',(30.5,2.50358616165916E-12,-1.35355456808391E-12)) ;
#53311 = CARTESIAN_POINT('',(30.5,-39.654644293013,24.511177224539)) ;
#53312 = CARTESIAN_POINT('Origin',(30.5,-39.3821488564453,24.9773812968611)) ;
#53313 = CARTESIAN_POINT('',(30.5,-41.0546242996198,22.0863407235153)) ;
#53314 = CARTESIAN_POINT('Origin',(30.5,-40.3611139433656,23.3024999999953)) ;
#53315 = CARTESIAN_POINT('Origin',(30.5,-41.3221211513146,21.6172507168713)) ;
#53316 = CARTESIAN_POINT('Origin',(30.5,-41.3221211513146,21.6172507168713)) ;
#53317 = CARTESIAN_POINT('',(30.5,-41.0546242996198,22.0863407235153)) ;
#53318 = CARTESIAN_POINT('Origin',(30.5,-40.3611139433656,23.3024999999953)) ;
#53319 = CARTESIAN_POINT('',(30.5,-39.654644293013,24.511177224539)) ;
#53320 = CARTESIAN_POINT('Origin',(30.5,-39.3821488564453,24.9773812968611)) ;
#53321 = CARTESIAN_POINT('Origin',(2.5,2.34838627576032E-12,-1.6078356686716E-12)) ;
#53322 = CARTESIAN_POINT('',(2.5,-38.5210715170553,26.2567262261701)) ;
#53323 = CARTESIAN_POINT('Origin',(2.5,-38.8361362505367,25.8181669785007)) ;
#53324 = CARTESIAN_POINT('',(2.5,-36.8752963142798,28.5219414604302)) ;
#53325 = CARTESIAN_POINT('Origin',(2.5,-37.7042370228367,27.3937316830852)) ;
#53326 = CARTESIAN_POINT('Origin',(2.5,-36.5555620409763,28.9571080888326)) ;
#53327 = CARTESIAN_POINT('Origin',(30.5,2.34838627576032E-12,-1.6078356686716E-12)) ;
#53328 = CARTESIAN_POINT('',(30.5,-36.8752963142798,28.5219414604302)) ;
#53329 = CARTESIAN_POINT('Origin',(30.5,-36.5555620409763,28.9571080888326)) ;
#53330 = CARTESIAN_POINT('',(30.5,-38.5210715170553,26.2567262261701)) ;
#53331 = CARTESIAN_POINT('Origin',(30.5,-37.7042370228367,27.3937316830852)) ;
#53332 = CARTESIAN_POINT('Origin',(30.5,-38.8361362505367,25.8181669785007)) ;
#53333 = CARTESIAN_POINT('Origin',(30.5,-38.8361362505367,25.8181669785007)) ;
#53334 = CARTESIAN_POINT('',(30.5,-38.5210715170553,26.2567262261701)) ;
#53335 = CARTESIAN_POINT('Origin',(30.5,-37.7042370228367,27.3937316830852)) ;
#53336 = CARTESIAN_POINT('',(30.5,-36.8752963142798,28.5219414604302)) ;
#53337 = CARTESIAN_POINT('Origin',(30.5,-36.5555620409763,28.9571080888326)) ;
#53338 = CARTESIAN_POINT('Origin',(2.5,1.96278056880054E-12,-2.06095756297191E-12)) ;
#53339 = CARTESIAN_POINT('',(2.5,-32.220213337081,33.6919348724755)) ;
#53340 = CARTESIAN_POINT('Origin',(2.5,-32.6195747449183,33.3284648380432)) ;
#53341 = CARTESIAN_POINT('',(2.5,-30.1394375417177,35.5654738138977)) ;
#53342 = CARTESIAN_POINT('Origin',(2.5,-31.1848319093482,34.6342645913669)) ;
#53343 = CARTESIAN_POINT('Origin',(2.5,-29.7362139999149,35.924654514014)) ;
#53344 = CARTESIAN_POINT('Origin',(30.5,1.96278056880054E-12,-2.06095756297191E-12)) ;
#53345 = CARTESIAN_POINT('',(30.5,-30.1394375417177,35.5654738138977)) ;
#53346 = CARTESIAN_POINT('Origin',(30.5,-29.7362139999149,35.924654514014)) ;
#53347 = CARTESIAN_POINT('',(30.5,-32.220213337081,33.6919348724755)) ;
#53348 = CARTESIAN_POINT('Origin',(30.5,-31.1848319093482,34.6342645913669)) ;
#53349 = CARTESIAN_POINT('Origin',(30.5,-32.6195747449183,33.3284648380432)) ;
#53350 = CARTESIAN_POINT('Origin',(30.5,-32.6195747449183,33.3284648380432)) ;
#53351 = CARTESIAN_POINT('',(30.5,-32.220213337081,33.6919348724755)) ;
#53352 = CARTESIAN_POINT('Origin',(30.5,-31.1848319093482,34.6342645913669)) ;
#53353 = CARTESIAN_POINT('',(30.5,-30.1394375417177,35.5654738138977)) ;
#53354 = CARTESIAN_POINT('Origin',(30.5,-29.7362139999149,35.924654514014)) ;
#53355 = CARTESIAN_POINT('Origin',(2.5,2.16745697839284E-12,-1.84450098521206E-12)) ;
#53356 = CARTESIAN_POINT('',(2.5,-35.5654738138976,30.1394375417177)) ;
#53357 = CARTESIAN_POINT('Origin',(2.5,-35.9246545140139,29.7362139999149)) ;
#53358 = CARTESIAN_POINT('',(2.5,-33.6919348724755,32.220213337081)) ;
#53359 = CARTESIAN_POINT('Origin',(2.5,-34.6342645913669,31.1848319093482)) ;
#53360 = CARTESIAN_POINT('Origin',(2.5,-33.3284648380432,32.6195747449184)) ;
#53361 = CARTESIAN_POINT('Origin',(30.5,2.16745697839284E-12,-1.84450098521206E-12)) ;
#53362 = CARTESIAN_POINT('',(30.5,-33.6919348724755,32.220213337081)) ;
#53363 = CARTESIAN_POINT('Origin',(30.5,-33.3284648380432,32.6195747449184)) ;
#53364 = CARTESIAN_POINT('',(30.5,-35.5654738138976,30.1394375417177)) ;
#53365 = CARTESIAN_POINT('Origin',(30.5,-34.6342645913669,31.1848319093482)) ;
#53366 = CARTESIAN_POINT('Origin',(30.5,-35.9246545140139,29.7362139999149)) ;
#53367 = CARTESIAN_POINT('Origin',(30.5,-35.9246545140139,29.7362139999149)) ;
#53368 = CARTESIAN_POINT('',(30.5,-35.5654738138976,30.1394375417177)) ;
#53369 = CARTESIAN_POINT('Origin',(30.5,-34.6342645913669,31.1848319093482)) ;
#53370 = CARTESIAN_POINT('',(30.5,-33.6919348724755,32.220213337081)) ;
#53371 = CARTESIAN_POINT('Origin',(30.5,-33.3284648380432,32.6195747449184)) ;
#53372 = CARTESIAN_POINT('Origin',(2.5,1.73659952455823E-12,-2.25483385838873E-12)) ;
#53373 = CARTESIAN_POINT('',(2.5,-28.5219414604302,36.8752963142798)) ;
#53374 = CARTESIAN_POINT('Origin',(2.5,-28.9571080888325,36.5555620409762)) ;
#53375 = CARTESIAN_POINT('',(2.5,-26.2567262261701,38.5210715170554)) ;
#53376 = CARTESIAN_POINT('Origin',(2.5,-27.3937316830851,37.7042370228368)) ;
#53377 = CARTESIAN_POINT('Origin',(2.5,-25.8181669785007,38.8361362505368)) ;
#53378 = CARTESIAN_POINT('Origin',(30.5,1.73659952455823E-12,-2.25483385838873E-12)) ;
#53379 = CARTESIAN_POINT('',(30.5,-26.2567262261701,38.5210715170554)) ;
#53380 = CARTESIAN_POINT('Origin',(30.5,-25.8181669785007,38.8361362505368)) ;
#53381 = CARTESIAN_POINT('',(30.5,-28.5219414604302,36.8752963142798)) ;
#53382 = CARTESIAN_POINT('Origin',(30.5,-27.3937316830851,37.7042370228368)) ;
#53383 = CARTESIAN_POINT('Origin',(30.5,-28.9571080888325,36.5555620409762)) ;
#53384 = CARTESIAN_POINT('Origin',(30.5,-28.9571080888325,36.5555620409762)) ;
#53385 = CARTESIAN_POINT('',(30.5,-28.5219414604302,36.8752963142798)) ;
#53386 = CARTESIAN_POINT('Origin',(30.5,-27.3937316830851,37.7042370228368)) ;
#53387 = CARTESIAN_POINT('',(30.5,-26.2567262261701,38.5210715170554)) ;
#53388 = CARTESIAN_POINT('Origin',(30.5,-25.8181669785007,38.8361362505368)) ;
#53389 = CARTESIAN_POINT('Origin',(2.5,1.49139193251805E-12,-2.42400572219872E-12)) ;
#53390 = CARTESIAN_POINT('',(2.5,-24.5111772245389,39.654644293013)) ;
#53391 = CARTESIAN_POINT('Origin',(2.5,-24.9773812968611,39.3821488564452)) ;
#53392 = CARTESIAN_POINT('',(2.5,-22.0863407235153,41.0546242996198)) ;
#53393 = CARTESIAN_POINT('Origin',(2.5,-23.3024999999952,40.3611139433656)) ;
#53394 = CARTESIAN_POINT('Origin',(2.5,-21.6172507168713,41.3221211513147)) ;
#53395 = CARTESIAN_POINT('Origin',(30.5,1.49139193251805E-12,-2.42400572219872E-12)) ;
#53396 = CARTESIAN_POINT('',(30.5,-22.0863407235153,41.0546242996198)) ;
#53397 = CARTESIAN_POINT('Origin',(30.5,-21.6172507168713,41.3221211513147)) ;
#53398 = CARTESIAN_POINT('',(30.5,-24.5111772245389,39.654644293013)) ;
#53399 = CARTESIAN_POINT('Origin',(30.5,-23.3024999999952,40.3611139433656)) ;
#53400 = CARTESIAN_POINT('Origin',(30.5,-24.9773812968611,39.3821488564452)) ;
#53401 = CARTESIAN_POINT('Origin',(30.5,-24.9773812968611,39.3821488564452)) ;
#53402 = CARTESIAN_POINT('',(30.5,-24.5111772245389,39.654644293013)) ;
#53403 = CARTESIAN_POINT('Origin',(30.5,-23.3024999999952,40.3611139433656)) ;
#53404 = CARTESIAN_POINT('',(30.5,-22.0863407235153,41.0546242996198)) ;
#53405 = CARTESIAN_POINT('Origin',(30.5,-21.6172507168713,41.3221211513147)) ;
#53406 = CARTESIAN_POINT('Origin',(2.5,1.22984433837137E-12,-2.5666196720605E-12)) ;
#53407 = CARTESIAN_POINT('',(2.5,-20.2318634016821,41.9995276906041)) ;
#53408 = CARTESIAN_POINT('Origin',(2.5,-20.7239970885482,41.7772566077985)) ;
#53409 = CARTESIAN_POINT('',(2.5,-17.6739726500298,43.1383740271251)) ;
#53410 = CARTESIAN_POINT('Origin',(2.5,-18.9559612505438,42.5757860534248)) ;
#53411 = CARTESIAN_POINT('Origin',(2.5,-17.1794913326873,43.355372245549)) ;
#53412 = CARTESIAN_POINT('Origin',(30.5,1.22984433837137E-12,-2.5666196720605E-12)) ;
#53413 = CARTESIAN_POINT('',(30.5,-17.6739726500298,43.1383740271251)) ;
#53414 = CARTESIAN_POINT('Origin',(30.5,-17.1794913326873,43.355372245549)) ;
#53415 = CARTESIAN_POINT('',(30.5,-20.2318634016821,41.9995276906041)) ;
#53416 = CARTESIAN_POINT('Origin',(30.5,-18.9559612505438,42.5757860534248)) ;
#53417 = CARTESIAN_POINT('Origin',(30.5,-20.7239970885482,41.7772566077985)) ;
#53418 = CARTESIAN_POINT('Origin',(30.5,-20.7239970885482,41.7772566077985)) ;
#53419 = CARTESIAN_POINT('',(30.5,-20.2318634016821,41.9995276906041)) ;
#53420 = CARTESIAN_POINT('Origin',(30.5,-18.9559612505438,42.5757860534248)) ;
#53421 = CARTESIAN_POINT('',(30.5,-17.6739726500298,43.1383740271251)) ;
#53422 = CARTESIAN_POINT('Origin',(30.5,-17.1794913326873,43.355372245549)) ;
#53423 = CARTESIAN_POINT('Origin',(2.5,9.54822312292022E-13,-2.68111319969549E-12)) ;
#53424 = CARTESIAN_POINT('',(2.5,-15.7308850496067,43.8842554738508)) ;
#53425 = CARTESIAN_POINT('Origin',(2.5,-16.2435564313579,43.7146439933037)) ;
#53426 = CARTESIAN_POINT('',(2.5,-13.067964833674,44.7494907015041)) ;
#53427 = CARTESIAN_POINT('Origin',(2.5,-14.4017370228415,44.3239889419266)) ;
#53428 = CARTESIAN_POINT('Origin',(2.5,-12.5535098464227,44.9136128087662)) ;
#53429 = CARTESIAN_POINT('Origin',(30.5,9.54822312292022E-13,-2.68111319969549E-12)) ;
#53430 = CARTESIAN_POINT('',(30.5,-13.067964833674,44.7494907015041)) ;
#53431 = CARTESIAN_POINT('Origin',(30.5,-12.5535098464227,44.9136128087662)) ;
#53432 = CARTESIAN_POINT('',(30.5,-15.7308850496067,43.8842554738508)) ;
#53433 = CARTESIAN_POINT('Origin',(30.5,-14.4017370228415,44.3239889419266)) ;
#53434 = CARTESIAN_POINT('Origin',(30.5,-16.2435564313579,43.7146439933037)) ;
#53435 = CARTESIAN_POINT('Origin',(30.5,-16.2435564313579,43.7146439933037)) ;
#53436 = CARTESIAN_POINT('',(30.5,-15.7308850496067,43.8842554738508)) ;
#53437 = CARTESIAN_POINT('Origin',(30.5,-14.4017370228415,44.3239889419266)) ;
#53438 = CARTESIAN_POINT('',(30.5,-13.067964833674,44.7494907015041)) ;
#53439 = CARTESIAN_POINT('Origin',(30.5,-12.5535098464227,44.9136128087662)) ;
#53440 = CARTESIAN_POINT('Origin',(2.5,6.69339053149789E-13,-2.76623189005561E-12)) ;
#53441 = CARTESIAN_POINT('',(2.5,-11.0575558290286,45.2881781707551)) ;
#53442 = CARTESIAN_POINT('Origin',(2.5,-11.585147970723,45.173084591341)) ;
#53443 = CARTESIAN_POINT('',(2.5,-8.3187816599531,45.8703225913245)) ;
#53444 = CARTESIAN_POINT('Origin',(2.5,-9.68972435055969,45.5865689321897)) ;
#53445 = CARTESIAN_POINT('Origin',(2.5,-7.78998947928983,45.9797704312729)) ;
#53446 = CARTESIAN_POINT('Origin',(30.5,6.69339053149789E-13,-2.76623189005561E-12)) ;
#53447 = CARTESIAN_POINT('',(30.5,-8.3187816599531,45.8703225913245)) ;
#53448 = CARTESIAN_POINT('Origin',(30.5,-7.78998947928983,45.9797704312729)) ;
#53449 = CARTESIAN_POINT('',(30.5,-11.0575558290286,45.2881781707551)) ;
#53450 = CARTESIAN_POINT('Origin',(30.5,-9.68972435055969,45.5865689321897)) ;
#53451 = CARTESIAN_POINT('Origin',(30.5,-11.585147970723,45.173084591341)) ;
#53452 = CARTESIAN_POINT('Origin',(30.5,-11.585147970723,45.173084591341)) ;
#53453 = CARTESIAN_POINT('',(30.5,-11.0575558290286,45.2881781707551)) ;
#53454 = CARTESIAN_POINT('Origin',(30.5,-9.68972435055969,45.5865689321897)) ;
#53455 = CARTESIAN_POINT('',(30.5,-8.3187816599531,45.8703225913245)) ;
#53456 = CARTESIAN_POINT('Origin',(30.5,-7.78998947928983,45.9797704312729)) ;
#53457 = CARTESIAN_POINT('Origin',(2.5,3.76522375273042E-13,-2.82104316495704E-12)) ;
#53458 = CARTESIAN_POINT('',(2.5,-6.26307771284528,46.1959141104601)) ;
#53459 = CARTESIAN_POINT('Origin',(2.5,-6.7998102045727,46.1365994215198)) ;
#53460 = CARTESIAN_POINT('',(2.5,-3.47845617354868,46.4885896278522)) ;
#53461 = CARTESIAN_POINT('Origin',(2.5,-4.87154903058796,46.349692933629)) ;
#53462 = CARTESIAN_POINT('Origin',(2.5,-2.94112035726176,46.5421640670489)) ;
#53463 = CARTESIAN_POINT('Origin',(30.5,3.76522375273042E-13,-2.82104316495704E-12)) ;
#53464 = CARTESIAN_POINT('',(30.5,-3.47845617354868,46.4885896278522)) ;
#53465 = CARTESIAN_POINT('Origin',(30.5,-2.94112035726176,46.5421640670489)) ;
#53466 = CARTESIAN_POINT('',(30.5,-6.26307771284528,46.1959141104601)) ;
#53467 = CARTESIAN_POINT('Origin',(30.5,-4.87154903058796,46.349692933629)) ;
#53468 = CARTESIAN_POINT('Origin',(30.5,-6.7998102045727,46.1365994215198)) ;
#53469 = CARTESIAN_POINT('Origin',(30.5,-6.7998102045727,46.1365994215198)) ;
#53470 = CARTESIAN_POINT('',(30.5,-6.26307771284528,46.1959141104601)) ;
#53471 = CARTESIAN_POINT('Origin',(30.5,-4.87154903058796,46.349692933629)) ;
#53472 = CARTESIAN_POINT('',(30.5,-3.47845617354868,46.4885896278522)) ;
#53473 = CARTESIAN_POINT('Origin',(30.5,-2.94112035726176,46.5421640670489)) ;
#53474 = CARTESIAN_POINT('Origin',(2.5,7.95804394604358E-14,-2.84494650060196E-12)) ;
#53475 = CARTESIAN_POINT('',(2.5,-1.39998000660682,46.5975179480543)) ;
#53476 = CARTESIAN_POINT('Origin',(2.5,-1.93997229486942,46.5946320137324)) ;
#53477 = CARTESIAN_POINT('',(2.5,1.39998000660682,46.5975179480543)) ;
#53478 = CARTESIAN_POINT('Origin',(2.5,2.85373320371254E-15,46.6049999999905)) ;
#53479 = CARTESIAN_POINT('Origin',(2.5,1.93997229486942,46.5946320137324)) ;
#53480 = CARTESIAN_POINT('Origin',(30.5,7.95804394604358E-14,-2.84494650060196E-12)) ;
#53481 = CARTESIAN_POINT('',(30.5,1.39998000660682,46.5975179480543)) ;
#53482 = CARTESIAN_POINT('Origin',(30.5,1.93997229486942,46.5946320137324)) ;
#53483 = CARTESIAN_POINT('',(30.5,-1.39998000660682,46.5975179480543)) ;
#53484 = CARTESIAN_POINT('Origin',(30.5,2.85373320371254E-15,46.6049999999905)) ;
#53485 = CARTESIAN_POINT('Origin',(30.5,-1.93997229486942,46.5946320137324)) ;
#53486 = CARTESIAN_POINT('Origin',(30.5,-1.93997229486942,46.5946320137324)) ;
#53487 = CARTESIAN_POINT('',(30.5,-1.39998000660682,46.5975179480543)) ;
#53488 = CARTESIAN_POINT('Origin',(30.5,2.85373320371254E-15,46.6049999999905)) ;
#53489 = CARTESIAN_POINT('',(30.5,1.39998000660682,46.5975179480543)) ;
#53490 = CARTESIAN_POINT('Origin',(30.5,1.93997229486942,46.5946320137324)) ;
#53491 = CARTESIAN_POINT('Origin',(2.5,-2.18233396300179E-13,-2.83768000704297E-12)) ;
#53492 = CARTESIAN_POINT('',(2.5,3.47845617354871,46.4885896278521)) ;
#53493 = CARTESIAN_POINT('Origin',(2.5,2.94112035726178,46.5421640670489)) ;
#53494 = CARTESIAN_POINT('',(2.5,6.26307771284532,46.1959141104601)) ;
#53495 = CARTESIAN_POINT('Origin',(2.5,4.871549030588,46.3496929336289)) ;
#53496 = CARTESIAN_POINT('Origin',(2.5,6.79981020457273,46.1365994215199)) ;
#53497 = CARTESIAN_POINT('Origin',(30.5,-2.18233396300179E-13,-2.83768000704297E-12)) ;
#53498 = CARTESIAN_POINT('',(30.5,6.26307771284532,46.1959141104601)) ;
#53499 = CARTESIAN_POINT('Origin',(30.5,6.79981020457273,46.1365994215199)) ;
#53500 = CARTESIAN_POINT('',(30.5,3.47845617354871,46.4885896278521)) ;
#53501 = CARTESIAN_POINT('Origin',(30.5,4.871549030588,46.3496929336289)) ;
#53502 = CARTESIAN_POINT('Origin',(30.5,2.94112035726178,46.5421640670489)) ;
#53503 = CARTESIAN_POINT('Origin',(30.5,2.94112035726178,46.5421640670489)) ;
#53504 = CARTESIAN_POINT('',(30.5,3.47845617354871,46.4885896278521)) ;
#53505 = CARTESIAN_POINT('Origin',(30.5,4.871549030588,46.3496929336289)) ;
#53506 = CARTESIAN_POINT('',(30.5,6.26307771284532,46.1959141104601)) ;
#53507 = CARTESIAN_POINT('Origin',(30.5,6.79981020457273,46.1365994215199)) ;
#53508 = CARTESIAN_POINT('Origin',(2.5,-5.13656221302655E-13,-2.79932329750409E-12)) ;
#53509 = CARTESIAN_POINT('',(2.5,8.31878165995311,45.8703225913244)) ;
#53510 = CARTESIAN_POINT('Origin',(2.5,7.78998947928982,45.9797704312728)) ;
#53511 = CARTESIAN_POINT('',(2.5,11.0575558290286,45.2881781707551)) ;
#53512 = CARTESIAN_POINT('Origin',(2.5,9.68972435055971,45.5865689321897)) ;
#53513 = CARTESIAN_POINT('Origin',(2.5,11.585147970723,45.173084591341)) ;
#53514 = CARTESIAN_POINT('Origin',(30.5,-5.13656221302655E-13,-2.79932329750409E-12)) ;
#53515 = CARTESIAN_POINT('',(30.5,11.0575558290286,45.2881781707551)) ;
#53516 = CARTESIAN_POINT('Origin',(30.5,11.585147970723,45.173084591341)) ;
#53517 = CARTESIAN_POINT('',(30.5,8.31878165995311,45.8703225913244)) ;
#53518 = CARTESIAN_POINT('Origin',(30.5,9.68972435055971,45.5865689321897)) ;
#53519 = CARTESIAN_POINT('Origin',(30.5,7.78998947928982,45.9797704312728)) ;
#53520 = CARTESIAN_POINT('Origin',(30.5,7.78998947928982,45.9797704312728)) ;
#53521 = CARTESIAN_POINT('',(30.5,8.31878165995311,45.8703225913244)) ;
#53522 = CARTESIAN_POINT('Origin',(30.5,9.68972435055971,45.5865689321897)) ;
#53523 = CARTESIAN_POINT('',(30.5,11.0575558290286,45.2881781707551)) ;
#53524 = CARTESIAN_POINT('Origin',(30.5,11.585147970723,45.173084591341)) ;
#53525 = CARTESIAN_POINT('Origin',(2.5,-8.03451321255064E-13,-2.73029661612169E-12)) ;
#53526 = CARTESIAN_POINT('',(2.5,13.0679648336741,44.7494907015041)) ;
#53527 = CARTESIAN_POINT('Origin',(2.5,12.5535098464227,44.9136128087662)) ;
#53528 = CARTESIAN_POINT('',(2.5,15.7308850496068,43.8842554738508)) ;
#53529 = CARTESIAN_POINT('Origin',(2.5,14.4017370228415,44.3239889419266)) ;
#53530 = CARTESIAN_POINT('Origin',(2.5,16.2435564313579,43.7146439933038)) ;
#53531 = CARTESIAN_POINT('Origin',(30.5,-8.03451321255064E-13,-2.73029661612169E-12)) ;
#53532 = CARTESIAN_POINT('',(30.5,15.7308850496068,43.8842554738508)) ;
#53533 = CARTESIAN_POINT('Origin',(30.5,16.2435564313579,43.7146439933038)) ;
#53534 = CARTESIAN_POINT('',(30.5,13.0679648336741,44.7494907015041)) ;
#53535 = CARTESIAN_POINT('Origin',(30.5,14.4017370228415,44.3239889419266)) ;
#53536 = CARTESIAN_POINT('Origin',(30.5,12.5535098464227,44.9136128087662)) ;
#53537 = CARTESIAN_POINT('Origin',(30.5,12.5535098464227,44.9136128087662)) ;
#53538 = CARTESIAN_POINT('',(30.5,13.0679648336741,44.7494907015041)) ;
#53539 = CARTESIAN_POINT('Origin',(30.5,14.4017370228415,44.3239889419266)) ;
#53540 = CARTESIAN_POINT('',(30.5,15.7308850496068,43.8842554738508)) ;
#53541 = CARTESIAN_POINT('Origin',(30.5,16.2435564313579,43.7146439933038)) ;
#53542 = CARTESIAN_POINT('Origin',(2.5,-1.0844436403988E-12,-2.63135623366177E-12)) ;
#53543 = CARTESIAN_POINT('',(2.5,17.6739726500298,43.1383740271251)) ;
#53544 = CARTESIAN_POINT('Origin',(2.5,17.1794913326873,43.355372245549)) ;
#53545 = CARTESIAN_POINT('',(2.5,20.2318634016821,41.9995276906041)) ;
#53546 = CARTESIAN_POINT('Origin',(2.5,18.9559612505438,42.5757860534247)) ;
#53547 = CARTESIAN_POINT('Origin',(2.5,20.7239970885482,41.7772566077985)) ;
#53548 = CARTESIAN_POINT('Origin',(30.5,-1.0844436403988E-12,-2.63135623366177E-12)) ;
#53549 = CARTESIAN_POINT('',(30.5,20.2318634016821,41.9995276906041)) ;
#53550 = CARTESIAN_POINT('Origin',(30.5,20.7239970885482,41.7772566077985)) ;
#53551 = CARTESIAN_POINT('',(30.5,17.6739726500298,43.1383740271251)) ;
#53552 = CARTESIAN_POINT('Origin',(30.5,18.9559612505438,42.5757860534247)) ;
#53553 = CARTESIAN_POINT('Origin',(30.5,17.1794913326873,43.355372245549)) ;
#53554 = CARTESIAN_POINT('Origin',(30.5,17.1794913326873,43.355372245549)) ;
#53555 = CARTESIAN_POINT('',(30.5,17.6739726500298,43.1383740271251)) ;
#53556 = CARTESIAN_POINT('Origin',(30.5,18.9559612505438,42.5757860534247)) ;
#53557 = CARTESIAN_POINT('',(30.5,20.2318634016821,41.9995276906041)) ;
#53558 = CARTESIAN_POINT('Origin',(30.5,20.7239970885482,41.7772566077985)) ;
#53559 = CARTESIAN_POINT('Origin',(2.5,-1.35355456808391E-12,-2.50358616165916E-12)) ;
#53560 = CARTESIAN_POINT('',(2.5,22.0863407235153,41.0546242996198)) ;
#53561 = CARTESIAN_POINT('Origin',(2.5,21.6172507168712,41.3221211513146)) ;
#53562 = CARTESIAN_POINT('',(2.5,24.511177224539,39.654644293013)) ;
#53563 = CARTESIAN_POINT('Origin',(2.5,23.3024999999952,40.3611139433656)) ;
#53564 = CARTESIAN_POINT('Origin',(2.5,24.9773812968611,39.3821488564453)) ;
#53565 = CARTESIAN_POINT('Origin',(30.5,-1.35355456808391E-12,-2.50358616165916E-12)) ;
#53566 = CARTESIAN_POINT('',(30.5,24.511177224539,39.654644293013)) ;
#53567 = CARTESIAN_POINT('Origin',(30.5,24.9773812968611,39.3821488564453)) ;
#53568 = CARTESIAN_POINT('',(30.5,22.0863407235153,41.0546242996198)) ;
#53569 = CARTESIAN_POINT('Origin',(30.5,23.3024999999952,40.3611139433656)) ;
#53570 = CARTESIAN_POINT('Origin',(30.5,21.6172507168712,41.3221211513146)) ;
#53571 = CARTESIAN_POINT('Origin',(30.5,21.6172507168712,41.3221211513146)) ;
#53572 = CARTESIAN_POINT('',(30.5,22.0863407235153,41.0546242996198)) ;
#53573 = CARTESIAN_POINT('Origin',(30.5,23.3024999999952,40.3611139433656)) ;
#53574 = CARTESIAN_POINT('',(30.5,24.511177224539,39.654644293013)) ;
#53575 = CARTESIAN_POINT('Origin',(30.5,24.9773812968611,39.3821488564453)) ;
#53576 = CARTESIAN_POINT('Origin',(2.5,-2.25483385838873E-12,-1.73659952455823E-12)) ;
#53577 = CARTESIAN_POINT('',(2.5,36.8752963142797,28.5219414604302)) ;
#53578 = CARTESIAN_POINT('Origin',(2.5,36.5555620409762,28.9571080888326)) ;
#53579 = CARTESIAN_POINT('',(2.5,38.5210715170554,26.2567262261701)) ;
#53580 = CARTESIAN_POINT('Origin',(2.5,37.7042370228368,27.3937316830851)) ;
#53581 = CARTESIAN_POINT('Origin',(2.5,38.8361362505368,25.8181669785007)) ;
#53582 = CARTESIAN_POINT('Origin',(30.5,-2.25483385838873E-12,-1.73659952455823E-12)) ;
#53583 = CARTESIAN_POINT('',(30.5,38.5210715170554,26.2567262261701)) ;
#53584 = CARTESIAN_POINT('Origin',(30.5,38.8361362505368,25.8181669785007)) ;
#53585 = CARTESIAN_POINT('',(30.5,36.8752963142797,28.5219414604302)) ;
#53586 = CARTESIAN_POINT('Origin',(30.5,37.7042370228368,27.3937316830851)) ;
#53587 = CARTESIAN_POINT('Origin',(30.5,36.5555620409762,28.9571080888326)) ;
#53588 = CARTESIAN_POINT('Origin',(30.5,36.5555620409762,28.9571080888326)) ;
#53589 = CARTESIAN_POINT('',(30.5,36.8752963142797,28.5219414604302)) ;
#53590 = CARTESIAN_POINT('Origin',(30.5,37.7042370228368,27.3937316830851)) ;
#53591 = CARTESIAN_POINT('',(30.5,38.5210715170554,26.2567262261701)) ;
#53592 = CARTESIAN_POINT('Origin',(30.5,38.8361362505368,25.8181669785007)) ;
#53593 = CARTESIAN_POINT('Origin',(2.5,-2.0609575629719E-12,-1.96278056880054E-12)) ;
#53594 = CARTESIAN_POINT('',(2.5,33.6919348724754,32.220213337081)) ;
#53595 = CARTESIAN_POINT('Origin',(2.5,33.3284648380432,32.6195747449183)) ;
#53596 = CARTESIAN_POINT('',(2.5,35.5654738138977,30.1394375417177)) ;
#53597 = CARTESIAN_POINT('Origin',(2.5,34.6342645913669,31.1848319093482)) ;
#53598 = CARTESIAN_POINT('Origin',(2.5,35.924654514014,29.7362139999149)) ;
#53599 = CARTESIAN_POINT('Origin',(30.5,-2.0609575629719E-12,-1.96278056880054E-12)) ;
#53600 = CARTESIAN_POINT('',(30.5,35.5654738138977,30.1394375417177)) ;
#53601 = CARTESIAN_POINT('Origin',(30.5,35.924654514014,29.7362139999149)) ;
#53602 = CARTESIAN_POINT('',(30.5,33.6919348724754,32.220213337081)) ;
#53603 = CARTESIAN_POINT('Origin',(30.5,34.6342645913669,31.1848319093482)) ;
#53604 = CARTESIAN_POINT('Origin',(30.5,33.3284648380432,32.6195747449183)) ;
#53605 = CARTESIAN_POINT('Origin',(30.5,33.3284648380432,32.6195747449183)) ;
#53606 = CARTESIAN_POINT('',(30.5,33.6919348724754,32.220213337081)) ;
#53607 = CARTESIAN_POINT('Origin',(30.5,34.6342645913669,31.1848319093482)) ;
#53608 = CARTESIAN_POINT('',(30.5,35.5654738138977,30.1394375417177)) ;
#53609 = CARTESIAN_POINT('Origin',(30.5,35.924654514014,29.7362139999149)) ;
#53610 = CARTESIAN_POINT('Origin',(2.5,-1.84450098521206E-12,-2.16745697839283E-12)) ;
#53611 = CARTESIAN_POINT('',(2.5,30.1394375417177,35.5654738138976)) ;
#53612 = CARTESIAN_POINT('Origin',(2.5,29.7362139999149,35.9246545140139)) ;
#53613 = CARTESIAN_POINT('',(2.5,32.2202133370811,33.6919348724755)) ;
#53614 = CARTESIAN_POINT('Origin',(2.5,31.1848319093483,34.6342645913669)) ;
#53615 = CARTESIAN_POINT('Origin',(2.5,32.6195747449184,33.3284648380432)) ;
#53616 = CARTESIAN_POINT('Origin',(30.5,-1.84450098521206E-12,-2.16745697839283E-12)) ;
#53617 = CARTESIAN_POINT('',(30.5,32.2202133370811,33.6919348724755)) ;
#53618 = CARTESIAN_POINT('Origin',(30.5,32.6195747449184,33.3284648380432)) ;
#53619 = CARTESIAN_POINT('',(30.5,30.1394375417177,35.5654738138976)) ;
#53620 = CARTESIAN_POINT('Origin',(30.5,31.1848319093483,34.6342645913669)) ;
#53621 = CARTESIAN_POINT('Origin',(30.5,29.7362139999149,35.9246545140139)) ;
#53622 = CARTESIAN_POINT('Origin',(30.5,29.7362139999149,35.9246545140139)) ;
#53623 = CARTESIAN_POINT('',(30.5,30.1394375417177,35.5654738138976)) ;
#53624 = CARTESIAN_POINT('Origin',(30.5,31.1848319093483,34.6342645913669)) ;
#53625 = CARTESIAN_POINT('',(30.5,32.2202133370811,33.6919348724755)) ;
#53626 = CARTESIAN_POINT('Origin',(30.5,32.6195747449184,33.3284648380432)) ;
#53627 = CARTESIAN_POINT('Origin',(2.5,-1.60783566867159E-12,-2.34838627576032E-12)) ;
#53628 = CARTESIAN_POINT('',(2.5,26.2567262261701,38.5210715170554)) ;
#53629 = CARTESIAN_POINT('Origin',(2.5,25.8181669785007,38.8361362505367)) ;
#53630 = CARTESIAN_POINT('',(2.5,28.5219414604302,36.8752963142798)) ;
#53631 = CARTESIAN_POINT('Origin',(2.5,27.3937316830851,37.7042370228368)) ;
#53632 = CARTESIAN_POINT('Origin',(2.5,28.9571080888326,36.5555620409763)) ;
#53633 = CARTESIAN_POINT('Origin',(30.5,-1.60783566867159E-12,-2.34838627576032E-12)) ;
#53634 = CARTESIAN_POINT('',(30.5,28.5219414604302,36.8752963142798)) ;
#53635 = CARTESIAN_POINT('Origin',(30.5,28.9571080888326,36.5555620409763)) ;
#53636 = CARTESIAN_POINT('',(30.5,26.2567262261701,38.5210715170554)) ;
#53637 = CARTESIAN_POINT('Origin',(30.5,27.3937316830851,37.7042370228368)) ;
#53638 = CARTESIAN_POINT('Origin',(30.5,25.8181669785007,38.8361362505367)) ;
#53639 = CARTESIAN_POINT('Origin',(30.5,25.8181669785007,38.8361362505367)) ;
#53640 = CARTESIAN_POINT('',(30.5,26.2567262261701,38.5210715170554)) ;
#53641 = CARTESIAN_POINT('Origin',(30.5,27.3937316830851,37.7042370228368)) ;
#53642 = CARTESIAN_POINT('',(30.5,28.5219414604302,36.8752963142798)) ;
#53643 = CARTESIAN_POINT('Origin',(30.5,28.9571080888326,36.5555620409763)) ;
#53644 = CARTESIAN_POINT('Origin',(2.5,-2.42400572219872E-12,-1.49139193251805E-12)) ;
#53645 = CARTESIAN_POINT('',(2.5,39.6546442930129,24.511177224539)) ;
#53646 = CARTESIAN_POINT('Origin',(2.5,39.3821488564452,24.9773812968611)) ;
#53647 = CARTESIAN_POINT('',(2.5,41.0546242996198,22.0863407235154)) ;
#53648 = CARTESIAN_POINT('Origin',(2.5,40.3611139433656,23.3024999999953)) ;
#53649 = CARTESIAN_POINT('Origin',(2.5,41.3221211513147,21.6172507168713)) ;
#53650 = CARTESIAN_POINT('Origin',(30.5,-2.42400572219872E-12,-1.49139193251805E-12)) ;
#53651 = CARTESIAN_POINT('',(30.5,41.0546242996198,22.0863407235154)) ;
#53652 = CARTESIAN_POINT('Origin',(30.5,41.3221211513147,21.6172507168713)) ;
#53653 = CARTESIAN_POINT('',(30.5,39.6546442930129,24.511177224539)) ;
#53654 = CARTESIAN_POINT('Origin',(30.5,40.3611139433656,23.3024999999953)) ;
#53655 = CARTESIAN_POINT('Origin',(30.5,39.3821488564452,24.9773812968611)) ;
#53656 = CARTESIAN_POINT('Origin',(30.5,39.3821488564452,24.9773812968611)) ;
#53657 = CARTESIAN_POINT('',(30.5,39.6546442930129,24.511177224539)) ;
#53658 = CARTESIAN_POINT('Origin',(30.5,40.3611139433656,23.3024999999953)) ;
#53659 = CARTESIAN_POINT('',(30.5,41.0546242996198,22.0863407235154)) ;
#53660 = CARTESIAN_POINT('Origin',(30.5,41.3221211513147,21.6172507168713)) ;
#53661 = CARTESIAN_POINT('Origin',(2.5,-2.5666196720605E-12,-1.22984433837137E-12)) ;
#53662 = CARTESIAN_POINT('',(2.5,41.9995276906041,20.2318634016821)) ;
#53663 = CARTESIAN_POINT('Origin',(2.5,41.7772566077985,20.7239970885482)) ;
#53664 = CARTESIAN_POINT('',(2.5,43.1383740271251,17.6739726500298)) ;
#53665 = CARTESIAN_POINT('Origin',(2.5,42.5757860534247,18.9559612505438)) ;
#53666 = CARTESIAN_POINT('Origin',(2.5,43.355372245549,17.1794913326873)) ;
#53667 = CARTESIAN_POINT('Origin',(30.5,-2.5666196720605E-12,-1.22984433837137E-12)) ;
#53668 = CARTESIAN_POINT('',(30.5,43.1383740271251,17.6739726500298)) ;
#53669 = CARTESIAN_POINT('Origin',(30.5,43.355372245549,17.1794913326873)) ;
#53670 = CARTESIAN_POINT('',(30.5,41.9995276906041,20.2318634016821)) ;
#53671 = CARTESIAN_POINT('Origin',(30.5,42.5757860534247,18.9559612505438)) ;
#53672 = CARTESIAN_POINT('Origin',(30.5,41.7772566077985,20.7239970885482)) ;
#53673 = CARTESIAN_POINT('Origin',(30.5,41.7772566077985,20.7239970885482)) ;
#53674 = CARTESIAN_POINT('',(30.5,41.9995276906041,20.2318634016821)) ;
#53675 = CARTESIAN_POINT('Origin',(30.5,42.5757860534247,18.9559612505438)) ;
#53676 = CARTESIAN_POINT('',(30.5,43.1383740271251,17.6739726500298)) ;
#53677 = CARTESIAN_POINT('Origin',(30.5,43.355372245549,17.1794913326873)) ;
#53678 = CARTESIAN_POINT('Origin',(2.5,-2.68111319969549E-12,-9.54822312292023E-13)) ;
#53679 = CARTESIAN_POINT('',(2.5,43.8842554738508,15.7308850496067)) ;
#53680 = CARTESIAN_POINT('Origin',(2.5,43.7146439933037,16.2435564313579)) ;
#53681 = CARTESIAN_POINT('',(2.5,44.7494907015041,13.0679648336741)) ;
#53682 = CARTESIAN_POINT('Origin',(2.5,44.3239889419266,14.4017370228415)) ;
#53683 = CARTESIAN_POINT('Origin',(2.5,44.9136128087662,12.5535098464227)) ;
#53684 = CARTESIAN_POINT('Origin',(30.5,-2.68111319969549E-12,-9.54822312292023E-13)) ;
#53685 = CARTESIAN_POINT('',(30.5,44.7494907015041,13.0679648336741)) ;
#53686 = CARTESIAN_POINT('Origin',(30.5,44.9136128087662,12.5535098464227)) ;
#53687 = CARTESIAN_POINT('',(30.5,43.8842554738508,15.7308850496067)) ;
#53688 = CARTESIAN_POINT('Origin',(30.5,44.3239889419266,14.4017370228415)) ;
#53689 = CARTESIAN_POINT('Origin',(30.5,43.7146439933037,16.2435564313579)) ;
#53690 = CARTESIAN_POINT('Origin',(30.5,43.7146439933037,16.2435564313579)) ;
#53691 = CARTESIAN_POINT('',(30.5,43.8842554738508,15.7308850496067)) ;
#53692 = CARTESIAN_POINT('Origin',(30.5,44.3239889419266,14.4017370228415)) ;
#53693 = CARTESIAN_POINT('',(30.5,44.7494907015041,13.0679648336741)) ;
#53694 = CARTESIAN_POINT('Origin',(30.5,44.9136128087662,12.5535098464227)) ;
#53695 = CARTESIAN_POINT('Origin',(2.5,-2.76623189005561E-12,-6.69339053149789E-13)) ;
#53696 = CARTESIAN_POINT('',(2.5,45.2881781707551,11.0575558290286)) ;
#53697 = CARTESIAN_POINT('Origin',(2.5,45.173084591341,11.585147970723)) ;
#53698 = CARTESIAN_POINT('',(2.5,45.8703225913245,8.31878165995311)) ;
#53699 = CARTESIAN_POINT('Origin',(2.5,45.5865689321897,9.6897243505597)) ;
#53700 = CARTESIAN_POINT('Origin',(2.5,45.9797704312729,7.78998947928984)) ;
#53701 = CARTESIAN_POINT('Origin',(30.5,-2.76623189005561E-12,-6.69339053149789E-13)) ;
#53702 = CARTESIAN_POINT('',(30.5,45.8703225913245,8.31878165995311)) ;
#53703 = CARTESIAN_POINT('Origin',(30.5,45.9797704312729,7.78998947928984)) ;
#53704 = CARTESIAN_POINT('',(30.5,45.2881781707551,11.0575558290286)) ;
#53705 = CARTESIAN_POINT('Origin',(30.5,45.5865689321897,9.6897243505597)) ;
#53706 = CARTESIAN_POINT('Origin',(30.5,45.173084591341,11.585147970723)) ;
#53707 = CARTESIAN_POINT('Origin',(30.5,45.173084591341,11.585147970723)) ;
#53708 = CARTESIAN_POINT('',(30.5,45.2881781707551,11.0575558290286)) ;
#53709 = CARTESIAN_POINT('Origin',(30.5,45.5865689321897,9.6897243505597)) ;
#53710 = CARTESIAN_POINT('',(30.5,45.8703225913245,8.31878165995311)) ;
#53711 = CARTESIAN_POINT('Origin',(30.5,45.9797704312729,7.78998947928984)) ;
#53712 = CARTESIAN_POINT('Origin',(45.,0.,0.)) ;
#53713 = CARTESIAN_POINT('',(0.,0.,0.)) ;
#53714 = CARTESIAN_POINT('Origin',(-3.,-1.83697019872103E-16,0.)) ;
#53715 = CARTESIAN_POINT('',(29.5,-20.,0.)) ;
#53716 = CARTESIAN_POINT('',(29.5,20.,-2.44929359829471E-15)) ;
#53717 = CARTESIAN_POINT('Origin',(29.5,1.80635402874235E-15,0.)) ;
#53718 = CARTESIAN_POINT('Origin',(29.5,1.80635402874235E-15,0.)) ;
#53719 = CARTESIAN_POINT('',(0.499999999999999,20.,-2.44929359829471E-15)) ;
#53720 = CARTESIAN_POINT('',(-3.,20.,-2.44929359829471E-15)) ;
#53721 = CARTESIAN_POINT('Origin',(0.5,3.06161699786838E-17,0.)) ;
#53722 = CARTESIAN_POINT('Origin',(0.5,3.06161699786838E-17,0.)) ;
#53723 = CARTESIAN_POINT('',(-2.28983498828939E-15,20.5,-2.51052593825207E-15)) ;
#53724 = CARTESIAN_POINT('',(0.499999999999999,20.,-2.44929359829471E-15)) ;
#53725 = CARTESIAN_POINT('Origin',(0.,0.,0.)) ;
#53726 = CARTESIAN_POINT('Origin',(1.27815278805432E-15,-20.5,0.)) ;
#53727 = CARTESIAN_POINT('',(1.50019232895551E-15,-24.5,0.)) ;
#53728 = CARTESIAN_POINT('Origin',(0.,0.,0.)) ;
#53729 = CARTESIAN_POINT('Origin',(0.,0.,0.)) ;
#53730 = CARTESIAN_POINT('',(0.499999999999998,25.,-3.06161699786838E-15)) ;
#53731 = CARTESIAN_POINT('',(0.500000000000001,-25.,-3.06161699786838E-15)) ;
#53732 = CARTESIAN_POINT('Origin',(0.5,3.06161699786838E-17,0.)) ;
#53733 = CARTESIAN_POINT('',(1.50019232895551E-15,-24.5,-3.00038465791102E-15)) ;
#53734 = CARTESIAN_POINT('Origin',(0.5,3.06161699786838E-17,0.)) ;
#53735 = CARTESIAN_POINT('Origin',(-3.,-1.83697019872103E-16,0.)) ;
#53736 = CARTESIAN_POINT('',(29.5,25.,-3.06161699786838E-15)) ;
#53737 = CARTESIAN_POINT('',(-3.,25.,-3.06161699786838E-15)) ;
#53738 = CARTESIAN_POINT('Origin',(29.5,1.80635402874235E-15,0.)) ;
#53739 = CARTESIAN_POINT('Origin',(29.5,1.80635402874235E-15,0.)) ;
#53740 = CARTESIAN_POINT('',(30.,24.5,-3.00038465791102E-15)) ;
#53741 = CARTESIAN_POINT('',(29.5,25.,-3.06161699786838E-15)) ;
#53742 = CARTESIAN_POINT('Origin',(30.,1.83697019872103E-15,0.)) ;
#53743 = CARTESIAN_POINT('Origin',(30.,-24.5,0.)) ;
#53744 = CARTESIAN_POINT('',(30.,-20.5,0.)) ;
#53745 = CARTESIAN_POINT('Origin',(30.,1.83697019872103E-15,0.)) ;
#53746 = CARTESIAN_POINT('Origin',(30.,1.83697019872103E-15,0.)) ;
#53747 = CARTESIAN_POINT('',(30.,-20.5,-2.51052593825207E-15)) ;
#53748 = CARTESIAN_POINT('',(0.,0.,0.)) ;
#53749 = CARTESIAN_POINT('Origin',(28.8444102037119,-3.00000000000001,10.)) ;
#53750 = CARTESIAN_POINT('',(28.8444102037119,-3.00000000000001,6.)) ;
#53751 = CARTESIAN_POINT('',(24.8193472919817,-3.,10.)) ;
#53752 = CARTESIAN_POINT('Ctrl Pts',(28.8444102037119,-3.00000000000001,6.)) ;
#53753 = CARTESIAN_POINT('Ctrl Pts',(26.6828023435557,-3.00000000000001,8.1500104764796)) ;
#53754 = CARTESIAN_POINT('Ctrl Pts',(24.8193472919817,-3.00000000000001,10.)) ;
#53755 = CARTESIAN_POINT('',(28.8444102037119,-3.00000000000001,0.)) ;
#53756 = CARTESIAN_POINT('',(28.8444102037119,-3.00000000000001,0.)) ;
#53757 = CARTESIAN_POINT('',(24.8193472919817,-3.,0.)) ;
#53758 = CARTESIAN_POINT('',(14.422205101856,-3.,0.)) ;
#53759 = CARTESIAN_POINT('',(24.8193472919817,-3.,10.)) ;
#53760 = CARTESIAN_POINT('Origin',(24.8193472919817,3.,10.)) ;
#53761 = CARTESIAN_POINT('',(24.8193472919817,3.,10.)) ;
#53762 = CARTESIAN_POINT('',(28.8444102037119,2.99999999999999,6.)) ;
#53763 = CARTESIAN_POINT('Ctrl Pts',(24.8193472919817,3.,10.)) ;
#53764 = CARTESIAN_POINT('Ctrl Pts',(26.6828023431939,3.,8.15001047683915)) ;
#53765 = CARTESIAN_POINT('Ctrl Pts',(28.8444102037119,2.99999999999999,6.)) ;
#53766 = CARTESIAN_POINT('',(24.8193472919817,3.,0.)) ;
#53767 = CARTESIAN_POINT('',(24.8193472919817,3.,10.)) ;
#53768 = CARTESIAN_POINT('',(28.8444102037119,2.99999999999999,0.)) ;
#53769 = CARTESIAN_POINT('',(12.4096736459909,3.,0.)) ;
#53770 = CARTESIAN_POINT('',(28.8444102037119,2.99999999999999,0.)) ;
#53771 = CARTESIAN_POINT('Origin',(0.,0.,10.)) ;
#53772 = CARTESIAN_POINT('Origin',(0.,0.,10.)) ;
#53773 = CARTESIAN_POINT('Origin',(0.,0.,0.)) ;
#53774 = CARTESIAN_POINT('Origin',(0.,0.,0.)) ;
#53775 = CARTESIAN_POINT('',(3.,-28.8444102037119,0.)) ;
#53776 = CARTESIAN_POINT('Origin',(0.,0.,0.)) ;
#53777 = CARTESIAN_POINT('',(3.,-24.8193472919817,0.)) ;
#53778 = CARTESIAN_POINT('',(3.,-12.4096736459909,0.)) ;
#53779 = CARTESIAN_POINT('',(-3.,-24.8193472919817,0.)) ;
#53780 = CARTESIAN_POINT('Origin',(0.,0.,0.)) ;
#53781 = CARTESIAN_POINT('',(-3.,-28.8444102037119,0.)) ;
#53782 = CARTESIAN_POINT('',(-3.,-14.422205101856,0.)) ;
#53783 = CARTESIAN_POINT('',(-28.8444102037119,-3.,0.)) ;
#53784 = CARTESIAN_POINT('Origin',(0.,0.,0.)) ;
#53785 = CARTESIAN_POINT('',(-24.8193472919817,-3.,0.)) ;
#53786 = CARTESIAN_POINT('',(-12.4096736459909,-3.,0.)) ;
#53787 = CARTESIAN_POINT('',(-24.8193472919817,3.,0.)) ;
#53788 = CARTESIAN_POINT('Origin',(0.,0.,0.)) ;
#53789 = CARTESIAN_POINT('',(-28.8444102037119,3.,0.)) ;
#53790 = CARTESIAN_POINT('',(-14.422205101856,3.,0.)) ;
#53791 = CARTESIAN_POINT('',(-3.,28.8444102037119,0.)) ;
#53792 = CARTESIAN_POINT('Origin',(0.,0.,0.)) ;
#53793 = CARTESIAN_POINT('',(-3.,24.8193472919817,0.)) ;
#53794 = CARTESIAN_POINT('',(-3.,12.4096736459909,0.)) ;
#53795 = CARTESIAN_POINT('',(3.,24.8193472919817,0.)) ;
#53796 = CARTESIAN_POINT('Origin',(0.,0.,0.)) ;
#53797 = CARTESIAN_POINT('',(3.,28.8444102037119,0.)) ;
#53798 = CARTESIAN_POINT('',(3.,14.422205101856,0.)) ;
#53799 = CARTESIAN_POINT('Origin',(0.,0.,0.)) ;
#53800 = CARTESIAN_POINT('',(-18.7631,-2.29781703570817E-15,0.)) ;
#53801 = CARTESIAN_POINT('Origin',(0.,0.,0.)) ;
#53802 = CARTESIAN_POINT('Origin',(0.,0.,0.)) ;
#53803 = CARTESIAN_POINT('',(3.,-28.8444102037119,6.)) ;
#53804 = CARTESIAN_POINT('Origin',(0.,0.,6.)) ;
#53805 = CARTESIAN_POINT('',(3.,-28.8444102037119,0.)) ;
#53806 = CARTESIAN_POINT('Origin',(0.,0.,8.)) ;
#53807 = CARTESIAN_POINT('',(3.,-24.8193472919817,10.)) ;
#53808 = CARTESIAN_POINT('Origin',(0.,0.,10.)) ;
#53809 = CARTESIAN_POINT('Ctrl Pts',(3.,-24.8193472919817,10.)) ;
#53810 = CARTESIAN_POINT('Ctrl Pts',(3.,-26.6828023431939,8.15001047683915)) ;
#53811 = CARTESIAN_POINT('Ctrl Pts',(3.,-28.8444102037119,6.)) ;
#53812 = CARTESIAN_POINT('Origin',(-3.,-28.8444102037119,10.)) ;
#53813 = CARTESIAN_POINT('',(-3.,-28.8444102037119,6.)) ;
#53814 = CARTESIAN_POINT('',(-3.,-24.8193472919817,10.)) ;
#53815 = CARTESIAN_POINT('Ctrl Pts',(-3.,-28.8444102037119,6.)) ;
#53816 = CARTESIAN_POINT('Ctrl Pts',(-3.,-26.6828023431939,8.15001047683915)) ;
#53817 = CARTESIAN_POINT('Ctrl Pts',(-3.,-24.8193472919817,10.)) ;
#53818 = CARTESIAN_POINT('',(-3.,-28.8444102037119,0.)) ;
#53819 = CARTESIAN_POINT('',(-3.,-24.8193472919817,10.)) ;
#53820 = CARTESIAN_POINT('Origin',(3.,-24.8193472919817,10.)) ;
#53821 = CARTESIAN_POINT('',(3.,-24.8193472919817,10.)) ;
#53822 = CARTESIAN_POINT('Origin',(0.,0.,10.)) ;
#53823 = CARTESIAN_POINT('Origin',(0.,0.,10.)) ;
#53824 = CARTESIAN_POINT('Origin',(0.,0.,0.)) ;
#53825 = CARTESIAN_POINT('',(-28.8444102037119,-3.,6.)) ;
#53826 = CARTESIAN_POINT('Origin',(0.,0.,6.)) ;
#53827 = CARTESIAN_POINT('',(-28.8444102037119,-3.,0.)) ;
#53828 = CARTESIAN_POINT('Origin',(0.,0.,8.)) ;
#53829 = CARTESIAN_POINT('',(-24.8193472919817,-3.,10.)) ;
#53830 = CARTESIAN_POINT('Origin',(0.,0.,10.)) ;
#53831 = CARTESIAN_POINT('Ctrl Pts',(-24.8193472919817,-3.,10.)) ;
#53832 = CARTESIAN_POINT('Ctrl Pts',(-26.6828023431939,-3.,8.15001047683915)) ;
#53833 = CARTESIAN_POINT('Ctrl Pts',(-28.8444102037119,-3.,6.)) ;
#53834 = CARTESIAN_POINT('Origin',(-28.8444102037119,3.,10.)) ;
#53835 = CARTESIAN_POINT('',(-28.8444102037119,3.,6.)) ;
#53836 = CARTESIAN_POINT('',(-24.8193472919817,3.,10.)) ;
#53837 = CARTESIAN_POINT('Ctrl Pts',(-28.8444102037119,3.,6.)) ;
#53838 = CARTESIAN_POINT('Ctrl Pts',(-26.6828023431939,3.,8.15001047683915)) ;
#53839 = CARTESIAN_POINT('Ctrl Pts',(-24.8193472919817,3.,10.)) ;
#53840 = CARTESIAN_POINT('',(-28.8444102037119,3.,0.)) ;
#53841 = CARTESIAN_POINT('',(-24.8193472919817,3.,10.)) ;
#53842 = CARTESIAN_POINT('Origin',(-24.8193472919817,-3.,10.)) ;
#53843 = CARTESIAN_POINT('',(-24.8193472919817,-3.,10.)) ;
#53844 = CARTESIAN_POINT('Origin',(0.,0.,10.)) ;
#53845 = CARTESIAN_POINT('Origin',(0.,0.,10.)) ;
#53846 = CARTESIAN_POINT('Origin',(0.,0.,0.)) ;
#53847 = CARTESIAN_POINT('',(-3.,28.8444102037119,6.)) ;
#53848 = CARTESIAN_POINT('Origin',(0.,0.,6.)) ;
#53849 = CARTESIAN_POINT('',(-3.,28.8444102037119,0.)) ;
#53850 = CARTESIAN_POINT('Origin',(0.,0.,8.)) ;
#53851 = CARTESIAN_POINT('',(-3.,24.8193472919817,10.)) ;
#53852 = CARTESIAN_POINT('Origin',(0.,0.,10.)) ;
#53853 = CARTESIAN_POINT('Ctrl Pts',(-3.,24.8193472919817,10.)) ;
#53854 = CARTESIAN_POINT('Ctrl Pts',(-3.,26.6828023431935,8.15001047683959)) ;
#53855 = CARTESIAN_POINT('Ctrl Pts',(-3.,28.8444102037119,6.)) ;
#53856 = CARTESIAN_POINT('Origin',(3.,28.8444102037119,10.)) ;
#53857 = CARTESIAN_POINT('',(3.,28.8444102037119,6.)) ;
#53858 = CARTESIAN_POINT('',(3.,24.8193472919817,10.)) ;
#53859 = CARTESIAN_POINT('Ctrl Pts',(3.,28.8444102037119,6.)) ;
#53860 = CARTESIAN_POINT('Ctrl Pts',(3.,26.6828023431935,8.15001047683959)) ;
#53861 = CARTESIAN_POINT('Ctrl Pts',(3.,24.8193472919817,10.)) ;
#53862 = CARTESIAN_POINT('',(3.,28.8444102037119,0.)) ;
#53863 = CARTESIAN_POINT('',(3.,24.8193472919817,10.)) ;
#53864 = CARTESIAN_POINT('Origin',(-3.,24.8193472919817,10.)) ;
#53865 = CARTESIAN_POINT('',(-3.,24.8193472919817,10.)) ;
#53866 = CARTESIAN_POINT('Origin',(0.,0.,10.)) ;
#53867 = CARTESIAN_POINT('Origin',(0.,0.,10.)) ;
#53868 = CARTESIAN_POINT('Origin',(0.,0.,8.)) ;
#53869 = CARTESIAN_POINT('Origin',(0.,0.,6.)) ;
#53870 = CARTESIAN_POINT('Origin',(0.,0.,10.)) ;
#53871 = CARTESIAN_POINT('Origin',(0.,0.,0.)) ;
#53872 = CARTESIAN_POINT('Origin',(0.,0.,10.)) ;
#53873 = CARTESIAN_POINT('',(-18.7631,-2.29781703570817E-15,10.)) ;
#53874 = CARTESIAN_POINT('Origin',(0.,0.,10.)) ;
#53875 = CARTESIAN_POINT('Origin',(0.,0.,0.)) ;
#53876 = CARTESIAN_POINT('',(-18.7631,-2.29781703570817E-15,0.)) ;
#53877 = CARTESIAN_POINT('',(0.,0.,0.)) ;
#53878 = CARTESIAN_POINT('Origin',(-2.94971926719218E-15,-16.0575237924159,
0.)) ;
#53879 = CARTESIAN_POINT('',(-1.27821691295437E-15,-16.2041857066289,-27.7395230264339)) ;
#53880 = CARTESIAN_POINT('Origin',(-2.97666062376185E-15,-16.2041857066289,
0.)) ;
#53881 = CARTESIAN_POINT('',(-8.3065322003863E-15,-15.9108618782029,-29.3077933083083)) ;
#53882 = CARTESIAN_POINT('',(-8.1894302683888E-15,-16.0575237924159,-28.523658167371)) ;
#53883 = CARTESIAN_POINT('',(-0.49246023091464,-15.9108618818334,-29.3036555873477)) ;
#53884 = CARTESIAN_POINT('Origin',(-2.92277791062251E-15,-15.9108618782028,
0.)) ;
#53885 = CARTESIAN_POINT('',(-2.30180707398644,-16.187744273641,-27.7320650306517)) ;
#53886 = CARTESIAN_POINT('Ctrl Pts',(-0.49246024089823,-15.9108618853164,
-29.3036555618719)) ;
#53887 = CARTESIAN_POINT('Ctrl Pts',(-0.524186138723702,-15.922600883412,
-29.2403504016751)) ;
#53888 = CARTESIAN_POINT('Ctrl Pts',(-0.558017475224188,-15.9340937421157,
-29.178271027574)) ;
#53889 = CARTESIAN_POINT('Ctrl Pts',(-0.593757701662899,-15.9452906232649,
-29.1176651035937)) ;
#53890 = CARTESIAN_POINT('Ctrl Pts',(-0.606024695686751,-15.9491336899667,
-29.0968635424019)) ;
#53891 = CARTESIAN_POINT('Ctrl Pts',(-0.618516201253947,-15.9529419398964,
-29.0762352962752)) ;
#53892 = CARTESIAN_POINT('Ctrl Pts',(-0.631223168391001,-15.9567135267634,
-29.0557895107889)) ;
#53893 = CARTESIAN_POINT('Ctrl Pts',(-0.667165886993807,-15.9673817754482,
-28.9979568976706)) ;
#53894 = CARTESIAN_POINT('Ctrl Pts',(-0.704840463204382,-15.977757691291,
-28.9415784282644)) ;
#53895 = CARTESIAN_POINT('Ctrl Pts',(-0.744004740092162,-15.9877997661731,
-28.8868614676232)) ;
#53896 = CARTESIAN_POINT('Ctrl Pts',(-0.783488107070585,-15.997923658641,
-28.8316987017401)) ;
#53897 = CARTESIAN_POINT('Ctrl Pts',(-0.824485149876229,-16.0077081692745,
-28.778224943148)) ;
#53898 = CARTESIAN_POINT('Ctrl Pts',(-0.866713327822006,-16.0171189356806,
-28.7266128516104)) ;
#53899 = CARTESIAN_POINT('Ctrl Pts',(-0.901270087053801,-16.0248200870137,
-28.6843769156199)) ;
#53900 = CARTESIAN_POINT('Ctrl Pts',(-0.936650542924225,-16.0322710948775,
-28.6433869753027)) ;
#53901 = CARTESIAN_POINT('Ctrl Pts',(-0.972685940156585,-16.0394576303854,
-28.6037161955719)) ;
#53902 = CARTESIAN_POINT('Ctrl Pts',(-1.01677654000943,-16.0482506141109,
-28.5551775749572)) ;
#53903 = CARTESIAN_POINT('Ctrl Pts',(-1.06297919541555,-16.0568730319549,
-28.5073700699597)) ;
#53904 = CARTESIAN_POINT('Ctrl Pts',(-1.11118837792726,-16.0652608298865,
-28.4606078955835)) ;
#53905 = CARTESIAN_POINT('Ctrl Pts',(-1.15900238541565,-16.073579872281,-28.4142290349743)) ;
#53906 = CARTESIAN_POINT('Ctrl Pts',(-1.20878996696043,-16.081668020051,-28.3688788822698)) ;
#53907 = CARTESIAN_POINT('Ctrl Pts',(-1.26040263359772,-16.0894673869311,
-28.3248412518989)) ;
#53908 = CARTESIAN_POINT('Ctrl Pts',(-1.30281303157267,-16.0958761674669,
-28.2886553008216)) ;
#53909 = CARTESIAN_POINT('Ctrl Pts',(-1.34645482892762,-16.1020900207685,
-28.2533552584702)) ;
#53910 = CARTESIAN_POINT('Ctrl Pts',(-1.39122398593242,-16.108079933754,-28.2190838414456)) ;
#53911 = CARTESIAN_POINT('Ctrl Pts',(-1.44727760151981,-16.1155796568301,
-28.17617401325)) ;
#53912 = CARTESIAN_POINT('Ctrl Pts',(-1.50510762653917,-16.1227292229207,
-28.1348712493097)) ;
#53913 = CARTESIAN_POINT('Ctrl Pts',(-1.56449742296339,-16.1294814162036,
-28.0954072564998)) ;
#53914 = CARTESIAN_POINT('Ctrl Pts',(-1.62376979496718,-16.1362202591733,
-28.0560212911755)) ;
#53915 = CARTESIAN_POINT('Ctrl Pts',(-1.68459540193731,-16.1425632136358,
-28.0184671715736)) ;
#53916 = CARTESIAN_POINT('Ctrl Pts',(-1.74672461632394,-16.148471764915,-27.9829371559304)) ;
#53917 = CARTESIAN_POINT('Ctrl Pts',(-1.79357965334542,-16.1529277264407,
-27.9561420287946)) ;
#53918 = CARTESIAN_POINT('Ctrl Pts',(-1.84117536584348,-16.1571367885211,
-27.9304973511167)) ;
#53919 = CARTESIAN_POINT('Ctrl Pts',(-1.88939385278889,-16.1610860188908,
-27.9060696007688)) ;
#53920 = CARTESIAN_POINT('Ctrl Pts',(-1.95609837828205,-16.1665493080681,
-27.8722767217499)) ;
#53921 = CARTESIAN_POINT('Ctrl Pts',(-2.02404088075897,-16.171518536629,-27.8407920493046)) ;
#53922 = CARTESIAN_POINT('Ctrl Pts',(-2.09289039826686,-16.175968006779,-27.8117544103004)) ;
#53923 = CARTESIAN_POINT('Ctrl Pts',(-2.16173991573683,-16.1804174769265,
-27.7827167713122)) ;
#53924 = CARTESIAN_POINT('Ctrl Pts',(-2.23149584064641,-16.184347145014,-27.7561263494921)) ;
#53925 = CARTESIAN_POINT('Ctrl Pts',(-2.30180707408357,-16.1877442734702,
-27.7320650305882)) ;
#53926 = CARTESIAN_POINT('',(-2.44332709960924,-15.9108618782028,-29.2057682879055)) ;
#53927 = CARTESIAN_POINT('Ctrl Pts',(-2.44332709960925,-15.9108618782028,
-29.2057682879055)) ;
#53928 = CARTESIAN_POINT('Ctrl Pts',(-2.37152999340033,-16.0510971574587,
-28.4593807438797)) ;
#53929 = CARTESIAN_POINT('Ctrl Pts',(-2.30180707378936,-16.1877442737199,
-27.7320650307343)) ;
#53930 = CARTESIAN_POINT('',(-3.89217339575026,-15.9108618782028,-29.0481967574568)) ;
#53931 = CARTESIAN_POINT('Origin',(-2.92277791062251E-15,-15.9108618782028,
0.)) ;
#53932 = CARTESIAN_POINT('',(-3.71358212386582,-16.187744273641,-27.578525241199)) ;
#53933 = CARTESIAN_POINT('Ctrl Pts',(-3.71358212407606,-16.1877442737199,
-27.5785252412373)) ;
#53934 = CARTESIAN_POINT('Ctrl Pts',(-3.80184066656078,-16.0510971575306,
-28.3038250835262)) ;
#53935 = CARTESIAN_POINT('Ctrl Pts',(-3.89217339575026,-15.9108618782028,
-29.0481967574569)) ;
#53936 = CARTESIAN_POINT('',(-5.81847295702336,-15.9108618818334,-28.7244167966786)) ;
#53937 = CARTESIAN_POINT('Ctrl Pts',(-3.71358212375731,-16.1877442734702,
-27.5785252411579)) ;
#53938 = CARTESIAN_POINT('Ctrl Pts',(-3.78742199194626,-16.1843471450141,
-27.5869091829932)) ;
#53939 = CARTESIAN_POINT('Ctrl Pts',(-3.86126321677957,-16.1804174769265,
-27.5978824736425)) ;
#53940 = CARTESIAN_POINT('Ctrl Pts',(-3.93474530482747,-16.175968006779,-27.6114406176889)) ;
#53941 = CARTESIAN_POINT('Ctrl Pts',(-4.00822739291584,-16.1715185366291,
-27.6249987617427)) ;
#53942 = CARTESIAN_POINT('Ctrl Pts',(-4.08134971133666,-16.166549308068,-27.6411417103761)) ;
#53943 = CARTESIAN_POINT('Ctrl Pts',(-4.15375919217085,-16.1610860188908,
-27.6598050294532)) ;
#53944 = CARTESIAN_POINT('Ctrl Pts',(-4.22313933618834,-16.155851292919,-27.6776875463626)) ;
#53945 = CARTESIAN_POINT('Ctrl Pts',(-4.29190989303592,-16.1501596984485,
-27.6978951324919)) ;
#53946 = CARTESIAN_POINT('Ctrl Pts',(-4.35977148811458,-16.1440425621065,
-27.7203296643783)) ;
#53947 = CARTESIAN_POINT('Ctrl Pts',(-4.42777328397754,-16.1379127878753,
-27.7428105455873)) ;
#53948 = CARTESIAN_POINT('Ctrl Pts',(-4.49486188205611,-16.1313557844548,
-27.7675273949414)) ;
#53949 = CARTESIAN_POINT('Ctrl Pts',(-4.5607563501789,-16.1244124680043,-27.7943340449523)) ;
#53950 = CARTESIAN_POINT('Ctrl Pts',(-4.61040891985226,-16.1191805644221,
-27.8145332983235)) ;
#53951 = CARTESIAN_POINT('Ctrl Pts',(-4.6593838589112,-16.1137295207043,-27.8359181045309)) ;
#53952 = CARTESIAN_POINT('Ctrl Pts',(-4.7075709334888,-16.1080799337539,-27.8584093755501)) ;
#53953 = CARTESIAN_POINT('Ctrl Pts',(-4.76966295670377,-16.1008000918637,
-27.8873907680604)) ;
#53954 = CARTESIAN_POINT('Ctrl Pts',(-4.83045442176362,-16.0931892946344,
-27.9182150248434)) ;
#53955 = CARTESIAN_POINT('Ctrl Pts',(-4.88971084783703,-16.085300212968,-27.9506685948721)) ;
#53956 = CARTESIAN_POINT('Ctrl Pts',(-4.94945047354874,-16.0773468007022,
-27.9833868037652)) ;
#53957 = CARTESIAN_POINT('Ctrl Pts',(-5.00762956373555,-16.0691106491232,
-28.0177606545818)) ;
#53958 = CARTESIAN_POINT('Ctrl Pts',(-5.06404484329238,-16.060651803057,-28.0535335007289)) ;
#53959 = CARTESIAN_POINT('Ctrl Pts',(-5.110245354077,-16.0537245483846,-28.082829176957)) ;
#53960 = CARTESIAN_POINT('Ctrl Pts',(-5.15526359580896,-16.0466480826282,
-28.1130622837498)) ;
#53961 = CARTESIAN_POINT('Ctrl Pts',(-5.19900837882609,-16.0394576303854,
-28.1440759310355)) ;
#53962 = CARTESIAN_POINT('Ctrl Pts',(-5.25251261681066,-16.0306629892538,
-28.1820087186892)) ;
#53963 = CARTESIAN_POINT('Ctrl Pts',(-5.30548320190949,-16.0214720150689,
-28.2220830974099)) ;
#53964 = CARTESIAN_POINT('Ctrl Pts',(-5.35759068651864,-16.0119118209665,
-28.2642301528485)) ;
#53965 = CARTESIAN_POINT('Ctrl Pts',(-5.40927139607099,-16.0024299275614,
-28.3060320119662)) ;
#53966 = CARTESIAN_POINT('Ctrl Pts',(-5.46010261316689,-15.9925848997548,
-28.3498725976557)) ;
#53967 = CARTESIAN_POINT('Ctrl Pts',(-5.50978147538154,-15.9824119250018,
-28.3956378490517)) ;
#53968 = CARTESIAN_POINT('Ctrl Pts',(-5.55057275114205,-15.9740589032143,
-28.4332156619629)) ;
#53969 = CARTESIAN_POINT('Ctrl Pts',(-5.59058732671593,-15.965484957055,-28.4720901843792)) ;
#53970 = CARTESIAN_POINT('Ctrl Pts',(-5.62967034032201,-15.9567135267634,
-28.5121756210024)) ;
#53971 = CARTESIAN_POINT('Ctrl Pts',(-5.67863253635718,-15.9457249040903,
-28.5623936268574)) ;
#53972 = CARTESIAN_POINT('Ctrl Pts',(-5.72613910993178,-15.9344245943246,
-28.6145204117879)) ;
#53973 = CARTESIAN_POINT('Ctrl Pts',(-5.7719333306353,-15.9228603613917,-28.6683698779022)) ;
#53974 = CARTESIAN_POINT('Ctrl Pts',(-5.78765112225729,-15.9188912098106,
-28.6868524434823)) ;
#53975 = CARTESIAN_POINT('Ctrl Pts',(-5.8031674745876,-15.9148910209384,-28.7055376017322)) ;
#53976 = CARTESIAN_POINT('Ctrl Pts',(-5.81847294179664,-15.9108618853164,
-28.7244167739446)) ;
#53977 = CARTESIAN_POINT('',(-6.78036653080772,-15.9108618828344,-28.5126880007908)) ;
#53978 = CARTESIAN_POINT('Origin',(-2.92277791062251E-15,-15.9108618782028,
0.)) ;
#53979 = CARTESIAN_POINT('',(-8.20956633133313,-16.1877442736409,-26.5888842812482)) ;
#53980 = CARTESIAN_POINT('Ctrl Pts',(-6.78036653281022,-15.9108618871751,
-28.5126879735306)) ;
#53981 = CARTESIAN_POINT('Ctrl Pts',(-6.79774195886506,-15.9226008852454,
-28.4440427226535)) ;
#53982 = CARTESIAN_POINT('Ctrl Pts',(-6.81743710737947,-15.9340937439209,
-28.3761419926111)) ;
#53983 = CARTESIAN_POINT('Ctrl Pts',(-6.83931326525882,-15.9452906250393,
-28.3092699093489)) ;
#53984 = CARTESIAN_POINT('Ctrl Pts',(-6.84682174193608,-15.9491336911389,
-28.2863176395625)) ;
#53985 = CARTESIAN_POINT('Ctrl Pts',(-6.85458673873747,-15.9529419404769,
-28.2634863694506)) ;
#53986 = CARTESIAN_POINT('Ctrl Pts',(-6.86260138330426,-15.9567135267634,
-28.2407869762416)) ;
#53987 = CARTESIAN_POINT('Ctrl Pts',(-6.8852714788191,-15.9673817754481,-28.1765798354398)) ;
#53988 = CARTESIAN_POINT('Ctrl Pts',(-6.90994553998719,-15.9777576912908,
-28.1134205430859)) ;
#53989 = CARTESIAN_POINT('Ctrl Pts',(-6.93643164872909,-15.9877997661729,
-28.0515636727349)) ;
#53990 = CARTESIAN_POINT('Ctrl Pts',(-6.96313355246351,-15.9979236586408,
-27.9892028248837)) ;
#53991 = CARTESIAN_POINT('Ctrl Pts',(-6.99167682976634,-16.0077081692742,
-27.9281661007126)) ;
#53992 = CARTESIAN_POINT('Ctrl Pts',(-7.02182266234008,-16.0171189356803,
-27.8686828611919)) ;
#53993 = CARTESIAN_POINT('Ctrl Pts',(-7.04649202599232,-16.0248200870135,
-27.8200056961688)) ;
#53994 = CARTESIAN_POINT('Ctrl Pts',(-7.07223368095194,-16.0322710948773,
-27.7723683257036)) ;
#53995 = CARTESIAN_POINT('Ctrl Pts',(-7.09889854564042,-16.0394576303853,
-27.7258784815505)) ;
#53996 = CARTESIAN_POINT('Ctrl Pts',(-7.13152396312936,-16.0482506141108,
-27.6689964912531)) ;
#53997 = CARTESIAN_POINT('Ctrl Pts',(-7.16636922573244,-16.0568730319548,
-27.6123744939841)) ;
#53998 = CARTESIAN_POINT('Ctrl Pts',(-7.20339881913625,-16.0652608298864,
-27.5563420440722)) ;
#53999 = CARTESIAN_POINT('Ctrl Pts',(-7.24012487761836,-16.0735798722808,
-27.5007688972131)) ;
#54000 = CARTESIAN_POINT('Ctrl Pts',(-7.27899951088328,-16.0816680200507,
-27.4457761475559)) ;
#54001 = CARTESIAN_POINT('Ctrl Pts',(-7.31993871326926,-16.0894673869308,
-27.3916728948438)) ;
#54002 = CARTESIAN_POINT('Ctrl Pts',(-7.35357866987537,-16.0958761674666,
-27.347215969271)) ;
#54003 = CARTESIAN_POINT('Ctrl Pts',(-7.38861168061711,-16.1020900207684,
-27.3033595259035)) ;
#54004 = CARTESIAN_POINT('Ctrl Pts',(-7.42496681800589,-16.1080799337539,
-27.2602653101741)) ;
#54005 = CARTESIAN_POINT('Ctrl Pts',(-7.47048558655389,-16.1155796568301,
-27.206308819498)) ;
#54006 = CARTESIAN_POINT('Ctrl Pts',(-7.51808470437888,-16.1227292229208,
-27.1535399452904)) ;
#54007 = CARTESIAN_POINT('Ctrl Pts',(-7.56760240845947,-16.1294814162036,
-27.1022315480204)) ;
#54008 = CARTESIAN_POINT('Ctrl Pts',(-7.61702220704024,-16.1362202591733,
-27.0510245967762)) ;
#54009 = CARTESIAN_POINT('Ctrl Pts',(-7.66835271949838,-16.1425632136358,
-27.0012727641148)) ;
#54010 = CARTESIAN_POINT('Ctrl Pts',(-7.72139148427502,-16.148471764915,-26.9532174759262)) ;
#54011 = CARTESIAN_POINT('Ctrl Pts',(-7.76139091629272,-16.1529277264407,
-26.916976356038)) ;
#54012 = CARTESIAN_POINT('Ctrl Pts',(-7.80236101983229,-16.1571367885211,
-26.8816995654055)) ;
#54013 = CARTESIAN_POINT('Ctrl Pts',(-7.84420094110262,-16.1610860188908,
-26.8474773729212)) ;
#54014 = CARTESIAN_POINT('Ctrl Pts',(-7.90208148177932,-16.166549308068,-26.8001350514255)) ;
#54015 = CARTESIAN_POINT('Ctrl Pts',(-7.96166725240902,-16.171518536629,-26.7547808434592)) ;
#54016 = CARTESIAN_POINT('Ctrl Pts',(-8.02266487241837,-16.1759680067789,
-26.7116214772316)) ;
#54017 = CARTESIAN_POINT('Ctrl Pts',(-8.08366249239416,-16.1804174769265,
-26.6684621110276)) ;
#54018 = CARTESIAN_POINT('Ctrl Pts',(-8.14607140785925,-16.184347145014,-26.6274978966081)) ;
#54019 = CARTESIAN_POINT('Ctrl Pts',(-8.20956633141436,-16.1877442734702,
-26.5888842811653)) ;
#54020 = CARTESIAN_POINT('',(-8.6645803353537,-15.9108618782028,-27.9977105530919)) ;
#54021 = CARTESIAN_POINT('Ctrl Pts',(-8.66458033535307,-15.9108618782028,
-27.9977105530921)) ;
#54022 = CARTESIAN_POINT('Ctrl Pts',(-8.43401054721174,-16.0510971571362,
-27.2842073922392)) ;
#54023 = CARTESIAN_POINT('Ctrl Pts',(-8.20956633115848,-16.1877442737199,
-26.5888842813712)) ;
#54024 = CARTESIAN_POINT('',(-10.0456801889648,-15.9108618782028,-27.5323638313813)) ;
#54025 = CARTESIAN_POINT('Origin',(-2.92277791062251E-15,-15.9108618782028,
0.)) ;
#54026 = CARTESIAN_POINT('',(-9.55532834895708,-16.187744273641,-26.1354442627972)) ;
#54027 = CARTESIAN_POINT('Ctrl Pts',(-9.55532834917054,-16.1877442737199,
-26.1354442627894)) ;
#54028 = CARTESIAN_POINT('Ctrl Pts',(-9.79744148403593,-16.0510971565844,
-26.8248140248655)) ;
#54029 = CARTESIAN_POINT('Ctrl Pts',(-10.0456801889654,-15.9108618782028,
-27.5323638313811)) ;
#54030 = CARTESIAN_POINT('',(-11.8573408058246,-15.9108618828344,-26.8020561960657)) ;
#54031 = CARTESIAN_POINT('Ctrl Pts',(-9.55532834884232,-16.1877442734702,
-26.1354442627804)) ;
#54032 = CARTESIAN_POINT('Ctrl Pts',(-9.62924418161346,-16.184347145014,-26.1277588037449)) ;
#54033 = CARTESIAN_POINT('Ctrl Pts',(-9.70371797276582,-16.1804174769265,
-26.1226018643487)) ;
#54034 = CARTESIAN_POINT('Ctrl Pts',(-9.77839669062387,-16.1759680067789,
-26.1200465497064)) ;
#54035 = CARTESIAN_POINT('Ctrl Pts',(-9.85307540852301,-16.1715185366289,
-26.1174912350626)) ;
#54036 = CARTESIAN_POINT('Ctrl Pts',(-9.92795842454781,-16.166549308068,-26.1175376335476)) ;
#54037 = CARTESIAN_POINT('Ctrl Pts',(-10.0026870738764,-16.1610860188908,
-26.1201987166258)) ;
#54038 = CARTESIAN_POINT('Ctrl Pts',(-10.0742893612143,-16.155851292919,-26.1227484701259)) ;
#54039 = CARTESIAN_POINT('Ctrl Pts',(-10.1457961343455,-16.1501596984485,
-26.1276999772421)) ;
#54040 = CARTESIAN_POINT('Ctrl Pts',(-10.2168939242383,-16.1440425621064,
-26.1350217652726)) ;
#54041 = CARTESIAN_POINT('Ctrl Pts',(-10.2881386008333,-16.1379127878752,
-26.1423586799801)) ;
#54042 = CARTESIAN_POINT('Ctrl Pts',(-10.3589720967571,-16.1313557844547,
-26.1520755976696)) ;
#54043 = CARTESIAN_POINT('Ctrl Pts',(-10.4290886261871,-16.1244124680042,
-26.1640901602802)) ;
#54044 = CARTESIAN_POINT('Ctrl Pts',(-10.4819225887626,-16.119180564422,-26.1731433315722)) ;
#54045 = CARTESIAN_POINT('Ctrl Pts',(-10.534349622166,-16.1137295207043,-26.1835000086853)) ;
#54046 = CARTESIAN_POINT('Ctrl Pts',(-10.5862450681494,-16.108079933754,-26.1951066496522)) ;
#54047 = CARTESIAN_POINT('Ctrl Pts',(-10.6531155570727,-16.1008000918637,
-26.2100625237468)) ;
#54048 = CARTESIAN_POINT('Ctrl Pts',(-10.7191120555118,-16.0931892946344,
-26.2270977585306)) ;
#54049 = CARTESIAN_POINT('Ctrl Pts',(-10.7839596575085,-16.085300212968,-26.2460542021285)) ;
#54050 = CARTESIAN_POINT('Ctrl Pts',(-10.8493360517377,-16.0773468007022,
-26.2651652238421)) ;
#54051 = CARTESIAN_POINT('Ctrl Pts',(-10.9135443089684,-16.0691106491231,
-26.2862286485001)) ;
#54052 = CARTESIAN_POINT('Ctrl Pts',(-10.9763307351236,-16.0606518030569,
-26.3090375279026)) ;
#54053 = CARTESIAN_POINT('Ctrl Pts',(-11.0277488080551,-16.0537245483846,
-26.327716543359)) ;
#54054 = CARTESIAN_POINT('Ctrl Pts',(-11.0782137725886,-16.0466480826281,
-26.3475652256732)) ;
#54055 = CARTESIAN_POINT('Ctrl Pts',(-11.1276028442977,-16.0394576303853,
-26.3684499558578)) ;
#54056 = CARTESIAN_POINT('Ctrl Pts',(-11.1880106109912,-16.0306629892538,
-26.393994066423)) ;
#54057 = CARTESIAN_POINT('Ctrl Pts',(-11.2483575800814,-16.0214720150689,
-26.421744418442)) ;
#54058 = CARTESIAN_POINT('Ctrl Pts',(-11.3083071917182,-16.0119118209665,
-26.4517045302412)) ;
#54059 = CARTESIAN_POINT('Ctrl Pts',(-11.3677657990569,-16.0024299275615,
-26.4814192602395)) ;
#54060 = CARTESIAN_POINT('Ctrl Pts',(-11.4268330405492,-15.9925848997549,
-26.5133076682826)) ;
#54061 = CARTESIAN_POINT('Ctrl Pts',(-11.4851886148112,-15.9824119250019,
-26.5473234666537)) ;
#54062 = CARTESIAN_POINT('Ctrl Pts',(-11.5331043321964,-15.9740589032144,
-26.5752538126744)) ;
#54063 = CARTESIAN_POINT('Ctrl Pts',(-11.5805402624269,-15.965484957055,-26.6046175194338)) ;
#54064 = CARTESIAN_POINT('Ctrl Pts',(-11.6273267208508,-15.9567135267634,
-26.635364088185)) ;
#54065 = CARTESIAN_POINT('Ctrl Pts',(-11.685939594779,-15.9457249040899,-26.673882600136)) ;
#54066 = CARTESIAN_POINT('Ctrl Pts',(-11.743541208969,-15.9344245943236,-26.7145781807697)) ;
#54067 = CARTESIAN_POINT('Ctrl Pts',(-11.7998408296788,-15.9228603613902,
-26.7573242725093)) ;
#54068 = CARTESIAN_POINT('Ctrl Pts',(-11.8191643503523,-15.91889121042,-26.7719958631351)) ;
#54069 = CARTESIAN_POINT('Ctrl Pts',(-11.8383346927553,-15.9148910221682,
-26.7869086133455)) ;
#54070 = CARTESIAN_POINT('Ctrl Pts',(-11.8573407877332,-15.9108618871751,
-26.802056175576)) ;
#54071 = CARTESIAN_POINT('',(-12.751230463362,-15.9108618962294,-26.3884985273164)) ;
#54072 = CARTESIAN_POINT('Origin',(-2.92277791062251E-15,-15.9108618782028,
0.)) ;
#54073 = CARTESIAN_POINT('',(-13.733455391304,-16.1877442736409,-24.2024368542766)) ;
#54074 = CARTESIAN_POINT('Ctrl Pts',(-12.7512304249355,-15.9108619321403,
-26.3884985240484)) ;
#54075 = CARTESIAN_POINT('Ctrl Pts',(-12.7534429295709,-15.9226009295965,
-26.317722958503)) ;
#54076 = CARTESIAN_POINT('Ctrl Pts',(-12.7580809727586,-15.9340937875902,
-26.2471758359495)) ;
#54077 = CARTESIAN_POINT('Ctrl Pts',(-12.7650701630532,-15.9452906679662,
-26.1771644588304)) ;
#54078 = CARTESIAN_POINT('Ctrl Pts',(-12.7674690293055,-15.9491337194976,
-26.1531347897597)) ;
#54079 = CARTESIAN_POINT('Ctrl Pts',(-12.7701444276626,-15.9529419545197,
-26.1291681467903)) ;
#54080 = CARTESIAN_POINT('Ctrl Pts',(-12.7730919847679,-15.9567135267634,
-26.1052766300655)) ;
#54081 = CARTESIAN_POINT('Ctrl Pts',(-12.7814294287248,-15.9673817754482,
-26.0376972161225)) ;
#54082 = CARTESIAN_POINT('Ctrl Pts',(-12.7919492431736,-15.9777576912909,
-25.9707103591345)) ;
#54083 = CARTESIAN_POINT('Ctrl Pts',(-12.8045187227623,-15.987799766173,-25.904605937582)) ;
#54084 = CARTESIAN_POINT('Ctrl Pts',(-12.8171906119115,-15.9979236586409,
-25.8379629316985)) ;
#54085 = CARTESIAN_POINT('Ctrl Pts',(-12.8319454717887,-16.0077081692743,
-25.7722172513329)) ;
#54086 = CARTESIAN_POINT('Ctrl Pts',(-12.8485993733643,-16.0171189356803,
-25.7076442339976)) ;
#54087 = CARTESIAN_POINT('Ctrl Pts',(-12.8622278294101,-16.0248200870135,
-25.6548019300786)) ;
#54088 = CARTESIAN_POINT('Ctrl Pts',(-12.8771270322822,-16.0322710948774,
-25.6027445999641)) ;
#54089 = CARTESIAN_POINT('Ctrl Pts',(-12.8931745449892,-16.0394576303854,
-25.5516095048324)) ;
#54090 = CARTESIAN_POINT('Ctrl Pts',(-12.9128092518532,-16.0482506141109,
-25.4890438834985)) ;
#54091 = CARTESIAN_POINT('Ctrl Pts',(-12.934667795902,-16.0568730319549,-25.4262549756191)) ;
#54092 = CARTESIAN_POINT('Ctrl Pts',(-12.9587863375661,-16.0652608298865,
-25.3635722652533)) ;
#54093 = CARTESIAN_POINT('Ctrl Pts',(-12.9827071773659,-16.0735798722809,
-25.3014033707258)) ;
#54094 = CARTESIAN_POINT('Ctrl Pts',(-13.008851127706,-16.0816680200508,-25.2393394239693)) ;
#54095 = CARTESIAN_POINT('Ctrl Pts',(-13.0372025942384,-16.089467386931,-25.1777003568806)) ;
#54096 = CARTESIAN_POINT('Ctrl Pts',(-13.0604991424922,-16.0958761674668,
-25.1270512132426)) ;
#54097 = CARTESIAN_POINT('Ctrl Pts',(-13.0852852619739,-16.1020900207685,
-25.0766890474091)) ;
#54098 = CARTESIAN_POINT('Ctrl Pts',(-13.1115264539273,-16.108079933754,-25.0267870706076)) ;
#54099 = CARTESIAN_POINT('Ctrl Pts',(-13.1443819684093,-16.1155796568302,
-24.9643068629862)) ;
#54100 = CARTESIAN_POINT('Ctrl Pts',(-13.1795244971934,-16.1227292229209,
-24.9025392924203)) ;
#54101 = CARTESIAN_POINT('Ctrl Pts',(-13.2168547161228,-16.1294814162038,
-24.8417856143209)) ;
#54102 = CARTESIAN_POINT('Ctrl Pts',(-13.2541111264253,-16.1362202591735,
-24.7811520572841)) ;
#54103 = CARTESIAN_POINT('Ctrl Pts',(-13.2935463866587,-16.142563213636,-24.7215288519631)) ;
#54104 = CARTESIAN_POINT('Ctrl Pts',(-13.335014668133,-16.1484717649152,-24.663195303095)) ;
#54105 = CARTESIAN_POINT('Ctrl Pts',(-13.3662881661615,-16.1529277264408,
-24.6192027849421)) ;
#54106 = CARTESIAN_POINT('Ctrl Pts',(-13.3987169442358,-16.1571367885212,
-24.5759433848783)) ;
#54107 = CARTESIAN_POINT('Ctrl Pts',(-13.4322219116137,-16.1610860188908,
-24.5335269419437)) ;
#54108 = CARTESIAN_POINT('Ctrl Pts',(-13.4785720377214,-16.166549308068,-24.4748488523074)) ;
#54109 = CARTESIAN_POINT('Ctrl Pts',(-13.5270149120941,-16.171518536629,-24.4177458211771)) ;
#54110 = CARTESIAN_POINT('Ctrl Pts',(-13.5773084536872,-16.1759680067789,
-24.3624828117227)) ;
#54111 = CARTESIAN_POINT('Ctrl Pts',(-13.6276019952526,-16.1804174769264,
-24.3072198022987)) ;
#54112 = CARTESIAN_POINT('Ctrl Pts',(-13.6797457297486,-16.1843471450139,
-24.2537972364176)) ;
#54113 = CARTESIAN_POINT('Ctrl Pts',(-13.7334553913656,-16.1877442734701,
-24.2024368541783)) ;
#54114 = CARTESIAN_POINT('',(-14.4806874246056,-15.9108618782028,-25.4805109900367)) ;
#54115 = CARTESIAN_POINT('Ctrl Pts',(-14.4806874246052,-15.9108618782028,
-25.480510990037)) ;
#54116 = CARTESIAN_POINT('Ctrl Pts',(-14.1021261398189,-16.0510971577221,
-24.8332548227359)) ;
#54117 = CARTESIAN_POINT('Ctrl Pts',(-13.7334553911596,-16.1877442737198,
-24.2024368544343)) ;
#54118 = CARTESIAN_POINT('',(-15.7294621415161,-15.9108618782028,-24.7291481725741)) ;
#54119 = CARTESIAN_POINT('Origin',(-2.92277791062251E-15,-15.9108618782028,
0.)) ;
#54120 = CARTESIAN_POINT('',(-14.9502780404369,-16.1877442736409,-23.4702989581261)) ;
#54121 = CARTESIAN_POINT('Ctrl Pts',(-14.9502780406439,-16.1877442737198,
-23.4702989580725)) ;
#54122 = CARTESIAN_POINT('Ctrl Pts',(-15.334924823484,-16.051097157543,-24.0915044666593)) ;
#54123 = CARTESIAN_POINT('Ctrl Pts',(-15.7294621415166,-15.9108618782028,
-24.7291481725738)) ;
#54124 = CARTESIAN_POINT('',(-17.3417723053831,-15.9108618962294,-23.6264611434764)) ;
#54125 = CARTESIAN_POINT('Ctrl Pts',(-14.9502780403211,-16.1877442734701,
-23.4702989581345)) ;
#54126 = CARTESIAN_POINT('Ctrl Pts',(-15.0208136154855,-16.1843471450139,
-23.4469034617511)) ;
#54127 = CARTESIAN_POINT('Ctrl Pts',(-15.0924376612541,-16.1804174769263,
-23.4258574250642)) ;
#54128 = CARTESIAN_POINT('Ctrl Pts',(-15.1648211150744,-16.1759680067789,
-23.4073081354059)) ;
#54129 = CARTESIAN_POINT('Ctrl Pts',(-15.2372045689347,-16.171518536629,-23.3887588457375)) ;
#54130 = CARTESIAN_POINT('Ctrl Pts',(-15.3103468359606,-16.166549308068,-23.3727065245325)) ;
#54131 = CARTESIAN_POINT('Ctrl Pts',(-15.3839004251958,-16.1610860188908,
-23.3592409423246)) ;
#54132 = CARTESIAN_POINT('Ctrl Pts',(-15.4543768124774,-16.155851292919,-23.3463387087759)) ;
#54133 = CARTESIAN_POINT('Ctrl Pts',(-15.5252762246533,-16.1501596984486,
-23.3358026099092)) ;
#54134 = CARTESIAN_POINT('Ctrl Pts',(-15.5962857557236,-16.1440425621066,
-23.3276692954131)) ;
#54135 = CARTESIAN_POINT('Ctrl Pts',(-15.6674419911549,-16.1379127878755,
-23.3195191776417)) ;
#54136 = CARTESIAN_POINT('Ctrl Pts',(-15.7387082893792,-16.1313557844551,
-23.3137818113949)) ;
#54137 = CARTESIAN_POINT('Ctrl Pts',(-15.8097683091281,-16.1244124680047,
-23.3104424990107)) ;
#54138 = CARTESIAN_POINT('Ctrl Pts',(-15.8633132072386,-16.1191805644224,
-23.3079262719957)) ;
#54139 = CARTESIAN_POINT('Ctrl Pts',(-15.9167409051749,-16.1137295207044,
-23.3067705533035)) ;
#54140 = CARTESIAN_POINT('Ctrl Pts',(-15.9699181491897,-16.1080799337539,
-23.3069498505864)) ;
#54141 = CARTESIAN_POINT('Ctrl Pts',(-16.0384403140804,-16.1008000918637,
-23.3071808862148)) ;
#54142 = CARTESIAN_POINT('Ctrl Pts',(-16.1065559229815,-16.0931892946344,
-23.3096305503542)) ;
#54143 = CARTESIAN_POINT('Ctrl Pts',(-16.173962499105,-16.085300212968,-23.3142034852872)) ;
#54144 = CARTESIAN_POINT('Ctrl Pts',(-16.2419187343181,-16.0773468007022,
-23.3188137096865)) ;
#54145 = CARTESIAN_POINT('Ctrl Pts',(-16.3091538518471,-16.0691106491231,
-23.3255818058591)) ;
#54146 = CARTESIAN_POINT('Ctrl Pts',(-16.3753756010958,-16.0606518030569,
-23.3343602006664)) ;
#54147 = CARTESIAN_POINT('Ctrl Pts',(-16.429606984231,-16.0537245483846,-23.3415491453487)) ;
#54148 = CARTESIAN_POINT('Ctrl Pts',(-16.4831589859123,-16.0466480826281,
-23.3500853008595)) ;
#54149 = CARTESIAN_POINT('Ctrl Pts',(-16.5358829682123,-16.0394576303854,
-23.3598645671713)) ;
#54150 = CARTESIAN_POINT('Ctrl Pts',(-16.6003696635835,-16.0306629892537,
-23.3718255864285)) ;
#54151 = CARTESIAN_POINT('Ctrl Pts',(-16.6652712594621,-16.0214720150687,
-23.3859543361279)) ;
#54152 = CARTESIAN_POINT('Ctrl Pts',(-16.7302598209164,-16.0119118209662,
-23.4023266027586)) ;
#54153 = CARTESIAN_POINT('Ctrl Pts',(-16.7947161076464,-16.002429927561,-23.4185647758886)) ;
#54154 = CARTESIAN_POINT('Ctrl Pts',(-16.8592574549723,-15.9925848997543,
-23.437009939767)) ;
#54155 = CARTESIAN_POINT('Ctrl Pts',(-16.9235610994876,-15.9824119250012,
-23.4576857441875)) ;
#54156 = CARTESIAN_POINT('Ctrl Pts',(-16.9763607728054,-15.9740589032139,
-23.4746626313798)) ;
#54157 = CARTESIAN_POINT('Ctrl Pts',(-17.0290000063144,-15.9654849570548,
-23.4931425081888)) ;
#54158 = CARTESIAN_POINT('Ctrl Pts',(-17.081302226758,-15.9567135267635,-23.513112533685)) ;
#54159 = CARTESIAN_POINT('Ctrl Pts',(-17.1468251058111,-15.9457249040773,
-23.53813046895)) ;
#54160 = CARTESIAN_POINT('Ctrl Pts',(-17.2118283732285,-15.9344245942977,
-23.5654919651982)) ;
#54161 = CARTESIAN_POINT('Ctrl Pts',(-17.2760008863226,-15.9228603613504,
-23.5951359228588)) ;
#54162 = CARTESIAN_POINT('Ctrl Pts',(-17.2980265101066,-15.9188912251585,
-23.6053104762216)) ;
#54163 = CARTESIAN_POINT('Ctrl Pts',(-17.3199543797531,-15.9148910519162,
-23.6157534777929)) ;
#54164 = CARTESIAN_POINT('Ctrl Pts',(-17.341772320495,-15.9108619321403,-23.6264611079952)) ;
#54165 = CARTESIAN_POINT('',(-18.1258609279822,-15.9108618949459,-23.0304124971064)) ;
#54166 = CARTESIAN_POINT('Origin',(-2.92277791062251E-15,-15.9108618782028,
0.)) ;
#54167 = CARTESIAN_POINT('',(-18.6151833408184,-16.1877442736409,-20.6843103790748)) ;
#54168 = CARTESIAN_POINT('Ctrl Pts',(-18.125860892512,-15.9108619279123,-23.0304125002963)) ;
#54169 = CARTESIAN_POINT('Ctrl Pts',(-18.1128070149588,-15.9226009254264,
-22.9608160051258)) ;
#54170 = CARTESIAN_POINT('Ctrl Pts',(-18.1021710767023,-15.9340937834842,
-22.8909211929491)) ;
#54171 = CARTESIAN_POINT('Ctrl Pts',(-18.0939464864751,-15.9452906639301,
-22.8210441736094)) ;
#54172 = CARTESIAN_POINT('Ctrl Pts',(-18.0911235988425,-15.9491337168313,
-22.7970606111163)) ;
#54173 = CARTESIAN_POINT('Ctrl Pts',(-18.0885843270955,-15.9529419531994,
-22.7730791549778)) ;
#54174 = CARTESIAN_POINT('Ctrl Pts',(-18.0863270012958,-15.9567135267635,
-22.7491125625987)) ;
#54175 = CARTESIAN_POINT('Ctrl Pts',(-18.0799419440817,-15.9673817754481,
-22.6813208138021)) ;
#54176 = CARTESIAN_POINT('Ctrl Pts',(-18.0758156169796,-15.9777576912907,
-22.6136386231626)) ;
#54177 = CARTESIAN_POINT('Ctrl Pts',(-18.0738807325195,-15.9877997661727,
-22.5463776196913)) ;
#54178 = CARTESIAN_POINT('Ctrl Pts',(-18.0719300836305,-15.9979236586405,
-22.478568608663)) ;
#54179 = CARTESIAN_POINT('Ctrl Pts',(-18.0722066052329,-16.0077081692739,
-22.4111881670463)) ;
#54180 = CARTESIAN_POINT('Ctrl Pts',(-18.0745898578821,-16.0171189356799,
-22.3445447344199)) ;
#54181 = CARTESIAN_POINT('Ctrl Pts',(-18.0765401548637,-16.0248200870132,
-22.2900081390048)) ;
#54182 = CARTESIAN_POINT('Ctrl Pts',(-18.0799002354814,-16.0322710948773,
-22.2359649921384)) ;
#54183 = CARTESIAN_POINT('Ctrl Pts',(-18.0845800323485,-16.0394576303854,
-22.1825756662427)) ;
#54184 = CARTESIAN_POINT('Ctrl Pts',(-18.090305931517,-16.0482506141108,-22.1172519127896)) ;
#54185 = CARTESIAN_POINT('Ctrl Pts',(-18.0981556757857,-16.0568730319548,
-22.0512320338478)) ;
#54186 = CARTESIAN_POINT('Ctrl Pts',(-18.1082354095076,-16.0652608298863,
-21.9848300368986)) ;
#54187 = CARTESIAN_POINT('Ctrl Pts',(-18.1182325187418,-16.0735798722807,
-21.9189723431157)) ;
#54188 = CARTESIAN_POINT('Ctrl Pts',(-18.1304233240958,-16.0816680200506,
-21.8527392404316)) ;
#54189 = CARTESIAN_POINT('Ctrl Pts',(-18.1448613717095,-16.0894673869308,
-21.7864465332374)) ;
#54190 = CARTESIAN_POINT('Ctrl Pts',(-18.1567251909072,-16.0958761674667,
-21.7319734691972)) ;
#54191 = CARTESIAN_POINT('Ctrl Pts',(-18.1701054477303,-16.1020900207684,
-21.6774604597971)) ;
#54192 = CARTESIAN_POINT('Ctrl Pts',(-18.1850056852781,-16.108079933754,-21.6230840828955)) ;
#54193 = CARTESIAN_POINT('Ctrl Pts',(-18.2036616583526,-16.1155796568301,
-21.5550016633967)) ;
#54194 = CARTESIAN_POINT('Ctrl Pts',(-18.2247043725071,-16.1227292229207,
-21.4871235794238)) ;
#54195 = CARTESIAN_POINT('Ctrl Pts',(-18.2481015867369,-16.1294814162035,
-21.4197653949614)) ;
#54196 = CARTESIAN_POINT('Ctrl Pts',(-18.2714525404223,-16.1362202591732,
-21.3525403898704)) ;
#54197 = CARTESIAN_POINT('Ctrl Pts',(-18.2971485994912,-16.1425632136357,
-21.2858337267049)) ;
#54198 = CARTESIAN_POINT('Ctrl Pts',(-18.3251073869094,-16.1484717649149,
-21.2199495290698)) ;
#54199 = CARTESIAN_POINT('Ctrl Pts',(-18.3461926369402,-16.1529277264406,
-21.1702626539049)) ;
#54200 = CARTESIAN_POINT('Ctrl Pts',(-18.3685637559296,-16.1571367885211,
-21.1210434058756)) ;
#54201 = CARTESIAN_POINT('Ctrl Pts',(-18.39216711438,-16.1610860188908,-21.0724160582178)) ;
#54202 = CARTESIAN_POINT('Ctrl Pts',(-18.4248195455367,-16.166549308068,-21.0051459226958)) ;
#54203 = CARTESIAN_POINT('Ctrl Pts',(-18.4598543886873,-16.171518536629,-20.9389641426716)) ;
#54204 = CARTESIAN_POINT('Ctrl Pts',(-18.4970921817568,-16.1759680067789,
-20.8741815268919)) ;
#54205 = CARTESIAN_POINT('Ctrl Pts',(-18.5343299748059,-16.1804174769264,
-20.809398911148)) ;
#54206 = CARTESIAN_POINT('Ctrl Pts',(-18.5737703452613,-16.1843471450139,
-20.746015973611)) ;
#54207 = CARTESIAN_POINT('Ctrl Pts',(-18.6151833408574,-16.1877442734701,
-20.6843103789655)) ;
#54208 = CARTESIAN_POINT('',(-19.6196936640125,-15.9108618782028,-21.7718710526408)) ;
#54209 = CARTESIAN_POINT('Ctrl Pts',(-19.6196936640131,-15.9108618782028,
-21.7718710526403)) ;
#54210 = CARTESIAN_POINT('Ctrl Pts',(-19.1108419877152,-16.051097157933,-21.2211268600534)) ;
#54211 = CARTESIAN_POINT('Ctrl Pts',(-18.6151833407114,-16.1877442737198,
-20.6843103792598)) ;
#54212 = CARTESIAN_POINT('',(-20.67775192637,-15.9108618782028,-20.7696250296921)) ;
#54213 = CARTESIAN_POINT('Origin',(-2.92277791062251E-15,-15.9108618782028,
0.)) ;
#54214 = CARTESIAN_POINT('',(-19.6461693467843,-16.1877442736409,-19.7077085595372)) ;
#54215 = CARTESIAN_POINT('Ctrl Pts',(-19.6461693469749,-16.1877442737198,
-19.7077085594403)) ;
#54216 = CARTESIAN_POINT('Ctrl Pts',(-20.1553641225658,-16.0510971577741,
-20.2317029393282)) ;
#54217 = CARTESIAN_POINT('Ctrl Pts',(-20.6777519263695,-15.9108618782028,
-20.7696250296926)) ;
#54218 = CARTESIAN_POINT('',(-22.0153220853232,-15.9108618949459,-19.3461191882741)) ;
#54219 = CARTESIAN_POINT('Ctrl Pts',(-19.646169346673,-16.1877442734701,-19.7077085595702)) ;
#54220 = CARTESIAN_POINT('Ctrl Pts',(-19.710026499131,-16.1843471450139,-19.6696969732475)) ;
#54221 = CARTESIAN_POINT('Ctrl Pts',(-19.7754517387404,-16.1804174769264,
-19.6337459285543)) ;
#54222 = CARTESIAN_POINT('Ctrl Pts',(-19.8421553586713,-16.1759680067789,
-19.6000700080484)) ;
#54223 = CARTESIAN_POINT('Ctrl Pts',(-19.9088589786389,-16.171518536629,-19.5663940875241)) ;
#54224 = CARTESIAN_POINT('Ctrl Pts',(-19.9768404455518,-16.166549308068,-19.5349936353279)) ;
#54225 = CARTESIAN_POINT('Ctrl Pts',(-20.0457796906103,-16.1610860188908,
-19.506031023492)) ;
#54226 = CARTESIAN_POINT('Ctrl Pts',(-20.1118347802969,-16.155851292919,-19.4782800969949)) ;
#54227 = CARTESIAN_POINT('Ctrl Pts',(-20.178811653805,-16.1501596984485,-19.4527490484184)) ;
#54228 = CARTESIAN_POINT('Ctrl Pts',(-20.2464125993028,-16.1440425621064,
-19.4295409361418)) ;
#54229 = CARTESIAN_POINT('Ctrl Pts',(-20.3141532070876,-16.1379127878752,
-19.4062848763401)) ;
#54230 = CARTESIAN_POINT('Ctrl Pts',(-20.3825199747161,-16.1313557844546,
-19.3853614990262)) ;
#54231 = CARTESIAN_POINT('Ctrl Pts',(-20.4512007972396,-16.1244124680041,
-19.3668244541829)) ;
#54232 = CARTESIAN_POINT('Ctrl Pts',(-20.5029529309569,-16.119180564422,-19.3528564848399)) ;
#54233 = CARTESIAN_POINT('Ctrl Pts',(-20.554883073648,-16.1137295207043,-19.3402424104641)) ;
#54234 = CARTESIAN_POINT('Ctrl Pts',(-20.606855606863,-16.1080799337539,-19.3289859803215)) ;
#54235 = CARTESIAN_POINT('Ctrl Pts',(-20.6738254274474,-16.1008000918637,
-19.3144813745146)) ;
#54236 = CARTESIAN_POINT('Ctrl Pts',(-20.7408751366427,-16.0931892946345,
-19.3022309244371)) ;
#54237 = CARTESIAN_POINT('Ctrl Pts',(-20.8076888303103,-16.0853002129681,
-19.2922065253502)) ;
#54238 = CARTESIAN_POINT('Ctrl Pts',(-20.8750473484763,-16.0773468007024,
-19.2821003834662)) ;
#54239 = CARTESIAN_POINT('Ctrl Pts',(-20.9421654869339,-16.0691106491234,
-19.2742566824985)) ;
#54240 = CARTESIAN_POINT('Ctrl Pts',(-21.0087261038809,-16.0606518030573,
-19.268594124726)) ;
#54241 = CARTESIAN_POINT('Ctrl Pts',(-21.0632349980193,-16.0537245483848,
-19.2639568515705)) ;
#54242 = CARTESIAN_POINT('Ctrl Pts',(-21.1173700047693,-16.0466480826282,
-19.2607813391335)) ;
#54243 = CARTESIAN_POINT('Ctrl Pts',(-21.1709635828472,-16.0394576303853,
-19.2589978739486)) ;
#54244 = CARTESIAN_POINT('Ctrl Pts',(-21.236513880691,-16.0306629892538,-19.2568165179308)) ;
#54245 = CARTESIAN_POINT('Ctrl Pts',(-21.3029353768662,-16.0214720150689,
-19.2566630206773)) ;
#54246 = CARTESIAN_POINT('Ctrl Pts',(-21.3699240952328,-16.0119118209665,
-19.2586818931478)) ;
#54247 = CARTESIAN_POINT('Ctrl Pts',(-21.4363641570234,-16.0024299275614,
-19.260684230481)) ;
#54248 = CARTESIAN_POINT('Ctrl Pts',(-21.503361728513,-15.9925848997548,-19.2648236748315)) ;
#54249 = CARTESIAN_POINT('Ctrl Pts',(-21.570606676331,-15.9824119250018,-19.2711927076656)) ;
#54250 = CARTESIAN_POINT('Ctrl Pts',(-21.6258214515424,-15.9740589032143,
-19.2764223156535)) ;
#54251 = CARTESIAN_POINT('Ctrl Pts',(-21.6812026362782,-15.965484957055,-19.2831542640125)) ;
#54252 = CARTESIAN_POINT('Ctrl Pts',(-21.736575025046,-15.9567135267634,-19.2914139700576)) ;
#54253 = CARTESIAN_POINT('Ctrl Pts',(-21.8059441321483,-15.9457249040784,
-19.3017615177437)) ;
#54254 = CARTESIAN_POINT('Ctrl Pts',(-21.8753095721824,-15.9344245943001,
-19.3145095364013)) ;
#54255 = CARTESIAN_POINT('Ctrl Pts',(-21.9443543422025,-15.9228603613541,
-19.3296652414138)) ;
#54256 = CARTESIAN_POINT('Ctrl Pts',(-21.968052255654,-15.9188912237726,-19.3348670631533)) ;
#54257 = CARTESIAN_POINT('Ctrl Pts',(-21.9917124088085,-15.914891049119,-19.3403520713795)) ;
#54258 = CARTESIAN_POINT('Ctrl Pts',(-22.0153220904287,-15.9108619279123,
-19.3461191530285)) ;
#54259 = CARTESIAN_POINT('',(-22.6529462781943,-15.9108618960635,-18.5954499255471)) ;
#54260 = CARTESIAN_POINT('Origin',(-2.92277791062251E-15,-15.9108618782028,
0.)) ;
#54261 = CARTESIAN_POINT('',(-22.6264860066071,-16.1877442736409,-16.1990085395056)) ;
#54262 = CARTESIAN_POINT('Ctrl Pts',(-22.6529462422389,-15.9108619316234,
-18.5954499384047)) ;
#54263 = CARTESIAN_POINT('Ctrl Pts',(-22.6252363683656,-15.9226009290868,
-18.5302867682431)) ;
#54264 = CARTESIAN_POINT('Ctrl Pts',(-22.599823774383,-15.9340937870884,-18.4643124701177)) ;
#54265 = CARTESIAN_POINT('Ctrl Pts',(-22.5767699773912,-15.945290667473,-18.3978371803287)) ;
#54266 = CARTESIAN_POINT('Ctrl Pts',(-22.5688573329178,-15.9491337191718,
-18.3750211845709)) ;
#54267 = CARTESIAN_POINT('Ctrl Pts',(-22.5612221261822,-15.9529419543584,
-18.3521462769307)) ;
#54268 = CARTESIAN_POINT('Ctrl Pts',(-22.5538654687518,-15.9567135267635,
-18.3292252755274)) ;
#54269 = CARTESIAN_POINT('Ctrl Pts',(-22.5330564685454,-15.9673817754482,
-18.2643910587044)) ;
#54270 = CARTESIAN_POINT('Ctrl Pts',(-22.5144769423616,-15.9777576912909,
-18.1991782784233)) ;
#54271 = CARTESIAN_POINT('Ctrl Pts',(-22.4981281668995,-15.987799766173,-18.133905742799)) ;
#54272 = CARTESIAN_POINT('Ctrl Pts',(-22.4816461901464,-15.9979236586409,
-18.0681014006162)) ;
#54273 = CARTESIAN_POINT('Ctrl Pts',(-22.4674314436314,-16.0077081692744,
-18.0022368323092)) ;
#54274 = CARTESIAN_POINT('Ctrl Pts',(-22.4554326091091,-16.0171189356805,
-17.9366391572315)) ;
#54275 = CARTESIAN_POINT('Ctrl Pts',(-22.4456135533074,-16.0248200870136,
-17.8829583409114)) ;
#54276 = CARTESIAN_POINT('Ctrl Pts',(-22.4372773980355,-16.0322710948774,
-17.8294563747781)) ;
#54277 = CARTESIAN_POINT('Ctrl Pts',(-22.4303706569622,-16.0394576303854,
-17.7763092436615)) ;
#54278 = CARTESIAN_POINT('Ctrl Pts',(-22.4219200117541,-16.0482506141108,
-17.7112818241983)) ;
#54279 = CARTESIAN_POINT('Ctrl Pts',(-22.4153939109251,-16.0568730319548,
-17.6451179903573)) ;
#54280 = CARTESIAN_POINT('Ctrl Pts',(-22.410963519559,-16.0652608298863,-17.5781015904011)) ;
#54281 = CARTESIAN_POINT('Ctrl Pts',(-22.406569444511,-16.0735798722807,-17.5116345299279)) ;
#54282 = CARTESIAN_POINT('Ctrl Pts',(-22.4042370763699,-16.0816680200506,
-17.4443292575847)) ;
#54283 = CARTESIAN_POINT('Ctrl Pts',(-22.4040865980054,-16.0894673869308,
-17.3764826835936)) ;
#54284 = CARTESIAN_POINT('Ctrl Pts',(-22.4039629491467,-16.0958761674667,
-17.3207327990841)) ;
#54285 = CARTESIAN_POINT('Ctrl Pts',(-22.4053116973728,-16.1020900207684,
-17.2646179138511)) ;
#54286 = CARTESIAN_POINT('Ctrl Pts',(-22.4081742619674,-16.108079933754,-17.2083097157992)) ;
#54287 = CARTESIAN_POINT('Ctrl Pts',(-22.4117583610684,-16.1155796568301,
-17.1378085426898)) ;
#54288 = CARTESIAN_POINT('Ctrl Pts',(-22.4177173266673,-16.1227292229207,
-17.0669938490745)) ;
#54289 = CARTESIAN_POINT('Ctrl Pts',(-22.4260875084648,-16.1294814162036,
-16.9961807520905)) ;
#54290 = CARTESIAN_POINT('Ctrl Pts',(-22.4344411408918,-16.1362202591732,
-16.9255076654682)) ;
#54291 = CARTESIAN_POINT('Ctrl Pts',(-22.4451964796334,-16.1425632136357,
-16.8548366738882)) ;
#54292 = CARTESIAN_POINT('Ctrl Pts',(-22.4583384511702,-16.1484717649149,
-16.7844824993424)) ;
#54293 = CARTESIAN_POINT('Ctrl Pts',(-22.4682495303456,-16.1529277264406,
-16.7314245702261)) ;
#54294 = CARTESIAN_POINT('Ctrl Pts',(-22.4795169415893,-16.1571367885211,
-16.6785469115667)) ;
#54295 = CARTESIAN_POINT('Ctrl Pts',(-22.4921150243034,-16.1610860188908,
-16.6259824199178)) ;
#54296 = CARTESIAN_POINT('Ctrl Pts',(-22.5095429691188,-16.166549308068,-16.5532657152817)) ;
#54297 = CARTESIAN_POINT('Ctrl Pts',(-22.5295315907202,-16.171518536629,-16.4810997728415)) ;
#54298 = CARTESIAN_POINT('Ctrl Pts',(-22.5519724374491,-16.1759680067789,
-16.4098267138496)) ;
#54299 = CARTESIAN_POINT('Ctrl Pts',(-22.5744132841656,-16.1804174769265,
-16.3385536548968)) ;
#54300 = CARTESIAN_POINT('Ctrl Pts',(-22.5993061026932,-16.184347145014,-16.2681740614176)) ;
#54301 = CARTESIAN_POINT('Ctrl Pts',(-22.6264860066216,-16.1877442734701,
-16.1990085393905)) ;
#54302 = CARTESIAN_POINT('',(-23.841304833414,-15.9108618782028,-17.0452026225194)) ;
#54303 = CARTESIAN_POINT('Ctrl Pts',(-23.841304833414,-15.9108618782028,-17.0452026225194)) ;
#54304 = CARTESIAN_POINT('Ctrl Pts',(-23.2259561080038,-16.0510971572507,
-16.6167225940414)) ;
#54305 = CARTESIAN_POINT('Ctrl Pts',(-22.6264860065426,-16.1877442737199,
-16.1990085397092)) ;
#54306 = CARTESIAN_POINT('',(-24.6591730128172,-15.9108618782028,-15.8389373042025)) ;
#54307 = CARTESIAN_POINT('Origin',(-2.92277791062251E-15,-15.9108618782028,
0.)) ;
#54308 = CARTESIAN_POINT('',(-23.4234276096243,-16.1877442736409,-15.0236076122501)) ;
#54309 = CARTESIAN_POINT('Ctrl Pts',(-23.4234276097895,-16.1877442737199,
-15.0236076121148)) ;
#54310 = CARTESIAN_POINT('Ctrl Pts',(-24.0333609985744,-16.0510971574224,
-15.4258894705628)) ;
#54311 = CARTESIAN_POINT('Ctrl Pts',(-24.6591730128173,-15.9108618782028,
-15.8389373042025)) ;
#54312 = CARTESIAN_POINT('',(-25.6594598237771,-15.9108618960635,-14.1611741945453)) ;
#54313 = CARTESIAN_POINT('Ctrl Pts',(-23.4234276095227,-16.1877442734701,
-15.0236076123062)) ;
#54314 = CARTESIAN_POINT('Ctrl Pts',(-23.4776204497976,-16.184347145014,-14.9727573155735)) ;
#54315 = CARTESIAN_POINT('Ctrl Pts',(-23.5337876717588,-16.1804174769265,
-14.9235822937669)) ;
#54316 = CARTESIAN_POINT('Ctrl Pts',(-23.5916924706681,-16.1759680067789,
-14.8763543910281)) ;
#54317 = CARTESIAN_POINT('Ctrl Pts',(-23.6495972696091,-16.171518536629,-14.8291264882633)) ;
#54318 = CARTESIAN_POINT('Ctrl Pts',(-23.7092391985723,-16.166549308068,-14.7838461553214)) ;
#54319 = CARTESIAN_POINT('Ctrl Pts',(-23.7703405769756,-16.1610860188908,
-14.7407407733973)) ;
#54320 = CARTESIAN_POINT('Ctrl Pts',(-23.8288857064871,-16.155851292919,-14.6994387564324)) ;
#54321 = CARTESIAN_POINT('Ctrl Pts',(-23.8888082771604,-16.1501596984486,
-14.6601065616019)) ;
#54322 = CARTESIAN_POINT('Ctrl Pts',(-23.949839692006,-16.1440425621066,-14.6229088370813)) ;
#54323 = CARTESIAN_POINT('Ctrl Pts',(-24.0109971966116,-16.1379127878754,
-14.5856342627586)) ;
#54324 = CARTESIAN_POINT('Ctrl Pts',(-24.0732676795727,-16.1313557844549,
-14.5505032282463)) ;
#54325 = CARTESIAN_POINT('Ctrl Pts',(-24.1363578659418,-16.1244124680045,
-14.5176352225583)) ;
#54326 = CARTESIAN_POINT('Ctrl Pts',(-24.1838973630142,-16.1191805644222,
-14.4928686376089)) ;
#54327 = CARTESIAN_POINT('Ctrl Pts',(-24.2319017547066,-16.1137295207044,
-14.4693860276473)) ;
#54328 = CARTESIAN_POINT('Ctrl Pts',(-24.2802393992346,-16.108079933754,-14.4472202082417)) ;
#54329 = CARTESIAN_POINT('Ctrl Pts',(-24.3425254411343,-16.1008000918637,
-14.4186581802463)) ;
#54330 = CARTESIAN_POINT('Ctrl Pts',(-24.4053740807431,-16.0931892946345,
-14.392280433382)) ;
#54331 = CARTESIAN_POINT('Ctrl Pts',(-24.4684707578974,-16.0853002129681,
-14.3681274300352)) ;
#54332 = CARTESIAN_POINT('Ctrl Pts',(-24.5320819495711,-16.0773468007023,
-14.3437774738302)) ;
#54333 = CARTESIAN_POINT('Ctrl Pts',(-24.5959447393999,-16.0691106491233,
-14.3216887384619)) ;
#54334 = CARTESIAN_POINT('Ctrl Pts',(-24.6597319235742,-16.0606518030571,
-14.3018500030175)) ;
#54335 = CARTESIAN_POINT('Ctrl Pts',(-24.7119695534068,-16.0537245483847,
-14.2856033457633)) ;
#54336 = CARTESIAN_POINT('Ctrl Pts',(-24.7641562724755,-16.0466480826282,
-14.2708646488106)) ;
#54337 = CARTESIAN_POINT('Ctrl Pts',(-24.8161134701841,-16.0394576303854,
-14.2576018449789)) ;
#54338 = CARTESIAN_POINT('Ctrl Pts',(-24.8796623114282,-16.0306629892537,
-14.241380111469)) ;
#54339 = CARTESIAN_POINT('Ctrl Pts',(-24.9444979125622,-16.0214720150687,
-14.2269515446236)) ;
#54340 = CARTESIAN_POINT('Ctrl Pts',(-25.0103544698237,-16.0119118209663,
-14.2145226227012)) ;
#54341 = CARTESIAN_POINT('Ctrl Pts',(-25.0756716432292,-16.0024299275612,
-14.2021954971695)) ;
#54342 = CARTESIAN_POINT('Ctrl Pts',(-25.1419927069031,-15.9925848997546,
-14.1918356661752)) ;
#54343 = CARTESIAN_POINT('Ctrl Pts',(-25.2090346590021,-15.9824119250015,
-14.1836001185266)) ;
#54344 = CARTESIAN_POINT('Ctrl Pts',(-25.2640827545833,-15.9740589032141,
-14.1768379166526)) ;
#54345 = CARTESIAN_POINT('Ctrl Pts',(-25.3196163278975,-15.9654849570549,
-14.1715071581381)) ;
#54346 = CARTESIAN_POINT('Ctrl Pts',(-25.3754697336308,-15.9567135267634,
-14.1676703300569)) ;
#54347 = CARTESIAN_POINT('Ctrl Pts',(-25.4454414464462,-15.9457249040773,
-14.1628636503371)) ;
#54348 = CARTESIAN_POINT('Ctrl Pts',(-25.5159256082289,-15.9344245942979,
-14.160402108223)) ;
#54349 = CARTESIAN_POINT('Ctrl Pts',(-25.5866141784799,-15.9228603613507,
-14.1603608966696)) ;
#54350 = CARTESIAN_POINT('Ctrl Pts',(-25.6108762783375,-15.918891224989,-14.1603467518252)) ;
#54351 = CARTESIAN_POINT('Ctrl Pts',(-25.635162377422,-15.9148910515742,-14.1606172898976)) ;
#54352 = CARTESIAN_POINT('Ctrl Pts',(-25.6594598224132,-15.9108619316234,
-14.1611741563845)) ;
#54353 = CARTESIAN_POINT('',(-26.1208051708581,-15.9108618823941,-13.2909850543147)) ;
#54354 = CARTESIAN_POINT('Origin',(-2.92277791062251E-15,-15.9108618782028,
0.)) ;
#54355 = CARTESIAN_POINT('',(-25.5797993342587,-16.1877442736409,-10.9562590645362)) ;
#54356 = CARTESIAN_POINT('Ctrl Pts',(-26.1208051521851,-15.9108618900532,
-13.2909850310202)) ;
#54357 = CARTESIAN_POINT('Ctrl Pts',(-26.0797349595563,-15.9226008880842,
-13.2333021464419)) ;
#54358 = CARTESIAN_POINT('Ctrl Pts',(-26.0407339689744,-15.9340937467161,
-13.1743332500262)) ;
#54359 = CARTESIAN_POINT('Ctrl Pts',(-26.0039289294952,-15.9452906277871,
-13.1143680028723)) ;
#54360 = CARTESIAN_POINT('Ctrl Pts',(-25.9912964683392,-15.9491336929542,
-13.0937863470422)) ;
#54361 = CARTESIAN_POINT('Ctrl Pts',(-25.9789222960317,-15.9529419413758,
-13.0730875148955)) ;
#54362 = CARTESIAN_POINT('Ctrl Pts',(-25.96681025371,-15.9567135267635,-13.0522837860431)) ;
#54363 = CARTESIAN_POINT('Ctrl Pts',(-25.9325503162336,-15.9673817754482,
-12.9934386771153)) ;
#54364 = CARTESIAN_POINT('Ctrl Pts',(-25.9003863489627,-15.9777576912909,
-12.9337445843205)) ;
#54365 = CARTESIAN_POINT('Ctrl Pts',(-25.8703881330689,-15.987799766173,-12.8735125877646)) ;
#54366 = CARTESIAN_POINT('Ctrl Pts',(-25.8401455073662,-15.9979236586409,
-12.8127898523318)) ;
#54367 = CARTESIAN_POINT('Ctrl Pts',(-25.8121041584821,-16.0077081692744,
-12.7515209113459)) ;
#54368 = CARTESIAN_POINT('Ctrl Pts',(-25.7862842889548,-16.0171189356805,
-12.6900362681975)) ;
#54369 = CARTESIAN_POINT('Ctrl Pts',(-25.765155008506,-16.0248200870136,-12.6397212862801)) ;
#54370 = CARTESIAN_POINT('Ctrl Pts',(-25.7455124067001,-16.0322710948774,
-12.589262193352)) ;
#54371 = CARTESIAN_POINT('Ctrl Pts',(-25.7273420792229,-16.0394576303854,
-12.5388423577955)) ;
#54372 = CARTESIAN_POINT('Ctrl Pts',(-25.7051100324156,-16.0482506141109,
-12.477151882183)) ;
#54373 = CARTESIAN_POINT('Ctrl Pts',(-25.6845132397104,-16.0568730319549,
-12.4139378407768)) ;
#54374 = CARTESIAN_POINT('Ctrl Pts',(-25.6657798834323,-16.0652608298865,
-12.3494406501917)) ;
#54375 = CARTESIAN_POINT('Ctrl Pts',(-25.6472000861677,-16.0735798722809,
-12.2854721489032)) ;
#54376 = CARTESIAN_POINT('Ctrl Pts',(-25.6304536034734,-16.0816680200508,
-12.220241826631)) ;
#54377 = CARTESIAN_POINT('Ctrl Pts',(-25.6157216353318,-16.089467386931,-12.154013816237)) ;
#54378 = CARTESIAN_POINT('Ctrl Pts',(-25.6036163001002,-16.0958761674668,
-12.0995939138967)) ;
#54379 = CARTESIAN_POINT('Ctrl Pts',(-25.5928704737616,-16.1020900207685,
-12.0445010224976)) ;
#54380 = CARTESIAN_POINT('Ctrl Pts',(-25.583561515064,-16.1080799337539,-11.9888939120547)) ;
#54381 = CARTESIAN_POINT('Ctrl Pts',(-25.5719061517011,-16.11557965683,-11.9192705418331)) ;
#54382 = CARTESIAN_POINT('Ctrl Pts',(-25.5625027341359,-16.1227292229207,
-11.8488304549445)) ;
#54383 = CARTESIAN_POINT('Ctrl Pts',(-25.555454503103,-16.1294814162035,-11.7778735871511)) ;
#54384 = CARTESIAN_POINT('Ctrl Pts',(-25.5484202077037,-16.1362202591731,
-11.7070570139801)) ;
#54385 = CARTESIAN_POINT('Ctrl Pts',(-25.5437319184324,-16.1425632136356,
-11.6357261910069)) ;
#54386 = CARTESIAN_POINT('Ctrl Pts',(-25.5414425701049,-16.1484717649147,
-11.5641917225591)) ;
#54387 = CARTESIAN_POINT('Ctrl Pts',(-25.5397160473781,-16.1529277264405,
-11.5102436692869)) ;
#54388 = CARTESIAN_POINT('Ctrl Pts',(-25.5393528992489,-16.1571367885211,
-11.4561801005468)) ;
#54389 = CARTESIAN_POINT('Ctrl Pts',(-25.5403566338809,-16.1610860188908,
-11.4021363221146)) ;
#54390 = CARTESIAN_POINT('Ctrl Pts',(-25.541745181025,-16.166549308068,-11.3273732006547)) ;
#54391 = CARTESIAN_POINT('Ctrl Pts',(-25.5457529353466,-16.171518536629,-11.2525974950609)) ;
#54392 = CARTESIAN_POINT('Ctrl Pts',(-25.5523475266828,-16.1759680067789,
-11.1781666418811)) ;
#54393 = CARTESIAN_POINT('Ctrl Pts',(-25.5589421180155,-16.1804174769264,
-11.1037357887422)) ;
#54394 = CARTESIAN_POINT('Ctrl Pts',(-25.568123424087,-16.184347145014,-11.0296504108911)) ;
#54395 = CARTESIAN_POINT('Ctrl Pts',(-25.579799334248,-16.1877442734701,-10.9562590644207)) ;
#54396 = CARTESIAN_POINT('',(-26.9481230865112,-15.9108618782028,-11.5215194621523)) ;
#54397 = CARTESIAN_POINT('Ctrl Pts',(-26.9481230865112,-15.9108618782028,
-11.5215194621523)) ;
#54398 = CARTESIAN_POINT('Ctrl Pts',(-26.2550503307714,-16.0510971574997,
-11.2353388445058)) ;
#54399 = CARTESIAN_POINT('Ctrl Pts',(-25.5797993342394,-16.1877442737198,
-10.9562590647489)) ;
#54400 = CARTESIAN_POINT('',(-27.4875585758881,-15.9108618782028,-10.167638474082)) ;
#54401 = CARTESIAN_POINT('Origin',(-2.92277791062251E-15,-15.9108618782028,
0.)) ;
#54402 = CARTESIAN_POINT('',(-26.1054324307094,-16.1877442736409,-9.63701947055377)) ;
#54403 = CARTESIAN_POINT('Ctrl Pts',(-26.1054324308417,-16.1877442737199,
-9.637019470386)) ;
#54404 = CARTESIAN_POINT('Ctrl Pts',(-26.7875846245017,-16.0510971573504,
-9.89877855358705)) ;
#54405 = CARTESIAN_POINT('Ctrl Pts',(-27.4875585758881,-15.9108618782028,
-10.1676384740821)) ;
#54406 = CARTESIAN_POINT('',(-28.1037900289265,-15.9108618823941,-8.31406834816473)) ;
#54407 = CARTESIAN_POINT('Ctrl Pts',(-26.1054324306223,-16.1877442734701,
-9.63701947063037)) ;
#54408 = CARTESIAN_POINT('Ctrl Pts',(-26.1474269617335,-16.184347145014,-9.57570816684729)) ;
#54409 = CARTESIAN_POINT('Ctrl Pts',(-26.1917098491728,-16.1804174769264,
-9.51560853729301)) ;
#54410 = CARTESIAN_POINT('Ctrl Pts',(-26.2381082630198,-16.1759680067789,
-9.45703697656336)) ;
#54411 = CARTESIAN_POINT('Ctrl Pts',(-26.2845066768924,-16.171518536629,-9.39846541580148)) ;
#54412 = CARTESIAN_POINT('Ctrl Pts',(-26.3330202775945,-16.166549308068,-9.34142246015677)) ;
#54413 = CARTESIAN_POINT('Ctrl Pts',(-26.3834267567978,-16.1610860188908,
-9.28618986789506)) ;
#54414 = CARTESIAN_POINT('Ctrl Pts',(-26.4317244209472,-16.155851292919,-9.23326799687132)) ;
#54415 = CARTESIAN_POINT('Ctrl Pts',(-26.4817907759808,-16.1501596984485,
-9.1819737855022)) ;
#54416 = CARTESIAN_POINT('Ctrl Pts',(-26.5333988990483,-16.1440425621064,
-9.13252577299347)) ;
#54417 = CARTESIAN_POINT('Ctrl Pts',(-26.5851136435314,-16.1379127878752,
-9.08297560181711)) ;
#54418 = CARTESIAN_POINT('Ctrl Pts',(-26.6383761432513,-16.1313557844547,
-9.03527959823452)) ;
#54419 = CARTESIAN_POINT('Ctrl Pts',(-26.6929256664716,-16.1244124680042,
-8.98961750311754)) ;
#54420 = CARTESIAN_POINT('Ctrl Pts',(-26.734029632851,-16.119180564422,-8.95521036054868)) ;
#54421 = CARTESIAN_POINT('Ctrl Pts',(-26.7758636415409,-16.1137295207043,
-8.9219572357447)) ;
#54422 = CARTESIAN_POINT('Ctrl Pts',(-26.8183061828457,-16.108079933754,-8.8899184761565)) ;
#54423 = CARTESIAN_POINT('Ctrl Pts',(-26.8729960199674,-16.1008000918637,
-8.84863455465709)) ;
#54424 = CARTESIAN_POINT('Ctrl Pts',(-26.9287048574528,-16.0931892946344,
-8.80936290513267)) ;
#54425 = CARTESIAN_POINT('Ctrl Pts',(-26.985134187597,-16.085300212968,-8.77221066511824)) ;
#54426 = CARTESIAN_POINT('Ctrl Pts',(-27.0420236641543,-16.0773468007022,
-8.73475547148128)) ;
#54427 = CARTESIAN_POINT('Ctrl Pts',(-27.0996449522805,-16.0691106491232,
-8.69945454642825)) ;
#54428 = CARTESIAN_POINT('Ctrl Pts',(-27.1576760858445,-16.060651803057,-8.66636727053211)) ;
#54429 = CARTESIAN_POINT('Ctrl Pts',(-27.2051998778583,-16.0537245483846,
-8.63927090481558)) ;
#54430 = CARTESIAN_POINT('Ctrl Pts',(-27.2529981162635,-16.0466480826281,
-8.61365818843598)) ;
#54431 = CARTESIAN_POINT('Ctrl Pts',(-27.3008894727844,-16.0394576303854,
-8.5895361999242)) ;
#54432 = CARTESIAN_POINT('Ctrl Pts',(-27.3594653842418,-16.0306629892537,
-8.56003259915179)) ;
#54433 = CARTESIAN_POINT('Ctrl Pts',(-27.4196834496852,-16.0214720150686,
-8.53200362646388)) ;
#54434 = CARTESIAN_POINT('Ctrl Pts',(-27.4813284664185,-16.0119118209661,
-8.5057080727237)) ;
#54435 = CARTESIAN_POINT('Ctrl Pts',(-27.5424685930055,-16.0024299275609,
-8.4796278870161)) ;
#54436 = CARTESIAN_POINT('Ctrl Pts',(-27.6050120496373,-15.9925848997542,
-8.45525319485998)) ;
#54437 = CARTESIAN_POINT('Ctrl Pts',(-27.6687161988492,-15.9824119250011,
-8.43279815178344)) ;
#54438 = CARTESIAN_POINT('Ctrl Pts',(-27.7210236270318,-15.9740589032138,
-8.41436033309198)) ;
#54439 = CARTESIAN_POINT('Ctrl Pts',(-27.774112900757,-15.9654849570548,-8.39721612804761)) ;
#54440 = CARTESIAN_POINT('Ctrl Pts',(-27.82783568028,-15.9567135267635,-8.38146217165729)) ;
#54441 = CARTESIAN_POINT('Ctrl Pts',(-27.8951381992077,-15.9457249040889,
-8.36172601955273)) ;
#54442 = CARTESIAN_POINT('Ctrl Pts',(-27.963445321592,-15.9344245943217,-8.34417001565522)) ;
#54443 = CARTESIAN_POINT('Ctrl Pts',(-28.0324723730129,-15.9228603613872,
-8.32893381455141)) ;
#54444 = CARTESIAN_POINT('Ctrl Pts',(-28.0561642792868,-15.918891211363,-8.32370434811628)) ;
#54445 = CARTESIAN_POINT('Ctrl Pts',(-28.0799408226937,-15.9148910240721,
-8.31874775162405)) ;
#54446 = CARTESIAN_POINT('Ctrl Pts',(-28.1037899993503,-15.9108618900532,
-8.314068352235)) ;
#54447 = CARTESIAN_POINT('',(-28.3672841893431,-15.9108618818334,-7.36504824030182)) ;
#54448 = CARTESIAN_POINT('Origin',(-2.92277791062251E-15,-15.9108618782028,
0.)) ;
#54449 = CARTESIAN_POINT('',(-27.3370296749455,-16.187744273641,-5.20120709271515)) ;
#54450 = CARTESIAN_POINT('Ctrl Pts',(-28.3672841674668,-15.9108618853164,
-7.36504822386666)) ;
#54451 = CARTESIAN_POINT('Ctrl Pts',(-28.3147740575662,-15.922600883412,-7.31754281092639)) ;
#54452 = CARTESIAN_POINT('Ctrl Pts',(-28.2640083183597,-15.9340937421158,
-7.26833663508417)) ;
#54453 = CARTESIAN_POINT('Ctrl Pts',(-28.2151730041596,-15.9452906232649,
-7.21768533801899)) ;
#54454 = CARTESIAN_POINT('Ctrl Pts',(-28.1984114285588,-15.9491336899667,
-7.20030046891469)) ;
#54455 = CARTESIAN_POINT('Ctrl Pts',(-28.1818769138879,-15.9529419398964,
-7.18274563840582)) ;
#54456 = CARTESIAN_POINT('Ctrl Pts',(-28.1655758512416,-15.9567135267634,
-7.16503201329499)) ;
#54457 = CARTESIAN_POINT('Ctrl Pts',(-28.1194669330942,-15.9673817754482,
-7.11492754415393)) ;
#54458 = CARTESIAN_POINT('Ctrl Pts',(-28.0752224760982,-15.9777576912909,
-7.06354336827925)) ;
#54459 = CARTESIAN_POINT('Ctrl Pts',(-28.0329775030073,-15.987799766173,-7.01116829200742)) ;
#54460 = CARTESIAN_POINT('Ctrl Pts',(-27.9903883399206,-15.9979236586409,
-6.95836649094546)) ;
#54461 = CARTESIAN_POINT('Ctrl Pts',(-27.9498315709757,-16.0077081692744,
-6.90455804486584)) ;
#54462 = CARTESIAN_POINT('Ctrl Pts',(-27.9113979748458,-16.0171189356805,
-6.85006138722518)) ;
#54463 = CARTESIAN_POINT('Ctrl Pts',(-27.8799464514201,-16.0248200870136,
-6.80546491234382)) ;
#54464 = CARTESIAN_POINT('Ctrl Pts',(-27.8499158693093,-16.0322710948774,
-6.76040810372474)) ;
#54465 = CARTESIAN_POINT('Ctrl Pts',(-27.8213315797461,-16.0394576303854,
-6.71507313920122)) ;
#54466 = CARTESIAN_POINT('Ctrl Pts',(-27.7863576771393,-16.0482506141109,
-6.6596041855153)) ;
#54467 = CARTESIAN_POINT('Ctrl Pts',(-27.752653275693,-16.0568730319549,-6.60229575486319)) ;
#54468 = CARTESIAN_POINT('Ctrl Pts',(-27.7204929054219,-16.0652608298865,
-6.54333359059779)) ;
#54469 = CARTESIAN_POINT('Ctrl Pts',(-27.6885961566106,-16.0735798722809,
-6.48485474451842)) ;
#54470 = CARTESIAN_POINT('Ctrl Pts',(-27.6582186062815,-16.0816680200509,
-6.42474946968839)) ;
#54471 = CARTESIAN_POINT('Ctrl Pts',(-27.6295939988196,-16.0894673869311,
-6.36323677105028)) ;
#54472 = CARTESIAN_POINT('Ctrl Pts',(-27.6060730092364,-16.0958761674669,
-6.3126914650289)) ;
#54473 = CARTESIAN_POINT('Ctrl Pts',(-27.5837350712296,-16.1020900207685,
-6.26119664983373)) ;
#54474 = CARTESIAN_POINT('Ctrl Pts',(-27.5626898658027,-16.1080799337539,
-6.20889075368096)) ;
#54475 = CARTESIAN_POINT('Ctrl Pts',(-27.5363400318123,-16.1155796568301,
-6.14340069775686)) ;
#54476 = CARTESIAN_POINT('Ctrl Pts',(-27.512013924437,-16.1227292229208,-6.07662891776802)) ;
#54477 = CARTESIAN_POINT('Ctrl Pts',(-27.4898768480231,-16.1294814162037,
-6.00884614343911)) ;
#54478 = CARTESIAN_POINT('Ctrl Pts',(-27.4677835406323,-16.1362202591734,
-5.94119738797336)) ;
#54479 = CARTESIAN_POINT('Ctrl Pts',(-27.4478708425436,-16.142563213636,-5.87254208360997)) ;
#54480 = CARTESIAN_POINT('Ctrl Pts',(-27.4302572217353,-16.1484717649152,
-5.80317219349924)) ;
#54481 = CARTESIAN_POINT('Ctrl Pts',(-27.4169738273903,-16.1529277264408,
-5.75085656708513)) ;
#54482 = CARTESIAN_POINT('Ctrl Pts',(-27.4049971002915,-16.1571367885212,
-5.69813504065318)) ;
#54483 = CARTESIAN_POINT('Ctrl Pts',(-27.3943595533256,-16.1610860188908,
-5.64513900245386)) ;
#54484 = CARTESIAN_POINT('Ctrl Pts',(-27.3796437758774,-16.166549308068,-5.57182530463607)) ;
#54485 = CARTESIAN_POINT('Ctrl Pts',(-27.3674832647814,-16.171518536629,-5.4979362647745)) ;
#54486 = CARTESIAN_POINT('Ctrl Pts',(-27.3579232449636,-16.1759680067789,
-5.42382792137737)) ;
#54487 = CARTESIAN_POINT('Ctrl Pts',(-27.348363225151,-16.1804174769265,-5.34971957802103)) ;
#54488 = CARTESIAN_POINT('Ctrl Pts',(-27.3414037110988,-16.184347145014,-5.27539256572608)) ;
#54489 = CARTESIAN_POINT('Ctrl Pts',(-27.3370296749104,-16.1877442734702,
-5.20120709260462)) ;
#54490 = CARTESIAN_POINT('',(-28.7948770547711,-15.9108618782028,-5.4591028569837)) ;
#54491 = CARTESIAN_POINT('Ctrl Pts',(-28.7948770547711,-15.9108618782028,
-5.45910285698361)) ;
#54492 = CARTESIAN_POINT('Ctrl Pts',(-28.0564875827971,-16.0510971572643,
-5.32860313876284)) ;
#54493 = CARTESIAN_POINT('Ctrl Pts',(-27.3370296749724,-16.1877442737199,
-5.20120709292708)) ;
#54494 = CARTESIAN_POINT('',(-29.0306564501774,-15.9108618782028,-4.02091216943199)) ;
#54495 = CARTESIAN_POINT('Origin',(-2.92277791062251E-15,-15.9108618782028,
0.)) ;
#54496 = CARTESIAN_POINT('',(-27.5667762454386,-16.1877442736409,-3.79981500919265)) ;
#54497 = CARTESIAN_POINT('Ctrl Pts',(-27.5667762455317,-16.1877442737199,
-3.79981500900038)) ;
#54498 = CARTESIAN_POINT('Ctrl Pts',(-28.2892505640487,-16.0510971575924,
-3.90881175274295)) ;
#54499 = CARTESIAN_POINT('Ctrl Pts',(-29.0306564501774,-15.9108618782028,
-4.02091216943207)) ;
#54500 = CARTESIAN_POINT('',(-29.2340179925284,-15.9108618818334,-2.0782059266231)) ;
#54501 = CARTESIAN_POINT('Ctrl Pts',(-27.56677624537,-16.1877442734702,-3.79981500928619)) ;
#54502 = CARTESIAN_POINT('Ctrl Pts',(-27.5946088497164,-16.184347145014,-3.73090954687479)) ;
#54503 = CARTESIAN_POINT('Ctrl Pts',(-27.624936784034,-16.1804174769265,-3.66269550145485)) ;
#54504 = CARTESIAN_POINT('Ctrl Pts',(-27.6576592745555,-16.1759680067789,
-3.59551902381641)) ;
#54505 = CARTESIAN_POINT('Ctrl Pts',(-27.690381765095,-16.171518536629,-3.528342546141)) ;
#54506 = CARTESIAN_POINT('Ctrl Pts',(-27.7254985954864,-16.166549308068,-3.46220423300075)) ;
#54507 = CARTESIAN_POINT('Ctrl Pts',(-27.7628532245447,-16.1610860188908,
-3.39742704502896)) ;
#54508 = CARTESIAN_POINT('Ctrl Pts',(-27.798645078235,-16.155851292919,-3.33535988781728)) ;
#54509 = CARTESIAN_POINT('Ctrl Pts',(-27.8365141705119,-16.1501596984485,
-3.27450212022401)) ;
#54510 = CARTESIAN_POINT('Ctrl Pts',(-27.8762858633247,-16.1440425621065,
-3.21511595383477)) ;
#54511 = CARTESIAN_POINT('Ctrl Pts',(-27.9161397237098,-16.1379127878753,
-3.15560709673814)) ;
#54512 = CARTESIAN_POINT('Ctrl Pts',(-27.9579037448983,-16.1313557844547,
-3.09757633620262)) ;
#54513 = CARTESIAN_POINT('Ctrl Pts',(-28.001361929891,-16.1244124680043,-3.04125526047473)) ;
#54514 = CARTESIAN_POINT('Ctrl Pts',(-28.034108389794,-16.1191805644221,-2.99881640003158)) ;
#54515 = CARTESIAN_POINT('Ctrl Pts',(-28.067815903731,-16.1137295207043,-2.95734763954236)) ;
#54516 = CARTESIAN_POINT('Ctrl Pts',(-28.1023787757534,-16.1080799337539,
-2.91693403656097)) ;
#54517 = CARTESIAN_POINT('Ctrl Pts',(-28.1469151720963,-16.1008000918637,
-2.86485861184352)) ;
#54518 = CARTESIAN_POINT('Ctrl Pts',(-28.1928793241329,-16.0931892946345,
-2.81452935834372)) ;
#54519 = CARTESIAN_POINT('Ctrl Pts',(-28.2400027345056,-16.0853002129681,
-2.76611507911336)) ;
#54520 = CARTESIAN_POINT('Ctrl Pts',(-28.2875104072504,-16.0773468007024,
-2.71730601127082)) ;
#54521 = CARTESIAN_POINT('Ctrl Pts',(-28.3361958862822,-16.0691106491234,
-2.67044352855458)) ;
#54522 = CARTESIAN_POINT('Ctrl Pts',(-28.3857574979268,-16.0606518030573,
-2.62565483645402)) ;
#54523 = CARTESIAN_POINT('Ctrl Pts',(-28.4263452924272,-16.0537245483848,
-2.58897575821992)) ;
#54524 = CARTESIAN_POINT('Ctrl Pts',(-28.4675200576659,-16.0466480826283,
-2.55368664456423)) ;
#54525 = CARTESIAN_POINT('Ctrl Pts',(-28.5091062263966,-16.0394576303854,
-2.51983338874492)) ;
#54526 = CARTESIAN_POINT('Ctrl Pts',(-28.5599702635483,-16.0306629892539,
-2.47842747629227)) ;
#54527 = CARTESIAN_POINT('Ctrl Pts',(-28.6127550634868,-16.021472015069,-2.43810870137365)) ;
#54528 = CARTESIAN_POINT('Ctrl Pts',(-28.6673060872213,-16.0119118209667,
-2.399176066684)) ;
#54529 = CARTESIAN_POINT('Ctrl Pts',(-28.7214103226214,-16.0024299275618,
-2.36056230129898)) ;
#54530 = CARTESIAN_POINT('Ctrl Pts',(-28.7772517096891,-15.9925848997552,
-2.32331248149642)) ;
#54531 = CARTESIAN_POINT('Ctrl Pts',(-28.834639320797,-15.9824119250023,-2.28768791584975)) ;
#54532 = CARTESIAN_POINT('Ctrl Pts',(-28.8817602443783,-15.9740589032147,
-2.25843661224884)) ;
#54533 = CARTESIAN_POINT('Ctrl Pts',(-28.929922823083,-15.9654849570552,-2.23028060464648)) ;
#54534 = CARTESIAN_POINT('Ctrl Pts',(-28.9790029589372,-15.9567135267634,
-2.20334615743715)) ;
#54535 = CARTESIAN_POINT('Ctrl Pts',(-29.0404892930589,-15.9457249040904,
-2.16960337348452)) ;
#54536 = CARTESIAN_POINT('Ctrl Pts',(-29.1034254109862,-15.9344245943247,
-2.13777380703749)) ;
#54537 = CARTESIAN_POINT('Ctrl Pts',(-29.1675633154367,-15.9228603613918,
-2.10805504422152)) ;
#54538 = CARTESIAN_POINT('Ctrl Pts',(-29.1895771460413,-15.9188912098107,
-2.09785477628302)) ;
#54539 = CARTESIAN_POINT('Ctrl Pts',(-29.2117322940924,-15.9148910209385,
-2.08790280445291)) ;
#54540 = CARTESIAN_POINT('Ctrl Pts',(-29.2340179665494,-15.9108618853164,
-2.07820593521283)) ;
#54541 = CARTESIAN_POINT('',(-29.2873405113753,-15.9108618818334,-1.09472993550088)) ;
#54542 = CARTESIAN_POINT('Origin',(-2.92277791062251E-15,-15.9108618782028,
0.)) ;
#54543 = CARTESIAN_POINT('',(-27.8160108909582,-16.1877442736409,0.797047542034005)) ;
#54544 = CARTESIAN_POINT('Ctrl Pts',(-29.2873404864774,-15.9108618853164,
-1.09472992415271)) ;
#54545 = CARTESIAN_POINT('Ctrl Pts',(-29.2258457742339,-15.922600883412,-1.0596232828087)) ;
#54546 = CARTESIAN_POINT('Ctrl Pts',(-29.1656890365171,-15.9340937421157,
-1.02248065331821)) ;
#54547 = CARTESIAN_POINT('Ctrl Pts',(-29.1071069331975,-15.9452906232649,
-0.983511704422473)) ;
#54548 = CARTESIAN_POINT('Ctrl Pts',(-29.0870000009552,-15.9491336899667,
-0.970136527182337)) ;
#54549 = CARTESIAN_POINT('Ctrl Pts',(-29.0670782844065,-15.9529419398964,
-0.95654655075281)) ;
#54550 = CARTESIAN_POINT('Ctrl Pts',(-29.0473504257583,-15.9567135267634,
-0.942751306966341)) ;
#54551 = CARTESIAN_POINT('Ctrl Pts',(-28.9915485287064,-15.9673817754481,
-0.903730306902203)) ;
#54552 = CARTESIAN_POINT('Ctrl Pts',(-28.9372924036204,-15.9777576912908,
-0.863058714902215)) ;
#54553 = CARTESIAN_POINT('Ctrl Pts',(-28.8847760013223,-15.9877997661729,
-0.820989559270527)) ;
#54554 = CARTESIAN_POINT('Ctrl Pts',(-28.8318317227835,-15.9979236586407,
-0.778577646112123)) ;
#54555 = CARTESIAN_POINT('Ctrl Pts',(-28.7806559232182,-16.0077081692741,
-0.734745718073906)) ;
#54556 = CARTESIAN_POINT('Ctrl Pts',(-28.7314057127251,-16.0171189356801,
-0.68978524908376)) ;
#54557 = CARTESIAN_POINT('Ctrl Pts',(-28.6911025846015,-16.0248200870134,
-0.652992562838112)) ;
#54558 = CARTESIAN_POINT('Ctrl Pts',(-28.6520882188283,-16.0322710948773,
-0.615444844821693)) ;
#54559 = CARTESIAN_POINT('Ctrl Pts',(-28.6144265367895,-16.0394576303853,
-0.577314563885692)) ;
#54560 = CARTESIAN_POINT('Ctrl Pts',(-28.5683461191982,-16.0482506141109,
-0.530660798751411)) ;
#54561 = CARTESIAN_POINT('Ctrl Pts',(-28.5231100893626,-16.056873031955,-0.481937657376859)) ;
#54562 = CARTESIAN_POINT('Ctrl Pts',(-28.4790264882685,-16.0652608298866,
-0.431267524700463)) ;
#54563 = CARTESIAN_POINT('Ctrl Pts',(-28.4353042444341,-16.0735798722811,
-0.381012739678)) ;
#54564 = CARTESIAN_POINT('Ctrl Pts',(-28.3927160469611,-16.0816680200511,
-0.328842968138768)) ;
#54565 = CARTESIAN_POINT('Ctrl Pts',(-28.3515372550096,-16.0894673869314,
-0.274921846678084)) ;
#54566 = CARTESIAN_POINT('Ctrl Pts',(-28.3177004264064,-16.095876167467,-0.230614579308406)) ;
#54567 = CARTESIAN_POINT('Ctrl Pts',(-28.2848148738862,-16.1020900207686,
-0.185125680643661)) ;
#54568 = CARTESIAN_POINT('Ctrl Pts',(-28.2530174721459,-16.108079933754,-0.13856676435159)) ;
#54569 = CARTESIAN_POINT('Ctrl Pts',(-28.2132052564801,-16.1155796568301,
-0.0802722649541275)) ;
#54570 = CARTESIAN_POINT('Ctrl Pts',(-28.1750939210392,-16.1227292229208,
-0.0202909660870273)) ;
#54571 = CARTESIAN_POINT('Ctrl Pts',(-28.138903104334,-16.1294814162037,0.0411482675837251)) ;
#54572 = CARTESIAN_POINT('Ctrl Pts',(-28.1027838434504,-16.1362202591734,
0.102466024724218)) ;
#54573 = CARTESIAN_POINT('Ctrl Pts',(-28.0685778321754,-16.1425632136359,
0.165235564750095)) ;
#54574 = CARTESIAN_POINT('Ctrl Pts',(-28.036463532219,-16.1484717649151,0.229197217560653)) ;
#54575 = CARTESIAN_POINT('Ctrl Pts',(-28.0122443830118,-16.1529277264407,
0.277434196571948)) ;
#54576 = CARTESIAN_POINT('Ctrl Pts',(-27.9892140953912,-16.1571367885212,
0.326348480717388)) ;
#54577 = CARTESIAN_POINT('Ctrl Pts',(-27.9674326667007,-16.1610860188908,
0.375818742840291)) ;
#54578 = CARTESIAN_POINT('Ctrl Pts',(-27.9373006580581,-16.166549308068,0.444254949988105)) ;
#54579 = CARTESIAN_POINT('Ctrl Pts',(-27.909540493528,-16.171518536629,0.513802354735114)) ;
#54580 = CARTESIAN_POINT('Ctrl Pts',(-27.8842728784576,-16.1759680067789,
0.584122964577656)) ;
#54581 = CARTESIAN_POINT('Ctrl Pts',(-27.859005263401,-16.1804174769265,0.654443574381521)) ;
#54582 = CARTESIAN_POINT('Ctrl Pts',(-27.8362303483673,-16.184347145014,0.725536772633798)) ;
#54583 = CARTESIAN_POINT('Ctrl Pts',(-27.8160108909,-16.1877442734702,0.797047542134341)) ;
#54584 = CARTESIAN_POINT('',(-29.2952145751572,-15.9108618782028,0.858575330420999)) ;
#54585 = CARTESIAN_POINT('Ctrl Pts',(-29.2952145751572,-15.9108618782028,
0.858575330421035)) ;
#54586 = CARTESIAN_POINT('Ctrl Pts',(-28.5460346555085,-16.0510971575125,
0.827292127857017)) ;
#54587 = CARTESIAN_POINT('Ctrl Pts',(-27.8160108910301,-16.1877442737199,
0.79704754183291)) ;
#54588 = CARTESIAN_POINT('',(-29.2163130941136,-15.9108618782028,2.31382751933691)) ;
#54589 = CARTESIAN_POINT('Origin',(-2.92277791062251E-15,-15.9108618782028,
0.)) ;
#54590 = CARTESIAN_POINT('',(-27.7391282412025,-16.1877442736409,2.21506457880742)) ;
#54591 = CARTESIAN_POINT('Ctrl Pts',(-27.7391282412522,-16.1877442737199,
2.21506457901514)) ;
#54592 = CARTESIAN_POINT('Ctrl Pts',(-28.4681425923452,-16.0510971570914,
2.26392674104202)) ;
#54593 = CARTESIAN_POINT('Ctrl Pts',(-29.2163130941136,-15.9108618782028,
2.31382751933687)) ;
#54594 = CARTESIAN_POINT('',(-28.9972957403971,-15.9108618818334,4.25483109005219)) ;
#54595 = CARTESIAN_POINT('Ctrl Pts',(-27.7391282411555,-16.1877442734701,
2.21506457870136)) ;
#54596 = CARTESIAN_POINT('Ctrl Pts',(-27.7514974970917,-16.184347145014,2.28834225690161)) ;
#54597 = CARTESIAN_POINT('Ctrl Pts',(-27.766452377786,-16.1804174769264,2.36148110523782)) ;
#54598 = CARTESIAN_POINT('Ctrl Pts',(-27.7839688776935,-16.1759680067789,
2.43412140235194)) ;
#54599 = CARTESIAN_POINT('Ctrl Pts',(-27.8014853776107,-16.171518536629,2.50676169950601)) ;
#54600 = CARTESIAN_POINT('Ctrl Pts',(-27.8215634137317,-16.166549308068,2.57890281612686)) ;
#54601 = CARTESIAN_POINT('Ctrl Pts',(-27.8441195317072,-16.1610860188908,
2.65019569049379)) ;
#54602 = CARTESIAN_POINT('Ctrl Pts',(-27.8657319876396,-16.155851292919,2.71850594260504)) ;
#54603 = CARTESIAN_POINT('Ctrl Pts',(-27.8896331004936,-16.1501596984485,
2.78608162484854)) ;
#54604 = CARTESIAN_POINT('Ctrl Pts',(-27.9157086828988,-16.1440425621064,
2.85262911398106)) ;
#54605 = CARTESIAN_POINT('Ctrl Pts',(-27.9418381369688,-16.1379127878752,
2.91931408897965)) ;
#54606 = CARTESIAN_POINT('Ctrl Pts',(-27.9701508404126,-16.1313557844547,
2.98496615260209)) ;
#54607 = CARTESIAN_POINT('Ctrl Pts',(-28.000485630748,-16.1244124680042,3.04931269803643)) ;
#54608 = CARTESIAN_POINT('Ctrl Pts',(-28.0233433961044,-16.119180564422,3.09779888240661)) ;
#54609 = CARTESIAN_POINT('Ctrl Pts',(-28.0473482893997,-16.1137295207043,
3.14554424542948)) ;
#54610 = CARTESIAN_POINT('Ctrl Pts',(-28.0724153706577,-16.108079933754,3.19244299664483)) ;
#54611 = CARTESIAN_POINT('Ctrl Pts',(-28.1047158538276,-16.1008000918638,
3.25287493559833)) ;
#54612 = CARTESIAN_POINT('Ctrl Pts',(-28.138786087752,-16.0931892946346,3.31190845311691)) ;
#54613 = CARTESIAN_POINT('Ctrl Pts',(-28.1744001400584,-16.0853002129682,
3.36932097367515)) ;
#54614 = CARTESIAN_POINT('Ctrl Pts',(-28.2103046030145,-16.0773468007025,
3.42720165795851)) ;
#54615 = CARTESIAN_POINT('Ctrl Pts',(-28.2477777940625,-16.0691106491235,
3.48343446072996)) ;
#54616 = CARTESIAN_POINT('Ctrl Pts',(-28.2865524379113,-16.0606518030574,
3.53783029957149)) ;
#54617 = CARTESIAN_POINT('Ctrl Pts',(-28.318306394737,-16.0537245483849,3.58237701739061)) ;
#54618 = CARTESIAN_POINT('Ctrl Pts',(-28.3509324005486,-16.0466480826283,
3.62569244858873)) ;
#54619 = CARTESIAN_POINT('Ctrl Pts',(-28.3842688584583,-16.0394576303854,
3.66769403109849)) ;
#54620 = CARTESIAN_POINT('Ctrl Pts',(-28.4250426754601,-16.0306629892538,
3.71906616078553)) ;
#54621 = CARTESIAN_POINT('Ctrl Pts',(-28.4679260513165,-16.0214720150689,
3.76978947683178)) ;
#54622 = CARTESIAN_POINT('Ctrl Pts',(-28.5128323368133,-16.0119118209665,
3.81953874574425)) ;
#54623 = CARTESIAN_POINT('Ctrl Pts',(-28.5573708271134,-16.0024299275614,
3.86888055405428)) ;
#54624 = CARTESIAN_POINT('Ctrl Pts',(-28.6038990634226,-15.9925848997548,
3.91726374133018)) ;
#54625 = CARTESIAN_POINT('Ctrl Pts',(-28.6522867555149,-15.9824119250018,
3.96439206445185)) ;
#54626 = CARTESIAN_POINT('Ctrl Pts',(-28.6920178524757,-15.9740589032143,
4.00308909451437)) ;
#54627 = CARTESIAN_POINT('Ctrl Pts',(-28.733001707505,-15.965484957055,4.04094036105058)) ;
#54628 = CARTESIAN_POINT('Ctrl Pts',(-28.775144267083,-15.9567135267634,4.07779587426135)) ;
#54629 = CARTESIAN_POINT('Ctrl Pts',(-28.8279393837613,-15.9457249040904,
4.12396751498949)) ;
#54630 = CARTESIAN_POINT('Ctrl Pts',(-28.8825616743147,-15.9344245943247,
4.1685823288369)) ;
#54631 = CARTESIAN_POINT('Ctrl Pts',(-28.9388114146762,-15.9228603613918,
4.21139403704719)) ;
#54632 = CARTESIAN_POINT('Ctrl Pts',(-28.9581178180656,-15.9188912098107,
4.22608815124554)) ;
#54633 = CARTESIAN_POINT('Ctrl Pts',(-28.9776156113019,-15.9148910209385,
4.24057015343419)) ;
#54634 = CARTESIAN_POINT('Ctrl Pts',(-28.9972957168721,-15.9108618853164,
4.25483107607861)) ;
#54635 = CARTESIAN_POINT('',(-28.8379530854688,-15.9108618948274,5.22677683844469)) ;
#54636 = CARTESIAN_POINT('Origin',(-2.92277791062251E-15,-15.9108618782028,
0.)) ;
#54637 = CARTESIAN_POINT('',(-26.9943463529852,-16.1877442736409,6.75803311957258)) ;
#54638 = CARTESIAN_POINT('Ctrl Pts',(-28.8379530716378,-15.9108619275541,
5.22677680590787)) ;
#54639 = CARTESIAN_POINT('Ctrl Pts',(-28.7703491834565,-15.9226009250731,
5.24784313359756)) ;
#54640 = CARTESIAN_POINT('Ctrl Pts',(-28.7036143117797,-15.9340937831364,
5.27118547398356)) ;
#54641 = CARTESIAN_POINT('Ctrl Pts',(-28.6380246560567,-15.9452906635882,
5.29664993508353)) ;
#54642 = CARTESIAN_POINT('Ctrl Pts',(-28.6155126246555,-15.9491337166054,
5.30538998321425)) ;
#54643 = CARTESIAN_POINT('Ctrl Pts',(-28.5931353023263,-15.9529419530875,
5.31437962277664)) ;
#54644 = CARTESIAN_POINT('Ctrl Pts',(-28.5709031781777,-15.9567135267634,
5.32361140268328)) ;
#54645 = CARTESIAN_POINT('Ctrl Pts',(-28.5080175369082,-15.9673817754481,
5.34972435507637)) ;
#54646 = CARTESIAN_POINT('Ctrl Pts',(-28.4462866998398,-15.9777576912908,
5.37778160476311)) ;
#54647 = CARTESIAN_POINT('Ctrl Pts',(-28.3859544769382,-15.9877997661729,
5.40757773279399)) ;
#54648 = CARTESIAN_POINT('Ctrl Pts',(-28.3251306985681,-15.9979236586407,
5.4376166241273)) ;
#54649 = CARTESIAN_POINT('Ctrl Pts',(-28.265728791892,-16.0077081692741,5.46942250188518)) ;
#54650 = CARTESIAN_POINT('Ctrl Pts',(-28.2079648521405,-16.0171189356801,
5.50274448066511)) ;
#54651 = CARTESIAN_POINT('Ctrl Pts',(-28.1606946487967,-16.0248200870134,
5.53001299315784)) ;
#54652 = CARTESIAN_POINT('Ctrl Pts',(-28.1145207677436,-16.0322710948773,
5.55829593100791)) ;
#54653 = CARTESIAN_POINT('Ctrl Pts',(-28.0695427116236,-16.0394576303853,
5.58743859879807)) ;
#54654 = CARTESIAN_POINT('Ctrl Pts',(-28.0145104481598,-16.0482506141109,
5.62309569717482)) ;
#54655 = CARTESIAN_POINT('Ctrl Pts',(-27.9598579764138,-16.056873031955,5.66095530933291)) ;
#54656 = CARTESIAN_POINT('Ctrl Pts',(-27.9059124446885,-16.0652608298867,
5.70096413133199)) ;
#54657 = CARTESIAN_POINT('Ctrl Pts',(-27.8524091093593,-16.0735798722811,
5.74064499740345)) ;
#54658 = CARTESIAN_POINT('Ctrl Pts',(-27.7996016415232,-16.0816680200511,
5.7824398651166)) ;
#54659 = CARTESIAN_POINT('Ctrl Pts',(-27.7477941396272,-16.0894673869313,
5.82624811768868)) ;
#54660 = CARTESIAN_POINT('Ctrl Pts',(-27.7052236445022,-16.0958761674669,
5.86224558782921)) ;
#54661 = CARTESIAN_POINT('Ctrl Pts',(-27.6633281693541,-16.1020900207685,
5.89960155962014)) ;
#54662 = CARTESIAN_POINT('Ctrl Pts',(-27.6222653824652,-16.1080799337539,
5.93823645287304)) ;
#54663 = CARTESIAN_POINT('Ctrl Pts',(-27.5708523600797,-16.1155796568302,
5.98660960974249)) ;
#54664 = CARTESIAN_POINT('Ctrl Pts',(-27.5207378402602,-16.1227292229209,
6.03699576861805)) ;
#54665 = CARTESIAN_POINT('Ctrl Pts',(-27.4721855256291,-16.1294814162039,
6.08921863134986)) ;
#54666 = CARTESIAN_POINT('Ctrl Pts',(-27.4237292077474,-16.1362202591736,
6.14133823999151)) ;
#54667 = CARTESIAN_POINT('Ctrl Pts',(-27.3768293183559,-16.1425632136362,
6.19528698175209)) ;
#54668 = CARTESIAN_POINT('Ctrl Pts',(-27.3317159682247,-16.1484717649154,
6.25084962146588)) ;
#54669 = CARTESIAN_POINT('Ctrl Pts',(-27.2976935246555,-16.1529277264409,
6.29275244554604)) ;
#54670 = CARTESIAN_POINT('Ctrl Pts',(-27.2646865471668,-16.1571367885212,
6.3355723098413)) ;
#54671 = CARTESIAN_POINT('Ctrl Pts',(-27.2327797121498,-16.1610860188907,
6.37920362141181)) ;
#54672 = CARTESIAN_POINT('Ctrl Pts',(-27.1886404115476,-16.166549308068,6.43956233690491)) ;
#54673 = CARTESIAN_POINT('Ctrl Pts',(-27.1465786280237,-16.171518536629,6.50151614718778)) ;
#54674 = CARTESIAN_POINT('Ctrl Pts',(-27.1067849032983,-16.1759680067789,
6.56476090991532)) ;
#54675 = CARTESIAN_POINT('Ctrl Pts',(-27.0669911785948,-16.1804174769265,
6.62800567260807)) ;
#54676 = CARTESIAN_POINT('Ctrl Pts',(-27.0294657922941,-16.184347145014,6.69254081788182)) ;
#54677 = CARTESIAN_POINT('Ctrl Pts',(-26.9943463529069,-16.1877442734701,
6.75803311965814)) ;
#54678 = CARTESIAN_POINT('',(-28.4257404213015,-15.9108618782028,7.13610748961195)) ;
#54679 = CARTESIAN_POINT('Ctrl Pts',(-28.4257404213014,-15.9108618782028,
7.1361074896125)) ;
#54680 = CARTESIAN_POINT('Ctrl Pts',(-27.7008008765093,-16.0510971573508,
6.94450413403671)) ;
#54681 = CARTESIAN_POINT('Ctrl Pts',(-26.9943463530986,-16.1877442737199,
6.75803311939151)) ;
#54682 = CARTESIAN_POINT('',(-28.0358474093686,-15.9108618782028,8.54037520493741)) ;
#54683 = CARTESIAN_POINT('Origin',(-2.92277791062251E-15,-15.9108618782028,
0.)) ;
#54684 = CARTESIAN_POINT('',(-26.6144294302345,-16.1877442736409,8.12637020896991)) ;
#54685 = CARTESIAN_POINT('Ctrl Pts',(-26.6144294302383,-16.1877442737199,
8.12637020918352)) ;
#54686 = CARTESIAN_POINT('Ctrl Pts',(-27.315895907299,-16.0510971577038,8.3308065360743)) ;
#54687 = CARTESIAN_POINT('Ctrl Pts',(-28.0358474093688,-15.9108618782028,
8.54037520493686)) ;
#54688 = CARTESIAN_POINT('',(-27.4046920069319,-15.9108618948274,10.3889167040556)) ;
#54689 = CARTESIAN_POINT('Ctrl Pts',(-26.6144294302115,-16.1877442734702,
8.12637020885619)) ;
#54690 = CARTESIAN_POINT('Ctrl Pts',(-26.6107569650772,-16.184347145014,8.20059372005496)) ;
#54691 = CARTESIAN_POINT('Ctrl Pts',(-26.6096395185481,-16.1804174769265,
8.27523748004725)) ;
#54692 = CARTESIAN_POINT('Ctrl Pts',(-26.6111309757742,-16.1759680067789,
8.34994501707787)) ;
#54693 = CARTESIAN_POINT('Ctrl Pts',(-26.6126224330011,-16.171518536629,8.4246525541496)) ;
#54694 = CARTESIAN_POINT('Ctrl Pts',(-26.6167228481979,-16.166549308068,8.49942323581695)) ;
#54695 = CARTESIAN_POINT('Ctrl Pts',(-26.6234257560832,-16.1610860188908,
8.57389822100999)) ;
#54696 = CARTESIAN_POINT('Ctrl Pts',(-26.6298482398389,-16.155851292919,8.64525745655306)) ;
#54697 = CARTESIAN_POINT('Ctrl Pts',(-26.6386637837969,-16.1501596984486,
8.7163912896496)) ;
#54698 = CARTESIAN_POINT('Ctrl Pts',(-26.6498239905421,-16.1440425621066,
8.78698841489538)) ;
#54699 = CARTESIAN_POINT('Ctrl Pts',(-26.6610072540654,-16.1379127878754,
8.85773139247953)) ;
#54700 = CARTESIAN_POINT('Ctrl Pts',(-26.6745447692185,-16.1313557844549,
8.92793494166045)) ;
#54701 = CARTESIAN_POINT('Ctrl Pts',(-26.690337743815,-16.1244124680045,8.99729818385233)) ;
#54702 = CARTESIAN_POINT('Ctrl Pts',(-26.7022380109217,-16.1191805644222,
9.04956453205789)) ;
#54703 = CARTESIAN_POINT('Ctrl Pts',(-26.7154178414446,-16.1137295207044,
9.10135397750546)) ;
#54704 = CARTESIAN_POINT('Ctrl Pts',(-26.7298170230788,-16.108079933754,9.15254494347305)) ;
#54705 = CARTESIAN_POINT('Ctrl Pts',(-26.7483712583824,-16.1008000918637,
9.21850766636298)) ;
#54706 = CARTESIAN_POINT('Ctrl Pts',(-26.7689544879227,-16.0931892946345,
9.28348510623268)) ;
#54707 = CARTESIAN_POINT('Ctrl Pts',(-26.7913939086595,-16.085300212968,9.34721132246741)) ;
#54708 = CARTESIAN_POINT('Ctrl Pts',(-26.8140163090442,-16.0773468007022,
9.41145718672468)) ;
#54709 = CARTESIAN_POINT('Ctrl Pts',(-26.8385250073438,-16.0691106491232,
9.47443092619252)) ;
#54710 = CARTESIAN_POINT('Ctrl Pts',(-26.8646996241457,-16.0606518030571,
9.53589042280775)) ;
#54711 = CARTESIAN_POINT('Ctrl Pts',(-26.8861349635669,-16.0537245483847,
9.58622182519577)) ;
#54712 = CARTESIAN_POINT('Ctrl Pts',(-26.9086866541803,-16.0466480826282,
9.63553819251415)) ;
#54713 = CARTESIAN_POINT('Ctrl Pts',(-26.9322146255474,-16.0394576303854,
9.68372415439674)) ;
#54714 = CARTESIAN_POINT('Ctrl Pts',(-26.9609916840328,-16.0306629892538,
9.74266039762971)) ;
#54715 = CARTESIAN_POINT('Ctrl Pts',(-26.991968456813,-16.0214720150688,9.8014164889199)) ;
#54716 = CARTESIAN_POINT('Ctrl Pts',(-27.0251302360714,-16.0119118209664,
9.85965617153281)) ;
#54717 = CARTESIAN_POINT('Ctrl Pts',(-27.0580204109656,-16.0024299275614,
9.91741885465047)) ;
#54718 = CARTESIAN_POINT('Ctrl Pts',(-27.0930598878988,-15.9925848997548,
9.97467306533666)) ;
#54719 = CARTESIAN_POINT('Ctrl Pts',(-27.1301851062715,-15.9824119250018,
10.0311014779233)) ;
#54720 = CARTESIAN_POINT('Ctrl Pts',(-27.160668594677,-15.9740589032143,10.077434804331)) ;
#54721 = CARTESIAN_POINT('Ctrl Pts',(-27.192557366521,-15.965484957055,10.1232114466471)) ;
#54722 = CARTESIAN_POINT('Ctrl Pts',(-27.225791810576,-15.9567135267634,10.168264703024)) ;
#54723 = CARTESIAN_POINT('Ctrl Pts',(-27.2674270688776,-15.9457249040784,
10.2247062659845)) ;
#54724 = CARTESIAN_POINT('Ctrl Pts',(-27.3111814545091,-15.9344245943002,
10.2800201881814)) ;
#54725 = CARTESIAN_POINT('Ctrl Pts',(-27.3569128554931,-15.9228603613542,
10.3339230139472)) ;
#54726 = CARTESIAN_POINT('Ctrl Pts',(-27.372609030806,-15.9188912236551,10.3524238292486)) ;
#54727 = CARTESIAN_POINT('Ctrl Pts',(-27.3885377175626,-15.914891048882,10.3707586359222)) ;
#54728 = CARTESIAN_POINT('Ctrl Pts',(-27.4046919783062,-15.9108619275541,
10.3889167248043)) ;
#54729 = CARTESIAN_POINT('',(-27.040135303883,-15.9108618883339,11.303885129792)) ;
#54730 = CARTESIAN_POINT('Origin',(-2.92277791062251E-15,-15.9108618782028,
0.)) ;
#54731 = CARTESIAN_POINT('',(-24.9104561816077,-16.1877442736409,12.4030205794544)) ;
#54732 = CARTESIAN_POINT('Ctrl Pts',(-27.040135269086,-15.9108619232992,11.3038851331636)) ;
#54733 = CARTESIAN_POINT('Ctrl Pts',(-26.9695832844262,-15.9226009208762,
11.3099261036344)) ;
#54734 = CARTESIAN_POINT('Ctrl Pts',(-26.8993907236594,-15.934093779004,11.3183766877575)) ;
#54735 = CARTESIAN_POINT('Ctrl Pts',(-26.8298604110735,-15.945290659526,11.3291459661828)) ;
#54736 = CARTESIAN_POINT('Ctrl Pts',(-26.8059958379989,-15.9491337139218,
11.332842256655)) ;
#54737 = CARTESIAN_POINT('Ctrl Pts',(-26.7822091698441,-15.9529419517586,
11.3368112619122)) ;
#54738 = CARTESIAN_POINT('Ctrl Pts',(-26.7585122522638,-15.9567135267634,
11.3410479599125)) ;
#54739 = CARTESIAN_POINT('Ctrl Pts',(-26.6914833294693,-15.9673817754482,
11.3530318520033)) ;
#54740 = CARTESIAN_POINT('Ctrl Pts',(-26.6251642457505,-15.9777576912909,
11.367162833565)) ;
#54741 = CARTESIAN_POINT('Ctrl Pts',(-26.5598372699333,-15.9877997661731,
11.3832927001646)) ;
#54742 = CARTESIAN_POINT('Ctrl Pts',(-26.4939780440072,-15.997923658641,11.3995539845001)) ;
#54743 = CARTESIAN_POINT('Ctrl Pts',(-26.4291275973556,-16.0077081692744,
11.4178466044834)) ;
#54744 = CARTESIAN_POINT('Ctrl Pts',(-26.3655509059679,-16.0171189356805,
11.4379719943604)) ;
#54745 = CARTESIAN_POINT('Ctrl Pts',(-26.3135239295762,-16.0248200870137,
11.4544412877625)) ;
#54746 = CARTESIAN_POINT('Ctrl Pts',(-26.2623495726037,-16.0322710948774,
11.4721369667062)) ;
#54747 = CARTESIAN_POINT('Ctrl Pts',(-26.2121582663181,-16.0394576303854,
11.490929342594)) ;
#54748 = CARTESIAN_POINT('Ctrl Pts',(-26.1507474044579,-16.0482506141109,
11.513922487923)) ;
#54749 = CARTESIAN_POINT('Ctrl Pts',(-26.089233979639,-16.0568730319549,11.5391482974777)) ;
#54750 = CARTESIAN_POINT('Ctrl Pts',(-26.0279489503903,-16.0652608298865,
11.5666250407491)) ;
#54751 = CARTESIAN_POINT('Ctrl Pts',(-25.9671662800619,-16.0735798722808,
11.5938765546741)) ;
#54752 = CARTESIAN_POINT('Ctrl Pts',(-25.9066087603678,-16.0816680200508,
11.6233422369986)) ;
#54753 = CARTESIAN_POINT('Ctrl Pts',(-25.8465950097364,-16.0894673869309,
11.6549891954811)) ;
#54754 = CARTESIAN_POINT('Ctrl Pts',(-25.797281397127,-16.0958761674667,11.6809936666973)) ;
#54755 = CARTESIAN_POINT('Ctrl Pts',(-25.7483349852048,-16.1020900207684,
11.7084699878918)) ;
#54756 = CARTESIAN_POINT('Ctrl Pts',(-25.6999268634434,-16.1080799337539,
11.737374333437)) ;
#54757 = CARTESIAN_POINT('Ctrl Pts',(-25.6393170501245,-16.1155796568301,
11.7735642727251)) ;
#54758 = CARTESIAN_POINT('Ctrl Pts',(-25.5795426451758,-16.1227292229208,
11.8119992908194)) ;
#54759 = CARTESIAN_POINT('Ctrl Pts',(-25.5208990848898,-16.1294814162036,
11.8525638995912)) ;
#54760 = CARTESIAN_POINT('Ctrl Pts',(-25.4623714735797,-16.1362202591733,
11.8930483047598)) ;
#54761 = CARTESIAN_POINT('Ctrl Pts',(-25.4049706927747,-16.1425632136359,
11.9356536650492)) ;
#54762 = CARTESIAN_POINT('Ctrl Pts',(-25.3489677425815,-16.1484717649151,
11.9802192443856)) ;
#54763 = CARTESIAN_POINT('Ctrl Pts',(-25.3067328562967,-16.1529277264407,
12.0138285840543)) ;
#54764 = CARTESIAN_POINT('Ctrl Pts',(-25.265292558521,-16.1571367885212,12.0485518192378)) ;
#54765 = CARTESIAN_POINT('Ctrl Pts',(-25.2247522453195,-16.1610860188908,
12.0843040286216)) ;
#54766 = CARTESIAN_POINT('Ctrl Pts',(-25.1686695573967,-16.166549308068,12.1337629460074)) ;
#54767 = CARTESIAN_POINT('Ctrl Pts',(-25.1142729171279,-16.171518536629,12.1852262705141)) ;
#54768 = CARTESIAN_POINT('Ctrl Pts',(-25.0618137930884,-16.1759680067789,
12.2384379313129)) ;
#54769 = CARTESIAN_POINT('Ctrl Pts',(-25.0093546690776,-16.1804174769265,
12.2916495920825)) ;
#54770 = CARTESIAN_POINT('Ctrl Pts',(-24.9588334568666,-16.184347145014,12.3466090927105)) ;
#54771 = CARTESIAN_POINT('Ctrl Pts',(-24.9104561815128,-16.1877442734702,
12.403020579521)) ;
#54772 = CARTESIAN_POINT('',(-26.2271102382868,-15.9108618782028,13.0799631938038)) ;
#54773 = CARTESIAN_POINT('Ctrl Pts',(-26.2271102382867,-15.9108618782028,
13.0799631938041)) ;
#54774 = CARTESIAN_POINT('Ctrl Pts',(-25.5603084370629,-16.0510971568938,
12.7369988462526)) ;
#54775 = CARTESIAN_POINT('Ctrl Pts',(-24.9104561817574,-16.1877442737198,
12.4030205793021)) ;
#54776 = CARTESIAN_POINT('',(-25.5444566593682,-15.9108618782028,14.3675844378995)) ;
#54777 = CARTESIAN_POINT('Origin',(-2.92277791062251E-15,-15.9108618782028,
0.)) ;
#54778 = CARTESIAN_POINT('',(-24.2452694789224,-16.1877442736409,13.657695799973)) ;
#54779 = CARTESIAN_POINT('Ctrl Pts',(-24.2452694788804,-16.1877442737198,
13.6576958001824)) ;
#54780 = CARTESIAN_POINT('Ctrl Pts',(-24.8863882954023,-16.0510971570495,
14.0081470784022)) ;
#54781 = CARTESIAN_POINT('Ctrl Pts',(-25.5444566593684,-15.9108618782028,
14.3675844378992)) ;
#54782 = CARTESIAN_POINT('',(-24.530675536546,-15.9108618883339,16.0372283765163)) ;
#54783 = CARTESIAN_POINT('Ctrl Pts',(-24.2452694789243,-16.1877442734701,
13.6576957998571)) ;
#54784 = CARTESIAN_POINT('Ctrl Pts',(-24.2257270131077,-16.184347145014,13.7293945351642)) ;
#54785 = CARTESIAN_POINT('Ctrl Pts',(-24.2085894899129,-16.1804174769265,
13.8020529475559)) ;
#54786 = CARTESIAN_POINT('Ctrl Pts',(-24.1939861655753,-16.1759680067789,
13.8753344831029)) ;
#54787 = CARTESIAN_POINT('Ctrl Pts',(-24.1793828412297,-16.171518536629,13.9486160186902)) ;
#54788 = CARTESIAN_POINT('Ctrl Pts',(-24.167313904645,-16.166549308068,14.0225200714308)) ;
#54789 = CARTESIAN_POINT('Ctrl Pts',(-24.1578501819171,-16.1610860188908,
14.0966947999152)) ;
#54790 = CARTESIAN_POINT('Ctrl Pts',(-24.1487823852938,-16.155851292919,14.1677663403465)) ;
#54791 = CARTESIAN_POINT('Ctrl Pts',(-24.1421001553184,-16.1501596984486,
14.2391321853203)) ;
#54792 = CARTESIAN_POINT('Ctrl Pts',(-24.13782314754,-16.1440425621066,14.3104779035662)) ;
#54793 = CARTESIAN_POINT('Ctrl Pts',(-24.1335373035436,-16.1379127878754,
14.3819710207296)) ;
#54794 = CARTESIAN_POINT('Ctrl Pts',(-24.1316666312436,-16.1313557844549,
14.4534434155352)) ;
#54795 = CARTESIAN_POINT('Ctrl Pts',(-24.1321793281619,-16.1244124680045,
14.5245800063717)) ;
#54796 = CARTESIAN_POINT('Ctrl Pts',(-24.1325656537547,-16.1191805644222,
14.5781826020598)) ;
#54797 = CARTESIAN_POINT('Ctrl Pts',(-24.134304147278,-16.1137295207044,14.6315945130223)) ;
#54798 = CARTESIAN_POINT('Ctrl Pts',(-24.1373621395585,-16.108079933754,14.6846840610676)) ;
#54799 = CARTESIAN_POINT('Ctrl Pts',(-24.1413025515743,-16.1008000918638,
14.7530932242828)) ;
#54800 = CARTESIAN_POINT('Ctrl Pts',(-24.1474363277936,-16.0931892946346,
14.8209763136315)) ;
#54801 = CARTESIAN_POINT('Ctrl Pts',(-24.1556518745863,-16.0853002129683,
14.8880364584972)) ;
#54802 = CARTESIAN_POINT('Ctrl Pts',(-24.1639344141002,-16.0773468007026,
14.9556434375189)) ;
#54803 = CARTESIAN_POINT('Ctrl Pts',(-24.1743326201581,-16.0691106491237,
15.0224135316151)) ;
#54804 = CARTESIAN_POINT('Ctrl Pts',(-24.1866833139219,-16.0606518030576,
15.0880629082488)) ;
#54805 = CARTESIAN_POINT('Ctrl Pts',(-24.1967977432917,-16.053724548385,15.1418255547714)) ;
#54806 = CARTESIAN_POINT('Ctrl Pts',(-24.2082206267189,-16.0466480826284,
15.1948368796874)) ;
#54807 = CARTESIAN_POINT('Ctrl Pts',(-24.2208399697526,-16.0394576303854,
15.2469540989219)) ;
#54808 = CARTESIAN_POINT('Ctrl Pts',(-24.23627468645,-16.0306629892539,15.3106986624695)) ;
#54809 = CARTESIAN_POINT('Ctrl Pts',(-24.2538964166868,-16.021472015069,15.3747401594769)) ;
#54810 = CARTESIAN_POINT('Ctrl Pts',(-24.2737630817652,-16.0119118209667,
15.4387470329595)) ;
#54811 = CARTESIAN_POINT('Ctrl Pts',(-24.2934670332299,-16.0024299275618,
15.5022296720201)) ;
#54812 = CARTESIAN_POINT('Ctrl Pts',(-24.3153793437887,-15.9925848997553,
15.5656777628575)) ;
#54813 = CARTESIAN_POINT('Ctrl Pts',(-24.3395061544923,-15.9824119250024,
15.6287677350517)) ;
#54814 = CARTESIAN_POINT('Ctrl Pts',(-24.3593166603049,-15.9740589032147,
15.6805708629588)) ;
#54815 = CARTESIAN_POINT('Ctrl Pts',(-24.3806192654345,-15.9654849570552,
15.7321324161385)) ;
#54816 = CARTESIAN_POINT('Ctrl Pts',(-24.4033915883005,-15.9567135267634,
15.7832767754878)) ;
#54817 = CARTESIAN_POINT('Ctrl Pts',(-24.4319201697606,-15.9457249040799,
15.8473491158683)) ;
#54818 = CARTESIAN_POINT('Ctrl Pts',(-24.4627607439619,-15.9344245943031,
15.9107757288349)) ;
#54819 = CARTESIAN_POINT('Ctrl Pts',(-24.4958354560159,-15.9228603613588,
15.9732492358817)) ;
#54820 = CARTESIAN_POINT('Ctrl Pts',(-24.5071875390631,-15.918891222261,15.9946917336754)) ;
#54821 = CARTESIAN_POINT('Ctrl Pts',(-24.5188023846988,-15.9148910460673,
16.0160220870393)) ;
#54822 = CARTESIAN_POINT('Ctrl Pts',(-24.5306755198089,-15.9108619232992,
16.0372283458231)) ;
#54823 = CARTESIAN_POINT('',(-23.9779507369461,-15.910861895147,16.8524363944926)) ;
#54824 = CARTESIAN_POINT('Origin',(-2.92277791062251E-15,-15.9108618782028,
0.)) ;
#54825 = CARTESIAN_POINT('',(-21.6617807651637,-16.1877442736408,17.4680565820063)) ;
#54826 = CARTESIAN_POINT('Ctrl Pts',(-23.9779507384798,-15.9108619285364,
16.8524363584598)) ;
#54827 = CARTESIAN_POINT('Ctrl Pts',(-23.9077495898749,-15.9226009260419,
16.8431695039185)) ;
#54828 = CARTESIAN_POINT('Ctrl Pts',(-23.8373814663715,-15.9340937840903,
16.8363331931147)) ;
#54829 = CARTESIAN_POINT('Ctrl Pts',(-23.7671616573665,-15.9452906645258,
16.831903730605)) ;
#54830 = CARTESIAN_POINT('Ctrl Pts',(-23.7430604420255,-15.9491337172248,
16.8303834269855)) ;
#54831 = CARTESIAN_POINT('Ctrl Pts',(-23.7189766846033,-15.9529419533942,
16.8291462092394)) ;
#54832 = CARTESIAN_POINT('Ctrl Pts',(-23.6949230333843,-15.9567135267634,
16.8281897192057)) ;
#54833 = CARTESIAN_POINT('Ctrl Pts',(-23.6268850269974,-15.9673817754483,
16.825484197519)) ;
#54834 = CARTESIAN_POINT('Ctrl Pts',(-23.5590787032743,-15.9777576912911,
16.825028161963)) ;
#54835 = CARTESIAN_POINT('Ctrl Pts',(-23.491811591325,-15.9877997661733,16.826737552496)) ;
#54836 = CARTESIAN_POINT('Ctrl Pts',(-23.42399642205,-15.9979236586412,16.8284608702511)) ;
#54837 = CARTESIAN_POINT('Ctrl Pts',(-23.3567297702322,-16.0077081692747,
16.8323848898801)) ;
#54838 = CARTESIAN_POINT('Ctrl Pts',(-23.2903131026374,-16.0171189356809,
16.8383726499909)) ;
#54839 = CARTESIAN_POINT('Ctrl Pts',(-23.2359620767902,-16.0248200870139,
16.8432726384477)) ;
#54840 = CARTESIAN_POINT('Ctrl Pts',(-23.182180099954,-16.0322710948775,16.8495536282054)) ;
#54841 = CARTESIAN_POINT('Ctrl Pts',(-23.1291224332011,-16.0394576303853,
16.8571170015809)) ;
#54842 = CARTESIAN_POINT('Ctrl Pts',(-23.0642044765904,-16.048250614111,16.8663710599419)) ;
#54843 = CARTESIAN_POINT('Ctrl Pts',(-22.9987063980747,-16.0568730319551,
16.8777835360754)) ;
#54844 = CARTESIAN_POINT('Ctrl Pts',(-22.9329474911557,-16.0652608298868,
16.8914434186426)) ;
#54845 = CARTESIAN_POINT('Ctrl Pts',(-22.8677276159361,-16.0735798722813,
16.9049913299185)) ;
#54846 = CARTESIAN_POINT('Ctrl Pts',(-22.8022516466988,-16.0816680200513,
16.9207500442982)) ;
#54847 = CARTESIAN_POINT('Ctrl Pts',(-22.7368378236097,-16.0894673869316,
16.9387559320863)) ;
#54848 = CARTESIAN_POINT('Ctrl Pts',(-22.683086943236,-16.0958761674671,16.953551464205)) ;
#54849 = CARTESIAN_POINT('Ctrl Pts',(-22.6293782743638,-16.1020900207686,
16.9698633725608)) ;
#54850 = CARTESIAN_POINT('Ctrl Pts',(-22.5758883277042,-16.1080799337539,
16.9876856353241)) ;
#54851 = CARTESIAN_POINT('Ctrl Pts',(-22.5089157709591,-16.1155796568301,
17.0100001556925)) ;
#54852 = CARTESIAN_POINT('Ctrl Pts',(-22.4422764656216,-16.1227292229208,
17.0346868542773)) ;
#54853 = CARTESIAN_POINT('Ctrl Pts',(-22.3762837673814,-16.1294814162037,
17.0616964530681)) ;
#54854 = CARTESIAN_POINT('Ctrl Pts',(-22.3104215486986,-16.1362202591734,
17.0886526489736)) ;
#54855 = CARTESIAN_POINT('Ctrl Pts',(-22.2452038731938,-16.1425632136359,
17.1179224484975)) ;
#54856 = CARTESIAN_POINT('Ctrl Pts',(-22.1809299586464,-16.1484717649151,
17.1494071304985)) ;
#54857 = CARTESIAN_POINT('Ctrl Pts',(-22.132457485989,-16.1529277264407,17.1731514503858)) ;
#54858 = CARTESIAN_POINT('Ctrl Pts',(-22.0845215701936,-16.1571367885212,
17.1981544365714)) ;
#54859 = CARTESIAN_POINT('Ctrl Pts',(-22.0372433987965,-16.1610860188908,
17.2243558101924)) ;
#54860 = CARTESIAN_POINT('Ctrl Pts',(-21.9718396877092,-16.166549308068,17.2606022854633)) ;
#54861 = CARTESIAN_POINT('Ctrl Pts',(-21.9076517171375,-16.171518536629,17.299168756337)) ;
#54862 = CARTESIAN_POINT('Ctrl Pts',(-21.8449801241199,-16.1759680067789,
17.3398591970886)) ;
#54863 = CARTESIAN_POINT('Ctrl Pts',(-21.7823085311368,-16.1804174769263,
17.3805496378177)) ;
#54864 = CARTESIAN_POINT('Ctrl Pts',(-21.7211538087488,-16.1843471450139,
17.4233636486333)) ;
#54865 = CARTESIAN_POINT('Ctrl Pts',(-21.6617807650567,-16.1877442734701,
17.4680565820512)) ;
#54866 = CARTESIAN_POINT('',(-22.8021295298701,-15.9108618782028,18.4122143563869)) ;
#54867 = CARTESIAN_POINT('Ctrl Pts',(-22.8021295298702,-15.9108618782028,
18.4122143563868)) ;
#54868 = CARTESIAN_POINT('Ctrl Pts',(-22.2246443787864,-16.0510971574266,
17.9339256461324)) ;
#54869 = CARTESIAN_POINT('Ctrl Pts',(-21.6617807653427,-16.1877442737198,
17.4680565818894)) ;
#54870 = CARTESIAN_POINT('',(-21.8586355065995,-15.9108618782028,19.5229813909695)) ;
#54871 = CARTESIAN_POINT('Origin',(-2.92277791062251E-15,-15.9108618782028,
0.)) ;
#54872 = CARTESIAN_POINT('',(-20.7424276734563,-16.1877442736408,18.55040271481)) ;
#54873 = CARTESIAN_POINT('Ctrl Pts',(-20.7424276733699,-16.1877442737198,
18.5504027150055)) ;
#54874 = CARTESIAN_POINT('Ctrl Pts',(-21.2932208186878,-16.0510971580414,
19.0304822278201)) ;
#54875 = CARTESIAN_POINT('Ctrl Pts',(-21.8586355065993,-15.9108618782028,
19.5229813909696)) ;
#54876 = CARTESIAN_POINT('',(-20.5096319469963,-15.910861895147,20.935656936733)) ;
#54877 = CARTESIAN_POINT('Ctrl Pts',(-20.7424276734832,-16.18774427347,18.5504027146971)) ;
#54878 = CARTESIAN_POINT('Ctrl Pts',(-20.7079289909662,-16.1843471450139,
18.6162241209367)) ;
#54879 = CARTESIAN_POINT('Ctrl Pts',(-20.6755727226435,-16.1804174769264,
18.6834997591179)) ;
#54880 = CARTESIAN_POINT('Ctrl Pts',(-20.6455574519581,-16.1759680067789,
18.7519287300254)) ;
#54881 = CARTESIAN_POINT('Ctrl Pts',(-20.6155421812561,-16.171518536629,18.8203577009705)) ;
#54882 = CARTESIAN_POINT('Ctrl Pts',(-20.587868222951,-16.166549308068,18.8899394534164)) ;
#54883 = CARTESIAN_POINT('Ctrl Pts',(-20.5626803827667,-16.1610860188908,
18.9603455973273)) ;
#54884 = CARTESIAN_POINT('Ctrl Pts',(-20.5385463058567,-16.1558512929191,
19.0278062164059)) ;
#54885 = CARTESIAN_POINT('Ctrl Pts',(-20.5166787555948,-16.1501596984487,
19.0960670856629)) ;
#54886 = CARTESIAN_POINT('Ctrl Pts',(-20.4971645214231,-16.1440425621068,
19.1648253504181)) ;
#54887 = CARTESIAN_POINT('Ctrl Pts',(-20.4776099712092,-16.1379127878757,
19.2337256684603)) ;
#54888 = CARTESIAN_POINT('Ctrl Pts',(-20.4604185820138,-16.1313557844551,
19.3031249391449)) ;
#54889 = CARTESIAN_POINT('Ctrl Pts',(-20.4456270281159,-16.1244124680049,
19.3727086107004)) ;
#54890 = CARTESIAN_POINT('Ctrl Pts',(-20.4344813480391,-16.1191805644225,
19.4251410560729)) ;
#54891 = CARTESIAN_POINT('Ctrl Pts',(-20.4246972145375,-16.1137295207045,
19.4776779509581)) ;
#54892 = CARTESIAN_POINT('Ctrl Pts',(-20.4162710291437,-16.1080799337539,
19.5301836728207)) ;
#54893 = CARTESIAN_POINT('Ctrl Pts',(-20.4054133685855,-16.1008000918638,
19.597840539921)) ;
#54894 = CARTESIAN_POINT('Ctrl Pts',(-20.3968108829253,-16.0931892946347,
19.665455140938)) ;
#54895 = CARTESIAN_POINT('Ctrl Pts',(-20.390418405937,-16.0853002129684,19.732713556593)) ;
#54896 = CARTESIAN_POINT('Ctrl Pts',(-20.3839738022381,-16.0773468007026,
19.8005204231803)) ;
#54897 = CARTESIAN_POINT('Ctrl Pts',(-20.379775307496,-16.0691106491238,19.8679647765148)) ;
#54898 = CARTESIAN_POINT('Ctrl Pts',(-20.3777245735084,-16.0606518030577,
19.9347343412799)) ;
#54899 = CARTESIAN_POINT('Ctrl Pts',(-20.3760451533504,-16.0537245483851,
19.9894143503377)) ;
#54900 = CARTESIAN_POINT('Ctrl Pts',(-20.3758051082575,-16.0466480826284,
20.0436418822154)) ;
#54901 = CARTESIAN_POINT('Ctrl Pts',(-20.3769257565024,-16.0394576303854,
20.0972534155537)) ;
#54902 = CARTESIAN_POINT('Ctrl Pts',(-20.3782964212137,-16.0306629892539,
20.1628256744722)) ;
#54903 = CARTESIAN_POINT('Ctrl Pts',(-20.3817391363867,-16.021472015069,20.2291580679745)) ;
#54904 = CARTESIAN_POINT('Ctrl Pts',(-20.3873817441066,-16.0119118209667,
20.295939242062)) ;
#54905 = CARTESIAN_POINT('Ctrl Pts',(-20.3929781372712,-16.0024299275617,
20.3621734594199)) ;
#54906 = CARTESIAN_POINT('Ctrl Pts',(-20.4007386861682,-15.9925848997551,
20.4288486681995)) ;
#54907 = CARTESIAN_POINT('Ctrl Pts',(-20.4107389463496,-15.9824119250022,
20.4956501830215)) ;
#54908 = CARTESIAN_POINT('Ctrl Pts',(-20.4189501523347,-15.9740589032146,
20.5505008557405)) ;
#54909 = CARTESIAN_POINT('Ctrl Pts',(-20.4286705046094,-15.9654849570552,
20.6054363588621)) ;
#54910 = CARTESIAN_POINT('Ctrl Pts',(-20.4399158977778,-15.9567135267634,
20.6602803677819)) ;
#54911 = CARTESIAN_POINT('Ctrl Pts',(-20.454003837642,-15.9457249040784,20.7289875341744)) ;
#54912 = CARTESIAN_POINT('Ctrl Pts',(-20.4704885294489,-15.9344245943001,
20.7975610799983)) ;
#54913 = CARTESIAN_POINT('Ctrl Pts',(-20.4893600158069,-15.9228603613541,
20.8656840765868)) ;
#54914 = CARTESIAN_POINT('Ctrl Pts',(-20.4958371874622,-15.9188912239776,
20.8890656128477)) ;
#54915 = CARTESIAN_POINT('Ctrl Pts',(-20.5025950859566,-15.9148910495321,
20.9123941127885)) ;
#54916 = CARTESIAN_POINT('Ctrl Pts',(-20.5096319116864,-15.9108619285364,
20.935656944076)) ;
#54917 = CARTESIAN_POINT('',(-19.7945838954017,-15.910861895547,21.6129864201278)) ;
#54918 = CARTESIAN_POINT('Origin',(-2.92277791062251E-15,-15.9108618782028,
0.)) ;
#54919 = CARTESIAN_POINT('',(-17.400224555478,-16.1877442736409,21.7163056731368)) ;
#54920 = CARTESIAN_POINT('Ctrl Pts',(-19.7945839053568,-15.9108619297779,
21.6129863845241)) ;
#54921 = CARTESIAN_POINT('Ctrl Pts',(-19.7280161203445,-15.9226009272665,
21.588845012237)) ;
#54922 = CARTESIAN_POINT('Ctrl Pts',(-19.6607627691677,-15.934093785296,21.5670414642609)) ;
#54923 = CARTESIAN_POINT('Ctrl Pts',(-19.5931368637526,-15.945290665711,21.547620377037)) ;
#54924 = CARTESIAN_POINT('Ctrl Pts',(-19.5699259441484,-15.9491337180078,
21.5409545691427)) ;
#54925 = CARTESIAN_POINT('Ctrl Pts',(-19.5466712192221,-15.952941953782,21.5345689816102)) ;
#54926 = CARTESIAN_POINT('Ctrl Pts',(-19.5233855484791,-15.9567135267635,
21.5284640304184)) ;
#54927 = CARTESIAN_POINT('Ctrl Pts',(-19.4575198400606,-15.9673817754482,
21.5111956021413)) ;
#54928 = CARTESIAN_POINT('Ctrl Pts',(-19.3913968246702,-15.9777576912909,
21.4961738731834)) ;
#54929 = CARTESIAN_POINT('Ctrl Pts',(-19.3253349119823,-15.9877997661731,
21.4833828584483)) ;
#54930 = CARTESIAN_POINT('Ctrl Pts',(-19.2587347613034,-15.997923658641,21.4704876291999)) ;
#54931 = CARTESIAN_POINT('Ctrl Pts',(-19.1921972181978,-16.0077081692744,
21.4598595656779)) ;
#54932 = CARTESIAN_POINT('Ctrl Pts',(-19.1260461439565,-16.0171189356805,
21.4514297150146)) ;
#54933 = CARTESIAN_POINT('Ctrl Pts',(-19.0719124622137,-16.0248200870136,
21.4445312805117)) ;
#54934 = CARTESIAN_POINT('Ctrl Pts',(-19.0180376509747,-16.0322710948774,
21.4391038889833)) ;
#54935 = CARTESIAN_POINT('Ctrl Pts',(-18.9645945412809,-16.0394576303854,
21.4350846049139)) ;
#54936 = CARTESIAN_POINT('Ctrl Pts',(-18.8992049814215,-16.0482506141109,
21.4301668668228)) ;
#54937 = CARTESIAN_POINT('Ctrl Pts',(-18.8327848665661,-16.0568730319549,
21.4272323748349)) ;
#54938 = CARTESIAN_POINT('Ctrl Pts',(-18.7656268953802,-16.0652608298865,
21.4264366757703)) ;
#54939 = CARTESIAN_POINT('Ctrl Pts',(-18.6990194241494,-16.0735798722809,
21.4256474991228)) ;
#54940 = CARTESIAN_POINT('Ctrl Pts',(-18.6316865889201,-16.0816680200509,
21.4269623855873)) ;
#54941 = CARTESIAN_POINT('Ctrl Pts',(-18.5639313710398,-16.0894673869311,
21.4304852673795)) ;
#54942 = CARTESIAN_POINT('Ctrl Pts',(-18.5082565543254,-16.0958761674669,
21.4333800377636)) ;
#54943 = CARTESIAN_POINT('Ctrl Pts',(-18.4522969861638,-16.1020900207685,
21.4377648065762)) ;
#54944 = CARTESIAN_POINT('Ctrl Pts',(-18.3962263450592,-16.1080799337539,
21.44367163736)) ;
#54945 = CARTESIAN_POINT('Ctrl Pts',(-18.3260226072069,-16.1155796568301,
21.4510673366371)) ;
#54946 = CARTESIAN_POINT('Ctrl Pts',(-18.2556343813341,-16.1227292229208,
21.4608513931238)) ;
#54947 = CARTESIAN_POINT('Ctrl Pts',(-18.185378290364,-16.1294814162037,21.4730430431129)) ;
#54948 = CARTESIAN_POINT('Ctrl Pts',(-18.1152611084535,-16.1362202591734,
21.4852105879945)) ;
#54949 = CARTESIAN_POINT('Ctrl Pts',(-18.0452760442714,-16.1425632136359,
21.4997762034582)) ;
#54950 = CARTESIAN_POINT('Ctrl Pts',(-17.9757365421789,-16.1484717649151,
21.5167077993861)) ;
#54951 = CARTESIAN_POINT('Ctrl Pts',(-17.9232930020967,-16.1529277264407,
21.5294768414841)) ;
#54952 = CARTESIAN_POINT('Ctrl Pts',(-17.8711028984271,-16.1571367885211,
21.5435904668266)) ;
#54953 = CARTESIAN_POINT('Ctrl Pts',(-17.8192975435827,-16.1610860188907,
21.5590158575752)) ;
#54954 = CARTESIAN_POINT('Ctrl Pts',(-17.7476310141697,-16.166549308068,21.580355045833)) ;
#54955 = CARTESIAN_POINT('Ctrl Pts',(-17.6766530714589,-16.171518536629,21.6042213377595)) ;
#54956 = CARTESIAN_POINT('Ctrl Pts',(-17.6066994634978,-16.1759680067789,
21.6304879186787)) ;
#54957 = CARTESIAN_POINT('Ctrl Pts',(-17.5367458555753,-16.1804174769264,
21.6567544995834)) ;
#54958 = CARTESIAN_POINT('Ctrl Pts',(-17.46781714986,-16.184347145014,21.6854210850257)) ;
#54959 = CARTESIAN_POINT('Ctrl Pts',(-17.4002245553638,-16.1877442734701,
21.7163056731577)) ;
#54960 = CARTESIAN_POINT('',(-18.3109465873826,-15.9108618782028,22.883530839373)) ;
#54961 = CARTESIAN_POINT('Ctrl Pts',(-18.3109465873823,-15.9108618782028,
22.8835308393732)) ;
#54962 = CARTESIAN_POINT('Ctrl Pts',(-17.8497806514479,-16.05109715784,22.2922820144884)) ;
#54963 = CARTESIAN_POINT('Ctrl Pts',(-17.4002245556779,-16.1877442737199,
21.716305673061)) ;
#54964 = CARTESIAN_POINT('',(-17.1507288516715,-15.9108618782028,23.765505432432)) ;
#54965 = CARTESIAN_POINT('Origin',(-2.92277791062251E-15,-15.9108618782028,
0.)) ;
#54966 = CARTESIAN_POINT('',(-16.2696930035337,-16.1877442736409,22.5757134159908)) ;
#54967 = CARTESIAN_POINT('Ctrl Pts',(-16.2696930034074,-16.1877442737198,
22.5757134161632)) ;
#54968 = CARTESIAN_POINT('Ctrl Pts',(-16.7044060067849,-16.051097158066,23.1629731815623)) ;
#54969 = CARTESIAN_POINT('Ctrl Pts',(-17.1507288516718,-15.9108618782028,
23.7655054324318)) ;
#54970 = CARTESIAN_POINT('',(-15.5295807620181,-15.910861895547,24.8551575119669)) ;
#54971 = CARTESIAN_POINT('Ctrl Pts',(-16.2696930035843,-16.1877442734701,
22.5757134158863)) ;
#54972 = CARTESIAN_POINT('Ctrl Pts',(-16.2218512244183,-16.1843471450139,
22.6325797572584)) ;
#54973 = CARTESIAN_POINT('Ctrl Pts',(-16.1757891541129,-16.1804174769264,
22.69132688716)) ;
#54974 = CARTESIAN_POINT('Ctrl Pts',(-16.131765417777,-16.1759680067789,22.7517036308022)) ;
#54975 = CARTESIAN_POINT('Ctrl Pts',(-16.0877416814168,-16.171518536629,22.8120803744776)) ;
#54976 = CARTESIAN_POINT('Ctrl Pts',(-16.0457567049241,-16.166549308068,22.8740862612196)) ;
#54977 = CARTESIAN_POINT('Ctrl Pts',(-16.0060225026959,-16.1610860188908,
22.9374317075191)) ;
#54978 = CARTESIAN_POINT('Ctrl Pts',(-15.9679506281116,-16.155851292919,22.9981270216757)) ;
#54979 = CARTESIAN_POINT('Ctrl Pts',(-15.931920259909,-16.1501596984485,23.0600911128376)) ;
#54980 = CARTESIAN_POINT('Ctrl Pts',(-15.898081263245,-16.1440425621064,23.1230468640632)) ;
#54981 = CARTESIAN_POINT('Ctrl Pts',(-15.8641723558478,-16.1379127878752,
23.1861326806915)) ;
#54982 = CARTESIAN_POINT('Ctrl Pts',(-15.8324641000085,-16.1313557844547,
23.2502137944912)) ;
#54983 = CARTESIAN_POINT('Ctrl Pts',(-15.8030599319149,-16.1244124680043,
23.3149908916223)) ;
#54984 = CARTESIAN_POINT('Ctrl Pts',(-15.7809034057824,-16.1191805644221,
23.3638015038048)) ;
#54985 = CARTESIAN_POINT('Ctrl Pts',(-15.7600541404651,-16.1137295207043,
23.4130068157949)) ;
#54986 = CARTESIAN_POINT('Ctrl Pts',(-15.7405377764617,-16.108079933754,23.4624736022728)) ;
#54987 = CARTESIAN_POINT('Ctrl Pts',(-15.7153897354694,-16.1008000918637,
23.5262146133492)) ;
#54988 = CARTESIAN_POINT('Ctrl Pts',(-15.6924532305976,-16.0931892946344,
23.5903991424404)) ;
#54989 = CARTESIAN_POINT('Ctrl Pts',(-15.6717516349474,-16.0853002129679,
23.6547109001225)) ;
#54990 = CARTESIAN_POINT('Ctrl Pts',(-15.6508812305419,-16.0773468007021,
23.7195470805569)) ;
#54991 = CARTESIAN_POINT('Ctrl Pts',(-15.6322823519474,-16.069110649123,23.784512070128)) ;
#54992 = CARTESIAN_POINT('Ctrl Pts',(-15.6159260802505,-16.0606518030568,
23.8492797523866)) ;
#54993 = CARTESIAN_POINT('Ctrl Pts',(-15.6025313383852,-16.0537245483845,
23.902320347526)) ;
#54994 = CARTESIAN_POINT('Ctrl Pts',(-15.5906395890145,-16.0466480826281,
23.9552284672416)) ;
#54995 = CARTESIAN_POINT('Ctrl Pts',(-15.5802091422045,-16.0394576303854,
24.0078274989672)) ;
#54996 = CARTESIAN_POINT('Ctrl Pts',(-15.567451664171,-16.0306629892537,24.0721613673087)) ;
#54997 = CARTESIAN_POINT('Ctrl Pts',(-15.5565543867448,-16.0214720150687,
24.1376830283097)) ;
#54998 = CARTESIAN_POINT('Ctrl Pts',(-15.5477090950404,-16.0119118209662,
24.2041158895244)) ;
#54999 = CARTESIAN_POINT('Ctrl Pts',(-15.5389362487803,-16.0024299275611,
24.2700046467905)) ;
#55000 = CARTESIAN_POINT('Ctrl Pts',(-15.5321821613742,-15.9925848997544,
24.3367893148545)) ;
#55001 = CARTESIAN_POINT('Ctrl Pts',(-15.5275882699818,-15.9824119250013,
24.4041788077167)) ;
#55002 = CARTESIAN_POINT('Ctrl Pts',(-15.523816229274,-15.974058903214,24.4595122687521)) ;
#55003 = CARTESIAN_POINT('Ctrl Pts',(-15.5214998158251,-15.9654849570548,
24.5152529987445)) ;
#55004 = CARTESIAN_POINT('Ctrl Pts',(-15.52069245721,-15.9567135267634,24.571232212331)) ;
#55005 = CARTESIAN_POINT('Ctrl Pts',(-15.5196810190638,-15.9457249040781,
24.6413615339908)) ;
#55006 = CARTESIAN_POINT('Ctrl Pts',(-15.5210390226046,-15.9344245942994,
24.7118755898769)) ;
#55007 = CARTESIAN_POINT('Ctrl Pts',(-15.5248248735337,-15.922860361353,24.7824627203936)) ;
#55008 = CARTESIAN_POINT('Ctrl Pts',(-15.5261242732388,-15.9188912243845,
24.8066900072817)) ;
#55009 = CARTESIAN_POINT('Ctrl Pts',(-15.5277092377278,-15.9148910503535,
24.8309258457799)) ;
#55010 = CARTESIAN_POINT('Ctrl Pts',(-15.5295807250488,-15.9108619297779,
24.855157512034)) ;
#55011 = CARTESIAN_POINT('',(-14.6856444869839,-15.9108618855281,25.36293728564)) ;
#55012 = CARTESIAN_POINT('Origin',(-2.92277791062251E-15,-15.9108618782028,
0.)) ;
#55013 = CARTESIAN_POINT('',(-12.3250531845394,-16.1877442736409,24.9491244469309)) ;
#55014 = CARTESIAN_POINT('Ctrl Pts',(-14.6856444555744,-15.9108619063809,
25.3629372648498)) ;
#55015 = CARTESIAN_POINT('Ctrl Pts',(-14.625822671402,-15.9226009041889,25.3250501955733)) ;
#55016 = CARTESIAN_POINT('Ctrl Pts',(-14.5648287859113,-15.9340937625731,
25.2892989170221)) ;
#55017 = CARTESIAN_POINT('Ctrl Pts',(-14.5029588974541,-15.9452906433744,
25.2557943104058)) ;
#55018 = CARTESIAN_POINT('Ctrl Pts',(-14.4817235471669,-15.9491337032516,
25.2442946604876)) ;
#55019 = CARTESIAN_POINT('Ctrl Pts',(-14.460385176184,-15.9529419464749,25.233059263703)) ;
#55020 = CARTESIAN_POINT('Ctrl Pts',(-14.4389562540117,-15.9567135267634,
25.2220912907379)) ;
#55021 = CARTESIAN_POINT('Ctrl Pts',(-14.3783426508824,-15.9673817754482,
25.1910674083842)) ;
#55022 = CARTESIAN_POINT('Ctrl Pts',(-14.3169947825335,-15.9777576912909,
25.1621823853752)) ;
#55023 = CARTESIAN_POINT('Ctrl Pts',(-14.2552270507214,-15.987799766173,25.1354890590048)) ;
#55024 = CARTESIAN_POINT('Ctrl Pts',(-14.1929560676633,-15.9979236586409,
25.1085782493407)) ;
#55025 = CARTESIAN_POINT('Ctrl Pts',(-14.130258854834,-16.0077081692743,25.0838950591058)) ;
#55026 = CARTESIAN_POINT('Ctrl Pts',(-14.0674665246557,-16.0171189356804,
25.0614417681163)) ;
#55027 = CARTESIAN_POINT('Ctrl Pts',(-14.016081417811,-16.0248200870136,25.043067473784)) ;
#55028 = CARTESIAN_POINT('Ctrl Pts',(-13.9646328984659,-16.0322710948774,
25.0261854797651)) ;
#55029 = CARTESIAN_POINT('Ctrl Pts',(-13.9133032862434,-16.0394576303854,
25.0107714755065)) ;
#55030 = CARTESIAN_POINT('Ctrl Pts',(-13.8504996662784,-16.0482506141108,
24.991911888931)) ;
#55031 = CARTESIAN_POINT('Ctrl Pts',(-13.7862632458327,-16.0568730319548,
24.9747676424058)) ;
#55032 = CARTESIAN_POINT('Ctrl Pts',(-13.7208464424711,-16.0652608298864,
24.9595535677136)) ;
#55033 = CARTESIAN_POINT('Ctrl Pts',(-13.6559658665551,-16.0735798722808,
24.9444642041659)) ;
#55034 = CARTESIAN_POINT('Ctrl Pts',(-13.5899245738745,-16.0816680200507,
24.9312737800857)) ;
#55035 = CARTESIAN_POINT('Ctrl Pts',(-13.5229961198868,-16.0894673869308,
24.9201489298451)) ;
#55036 = CARTESIAN_POINT('Ctrl Pts',(-13.4680006593836,-16.0958761674666,
24.9110075822483)) ;
#55037 = CARTESIAN_POINT('Ctrl Pts',(-13.4124067991456,-16.1020900207684,
24.9032601846009)) ;
#55038 = CARTESIAN_POINT('Ctrl Pts',(-13.3563772644563,-16.1080799337539,
24.8969753865622)) ;
#55039 = CARTESIAN_POINT('Ctrl Pts',(-13.286224994253,-16.1155796568301,24.8891064500695)) ;
#55040 = CARTESIAN_POINT('Ctrl Pts',(-13.2153791230557,-16.1227292229208,
24.883530372851)) ;
#55041 = CARTESIAN_POINT('Ctrl Pts',(-13.1441447360857,-16.1294814162036,
24.8803340060351)) ;
#55042 = CARTESIAN_POINT('Ctrl Pts',(-13.0730511924442,-16.1362202591733,
24.8771439590173)) ;
#55043 = CARTESIAN_POINT('Ctrl Pts',(-13.0015711634035,-16.1425632136358,
24.8763243184304)) ;
#55044 = CARTESIAN_POINT('Ctrl Pts',(-12.9300176635963,-16.1484717649149,
24.8779111256775)) ;
#55045 = CARTESIAN_POINT('Ctrl Pts',(-12.8760552577365,-16.1529277264406,
24.8791078237695)) ;
#55046 = CARTESIAN_POINT('Ctrl Pts',(-12.8220513174348,-16.1571367885211,
24.8816721508341)) ;
#55047 = CARTESIAN_POINT('Ctrl Pts',(-12.7681411399577,-16.1610860188908,
24.8856002845828)) ;
#55048 = CARTESIAN_POINT('Ctrl Pts',(-12.6935628394831,-16.166549308068,24.8910343891013)) ;
#55049 = CARTESIAN_POINT('Ctrl Pts',(-12.6191137743479,-16.171518536629,24.8990845407954)) ;
#55050 = CARTESIAN_POINT('Ctrl Pts',(-12.5451491044039,-16.1759680067789,
24.9096990657516)) ;
#55051 = CARTESIAN_POINT('Ctrl Pts',(-12.4711844345007,-16.1804174769264,
24.920313590702)) ;
#55052 = CARTESIAN_POINT('Ctrl Pts',(-12.3977047751287,-16.184347145014,24.9334923330962)) ;
#55053 = CARTESIAN_POINT('Ctrl Pts',(-12.3250531844235,-16.1877442734701,
24.9491244469266)) ;
#55054 = CARTESIAN_POINT('',(-12.9635641336241,-15.9108618782028,26.2848388535279)) ;
#55055 = CARTESIAN_POINT('Ctrl Pts',(-12.9635641336243,-15.9108618782028,
26.2848388535278)) ;
#55056 = CARTESIAN_POINT('Ctrl Pts',(-12.6402810210044,-16.0510971579062,
25.6082760530286)) ;
#55057 = CARTESIAN_POINT('Ctrl Pts',(-12.3250531847509,-16.1877442737199,
24.9491244468999)) ;
#55058 = CARTESIAN_POINT('',(-11.6408731773057,-15.9108618782028,26.8967808533363)) ;
#55059 = CARTESIAN_POINT('Origin',(-2.92277791062251E-15,-15.9108618782028,
0.)) ;
#55060 = CARTESIAN_POINT('',(-11.0362055712307,-16.1877442736409,25.545408848944)) ;
#55061 = CARTESIAN_POINT('Ctrl Pts',(-11.0362055710702,-16.1877442737199,
25.5454088490852)) ;
#55062 = CARTESIAN_POINT('Ctrl Pts',(-11.3345117375303,-16.0510971572356,
26.2123892572703)) ;
#55063 = CARTESIAN_POINT('Ctrl Pts',(-11.6408731773055,-15.9108618782028,
26.8967808533364)) ;
#55064 = CARTESIAN_POINT('',(-9.82338358164157,-15.9108618855281,27.6124587235785)) ;
#55065 = CARTESIAN_POINT('Ctrl Pts',(-11.0362055713025,-16.1877442734701,
25.5454088488529)) ;
#55066 = CARTESIAN_POINT('Ctrl Pts',(-10.9772577239093,-16.184347145014,25.5906611184371)) ;
#55067 = CARTESIAN_POINT('Ctrl Pts',(-10.9196436628343,-16.1804174769264,
25.6381327895575)) ;
#55068 = CARTESIAN_POINT('Ctrl Pts',(-10.8636699618301,-16.1759680067789,
25.6876341565055)) ;
#55069 = CARTESIAN_POINT('Ctrl Pts',(-10.8076962607951,-16.171518536629,25.7371355234807)) ;
#55070 = CARTESIAN_POINT('Ctrl Pts',(-10.7533634369526,-16.166549308068,25.7886662181691)) ;
#55071 = CARTESIAN_POINT('Ctrl Pts',(-10.7009407998154,-16.1610860188908,
25.8419890041916)) ;
#55072 = CARTESIAN_POINT('Ctrl Pts',(-10.6507113260991,-16.155851292919,25.893080967993)) ;
#55073 = CARTESIAN_POINT('Ctrl Pts',(-10.6022028799284,-16.1501596984485,
25.9458509090239)) ;
#55074 = CARTESIAN_POINT('Ctrl Pts',(-10.5556213946471,-16.1440425621065,
26.0000604057616)) ;
#55075 = CARTESIAN_POINT('Ctrl Pts',(-10.5089436728898,-16.1379127878753,
26.0543818983042)) ;
#55076 = CARTESIAN_POINT('Ctrl Pts',(-10.4642011932089,-16.1313557844548,
26.1101484935574)) ;
#55077 = CARTESIAN_POINT('Ctrl Pts',(-10.4215593171393,-16.1244124680044,
26.1670901111956)) ;
#55078 = CARTESIAN_POINT('Ctrl Pts',(-10.3894279594871,-16.1191805644222,
26.2099965602139)) ;
#55079 = CARTESIAN_POINT('Ctrl Pts',(-10.3584884508272,-16.1137295207043,
26.2535695036106)) ;
#55080 = CARTESIAN_POINT('Ctrl Pts',(-10.3287944717036,-16.1080799337539,
26.2976843427492)) ;
#55081 = CARTESIAN_POINT('Ctrl Pts',(-10.2905319447247,-16.1008000918638,
26.3545290389645)) ;
#55082 = CARTESIAN_POINT('Ctrl Pts',(-10.254333906118,-16.0931892946347,26.4122822988833)) ;
#55083 = CARTESIAN_POINT('Ctrl Pts',(-10.2202911754108,-16.0853002129684,
26.4706402522785)) ;
#55084 = CARTESIAN_POINT('Ctrl Pts',(-10.1859708472133,-16.0773468007026,
26.529474078821)) ;
#55085 = CARTESIAN_POINT('Ctrl Pts',(-10.1538412476587,-16.0691106491238,
26.5889220139178)) ;
#55086 = CARTESIAN_POINT('Ctrl Pts',(-10.1239442393385,-16.0606518030577,
26.6486593488293)) ;
#55087 = CARTESIAN_POINT('Ctrl Pts',(-10.0994604990071,-16.0537245483851,
26.6975804107763)) ;
#55088 = CARTESIAN_POINT('Ctrl Pts',(-10.0764730903414,-16.0466480826284,
26.7466951934594)) ;
#55089 = CARTESIAN_POINT('Ctrl Pts',(-10.0549792645758,-16.0394576303854,
26.7958222513128)) ;
#55090 = CARTESIAN_POINT('Ctrl Pts',(-10.0286901692914,-16.0306629892537,
26.8559095488947)) ;
#55091 = CARTESIAN_POINT('Ctrl Pts',(-10.003962443847,-16.0214720150687,26.9175567573472)) ;
#55092 = CARTESIAN_POINT('Ctrl Pts',(-9.98104284872743,-16.0119118209662,
26.9805349789327)) ;
#55093 = CARTESIAN_POINT('Ctrl Pts',(-9.95831097158325,-16.0024299275611,
27.0429973910465)) ;
#55094 = CARTESIAN_POINT('Ctrl Pts',(-9.93735806149429,-15.9925848997544,
27.1067687415412)) ;
#55095 = CARTESIAN_POINT('Ctrl Pts',(-9.91838482378365,-15.9824119250013,
27.1715951546544)) ;
#55096 = CARTESIAN_POINT('Ctrl Pts',(-9.9028059128142,-15.974058903214,27.2248240728686)) ;
#55097 = CARTESIAN_POINT('Ctrl Pts',(-9.88856104656038,-15.9654849570548,
27.2787636551505)) ;
#55098 = CARTESIAN_POINT('Ctrl Pts',(-9.87573868735372,-15.9567135267634,
27.3332605475946)) ;
#55099 = CARTESIAN_POINT('Ctrl Pts',(-9.85967516493002,-15.9457249040846,
27.4015328553414)) ;
#55100 = CARTESIAN_POINT('Ctrl Pts',(-9.84584298147462,-15.9344245943129,
27.4706902623636)) ;
#55101 = CARTESIAN_POINT('Ctrl Pts',(-9.83436617479649,-15.9228603613737,
27.5404409509933)) ;
#55102 = CARTESIAN_POINT('Ctrl Pts',(-9.83042703709848,-15.9188912167155,
27.5643811962853)) ;
#55103 = CARTESIAN_POINT('Ctrl Pts',(-9.82676495056885,-15.9148910348745,
27.588391181513)) ;
#55104 = CARTESIAN_POINT('Ctrl Pts',(-9.82338358613012,-15.9108619063809,
27.61245868618)) ;
#55105 = CARTESIAN_POINT('',(-8.89001990812047,-15.9108619763187,27.92694497988)) ;
#55106 = CARTESIAN_POINT('Origin',(-2.92277791062251E-15,-15.9108618782028,
0.)) ;
#55107 = CARTESIAN_POINT('',(-6.67357602500529,-16.1877442736409,27.0153498905465)) ;
#55108 = CARTESIAN_POINT('Ctrl Pts',(-8.89002000637734,-15.9108620123611,
27.9269448892862)) ;
#55109 = CARTESIAN_POINT('Ctrl Pts',(-8.83974141393214,-15.922601008379,27.8770836956966)) ;
#55110 = CARTESIAN_POINT('Ctrl Pts',(-8.78785899221147,-15.9340938648278,
27.8290563925788)) ;
#55111 = CARTESIAN_POINT('Ctrl Pts',(-8.73463808083946,-15.9452907435693,
27.7830349210544)) ;
#55112 = CARTESIAN_POINT('Ctrl Pts',(-8.71637144205948,-15.9491337694432,
27.7672392953354)) ;
#55113 = CARTESIAN_POINT('Ctrl Pts',(-8.69794738737287,-15.952941979252,27.7516795942054)) ;
#55114 = CARTESIAN_POINT('Ctrl Pts',(-8.67937741285404,-15.9567135267634,
27.7363615946437)) ;
#55115 = CARTESIAN_POINT('Ctrl Pts',(-8.62685013972879,-15.9673817754482,
27.6930329004715)) ;
#55116 = CARTESIAN_POINT('Ctrl Pts',(-8.5731459765618,-15.977757691291,27.6516352149836)) ;
#55117 = CARTESIAN_POINT('Ctrl Pts',(-8.51856061611486,-15.9877997661731,
27.6122877272514)) ;
#55118 = CARTESIAN_POINT('Ctrl Pts',(-8.46353052263586,-15.997923658641,27.5726196567222)) ;
#55119 = CARTESIAN_POINT('Ctrl Pts',(-8.4076052920716,-16.0077081692744,27.5350354983163)) ;
#55120 = CARTESIAN_POINT('Ctrl Pts',(-8.35110780552667,-16.0171189356805,
27.4996086579324)) ;
#55121 = CARTESIAN_POINT('Ctrl Pts',(-8.30487398406619,-16.0248200870136,
27.4706176653522)) ;
#55122 = CARTESIAN_POINT('Ctrl Pts',(-8.25825743219905,-16.0322710948774,
27.4430704521203)) ;
#55123 = CARTESIAN_POINT('Ctrl Pts',(-8.21144143306706,-16.0394576303853,
27.4169824693803)) ;
#55124 = CARTESIAN_POINT('Ctrl Pts',(-8.15416038046395,-16.0482506141109,
27.3850628876275)) ;
#55125 = CARTESIAN_POINT('Ctrl Pts',(-8.09511127805334,-16.056873031955,27.3545105324776)) ;
#55126 = CARTESIAN_POINT('Ctrl Pts',(-8.03449445953493,-16.0652608298866,
27.3255894753811)) ;
#55127 = CARTESIAN_POINT('Ctrl Pts',(-7.97437452255286,-16.0735798722811,
27.2969054868018)) ;
#55128 = CARTESIAN_POINT('Ctrl Pts',(-7.91271278986576,-16.0816680200511,
27.2698265217467)) ;
#55129 = CARTESIAN_POINT('Ctrl Pts',(-7.84974059989247,-16.0894673869313,
27.244574125106)) ;
#55130 = CARTESIAN_POINT('Ctrl Pts',(-7.79799602221246,-16.095876167467,27.2238240987827)) ;
#55131 = CARTESIAN_POINT('Ctrl Pts',(-7.74536737701679,-16.1020900207685,
27.204306794379)) ;
#55132 = CARTESIAN_POINT('Ctrl Pts',(-7.69199882751462,-16.1080799337539,
27.1861242376894)) ;
#55133 = CARTESIAN_POINT('Ctrl Pts',(-7.62517826714627,-16.1155796568301,
27.1633586081517)) ;
#55134 = CARTESIAN_POINT('Ctrl Pts',(-7.55718742482217,-16.1227292229207,
27.1426831284015)) ;
#55135 = CARTESIAN_POINT('Ctrl Pts',(-7.48830558261541,-16.1294814162036,
27.1242482033404)) ;
#55136 = CARTESIAN_POINT('Ctrl Pts',(-7.41955993232838,-16.1362202591733,
27.1058497274763)) ;
#55137 = CARTESIAN_POINT('Ctrl Pts',(-7.34992726514201,-16.1425632136358,
27.0896831563216)) ;
#55138 = CARTESIAN_POINT('Ctrl Pts',(-7.27970552974461,-16.148471764915,27.0758509775448)) ;
#55139 = CARTESIAN_POINT('Ctrl Pts',(-7.22674748023081,-16.1529277264407,
27.0654193753579)) ;
#55140 = CARTESIAN_POINT('Ctrl Pts',(-7.17345486752508,-16.1571367885211,
27.0563144990611)) ;
#55141 = CARTESIAN_POINT('Ctrl Pts',(-7.11996064739795,-16.1610860188908,
27.0485617006416)) ;
#55142 = CARTESIAN_POINT('Ctrl Pts',(-7.04595777430401,-16.166549308068,27.037836628733)) ;
#55143 = CARTESIAN_POINT('Ctrl Pts',(-6.97151874228637,-16.171518536629,27.0296942240487)) ;
#55144 = CARTESIAN_POINT('Ctrl Pts',(-6.89700151612033,-16.1759680067789,
27.0241603696521)) ;
#55145 = CARTESIAN_POINT('Ctrl Pts',(-6.82248428999535,-16.1804174769264,
27.0186265152585)) ;
#55146 = CARTESIAN_POINT('Ctrl Pts',(-6.74788950417224,-16.184347145014,27.0157011912573)) ;
#55147 = CARTESIAN_POINT('Ctrl Pts',(-6.6735760249974,-16.1877442734653,27.0153498905179)) ;
#55148 = CARTESIAN_POINT('',(-7.01001982894532,-15.9108618782028,28.4570970163913)) ;
#55149 = CARTESIAN_POINT('Ctrl Pts',(-7.01001982894662,-15.9108618782028,
28.457097016391)) ;
#55150 = CARTESIAN_POINT('Ctrl Pts',(-6.83973590004788,-16.0510971569625,
27.7268555700758)) ;
#55151 = CARTESIAN_POINT('Ctrl Pts',(-6.67357602521852,-16.1877442737199,
27.0153498905617)) ;
#55152 = CARTESIAN_POINT('',(-5.58670321106903,-15.9108618782028,28.7703926951639)) ;
#55153 = CARTESIAN_POINT('Origin',(-2.92277791062251E-15,-15.9108618782028,
0.)) ;
#55154 = CARTESIAN_POINT('',(-5.28667743227751,-16.1877442736409,27.3206293558041)) ;
#55155 = CARTESIAN_POINT('Ctrl Pts',(-5.28667743209039,-16.1877442737198,
27.3206293559074)) ;
#55156 = CARTESIAN_POINT('Ctrl Pts',(-5.43462829436583,-16.0510971570733,
28.0361431415679)) ;
#55157 = CARTESIAN_POINT('Ctrl Pts',(-5.58670321106773,-15.9108618782028,
28.7703926951642)) ;
#55158 = CARTESIAN_POINT('',(-3.65785625118289,-15.9108619763187,29.0786312869383)) ;
#55159 = CARTESIAN_POINT('Ctrl Pts',(-5.28667743236728,-16.1877442734701,
27.3206293557305)) ;
#55160 = CARTESIAN_POINT('Ctrl Pts',(-5.21937985257516,-16.184347145014,27.3521516076954)) ;
#55161 = CARTESIAN_POINT('Ctrl Pts',(-5.15290777019315,-16.1804174769264,
27.3861280974538)) ;
#55162 = CARTESIAN_POINT('Ctrl Pts',(-5.08760137256953,-16.1759680067789,
27.4224394588058)) ;
#55163 = CARTESIAN_POINT('Ctrl Pts',(-5.02229497490993,-16.171518536629,27.4587508201778)) ;
#55164 = CARTESIAN_POINT('Ctrl Pts',(-4.95815484617409,-16.166549308068,27.4973968048012)) ;
#55165 = CARTESIAN_POINT('Ctrl Pts',(-4.89549499837687,-16.1610860188908,
27.5382036163359)) ;
#55166 = CARTESIAN_POINT('Ctrl Pts',(-4.83545659989313,-16.155851292919,27.5773032263399)) ;
#55167 = CARTESIAN_POINT('Ctrl Pts',(-4.77673827678375,-16.1501596984485,
27.6184115534471)) ;
#55168 = CARTESIAN_POINT('Ctrl Pts',(-4.7195924013649,-16.1440425621064,27.6613400198796)) ;
#55169 = CARTESIAN_POINT('Ctrl Pts',(-4.66232846363785,-16.1379127878752,
27.7043571757196)) ;
#55170 = CARTESIAN_POINT('Ctrl Pts',(-4.60664386873717,-16.1313557844547,
27.7492016684129)) ;
#55171 = CARTESIAN_POINT('Ctrl Pts',(-4.55275817142329,-16.1244124680042,
27.7956452798039)) ;
#55172 = CARTESIAN_POINT('Ctrl Pts',(-4.5121544088245,-16.119180564422,27.8306413077882)) ;
#55173 = CARTESIAN_POINT('Ctrl Pts',(-4.47257135386096,-16.1137295207043,
27.8665444601852)) ;
#55174 = CARTESIAN_POINT('Ctrl Pts',(-4.43408821707906,-16.108079933754,27.9032445911354)) ;
#55175 = CARTESIAN_POINT('Ctrl Pts',(-4.38450031734832,-16.1008000918637,
27.9505349776748)) ;
#55176 = CARTESIAN_POINT('Ctrl Pts',(-4.33673332505971,-16.0931892946345,
27.9991564901773)) ;
#55177 = CARTESIAN_POINT('Ctrl Pts',(-4.29094125954683,-16.085300212968,28.0488318862468)) ;
#55178 = CARTESIAN_POINT('Ctrl Pts',(-4.24477578795872,-16.0773468007022,
28.0989123545592)) ;
#55179 = CARTESIAN_POINT('Ctrl Pts',(-4.20061781180921,-16.0691106491232,
28.1500635158098)) ;
#55180 = CARTESIAN_POINT('Ctrl Pts',(-4.15857801774614,-16.0606518030571,
28.2019772519887)) ;
#55181 = CARTESIAN_POINT('Ctrl Pts',(-4.12415011143668,-16.0537245483847,
28.244491286255)) ;
#55182 = CARTESIAN_POINT('Ctrl Pts',(-4.09114190915792,-16.0466480826282,
28.2875161792511)) ;
#55183 = CARTESIAN_POINT('Ctrl Pts',(-4.05958973184235,-16.0394576303854,
28.3308741366043)) ;
#55184 = CARTESIAN_POINT('Ctrl Pts',(-4.02099826818466,-16.0306629892538,
28.3839052481734)) ;
#55185 = CARTESIAN_POINT('Ctrl Pts',(-3.98359633568106,-16.0214720150688,
28.4387954491257)) ;
#55186 = CARTESIAN_POINT('Ctrl Pts',(-3.94767413194106,-16.0119118209664,
28.4953742394354)) ;
#55187 = CARTESIAN_POINT('Ctrl Pts',(-3.9120461412236,-16.0024299275614,28.5514896334282)) ;
#55188 = CARTESIAN_POINT('Ctrl Pts',(-3.87787414324033,-15.9925848997548,
28.6092657888807)) ;
#55189 = CARTESIAN_POINT('Ctrl Pts',(-3.84540872671965,-15.9824119250018,
28.6684979112166)) ;
#55190 = CARTESIAN_POINT('Ctrl Pts',(-3.81875139805034,-15.9740589032143,
28.7171333615545)) ;
#55191 = CARTESIAN_POINT('Ctrl Pts',(-3.79324415310512,-15.965484957055,28.766749641209)) ;
#55192 = CARTESIAN_POINT('Ctrl Pts',(-3.76900635257193,-15.9567135267634,
28.8172159983899)) ;
#55193 = CARTESIAN_POINT('Ctrl Pts',(-3.73864185824403,-15.9457249040552,
28.8804389552036)) ;
#55194 = CARTESIAN_POINT('Ctrl Pts',(-3.71026626524916,-15.9344245942524,
28.9450059900909)) ;
#55195 = CARTESIAN_POINT('Ctrl Pts',(-3.68406344363511,-15.9228603612808,
29.0106587723793)) ;
#55196 = CARTESIAN_POINT('Ctrl Pts',(-3.67507003447375,-15.918891251378,29.0331923125605)) ;
#55197 = CARTESIAN_POINT('Ctrl Pts',(-3.66633220267684,-15.914891104836,29.0558535177718)) ;
#55198 = CARTESIAN_POINT('Ctrl Pts',(-3.65785616022794,-15.9108620121299,
29.0786312426591)) ;
#55199 = CARTESIAN_POINT('',(-2.67870907039602,-15.9108618818335,29.1851206195401)) ;
#55200 = CARTESIAN_POINT('Origin',(-2.92277791062251E-15,-15.9108618782028,
0.)) ;
#55201 = CARTESIAN_POINT('',(-0.710049867689416,-16.1877442736409,27.8183675986852)) ;
#55202 = CARTESIAN_POINT('Ctrl Pts',(-2.67870905771656,-15.9108618853164,
29.1851205952931)) ;
#55203 = CARTESIAN_POINT('Ctrl Pts',(-2.6403246466816,-15.9226008834121,29.1256167055889)) ;
#55204 = CARTESIAN_POINT('Ctrl Pts',(-2.59997966993281,-15.9340937421158,
29.0675590543327)) ;
#55205 = CARTESIAN_POINT('Ctrl Pts',(-2.55789630122123,-15.945290623265,29.0111726030762)) ;
#55206 = CARTESIAN_POINT('Ctrl Pts',(-2.54345217246438,-15.9491336899668,
28.9918192768804)) ;
#55207 = CARTESIAN_POINT('Ctrl Pts',(-2.52880358691511,-15.9529419398965,
28.9726625237371)) ;
#55208 = CARTESIAN_POINT('Ctrl Pts',(-2.51396053030637,-15.9567135267635,
28.9537104571357)) ;
#55209 = CARTESIAN_POINT('Ctrl Pts',(-2.47197570409715,-15.9673817754481,
28.9001029527286)) ;
#55210 = CARTESIAN_POINT('Ctrl Pts',(-2.42842639309452,-15.9777576912908,
28.8481283145256)) ;
#55211 = CARTESIAN_POINT('Ctrl Pts',(-2.38357575480059,-15.9877997661729,
28.7979665102268)) ;
#55212 = CARTESIAN_POINT('Ctrl Pts',(-2.33835969691063,-15.9979236586407,
28.7473960137229)) ;
#55213 = CARTESIAN_POINT('Ctrl Pts',(-2.29182145023647,-16.0077081692741,
28.6986682806216)) ;
#55214 = CARTESIAN_POINT('Ctrl Pts',(-2.24426056700373,-16.0171189356801,
28.6519244105256)) ;
#55215 = CARTESIAN_POINT('Ctrl Pts',(-2.20533987303285,-16.0248200870134,
28.6136723062887)) ;
#55216 = CARTESIAN_POINT('Ctrl Pts',(-2.16573502679743,-16.0322710948773,
28.5767479509172)) ;
#55217 = CARTESIAN_POINT('Ctrl Pts',(-2.12562170484212,-16.0394576303854,
28.5412058347734)) ;
#55218 = CARTESIAN_POINT('Ctrl Pts',(-2.07654161795819,-16.0482506141109,
28.4977187820102)) ;
#55219 = CARTESIAN_POINT('Ctrl Pts',(-2.02544090398406,-16.0568730319549,
28.4551869124065)) ;
#55220 = CARTESIAN_POINT('Ctrl Pts',(-1.9724584453729,-16.0652608298865,28.4139111893922)) ;
#55221 = CARTESIAN_POINT('Ctrl Pts',(-1.9199102887603,-16.0735798722809,28.3729738072076)) ;
#55222 = CARTESIAN_POINT('Ctrl Pts',(-1.86551135015594,-16.0816680200509,
28.3332724834876)) ;
#55223 = CARTESIAN_POINT('Ctrl Pts',(-1.80943993381238,-16.0894673869311,
28.2950733144478)) ;
#55224 = CARTESIAN_POINT('Ctrl Pts',(-1.76336575789626,-16.0958761674669,
28.2636848575662)) ;
#55225 = CARTESIAN_POINT('Ctrl Pts',(-1.71616318469793,-16.1020900207685,
28.2333102538678)) ;
#55226 = CARTESIAN_POINT('Ctrl Pts',(-1.66795107444097,-16.108079933754,28.2040801346692)) ;
#55227 = CARTESIAN_POINT('Ctrl Pts',(-1.60758667904453,-16.1155796568301,
28.1674823076214)) ;
#55228 = CARTESIAN_POINT('Ctrl Pts',(-1.54563004181418,-16.1227292229208,
28.1326741877935)) ;
#55229 = CARTESIAN_POINT('Ctrl Pts',(-1.48232158275546,-16.1294814162036,
28.0998627010941)) ;
#55230 = CARTESIAN_POINT('Ctrl Pts',(-1.41913829602524,-16.1362202591733,
28.0671160886667)) ;
#55231 = CARTESIAN_POINT('Ctrl Pts',(-1.35460893682001,-16.1425632136358,
28.0363585178435)) ;
#55232 = CARTESIAN_POINT('Ctrl Pts',(-1.28900245613401,-16.148471764915,28.0077541303492)) ;
#55233 = CARTESIAN_POINT('Ctrl Pts',(-1.23952502250277,-16.1529277264407,
27.9861819980077)) ;
#55234 = CARTESIAN_POINT('Ctrl Pts',(-1.18943564073249,-16.1571367885211,
27.9658336522457)) ;
#55235 = CARTESIAN_POINT('Ctrl Pts',(-1.13885870823377,-16.1610860188908,
27.9467624338955)) ;
#55236 = CARTESIAN_POINT('Ctrl Pts',(-1.06889155461827,-16.166549308068,27.9203796780022)) ;
#55237 = CARTESIAN_POINT('Ctrl Pts',(-0.997943242122202,-16.171518536629,
27.896425446733)) ;
#55238 = CARTESIAN_POINT('Ctrl Pts',(-0.926357802409802,-16.1759680067789,
27.8750019698647)) ;
#55239 = CARTESIAN_POINT('Ctrl Pts',(-0.854772362736824,-16.1804174769264,
27.8535784930083)) ;
#55240 = CARTESIAN_POINT('Ctrl Pts',(-0.782550419741656,-16.1843471450139,
27.8346858875108)) ;
#55241 = CARTESIAN_POINT('Ctrl Pts',(-0.71004986758597,-16.1877442734701,
27.8183675986327)) ;
#55242 = CARTESIAN_POINT('',(-0.72869478814225,-15.9108618782028,29.2987329505603)) ;
#55243 = CARTESIAN_POINT('Ctrl Pts',(-0.72869478814245,-15.9108618782028,
29.2987329505603)) ;
#55244 = CARTESIAN_POINT('Ctrl Pts',(-0.719372328009428,-16.0510971575387,
28.5489581292205)) ;
#55245 = CARTESIAN_POINT('Ctrl Pts',(-0.710049867894285,-16.1877442737198,
27.818367598746)) ;
#55246 = CARTESIAN_POINT('',(0.728694788142244,-15.9108618782028,29.2987329505603)) ;
#55247 = CARTESIAN_POINT('Origin',(-2.92277791062251E-15,-15.9108618782028,
0.)) ;
#55248 = CARTESIAN_POINT('',(0.710049867689371,-16.1877442736409,27.8183675986852)) ;
#55249 = CARTESIAN_POINT('Ctrl Pts',(0.710049867894279,-16.1877442737198,
27.818367598746)) ;
#55250 = CARTESIAN_POINT('Ctrl Pts',(0.71937232800943,-16.0510971575386,28.548958129221)) ;
#55251 = CARTESIAN_POINT('Ctrl Pts',(0.728694788142444,-15.9108618782028,
29.2987329505603)) ;
#55252 = CARTESIAN_POINT('',(2.67870907039602,-15.9108618818335,29.1851206195401)) ;
#55253 = CARTESIAN_POINT('Ctrl Pts',(0.710049867585909,-16.1877442734701,
27.8183675986327)) ;
#55254 = CARTESIAN_POINT('Ctrl Pts',(0.782550419741599,-16.1843471450139,
27.8346858875108)) ;
#55255 = CARTESIAN_POINT('Ctrl Pts',(0.854772362736772,-16.1804174769264,
27.8535784930083)) ;
#55256 = CARTESIAN_POINT('Ctrl Pts',(0.926357802409753,-16.1759680067789,
27.8750019698647)) ;
#55257 = CARTESIAN_POINT('Ctrl Pts',(0.99794324212217,-16.171518536629,27.8964254467329)) ;
#55258 = CARTESIAN_POINT('Ctrl Pts',(1.06889155461827,-16.166549308068,27.9203796780022)) ;
#55259 = CARTESIAN_POINT('Ctrl Pts',(1.13885870823377,-16.1610860188908,27.9467624338955)) ;
#55260 = CARTESIAN_POINT('Ctrl Pts',(1.20589870269909,-16.155851292919,27.9720414357938)) ;
#55261 = CARTESIAN_POINT('Ctrl Pts',(1.27208129921876,-16.1501596984486,27.9995659692902)) ;
#55262 = CARTESIAN_POINT('Ctrl Pts',(1.33711948715304,-16.1440425621066,28.029206118038)) ;
#55263 = CARTESIAN_POINT('Ctrl Pts',(1.40229204276538,-16.1379127878754,28.0589075027779)) ;
#55264 = CARTESIAN_POINT('Ctrl Pts',(1.46631500311679,-16.1313557844549,28.0907330142736)) ;
#55265 = CARTESIAN_POINT('Ctrl Pts',(1.52892488635768,-16.1244124680045,28.1245069677666)) ;
#55266 = CARTESIAN_POINT('Ctrl Pts',(1.57610246709302,-16.1191805644222,28.1499561993445)) ;
#55267 = CARTESIAN_POINT('Ctrl Pts',(1.62247820870467,-16.1137295207044,28.1765107692402)) ;
#55268 = CARTESIAN_POINT('Ctrl Pts',(1.66795107444096,-16.108079933754,28.2040801346692)) ;
#55269 = CARTESIAN_POINT('Ctrl Pts',(1.72654567184455,-16.1008000918637,28.2396049656167)) ;
#55270 = CARTESIAN_POINT('Ctrl Pts',(1.78364808634439,-16.0931892946345,28.2768212428165)) ;
#55271 = CARTESIAN_POINT('Ctrl Pts',(1.83904830057331,-16.0853002129681,28.3154913152495)) ;
#55272 = CARTESIAN_POINT('Ctrl Pts',(1.89490026940932,-16.0773468007023,28.354476718293)) ;
#55273 = CARTESIAN_POINT('Ctrl Pts',(1.94902184426688,-16.0691106491233,28.3949393342471)) ;
#55274 = CARTESIAN_POINT('Ctrl Pts',(2.00123869002606,-16.0606518030571,28.4366020430871)) ;
#55275 = CARTESIAN_POINT('Ctrl Pts',(2.04400095167941,-16.0537245483847,28.4707211406828)) ;
#55276 = CARTESIAN_POINT('Ctrl Pts',(2.08548652071937,-16.0466480826282,28.5056443478157)) ;
#55277 = CARTESIAN_POINT('Ctrl Pts',(2.12562170484212,-16.0394576303854,28.5412058347734)) ;
#55278 = CARTESIAN_POINT('Ctrl Pts',(2.17471104292392,-16.0306629892538,28.5847010844929)) ;
#55279 = CARTESIAN_POINT('Ctrl Pts',(2.22303830969206,-16.0214720150689,28.6302676731548)) ;
#55280 = CARTESIAN_POINT('Ctrl Pts',(2.27028343973035,-16.0119118209665,28.677801470837)) ;
#55281 = CARTESIAN_POINT('Ctrl Pts',(2.31714161877286,-16.0024299275614,28.7249459532537)) ;
#55282 = CARTESIAN_POINT('Ctrl Pts',(2.36293486000431,-15.9925848997548,28.7740253648491)) ;
#55283 = CARTESIAN_POINT('Ctrl Pts',(2.40737440854123,-15.9824119250019,28.8248935681996)) ;
#55284 = CARTESIAN_POINT('Ctrl Pts',(2.44386368784915,-15.9740589032144,28.866661411057)) ;
#55285 = CARTESIAN_POINT('Ctrl Pts',(2.47944062106131,-15.965484957055,28.9096343859912)) ;
#55286 = CARTESIAN_POINT('Ctrl Pts',(2.5139605303064,-15.9567135267634,28.9537104571357)) ;
#55287 = CARTESIAN_POINT('Ctrl Pts',(2.55720618635062,-15.9457249040902,29.0089278274643)) ;
#55288 = CARTESIAN_POINT('Ctrl Pts',(2.59879837753547,-15.9344245943244,29.0658854070521)) ;
#55289 = CARTESIAN_POINT('Ctrl Pts',(2.63850199913644,-15.9228603613915,29.1243704314812)) ;
#55290 = CARTESIAN_POINT('Ctrl Pts',(2.65212933554176,-15.9188912098105,29.1444440436715)) ;
#55291 = CARTESIAN_POINT('Ctrl Pts',(2.66553450938055,-15.9148910209383,29.1646972815063)) ;
#55292 = CARTESIAN_POINT('Ctrl Pts',(2.67870905771655,-15.9108618853164,29.1851205952931)) ;
#55293 = CARTESIAN_POINT('',(3.65785625118284,-15.9108619763187,29.0786312869383)) ;
#55294 = CARTESIAN_POINT('Origin',(-2.92277791062251E-15,-15.9108618782028,
0.)) ;
#55295 = CARTESIAN_POINT('',(5.28667743227854,-16.1877442736409,27.3206293558036)) ;
#55296 = CARTESIAN_POINT('Ctrl Pts',(3.65785616022789,-15.9108620121299,29.0786312426591)) ;
#55297 = CARTESIAN_POINT('Ctrl Pts',(3.68255160322085,-15.9226010082282,29.0122670155031)) ;
#55298 = CARTESIAN_POINT('Ctrl Pts',(3.70947267289441,-15.9340938647544,28.9468937518395)) ;
#55299 = CARTESIAN_POINT('Ctrl Pts',(3.7384507497277,-15.9452907435695,28.8827789144254)) ;
#55300 = CARTESIAN_POINT('Ctrl Pts',(3.74839669099248,-15.9491337694433,28.860773230239)) ;
#55301 = CARTESIAN_POINT('Ctrl Pts',(3.75858456122854,-15.9529419792521,28.838915568187)) ;
#55302 = CARTESIAN_POINT('Ctrl Pts',(3.76900635257187,-15.9567135267634,28.8172159983899)) ;
#55303 = CARTESIAN_POINT('Ctrl Pts',(3.79848556805471,-15.9673817754481,28.7558363110733)) ;
#55304 = CARTESIAN_POINT('Ctrl Pts',(3.82984370951264,-15.9777576912908,28.6957149964714)) ;
#55305 = CARTESIAN_POINT('Ctrl Pts',(3.86286245965529,-15.9877997661729,28.6370843858239)) ;
#55306 = CARTESIAN_POINT('Ctrl Pts',(3.89615022934365,-15.9979236586407,28.5779760835566)) ;
#55307 = CARTESIAN_POINT('Ctrl Pts',(3.93112541543707,-16.0077081692741,28.5203832304025)) ;
#55308 = CARTESIAN_POINT('Ctrl Pts',(3.96752580131824,-16.0171189356801,28.4645080220079)) ;
#55309 = CARTESIAN_POINT('Ctrl Pts',(3.99731347940591,-16.0248200870134,28.4187834319947)) ;
#55310 = CARTESIAN_POINT('Ctrl Pts',(4.02805474141638,-16.0322710948773,28.3742084763029)) ;
#55311 = CARTESIAN_POINT('Ctrl Pts',(4.05958973184228,-16.0394576303853,28.3308741366044)) ;
#55312 = CARTESIAN_POINT('Ctrl Pts',(4.09817392269338,-16.0482506141109,28.2778530190853)) ;
#55313 = CARTESIAN_POINT('Ctrl Pts',(4.13893683564045,-16.056873031955,28.2253303779792)) ;
#55314 = CARTESIAN_POINT('Ctrl Pts',(4.18180753346602,-16.0652608298866,28.1736299959803)) ;
#55315 = CARTESIAN_POINT('Ctrl Pts',(4.22432681630937,-16.0735798722811,28.1223534066824)) ;
#55316 = CARTESIAN_POINT('Ctrl Pts',(4.26891932692231,-16.0816680200511,28.0718861140696)) ;
#55317 = CARTESIAN_POINT('Ctrl Pts',(4.31546813252718,-16.0894673869313,28.0225263233196)) ;
#55318 = CARTESIAN_POINT('Ctrl Pts',(4.35371752942058,-16.0958761674669,27.9819671252383)) ;
#55319 = CARTESIAN_POINT('Ctrl Pts',(4.39328689075978,-16.1020900207685,27.9421555049558)) ;
#55320 = CARTESIAN_POINT('Ctrl Pts',(4.43408821707899,-16.1080799337539,27.9032445911354)) ;
#55321 = CARTESIAN_POINT('Ctrl Pts',(4.48517387546492,-16.1155796568301,27.8545258402948)) ;
#55322 = CARTESIAN_POINT('Ctrl Pts',(4.53819928410433,-16.1227292229207,27.8072126693859)) ;
#55323 = CARTESIAN_POINT('Ctrl Pts',(4.59297412683163,-16.1294814162036,27.761558849699)) ;
#55324 = CARTESIAN_POINT('Ctrl Pts',(4.64764066974046,-16.1362202591732,27.7159952959104)) ;
#55325 = CARTESIAN_POINT('Ctrl Pts',(4.70404939984709,-16.1425632136357,27.6720849152461)) ;
#55326 = CARTESIAN_POINT('Ctrl Pts',(4.76197293970087,-16.1484717649149,27.6300458284021)) ;
#55327 = CARTESIAN_POINT('Ctrl Pts',(4.80565624764355,-16.1529277264406,27.5983418548384)) ;
#55328 = CARTESIAN_POINT('Ctrl Pts',(4.85020027465751,-16.1571367885211,27.5677015056432)) ;
#55329 = CARTESIAN_POINT('Ctrl Pts',(4.89549499837679,-16.1610860188908,27.538203616336)) ;
#55330 = CARTESIAN_POINT('Ctrl Pts',(4.95815484617414,-16.166549308068,27.4973968048011)) ;
#55331 = CARTESIAN_POINT('Ctrl Pts',(5.02229497491018,-16.171518536629,27.4587508201776)) ;
#55332 = CARTESIAN_POINT('Ctrl Pts',(5.08760137256992,-16.1759680067789,27.4224394588056)) ;
#55333 = CARTESIAN_POINT('Ctrl Pts',(5.1529077701937,-16.1804174769265,27.3861280974535)) ;
#55334 = CARTESIAN_POINT('Ctrl Pts',(5.21937985257595,-16.184347145014,27.352151607695)) ;
#55335 = CARTESIAN_POINT('Ctrl Pts',(5.28667743236823,-16.1877442734702,27.32062935573)) ;
#55336 = CARTESIAN_POINT('',(5.58670321107024,-15.9108618782028,28.7703926951637)) ;
#55337 = CARTESIAN_POINT('Ctrl Pts',(5.58670321107023,-15.9108618782028,28.7703926951638)) ;
#55338 = CARTESIAN_POINT('Ctrl Pts',(5.43462829348381,-16.0510971578892,28.0361431372959)) ;
#55339 = CARTESIAN_POINT('Ctrl Pts',(5.2866774320916,-16.1877442737199,27.3206293559071)) ;
#55340 = CARTESIAN_POINT('',(7.01001982894394,-15.9108618782028,28.4570970163916)) ;
#55341 = CARTESIAN_POINT('Origin',(-2.92277791062251E-15,-15.9108618782028,
0.)) ;
#55342 = CARTESIAN_POINT('',(6.67357602500404,-16.1877442736409,27.0153498905466)) ;
#55343 = CARTESIAN_POINT('Ctrl Pts',(6.67357602521708,-16.1877442737199,27.015349890562)) ;
#55344 = CARTESIAN_POINT('Ctrl Pts',(6.83973589941515,-16.0510971574815,27.726855567374)) ;
#55345 = CARTESIAN_POINT('Ctrl Pts',(7.01001982894397,-15.9108618782028,28.4570970163916)) ;
#55346 = CARTESIAN_POINT('',(8.89001990812046,-15.9108619763187,27.92694497988)) ;
#55347 = CARTESIAN_POINT('Ctrl Pts',(6.67357602499615,-16.1877442734654,27.0153498905179)) ;
#55348 = CARTESIAN_POINT('Ctrl Pts',(6.74788950417132,-16.184347145014,27.0157011912573)) ;
#55349 = CARTESIAN_POINT('Ctrl Pts',(6.82248428999461,-16.1804174769264,27.0186265152585)) ;
#55350 = CARTESIAN_POINT('Ctrl Pts',(6.89700151611982,-16.1759680067789,27.024160369652)) ;
#55351 = CARTESIAN_POINT('Ctrl Pts',(6.97151874228602,-16.171518536629,27.0296942240486)) ;
#55352 = CARTESIAN_POINT('Ctrl Pts',(7.04595777430382,-16.166549308068,27.0378366287329)) ;
#55353 = CARTESIAN_POINT('Ctrl Pts',(7.1199606473979,-16.1610860188908,27.0485617006416)) ;
#55354 = CARTESIAN_POINT('Ctrl Pts',(7.19086752221375,-16.155851292919,27.0588380764014)) ;
#55355 = CARTESIAN_POINT('Ctrl Pts',(7.26141976748762,-16.1501596984485,27.0714917996922)) ;
#55356 = CARTESIAN_POINT('Ctrl Pts',(7.33130915455475,-16.1440425621065,27.0864576903428)) ;
#55357 = CARTESIAN_POINT('Ctrl Pts',(7.40134293178645,-16.1379127878753,27.1014545002433)) ;
#55358 = CARTESIAN_POINT('Ctrl Pts',(7.47071061511937,-16.1313557844548,27.1187729049957)) ;
#55359 = CARTESIAN_POINT('Ctrl Pts',(7.53911711573318,-16.1244124680043,27.1382979680627)) ;
#55360 = CARTESIAN_POINT('Ctrl Pts',(7.59066254336305,-16.1191805644221,27.1530104254499)) ;
#55361 = CARTESIAN_POINT('Ctrl Pts',(7.6416624934871,-16.1137295207043,27.1689747506686)) ;
#55362 = CARTESIAN_POINT('Ctrl Pts',(7.69199882751456,-16.1080799337539,27.1861242376894)) ;
#55363 = CARTESIAN_POINT('Ctrl Pts',(7.75686030433953,-16.1008000918637,27.208222411433)) ;
#55364 = CARTESIAN_POINT('Ctrl Pts',(7.82062809561323,-16.0931892946345,27.2322932615711)) ;
#55365 = CARTESIAN_POINT('Ctrl Pts',(7.88304600611371,-16.0853002129681,27.2581498407593)) ;
#55366 = CARTESIAN_POINT('Ctrl Pts',(7.94597289620977,-16.0773468007023,27.2842172644169)) ;
#55367 = CARTESIAN_POINT('Ctrl Pts',(8.00752740508663,-16.0691106491234,27.3120993481233)) ;
#55368 = CARTESIAN_POINT('Ctrl Pts',(8.06747970086894,-16.0606518030573,27.3415629276636)) ;
#55369 = CARTESIAN_POINT('Ctrl Pts',(8.1165768020383,-16.0537245483848,27.3656917175059)) ;
#55370 = CARTESIAN_POINT('Ctrl Pts',(8.16459991873938,-16.0466480826282,27.3908802684245)) ;
#55371 = CARTESIAN_POINT('Ctrl Pts',(8.21144143306702,-16.0394576303854,27.4169824693804)) ;
#55372 = CARTESIAN_POINT('Ctrl Pts',(8.26873328268348,-16.0306629892538,27.4489080677152)) ;
#55373 = CARTESIAN_POINT('Ctrl Pts',(8.32572615443434,-16.0214720150688,27.4830204010448)) ;
#55374 = CARTESIAN_POINT('Ctrl Pts',(8.3820850809998,-16.0119118209664,27.5192865785502)) ;
#55375 = CARTESIAN_POINT('Ctrl Pts',(8.43798241199483,-16.0024299275613,27.5552557257907)) ;
#55376 = CARTESIAN_POINT('Ctrl Pts',(8.49325565541029,-15.9925848997546,27.5933434947909)) ;
#55377 = CARTESIAN_POINT('Ctrl Pts',(8.54759139206526,-15.9824119250015,27.6334692385036)) ;
#55378 = CARTESIAN_POINT('Ctrl Pts',(8.59220642386558,-15.9740589032141,27.6664164559697)) ;
#55379 = CARTESIAN_POINT('Ctrl Pts',(8.63618950748789,-15.9654849570549,27.700736757636)) ;
#55380 = CARTESIAN_POINT('Ctrl Pts',(8.67937741285401,-15.9567135267634,27.7363615946437)) ;
#55381 = CARTESIAN_POINT('Ctrl Pts',(8.73348211207143,-15.9457249040552,27.7809914759642)) ;
#55382 = CARTESIAN_POINT('Ctrl Pts',(8.78634609706161,-15.9344245942523,27.8276763275003)) ;
#55383 = CARTESIAN_POINT('Ctrl Pts',(8.83769402165478,-15.9228603612807,27.8762588997127)) ;
#55384 = CARTESIAN_POINT('Ctrl Pts',(8.85531780635308,-15.9188912514538,27.8929335520875)) ;
#55385 = CARTESIAN_POINT('Ctrl Pts',(8.87276324047922,-15.914891104989,27.909831384247)) ;
#55386 = CARTESIAN_POINT('Ctrl Pts',(8.89002000637735,-15.9108620123611,27.9269448892862)) ;
#55387 = CARTESIAN_POINT('',(9.82338358164146,-15.9108618855281,27.6124587235785)) ;
#55388 = CARTESIAN_POINT('Origin',(-2.92277791062251E-15,-15.9108618782028,
0.)) ;
#55389 = CARTESIAN_POINT('',(11.0362055712312,-16.1877442736409,25.5454088489437)) ;
#55390 = CARTESIAN_POINT('Ctrl Pts',(9.82338358613002,-15.9108619063809,27.61245868618)) ;
#55391 = CARTESIAN_POINT('Ctrl Pts',(9.83323530215201,-15.922600904189,27.5423372231927)) ;
#55392 = CARTESIAN_POINT('Ctrl Pts',(9.84547363914043,-15.9340937625734,27.4727051106785)) ;
#55393 = CARTESIAN_POINT('Ctrl Pts',(9.85999141653387,-15.9452906433748,27.4038598065403)) ;
#55394 = CARTESIAN_POINT('Ctrl Pts',(9.86497429424729,-15.9491337032519,27.3802303126882)) ;
#55395 = CARTESIAN_POINT('Ctrl Pts',(9.8702252698575,-15.952941946475,27.3566933742252)) ;
#55396 = CARTESIAN_POINT('Ctrl Pts',(9.87573868735361,-15.9567135267634,27.3332605475947)) ;
#55397 = CARTESIAN_POINT('Ctrl Pts',(9.89133387675787,-15.9673817754481,27.2669787233288)) ;
#55398 = CARTESIAN_POINT('Ctrl Pts',(9.90903457682846,-15.9777576912908,27.2015219381791)) ;
#55399 = CARTESIAN_POINT('Ctrl Pts',(9.92867751876087,-15.9877997661728,27.1371640233736)) ;
#55400 = CARTESIAN_POINT('Ctrl Pts',(9.94848050113368,-15.9979236586406,27.0722817538628)) ;
#55401 = CARTESIAN_POINT('Ctrl Pts',(9.9702572258167,-16.007708169274,27.0085167584596)) ;
#55402 = CARTESIAN_POINT('Ctrl Pts',(9.99379507275848,-16.01711893568,26.9461228744104)) ;
#55403 = CARTESIAN_POINT('Ctrl Pts',(10.0130568962422,-16.0248200870133,26.8950638296305)) ;
#55404 = CARTESIAN_POINT('Ctrl Pts',(10.0334971467828,-16.0322710948773,26.8449225490046)) ;
#55405 = CARTESIAN_POINT('Ctrl Pts',(10.0549792645757,-16.0394576303854,26.7958222513128)) ;
#55406 = CARTESIAN_POINT('Ctrl Pts',(10.0812634055125,-16.0482506141108,26.7357462775652)) ;
#55407 = CARTESIAN_POINT('Ctrl Pts',(10.1097824889273,-16.0568730319548,26.6756887652808)) ;
#55408 = CARTESIAN_POINT('Ctrl Pts',(10.1405368397836,-16.0652608298864,26.6159811766996)) ;
#55409 = CARTESIAN_POINT('Ctrl Pts',(10.1710390944484,-16.0735798722808,26.5567630166145)) ;
#55410 = CARTESIAN_POINT('Ctrl Pts',(10.2037400808343,-16.0816680200508,26.4978895496216)) ;
#55411 = CARTESIAN_POINT('Ctrl Pts',(10.2385897052852,-16.089467386931,26.4396771461177)) ;
#55412 = CARTESIAN_POINT('Ctrl Pts',(10.2672258238691,-16.0958761674667,26.3918437098595)) ;
#55413 = CARTESIAN_POINT('Ctrl Pts',(10.2973117539923,-16.1020900207684,26.3444566201085)) ;
#55414 = CARTESIAN_POINT('Ctrl Pts',(10.3287944717035,-16.1080799337539,26.2976843427491)) ;
#55415 = CARTESIAN_POINT('Ctrl Pts',(10.3682126844706,-16.1155796568301,26.2391227027578)) ;
#55416 = CARTESIAN_POINT('Ctrl Pts',(10.4098274553449,-16.1227292229208,26.1815167920545)) ;
#55417 = CARTESIAN_POINT('Ctrl Pts',(10.4535074709729,-16.1294814162037,26.1251553612478)) ;
#55418 = CARTESIAN_POINT('Ctrl Pts',(10.497101123272,-16.1362202591734,26.0689053672325)) ;
#55419 = CARTESIAN_POINT('Ctrl Pts',(10.5427516147545,-16.1425632136358,26.0138953773238)) ;
#55420 = CARTESIAN_POINT('Ctrl Pts',(10.5902837734305,-16.148471764915,25.9603872921075)) ;
#55421 = CARTESIAN_POINT('Ctrl Pts',(10.626130372755,-16.1529277264407,25.9200339198896)) ;
#55422 = CARTESIAN_POINT('Ctrl Pts',(10.6630462158159,-16.1571367885211,25.8805342759359)) ;
#55423 = CARTESIAN_POINT('Ctrl Pts',(10.7009407998153,-16.1610860188908,25.8419890041916)) ;
#55424 = CARTESIAN_POINT('Ctrl Pts',(10.7533634369525,-16.166549308068,25.7886662181691)) ;
#55425 = CARTESIAN_POINT('Ctrl Pts',(10.8076962607951,-16.171518536629,25.7371355234806)) ;
#55426 = CARTESIAN_POINT('Ctrl Pts',(10.8636699618301,-16.1759680067789,25.6876341565054)) ;
#55427 = CARTESIAN_POINT('Ctrl Pts',(10.9196436628344,-16.1804174769265,25.6381327895573)) ;
#55428 = CARTESIAN_POINT('Ctrl Pts',(10.9772577239095,-16.184347145014,25.5906611184369)) ;
#55429 = CARTESIAN_POINT('Ctrl Pts',(11.0362055713028,-16.1877442734702,25.5454088488525)) ;
#55430 = CARTESIAN_POINT('',(11.6408731773052,-15.9108618782029,26.8967808533365)) ;
#55431 = CARTESIAN_POINT('Ctrl Pts',(11.6408731773062,-15.9108618782028,26.8967808533361)) ;
#55432 = CARTESIAN_POINT('Ctrl Pts',(11.3345117375673,-16.051097157219,26.2123892573509)) ;
#55433 = CARTESIAN_POINT('Ctrl Pts',(11.0362055710711,-16.1877442737198,25.5454088490849)) ;
#55434 = CARTESIAN_POINT('',(12.9635641336247,-15.9108618782029,26.2848388535276)) ;
#55435 = CARTESIAN_POINT('Origin',(-2.92277791062251E-15,-15.9108618782028,
0.)) ;
#55436 = CARTESIAN_POINT('',(12.325053184539,-16.1877442736409,24.9491244469311)) ;
#55437 = CARTESIAN_POINT('Ctrl Pts',(12.3250531847502,-16.1877442737198,24.9491244469006)) ;
#55438 = CARTESIAN_POINT('Ctrl Pts',(12.6402810223916,-16.0510971573044,25.6082760559321)) ;
#55439 = CARTESIAN_POINT('Ctrl Pts',(12.9635641336236,-15.9108618782028,26.2848388535281)) ;
#55440 = CARTESIAN_POINT('',(14.6856444869838,-15.9108618855281,25.36293728564)) ;
#55441 = CARTESIAN_POINT('Ctrl Pts',(12.3250531844232,-16.1877442734702,24.9491244469267)) ;
#55442 = CARTESIAN_POINT('Ctrl Pts',(12.3977047751286,-16.184347145014,24.9334923330962)) ;
#55443 = CARTESIAN_POINT('Ctrl Pts',(12.4711844345007,-16.1804174769265,24.920313590702)) ;
#55444 = CARTESIAN_POINT('Ctrl Pts',(12.545149104404,-16.1759680067789,24.9096990657516)) ;
#55445 = CARTESIAN_POINT('Ctrl Pts',(12.6191137743479,-16.171518536629,24.8990845407954)) ;
#55446 = CARTESIAN_POINT('Ctrl Pts',(12.693562839483,-16.1665493080681,24.8910343891013)) ;
#55447 = CARTESIAN_POINT('Ctrl Pts',(12.7681411399577,-16.1610860188908,24.8856002845829)) ;
#55448 = CARTESIAN_POINT('Ctrl Pts',(12.8395993684648,-16.155851292919,24.8803935222949)) ;
#55449 = CARTESIAN_POINT('Ctrl Pts',(12.9112223179169,-16.1501596984485,24.8775847613426)) ;
#55450 = CARTESIAN_POINT('Ctrl Pts',(12.982694954054,-16.1440425621065,24.8771766054826)) ;
#55451 = CARTESIAN_POINT('Ctrl Pts',(13.0543152513185,-16.1379127878753,24.8767676063803)) ;
#55452 = CARTESIAN_POINT('Ctrl Pts',(13.1257841018569,-16.1313557844548,24.8787691150311)) ;
#55453 = CARTESIAN_POINT('Ctrl Pts',(13.1967886079032,-16.1244124680043,24.8831323174237)) ;
#55454 = CARTESIAN_POINT('Ctrl Pts',(13.2502916755205,-16.1191805644221,24.8864200624646)) ;
#55455 = CARTESIAN_POINT('Ctrl Pts',(13.3035311331718,-16.1137295207043,24.8910476689023)) ;
#55456 = CARTESIAN_POINT('Ctrl Pts',(13.3563772644564,-16.1080799337539,24.8969753865622)) ;
#55457 = CARTESIAN_POINT('Ctrl Pts',(13.4244727701354,-16.1008000918637,24.9046136170581)) ;
#55458 = CARTESIAN_POINT('Ctrl Pts',(13.4919242271365,-16.0931892946344,24.9144135139351)) ;
#55459 = CARTESIAN_POINT('Ctrl Pts',(13.5584412417866,-16.0853002129679,24.9262475749734)) ;
#55460 = CARTESIAN_POINT('Ctrl Pts',(13.6255006617006,-16.0773468007021,24.9381781354869)) ;
#55461 = CARTESIAN_POINT('Ctrl Pts',(13.6916098841753,-16.0691106491231,24.9521759517005)) ;
#55462 = CARTESIAN_POINT('Ctrl Pts',(13.7564943272627,-16.0606518030569,24.9680627177085)) ;
#55463 = CARTESIAN_POINT('Ctrl Pts',(13.8096305420636,-16.0537245483846,24.9810729644013)) ;
#55464 = CARTESIAN_POINT('Ctrl Pts',(13.8619456988614,-16.0466480826281,24.9953490704592)) ;
#55465 = CARTESIAN_POINT('Ctrl Pts',(13.9133032862433,-16.0394576303854,25.0107714755065)) ;
#55466 = CARTESIAN_POINT('Ctrl Pts',(13.9761187441819,-16.0306629892537,25.0296346169612)) ;
#55467 = CARTESIAN_POINT('Ctrl Pts',(14.0391122975756,-16.0214720150687,25.0506976401651)) ;
#55468 = CARTESIAN_POINT('Ctrl Pts',(14.1019497399007,-16.0119118209662,25.0740004313405)) ;
#55469 = CARTESIAN_POINT('Ctrl Pts',(14.1642725257765,-16.002429927561,25.0971123660564)) ;
#55470 = CARTESIAN_POINT('Ctrl Pts',(14.2264412559457,-15.9925848997543,25.1224275507145)) ;
#55471 = CARTESIAN_POINT('Ctrl Pts',(14.2881325020626,-15.9824119250012,25.1499345996097)) ;
#55472 = CARTESIAN_POINT('Ctrl Pts',(14.3387871370542,-15.9740589032139,25.1725206164141)) ;
#55473 = CARTESIAN_POINT('Ctrl Pts',(14.3891197709798,-15.9654849570548,25.1965834656511)) ;
#55474 = CARTESIAN_POINT('Ctrl Pts',(14.4389562540117,-15.9567135267634,25.222091290738)) ;
#55475 = CARTESIAN_POINT('Ctrl Pts',(14.5013901204959,-15.9457249040844,25.2540468391412)) ;
#55476 = CARTESIAN_POINT('Ctrl Pts',(14.5630540378178,-15.9344245943125,25.2882760305698)) ;
#55477 = CARTESIAN_POINT('Ctrl Pts',(14.623645293248,-15.9228603613731,25.3246844831794)) ;
#55478 = CARTESIAN_POINT('Ctrl Pts',(14.6444417835184,-15.9188912167151,25.3371808083518)) ;
#55479 = CARTESIAN_POINT('Ctrl Pts',(14.6651120677952,-15.9148910348743,25.3499334400899)) ;
#55480 = CARTESIAN_POINT('Ctrl Pts',(14.6856444555743,-15.9108619063809,25.3629372648498)) ;
#55481 = CARTESIAN_POINT('',(15.5295807620182,-15.910861895547,24.8551575119669)) ;
#55482 = CARTESIAN_POINT('Origin',(-2.92277791062251E-15,-15.9108618782028,
0.)) ;
#55483 = CARTESIAN_POINT('',(16.2696930035343,-16.1877442736409,22.5757134159901)) ;
#55484 = CARTESIAN_POINT('Ctrl Pts',(15.5295807250489,-15.910861929778,24.855157512034)) ;
#55485 = CARTESIAN_POINT('Ctrl Pts',(15.5241280748862,-15.9226009272666,24.7845576220652)) ;
#55486 = CARTESIAN_POINT('Ctrl Pts',(15.5211114436977,-15.9340937852961,24.7139225890774)) ;
#55487 = CARTESIAN_POINT('Ctrl Pts',(15.5204901013657,-15.9452906657112,24.6435659572226)) ;
#55488 = CARTESIAN_POINT('Ctrl Pts',(15.5202768409764,-15.9491337180079,24.6194177833012)) ;
#55489 = CARTESIAN_POINT('Ctrl Pts',(15.5203453060798,-15.952941953782,24.5953023676499)) ;
#55490 = CARTESIAN_POINT('Ctrl Pts',(15.52069245721,-15.9567135267634,24.571232212331)) ;
#55491 = CARTESIAN_POINT('Ctrl Pts',(15.521674406812,-15.9673817754482,24.5031475155512)) ;
#55492 = CARTESIAN_POINT('Ctrl Pts',(15.524890000433,-15.9777576912909,24.4354159463767)) ;
#55493 = CARTESIAN_POINT('Ctrl Pts',(15.530238652022,-15.987799766173,24.3683400319804)) ;
#55494 = CARTESIAN_POINT('Ctrl Pts',(15.5356308816331,-15.9979236586409,24.3007176180363)) ;
#55495 = CARTESIAN_POINT('Ctrl Pts',(15.5431908894628,-16.0077081692743,24.233762060699)) ;
#55496 = CARTESIAN_POINT('Ctrl Pts',(15.5527655939029,-16.0171189356804,24.1677669696667)) ;
#55497 = CARTESIAN_POINT('Ctrl Pts',(15.5606009013244,-16.0248200870136,24.113760934307)) ;
#55498 = CARTESIAN_POINT('Ctrl Pts',(15.5697843769972,-16.0322710948774,24.0603978793023)) ;
#55499 = CARTESIAN_POINT('Ctrl Pts',(15.5802091422045,-16.0394576303854,24.0078274989672)) ;
#55500 = CARTESIAN_POINT('Ctrl Pts',(15.5929642160101,-16.048250614111,23.9435057547523)) ;
#55501 = CARTESIAN_POINT('Ctrl Pts',(15.6079059492495,-16.0568730319551,23.8787215938134)) ;
#55502 = CARTESIAN_POINT('Ctrl Pts',(15.6251059138724,-16.0652608298868,23.8137986591302)) ;
#55503 = CARTESIAN_POINT('Ctrl Pts',(15.6421648888317,-16.0735798722812,23.7494079036065)) ;
#55504 = CARTESIAN_POINT('Ctrl Pts',(15.6614452892122,-16.0816680200513,23.6848811201159)) ;
#55505 = CARTESIAN_POINT('Ctrl Pts',(15.6829662028032,-16.0894673869315,23.6205380511466)) ;
#55506 = CARTESIAN_POINT('Ctrl Pts',(15.7006500499983,-16.0958761674671,23.5676670150303)) ;
#55507 = CARTESIAN_POINT('Ctrl Pts',(15.7198457642496,-16.1020900207686,23.5149202234632)) ;
#55508 = CARTESIAN_POINT('Ctrl Pts',(15.7405377764617,-16.1080799337539,23.4624736022729)) ;
#55509 = CARTESIAN_POINT('Ctrl Pts',(15.7664453917911,-16.1155796568301,23.3968073503301)) ;
#55510 = CARTESIAN_POINT('Ctrl Pts',(15.7947036644655,-16.1227292229208,23.3316022881925)) ;
#55511 = CARTESIAN_POINT('Ctrl Pts',(15.8252464240103,-16.1294814162038,23.2671686441292)) ;
#55512 = CARTESIAN_POINT('Ctrl Pts',(15.8557287949689,-16.1362202591735,23.2028623970899)) ;
#55513 = CARTESIAN_POINT('Ctrl Pts',(15.8884864815826,-16.142563213636,23.1393250039253)) ;
#55514 = CARTESIAN_POINT('Ctrl Pts',(15.9234047081693,-16.1484717649152,23.0768498989313)) ;
#55515 = CARTESIAN_POINT('Ctrl Pts',(15.9497384517319,-16.1529277264408,23.0297340068949)) ;
#55516 = CARTESIAN_POINT('Ctrl Pts',(15.9772999670473,-16.1571367885212,22.9832220276334)) ;
#55517 = CARTESIAN_POINT('Ctrl Pts',(16.0060225026959,-16.1610860188908,22.9374317075191)) ;
#55518 = CARTESIAN_POINT('Ctrl Pts',(16.0457567049241,-16.1665493080681,22.8740862612195)) ;
#55519 = CARTESIAN_POINT('Ctrl Pts',(16.0877416814169,-16.171518536629,22.8120803744774)) ;
#55520 = CARTESIAN_POINT('Ctrl Pts',(16.1317654177772,-16.1759680067789,22.7517036308018)) ;
#55521 = CARTESIAN_POINT('Ctrl Pts',(16.1757891541133,-16.1804174769265,22.6913268871595)) ;
#55522 = CARTESIAN_POINT('Ctrl Pts',(16.2218512244188,-16.184347145014,22.6325797572578)) ;
#55523 = CARTESIAN_POINT('Ctrl Pts',(16.2696930035848,-16.1877442734701,22.5757134158856)) ;
#55524 = CARTESIAN_POINT('',(17.1507288516716,-15.9108618782029,23.7655054324319)) ;
#55525 = CARTESIAN_POINT('Ctrl Pts',(17.150728851672,-15.9108618782028,23.7655054324317)) ;
#55526 = CARTESIAN_POINT('Ctrl Pts',(16.7044060094453,-16.05109715723,23.1629731851543)) ;
#55527 = CARTESIAN_POINT('Ctrl Pts',(16.269693003408,-16.1877442737199,22.5757134161625)) ;
#55528 = CARTESIAN_POINT('',(18.3109465873825,-15.9108618782029,22.883530839373)) ;
#55529 = CARTESIAN_POINT('Origin',(-2.92277791062251E-15,-15.9108618782028,
0.)) ;
#55530 = CARTESIAN_POINT('',(17.4002245554774,-16.1877442736409,21.7163056731371)) ;
#55531 = CARTESIAN_POINT('Ctrl Pts',(17.4002245556773,-16.1877442737199,21.7163056730615)) ;
#55532 = CARTESIAN_POINT('Ctrl Pts',(17.849780652129,-16.0510971576328,22.2922820153621)) ;
#55533 = CARTESIAN_POINT('Ctrl Pts',(18.3109465873822,-15.9108618782028,22.8835308393733)) ;
#55534 = CARTESIAN_POINT('',(19.7945838954017,-15.910861895547,21.6129864201279)) ;
#55535 = CARTESIAN_POINT('Ctrl Pts',(17.4002245553632,-16.1877442734701,21.7163056731579)) ;
#55536 = CARTESIAN_POINT('Ctrl Pts',(17.4678171498596,-16.184347145014,21.6854210850259)) ;
#55537 = CARTESIAN_POINT('Ctrl Pts',(17.5367458555749,-16.1804174769265,21.6567544995836)) ;
#55538 = CARTESIAN_POINT('Ctrl Pts',(17.6066994634976,-16.1759680067789,21.6304879186788)) ;
#55539 = CARTESIAN_POINT('Ctrl Pts',(17.6766530714588,-16.171518536629,21.6042213377595)) ;
#55540 = CARTESIAN_POINT('Ctrl Pts',(17.7476310141696,-16.166549308068,21.580355045833)) ;
#55541 = CARTESIAN_POINT('Ctrl Pts',(17.8192975435826,-16.1610860188908,21.5590158575752)) ;
#55542 = CARTESIAN_POINT('Ctrl Pts',(17.8879658184361,-16.155851292919,21.5385694196573)) ;
#55543 = CARTESIAN_POINT('Ctrl Pts',(17.9573104625531,-16.1501596984486,21.5204295090022)) ;
#55544 = CARTESIAN_POINT('Ctrl Pts',(18.0270243667303,-16.1440425621066,21.5046663915461)) ;
#55545 = CARTESIAN_POINT('Ctrl Pts',(18.0968822985277,-16.1379127878754,21.4888707077845)) ;
#55546 = CARTESIAN_POINT('Ctrl Pts',(18.1671105122519,-16.1313557844549,21.4754617320138)) ;
#55547 = CARTESIAN_POINT('Ctrl Pts',(18.2373929319436,-16.1244124680045,21.4644590552373)) ;
#55548 = CARTESIAN_POINT('Ctrl Pts',(18.2903518955713,-16.1191805644222,21.4561683566278)) ;
#55549 = CARTESIAN_POINT('Ctrl Pts',(18.3433414428818,-16.1137295207044,21.4492428625507)) ;
#55550 = CARTESIAN_POINT('Ctrl Pts',(18.3962263450592,-16.108079933754,21.44367163736)) ;
#55551 = CARTESIAN_POINT('Ctrl Pts',(18.4643718094286,-16.1008000918637,21.4364927694394)) ;
#55552 = CARTESIAN_POINT('Ctrl Pts',(18.5323529769938,-16.0931892946345,21.4315634807689)) ;
#55553 = CARTESIAN_POINT('Ctrl Pts',(18.5998588341161,-16.0853002129681,21.4288216761156)) ;
#55554 = CARTESIAN_POINT('Ctrl Pts',(18.6679151599034,-16.0773468007023,21.4260575137349)) ;
#55555 = CARTESIAN_POINT('Ctrl Pts',(18.7354879022073,-16.0691106491233,21.4255165401268)) ;
#55556 = CARTESIAN_POINT('Ctrl Pts',(18.8022705681543,-16.0606518030571,21.4270836450806)) ;
#55557 = CARTESIAN_POINT('Ctrl Pts',(18.8569613062411,-16.0537245483847,21.4283670039488)) ;
#55558 = CARTESIAN_POINT('Ctrl Pts',(18.9111223045493,-16.0466480826282,21.4310631302938)) ;
#55559 = CARTESIAN_POINT('Ctrl Pts',(18.9645945412809,-16.0394576303854,21.4350846049139)) ;
#55560 = CARTESIAN_POINT('Ctrl Pts',(19.0299964265421,-16.0306629892537,21.4400032699587)) ;
#55561 = CARTESIAN_POINT('Ctrl Pts',(19.0960451530338,-16.0214720150687,21.4470320994815)) ;
#55562 = CARTESIAN_POINT('Ctrl Pts',(19.1624229021537,-16.0119118209663,21.4562818917105)) ;
#55563 = CARTESIAN_POINT('Ctrl Pts',(19.2282569987086,-16.0024299275612,21.4654559255213)) ;
#55564 = CARTESIAN_POINT('Ctrl Pts',(19.2944142749039,-15.9925848997545,21.476814815938)) ;
#55565 = CARTESIAN_POINT('Ctrl Pts',(19.3605764163785,-15.9824119250015,21.4904169709809)) ;
#55566 = CARTESIAN_POINT('Ctrl Pts',(19.4149021001289,-15.9740589032141,21.501585690081)) ;
#55567 = CARTESIAN_POINT('Ctrl Pts',(19.4692307863376,-15.9654849570549,21.5142659348029)) ;
#55568 = CARTESIAN_POINT('Ctrl Pts',(19.5233855484792,-15.9567135267635,21.5284640304184)) ;
#55569 = CARTESIAN_POINT('Ctrl Pts',(19.591229244208,-15.9457249040779,21.5462510401065)) ;
#55570 = CARTESIAN_POINT('Ctrl Pts',(19.6588097578,-15.934424594299,21.5664240526226)) ;
#55571 = CARTESIAN_POINT('Ctrl Pts',(19.7258111644737,-15.9228603613524,21.5889559670063)) ;
#55572 = CARTESIAN_POINT('Ctrl Pts',(19.7488077403279,-15.9188912243841,21.5966894893902)) ;
#55573 = CARTESIAN_POINT('Ctrl Pts',(19.7717361594137,-15.9148910503533,21.6047004555176)) ;
#55574 = CARTESIAN_POINT('Ctrl Pts',(19.7945839053567,-15.910861929778,21.612986384524)) ;
#55575 = CARTESIAN_POINT('',(20.5096319469963,-15.910861895147,20.935656936733)) ;
#55576 = CARTESIAN_POINT('Origin',(-2.92277791062251E-15,-15.9108618782028,
0.)) ;
#55577 = CARTESIAN_POINT('',(20.742427673457,-16.1877442736409,18.5504027148089)) ;
#55578 = CARTESIAN_POINT('Ctrl Pts',(20.5096319116864,-15.9108619285365,20.935656944076)) ;
#55579 = CARTESIAN_POINT('Ctrl Pts',(20.4891298518627,-15.922600926042,20.8678797989487)) ;
#55580 = CARTESIAN_POINT('Ctrl Pts',(20.470999303531,-15.9340937840905,20.7995446603445)) ;
#55581 = CARTESIAN_POINT('Ctrl Pts',(20.4552678915474,-15.9452906645261,20.7309664976985)) ;
#55582 = CARTESIAN_POINT('Ctrl Pts',(20.4498684728762,-15.949133717225,20.7074287369299)) ;
#55583 = CARTESIAN_POINT('Ctrl Pts',(20.4447512352301,-15.9529419533943,20.683862405901)) ;
#55584 = CARTESIAN_POINT('Ctrl Pts',(20.4399158977778,-15.9567135267634,20.660280367782)) ;
#55585 = CARTESIAN_POINT('Ctrl Pts',(20.4262386927054,-15.9673817754482,20.5935763632393)) ;
#55586 = CARTESIAN_POINT('Ctrl Pts',(20.4148188222928,-15.9777576912909,20.5267370629366)) ;
#55587 = CARTESIAN_POINT('Ctrl Pts',(20.4056230865347,-15.987799766173,20.4600795441574)) ;
#55588 = CARTESIAN_POINT('Ctrl Pts',(20.3963524287203,-15.9979236586409,20.3928789346997)) ;
#55589 = CARTESIAN_POINT('Ctrl Pts',(20.3893422221328,-16.0077081692743,20.3258635828738)) ;
#55590 = CARTESIAN_POINT('Ctrl Pts',(20.3845060815328,-16.0171189356804,20.2593531419674)) ;
#55591 = CARTESIAN_POINT('Ctrl Pts',(20.3805485026257,-16.0248200870136,20.2049253782172)) ;
#55592 = CARTESIAN_POINT('Ctrl Pts',(20.3780457943152,-16.0322710948774,20.1508357459762)) ;
#55593 = CARTESIAN_POINT('Ctrl Pts',(20.3769257565024,-16.0394576303854,20.0972534155538)) ;
#55594 = CARTESIAN_POINT('Ctrl Pts',(20.3755553501015,-16.0482506141109,20.0316935141443)) ;
#55595 = CARTESIAN_POINT('Ctrl Pts',(20.3762210743253,-16.0568730319549,19.9652119399159)) ;
#55596 = CARTESIAN_POINT('Ctrl Pts',(20.3790624014848,-16.0652608298864,19.8981093834015)) ;
#55597 = CARTESIAN_POINT('Ctrl Pts',(20.3818804380289,-16.0735798722808,19.8315568726035)) ;
#55598 = CARTESIAN_POINT('Ctrl Pts',(20.3868387223103,-16.0816680200508,19.7643939732964)) ;
#55599 = CARTESIAN_POINT('Ctrl Pts',(20.3940246310398,-16.0894673869309,19.6969288492561)) ;
#55600 = CARTESIAN_POINT('Ctrl Pts',(20.3999293298064,-16.0958761674667,19.6414924041653)) ;
#55601 = CARTESIAN_POINT('Ctrl Pts',(20.407337257923,-16.1020900207684,19.5858522921285)) ;
#55602 = CARTESIAN_POINT('Ctrl Pts',(20.4162710291438,-16.108079933754,19.5301836728207)) ;
#55603 = CARTESIAN_POINT('Ctrl Pts',(20.4274566357367,-16.1155796568302,19.4604832898847)) ;
#55604 = CARTESIAN_POINT('Ctrl Pts',(20.4410370847878,-16.1227292229209,19.3907279925483)) ;
#55605 = CARTESIAN_POINT('Ctrl Pts',(20.4570144427586,-16.1294814162038,19.3212349808121)) ;
#55606 = CARTESIAN_POINT('Ctrl Pts',(20.4729602105892,-16.1362202591735,19.2518793693892)) ;
#55607 = CARTESIAN_POINT('Ctrl Pts',(20.4912933793152,-16.142563213636,19.1827855108568)) ;
#55608 = CARTESIAN_POINT('Ctrl Pts',(20.511964936346,-16.1484717649152,19.1142646525586)) ;
#55609 = CARTESIAN_POINT('Ctrl Pts',(20.527554487566,-16.1529277264408,19.0625893274493)) ;
#55610 = CARTESIAN_POINT('Ctrl Pts',(20.5444729293125,-16.1571367885212,19.0112398613358)) ;
#55611 = CARTESIAN_POINT('Ctrl Pts',(20.5626803827667,-16.1610860188908,18.9603455973274)) ;
#55612 = CARTESIAN_POINT('Ctrl Pts',(20.587868222951,-16.166549308068,18.8899394534163)) ;
#55613 = CARTESIAN_POINT('Ctrl Pts',(20.6155421812562,-16.171518536629,18.8203577009702)) ;
#55614 = CARTESIAN_POINT('Ctrl Pts',(20.6455574519583,-16.1759680067789,18.7519287300249)) ;
#55615 = CARTESIAN_POINT('Ctrl Pts',(20.6755727226438,-16.1804174769264,18.6834997591173)) ;
#55616 = CARTESIAN_POINT('Ctrl Pts',(20.7079289909665,-16.184347145014,18.6162241209359)) ;
#55617 = CARTESIAN_POINT('Ctrl Pts',(20.7424276734838,-16.1877442734701,18.550402714696)) ;
#55618 = CARTESIAN_POINT('',(21.8586355065996,-15.9108618782029,19.5229813909693)) ;
#55619 = CARTESIAN_POINT('Ctrl Pts',(21.858635506599,-15.9108618782028,19.5229813909701)) ;
#55620 = CARTESIAN_POINT('Ctrl Pts',(21.293220824393,-16.0510971566263,19.0304822327909)) ;
#55621 = CARTESIAN_POINT('Ctrl Pts',(20.7424276733708,-16.1877442737198,18.5504027150044)) ;
#55622 = CARTESIAN_POINT('',(22.80212952987,-15.9108618782029,18.412214356387)) ;
#55623 = CARTESIAN_POINT('Origin',(-2.92277791062251E-15,-15.9108618782028,
0.)) ;
#55624 = CARTESIAN_POINT('',(21.6617807651629,-16.1877442736409,17.4680565820071)) ;
#55625 = CARTESIAN_POINT('Ctrl Pts',(21.6617807653418,-16.1877442737198,17.4680565818904)) ;
#55626 = CARTESIAN_POINT('Ctrl Pts',(22.2246443813642,-16.0510971568007,17.9339256482671)) ;
#55627 = CARTESIAN_POINT('Ctrl Pts',(22.8021295298706,-15.9108618782028,18.4122143563863)) ;
#55628 = CARTESIAN_POINT('',(23.977950736946,-15.910861895147,16.8524363944926)) ;
#55629 = CARTESIAN_POINT('Ctrl Pts',(21.6617807650558,-16.1877442734701,17.4680565820518)) ;
#55630 = CARTESIAN_POINT('Ctrl Pts',(21.7211538087481,-16.184347145014,17.4233636486337)) ;
#55631 = CARTESIAN_POINT('Ctrl Pts',(21.7823085311363,-16.1804174769264,17.380549637818)) ;
#55632 = CARTESIAN_POINT('Ctrl Pts',(21.8449801241196,-16.1759680067789,17.3398591970888)) ;
#55633 = CARTESIAN_POINT('Ctrl Pts',(21.9076517171373,-16.171518536629,17.2991687563371)) ;
#55634 = CARTESIAN_POINT('Ctrl Pts',(21.9718396877089,-16.166549308068,17.2606022854635)) ;
#55635 = CARTESIAN_POINT('Ctrl Pts',(22.0372433987964,-16.1610860188908,17.2243558101925)) ;
#55636 = CARTESIAN_POINT('Ctrl Pts',(22.0999108677834,-16.155851292919,17.189625749357)) ;
#55637 = CARTESIAN_POINT('Ctrl Pts',(22.1637347280774,-16.1501596984486,17.1570028910605)) ;
#55638 = CARTESIAN_POINT('Ctrl Pts',(22.228430155617,-16.1440425621066,17.126621877861)) ;
#55639 = CARTESIAN_POINT('Ctrl Pts',(22.293259242698,-16.1379127878754,17.0961780980572)) ;
#55640 = CARTESIAN_POINT('Ctrl Pts',(22.3589630263876,-16.1313557844549,17.067985626669)) ;
#55641 = CARTESIAN_POINT('Ctrl Pts',(22.4252370318935,-16.1244124680045,17.042131543661)) ;
#55642 = CARTESIAN_POINT('Ctrl Pts',(22.4751755892518,-16.1191805644222,17.0226500652536)) ;
#55643 = CARTESIAN_POINT('Ctrl Pts',(22.5254374938827,-16.1137295207044,17.0044952990674)) ;
#55644 = CARTESIAN_POINT('Ctrl Pts',(22.5758883277042,-16.108079933754,16.9876856353241)) ;
#55645 = CARTESIAN_POINT('Ctrl Pts',(22.6408973445889,-16.1008000918637,16.9660253448722)) ;
#55646 = CARTESIAN_POINT('Ctrl Pts',(22.7062294988791,-16.0931892946344,16.9465973587139)) ;
#55647 = CARTESIAN_POINT('Ctrl Pts',(22.7715676996226,-16.085300212968,16.9294078921073)) ;
#55648 = CARTESIAN_POINT('Ctrl Pts',(22.8374386931289,-16.0773468007022,16.9120782559934)) ;
#55649 = CARTESIAN_POINT('Ctrl Pts',(22.9033153289341,-16.069110649123,16.8970237878882)) ;
#55650 = CARTESIAN_POINT('Ctrl Pts',(22.968873534505,-16.0606518030569,16.8841979557019)) ;
#55651 = CARTESIAN_POINT('Ctrl Pts',(23.0225615177478,-16.0537245483846,16.8736944183111)) ;
#55652 = CARTESIAN_POINT('Ctrl Pts',(23.0760358494802,-16.0466480826281,16.8646844970719)) ;
#55653 = CARTESIAN_POINT('Ctrl Pts',(23.1291224332011,-16.0394576303853,16.857117001581)) ;
#55654 = CARTESIAN_POINT('Ctrl Pts',(23.1940526263188,-16.0306629892538,16.8478611989052)) ;
#55655 = CARTESIAN_POINT('Ctrl Pts',(23.2600681608652,-16.0214720150689,16.8405271744905)) ;
#55656 = CARTESIAN_POINT('Ctrl Pts',(23.3268824670043,-16.0119118209665,16.8352914577688)) ;
#55657 = CARTESIAN_POINT('Ctrl Pts',(23.3931495450529,-16.0024299275614,16.83009862305)) ;
#55658 = CARTESIAN_POINT('Ctrl Pts',(23.4602019265677,-15.9925848997549,16.8269700901341)) ;
#55659 = CARTESIAN_POINT('Ctrl Pts',(23.5277412951986,-15.9824119250019,16.8260313296728)) ;
#55660 = CARTESIAN_POINT('Ctrl Pts',(23.5831978191147,-15.9740589032144,16.8252605141762)) ;
#55661 = CARTESIAN_POINT('Ctrl Pts',(23.6389822086216,-15.9654849570551,16.8259652402328)) ;
#55662 = CARTESIAN_POINT('Ctrl Pts',(23.6949230333843,-15.9567135267635,16.8281897192057)) ;
#55663 = CARTESIAN_POINT('Ctrl Pts',(23.7650042625084,-15.9457249040783,16.8309764893552)) ;
#55664 = CARTESIAN_POINT('Ctrl Pts',(23.835341382626,-15.9344245942998,16.8361500552922)) ;
#55665 = CARTESIAN_POINT('Ctrl Pts',(23.9056200291962,-15.9228603613537,16.8437518641509)) ;
#55666 = CARTESIAN_POINT('Ctrl Pts',(23.9297414390779,-15.9188912239773,16.8463609973126)) ;
#55667 = CARTESIAN_POINT('Ctrl Pts',(23.9538559278607,-15.914891049532,16.8492557394864)) ;
#55668 = CARTESIAN_POINT('Ctrl Pts',(23.9779507384798,-15.9108619285365,16.8524363584598)) ;
#55669 = CARTESIAN_POINT('',(24.5306755365459,-15.9108618883339,16.0372283765163)) ;
#55670 = CARTESIAN_POINT('Origin',(-2.92277791062251E-15,-15.9108618782028,
0.)) ;
#55671 = CARTESIAN_POINT('',(24.2452694789222,-16.1877442736409,13.6576957999734)) ;
#55672 = CARTESIAN_POINT('Ctrl Pts',(24.5306755198089,-15.9108619232992,16.0372283458231)) ;
#55673 = CARTESIAN_POINT('Ctrl Pts',(24.4960827033786,-15.9226009208764,15.9754431298308)) ;
#55674 = CARTESIAN_POINT('Ctrl Pts',(24.4636860016978,-15.9340937790044,15.912603161026)) ;
#55675 = CARTESIAN_POINT('Ctrl Pts',(24.4335801028943,-15.9452906595266,15.8490101065037)) ;
#55676 = CARTESIAN_POINT('Ctrl Pts',(24.4232469921228,-15.9491337139222,15.8271833515223)) ;
#55677 = CARTESIAN_POINT('Ctrl Pts',(24.4131833236117,-15.9529419517588,15.8052680335759)) ;
#55678 = CARTESIAN_POINT('Ctrl Pts',(24.4033915883005,-15.9567135267634,15.7832767754878)) ;
#55679 = CARTESIAN_POINT('Ctrl Pts',(24.3756947594617,-15.9673817754482,15.7210724682984)) ;
#55680 = CARTESIAN_POINT('Ctrl Pts',(24.3501734054637,-15.9777576912909,15.6582507682632)) ;
#55681 = CARTESIAN_POINT('Ctrl Pts',(24.3268632647421,-15.9877997661731,15.5951284765947)) ;
#55682 = CARTESIAN_POINT('Ctrl Pts',(24.303363205158,-15.997923658641,15.5314918974333)) ;
#55683 = CARTESIAN_POINT('Ctrl Pts',(24.2821105736219,-16.0077081692744,15.467550314488)) ;
#55684 = CARTESIAN_POINT('Ctrl Pts',(24.2630897205414,-16.0171189356805,15.4036344780031)) ;
#55685 = CARTESIAN_POINT('Ctrl Pts',(24.2475243072968,-16.0248200870136,15.3513299676034)) ;
#55686 = CARTESIAN_POINT('Ctrl Pts',(24.2334524388622,-16.0322710948774,15.2990429292134)) ;
#55687 = CARTESIAN_POINT('Ctrl Pts',(24.2208399697526,-16.0394576303854,15.2469540989219)) ;
#55688 = CARTESIAN_POINT('Ctrl Pts',(24.2054081618257,-16.0482506141109,15.1832215484423)) ;
#55689 = CARTESIAN_POINT('Ctrl Pts',(24.1917667485092,-16.0568730319549,15.1181511654454)) ;
#55690 = CARTESIAN_POINT('Ctrl Pts',(24.1801165809055,-16.0652608298864,15.0520066280625)) ;
#55691 = CARTESIAN_POINT('Ctrl Pts',(24.1685619107778,-16.0735798722808,14.9864042834267)) ;
#55692 = CARTESIAN_POINT('Ctrl Pts',(24.1589662350982,-16.0816680200508,14.9197457308275)) ;
#55693 = CARTESIAN_POINT('Ctrl Pts',(24.151481133861,-16.0894673869309,14.8523131459332)) ;
#55694 = CARTESIAN_POINT('Ctrl Pts',(24.1453305870469,-16.0958761674667,14.796903438429)) ;
#55695 = CARTESIAN_POINT('Ctrl Pts',(24.1406043425428,-16.1020900207685,14.7409716757236)) ;
#55696 = CARTESIAN_POINT('Ctrl Pts',(24.1373621395585,-16.108079933754,14.6846840610676)) ;
#55697 = CARTESIAN_POINT('Ctrl Pts',(24.1333027108827,-16.1155796568301,14.6142086595785)) ;
#55698 = CARTESIAN_POINT('Ctrl Pts',(24.1315703296063,-16.1227292229208,14.5431648072197)) ;
#55699 = CARTESIAN_POINT('Ctrl Pts',(24.132235202502,-16.1294814162037,14.4718618438038)) ;
#55700 = CARTESIAN_POINT('Ctrl Pts',(24.1328987608232,-16.1362202591734,14.4006998593048)) ;
#55701 = CARTESIAN_POINT('Ctrl Pts',(24.1359501730677,-16.1425632136358,14.3292802874376)) ;
#55702 = CARTESIAN_POINT('Ctrl Pts',(24.1414084815104,-16.148471764915,14.2579176350146)) ;
#55703 = CARTESIAN_POINT('Ctrl Pts',(24.1455248902993,-16.1529277264407,14.2040991576006)) ;
#55704 = CARTESIAN_POINT('Ctrl Pts',(24.1510091709447,-16.1571367885211,14.1503132485985)) ;
#55705 = CARTESIAN_POINT('Ctrl Pts',(24.1578501819171,-16.1610860188908,14.0966947999152)) ;
#55706 = CARTESIAN_POINT('Ctrl Pts',(24.167313904645,-16.1665493080681,14.0225200714308)) ;
#55707 = CARTESIAN_POINT('Ctrl Pts',(24.1793828412297,-16.171518536629,13.9486160186902)) ;
#55708 = CARTESIAN_POINT('Ctrl Pts',(24.1939861655753,-16.1759680067789,13.8753344831029)) ;
#55709 = CARTESIAN_POINT('Ctrl Pts',(24.2085894899129,-16.1804174769265,13.8020529475559)) ;
#55710 = CARTESIAN_POINT('Ctrl Pts',(24.2257270131076,-16.184347145014,13.7293945351644)) ;
#55711 = CARTESIAN_POINT('Ctrl Pts',(24.2452694789242,-16.1877442734701,13.6576957998574)) ;
#55712 = CARTESIAN_POINT('',(25.5444566593685,-15.9108618782029,14.367584437899)) ;
#55713 = CARTESIAN_POINT('Ctrl Pts',(25.5444566593687,-15.9108618782028,14.3675844378987)) ;
#55714 = CARTESIAN_POINT('Ctrl Pts',(24.8863882921944,-16.0510971577332,14.0081470766494)) ;
#55715 = CARTESIAN_POINT('Ctrl Pts',(24.2452694788798,-16.1877442737199,13.6576958001829)) ;
#55716 = CARTESIAN_POINT('',(26.2271102382866,-15.9108618782029,13.0799631938043)) ;
#55717 = CARTESIAN_POINT('Origin',(-2.92277791062251E-15,-15.9108618782028,
0.)) ;
#55718 = CARTESIAN_POINT('',(24.9104561816079,-16.1877442736409,12.403020579454)) ;
#55719 = CARTESIAN_POINT('Ctrl Pts',(24.9104561817576,-16.1877442737199,12.4030205793014)) ;
#55720 = CARTESIAN_POINT('Ctrl Pts',(25.5603084332828,-16.0510971576887,12.7369988443091)) ;
#55721 = CARTESIAN_POINT('Ctrl Pts',(26.2271102382865,-15.9108618782028,13.0799631938046)) ;
#55722 = CARTESIAN_POINT('',(27.040135303883,-15.9108618883339,11.303885129792)) ;
#55723 = CARTESIAN_POINT('Ctrl Pts',(24.9104561815129,-16.1877442734702,12.4030205795208)) ;
#55724 = CARTESIAN_POINT('Ctrl Pts',(24.9588334568668,-16.184347145014,12.3466090927103)) ;
#55725 = CARTESIAN_POINT('Ctrl Pts',(25.0093546690776,-16.1804174769265,12.2916495920824)) ;
#55726 = CARTESIAN_POINT('Ctrl Pts',(25.0618137930884,-16.1759680067789,12.2384379313129)) ;
#55727 = CARTESIAN_POINT('Ctrl Pts',(25.114272917128,-16.171518536629,12.185226270514)) ;
#55728 = CARTESIAN_POINT('Ctrl Pts',(25.1686695573966,-16.166549308068,12.1337629460074)) ;
#55729 = CARTESIAN_POINT('Ctrl Pts',(25.2247522453194,-16.1610860188908,12.0843040286217)) ;
#55730 = CARTESIAN_POINT('Ctrl Pts',(25.2784886472403,-16.155851292919,12.0369142839135)) ;
#55731 = CARTESIAN_POINT('Ctrl Pts',(25.3338073909395,-16.1501596984485,11.9913338865715)) ;
#55732 = CARTESIAN_POINT('Ctrl Pts',(25.3904592555537,-16.1440425621065,11.9477555600397)) ;
#55733 = CARTESIAN_POINT('Ctrl Pts',(25.447228161859,-16.1379127878753,11.9040872015014)) ;
#55734 = CARTESIAN_POINT('Ctrl Pts',(25.5053352796135,-16.1313557844548,11.862429483124)) ;
#55735 = CARTESIAN_POINT('Ctrl Pts',(25.5645019720945,-16.1244124680043,11.8229329020711)) ;
#55736 = CARTESIAN_POINT('Ctrl Pts',(25.6090850517435,-16.1191805644221,11.7931715761443)) ;
#55737 = CARTESIAN_POINT('Ctrl Pts',(25.6542691228957,-16.1137295207043,11.7646364345387)) ;
#55738 = CARTESIAN_POINT('Ctrl Pts',(25.6999268634434,-16.1080799337539,11.737374333437)) ;
#55739 = CARTESIAN_POINT('Ctrl Pts',(25.7587596834656,-16.1008000918637,11.7022454315618)) ;
#55740 = CARTESIAN_POINT('Ctrl Pts',(25.8183879655569,-16.0931892946345,11.6692271789562)) ;
#55741 = CARTESIAN_POINT('Ctrl Pts',(25.8785033682724,-16.0853002129681,11.6383938107501)) ;
#55742 = CARTESIAN_POINT('Ctrl Pts',(25.9391089750513,-16.0773468007024,11.6073090154273)) ;
#55743 = CARTESIAN_POINT('Ctrl Pts',(26.0002091860835,-16.0691106491234,11.578444983022)) ;
#55744 = CARTESIAN_POINT('Ctrl Pts',(26.0614775024479,-16.0606518030573,11.5518259353539)) ;
#55745 = CARTESIAN_POINT('Ctrl Pts',(26.1116523404216,-16.0537245483848,11.5300266354382)) ;
#55746 = CARTESIAN_POINT('Ctrl Pts',(26.1619396052601,-16.0466480826282,11.5097319605179)) ;
#55747 = CARTESIAN_POINT('Ctrl Pts',(26.2121582663181,-16.0394576303853,11.490929342594)) ;
#55748 = CARTESIAN_POINT('Ctrl Pts',(26.273580703628,-16.0306629892537,11.4679318632436)) ;
#55749 = CARTESIAN_POINT('Ctrl Pts',(26.3364762332058,-16.0214720150687,11.4465779157217)) ;
#55750 = CARTESIAN_POINT('Ctrl Pts',(26.400602933669,-16.0119118209662,11.4271015063442)) ;
#55751 = CARTESIAN_POINT('Ctrl Pts',(26.4642044182933,-16.0024299275611,11.4077846142756)) ;
#55752 = CARTESIAN_POINT('Ctrl Pts',(26.5290166102924,-15.9925848997544,11.3903149447492)) ;
#55753 = CARTESIAN_POINT('Ctrl Pts',(26.5947751402681,-15.9824119250013,11.3748791641796)) ;
#55754 = CARTESIAN_POINT('Ctrl Pts',(26.6487694189249,-15.974058903214,11.3622048565625)) ;
#55755 = CARTESIAN_POINT('Ctrl Pts',(26.7034010956744,-15.9654849570548,11.3509011117465)) ;
#55756 = CARTESIAN_POINT('Ctrl Pts',(26.7585122522638,-15.9567135267634,11.3410479599125)) ;
#55757 = CARTESIAN_POINT('Ctrl Pts',(26.827554094393,-15.9457249040797,11.3287041842507)) ;
#55758 = CARTESIAN_POINT('Ctrl Pts',(26.8973589354675,-15.9344245943026,11.3186363934173)) ;
#55759 = CARTESIAN_POINT('Ctrl Pts',(26.9676286705233,-15.922860361358,11.310952644619)) ;
#55760 = CARTESIAN_POINT('Ctrl Pts',(26.9917470322096,-15.9188912222604,11.3083153864527)) ;
#55761 = CARTESIAN_POINT('Ctrl Pts',(27.0159200321511,-15.914891046067,11.3059585479934)) ;
#55762 = CARTESIAN_POINT('Ctrl Pts',(27.040135269086,-15.9108619232992,11.3038851331635)) ;
#55763 = CARTESIAN_POINT('',(27.4046920069319,-15.9108618948274,10.3889167040556)) ;
#55764 = CARTESIAN_POINT('Origin',(-2.92277791062251E-15,-15.9108618782028,
0.)) ;
#55765 = CARTESIAN_POINT('',(26.6144294302344,-16.1877442736409,8.1263702089704)) ;
#55766 = CARTESIAN_POINT('Ctrl Pts',(27.4046919783062,-15.9108619275541,10.3889167248043)) ;
#55767 = CARTESIAN_POINT('Ctrl Pts',(27.3576259280778,-15.9226009250732,10.3360124454355)) ;
#55768 = CARTESIAN_POINT('Ctrl Pts',(27.3124779080023,-15.9340937831366,10.2816059730657)) ;
#55769 = CARTESIAN_POINT('Ctrl Pts',(27.2694052419543,-15.9452906635885,10.2259715668355)) ;
#55770 = CARTESIAN_POINT('Ctrl Pts',(27.254621611824,-15.9491337166056,10.2068764292532)) ;
#55771 = CARTESIAN_POINT('Ctrl Pts',(27.2400820859543,-15.9529419530876,10.1876368772434)) ;
#55772 = CARTESIAN_POINT('Ctrl Pts',(27.2257918105759,-15.9567135267635,10.168264703024)) ;
#55773 = CARTESIAN_POINT('Ctrl Pts',(27.1853704309042,-15.9673817754483,10.1134686974568)) ;
#55774 = CARTESIAN_POINT('Ctrl Pts',(27.1469409434687,-15.977757691291,10.0576020705611)) ;
#55775 = CARTESIAN_POINT('Ctrl Pts',(27.1106063540562,-15.9877997661732,10.0009665342062)) ;
#55776 = CARTESIAN_POINT('Ctrl Pts',(27.07397572937,-15.9979236586412,9.94386956105565)) ;
#55777 = CARTESIAN_POINT('Ctrl Pts',(27.0394744223152,-16.0077081692747,9.88599158434337)) ;
#55778 = CARTESIAN_POINT('Ctrl Pts',(27.0071582507039,-16.0171189356808,9.82765898575631)) ;
#55779 = CARTESIAN_POINT('Ctrl Pts',(26.9807128245458,-16.0248200870138,9.77992342948141)) ;
#55780 = CARTESIAN_POINT('Ctrl Pts',(26.9557297809157,-16.0322710948775,9.73188386874515)) ;
#55781 = CARTESIAN_POINT('Ctrl Pts',(26.9322146255475,-16.0394576303853,9.6837241543968)) ;
#55782 = CARTESIAN_POINT('Ctrl Pts',(26.9034429902816,-16.0482506141109,9.62479901807348)) ;
#55783 = CARTESIAN_POINT('Ctrl Pts',(26.8761322967502,-16.056873031955,9.56418244509614)) ;
#55784 = CARTESIAN_POINT('Ctrl Pts',(26.850535383272,-16.0652608298866,9.50208877189789)) ;
#55785 = CARTESIAN_POINT('Ctrl Pts',(26.8251482900055,-16.073579872281,9.44050408614717)) ;
#55786 = CARTESIAN_POINT('Ctrl Pts',(26.8014473374946,-16.0816680200511,9.3774667600895)) ;
#55787 = CARTESIAN_POINT('Ctrl Pts',(26.7796412213054,-16.0894673869313,9.31321978706453)) ;
#55788 = CARTESIAN_POINT('Ctrl Pts',(26.761723021644,-16.0958761674669,9.26042771348703)) ;
#55789 = CARTESIAN_POINT('Ctrl Pts',(26.7450835984599,-16.1020900207685,9.20681960717438)) ;
#55790 = CARTESIAN_POINT('Ctrl Pts',(26.7298170230788,-16.1080799337539,9.1525449434731)) ;
#55791 = CARTESIAN_POINT('Ctrl Pts',(26.7107023735074,-16.1155796568301,9.08458987487628)) ;
#55792 = CARTESIAN_POINT('Ctrl Pts',(26.6937381661266,-16.1227292229208,9.01557939907129)) ;
#55793 = CARTESIAN_POINT('Ctrl Pts',(26.6790594652296,-16.1294814162037,8.94580053129722)) ;
#55794 = CARTESIAN_POINT('Ctrl Pts',(26.664409786792,-16.1362202591734,8.87615962902581)) ;
#55795 = CARTESIAN_POINT('Ctrl Pts',(26.6520367619099,-16.1425632136359,8.80575384362681)) ;
#55796 = CARTESIAN_POINT('Ctrl Pts',(26.6420265973284,-16.1484717649151,8.73488623539158)) ;
#55797 = CARTESIAN_POINT('Ctrl Pts',(26.6344773849863,-16.1529277264407,8.68144109786278)) ;
#55798 = CARTESIAN_POINT('Ctrl Pts',(26.6282710656625,-16.1571367885211,8.62773371529949)) ;
#55799 = CARTESIAN_POINT('Ctrl Pts',(26.6234257560832,-16.1610860188908,8.57389822101004)) ;
#55800 = CARTESIAN_POINT('Ctrl Pts',(26.6167228481979,-16.166549308068,8.49942323581703)) ;
#55801 = CARTESIAN_POINT('Ctrl Pts',(26.6126224330011,-16.171518536629,8.42465255414971)) ;
#55802 = CARTESIAN_POINT('Ctrl Pts',(26.6111309757742,-16.1759680067789,8.34994501707801)) ;
#55803 = CARTESIAN_POINT('Ctrl Pts',(26.6096395185481,-16.1804174769265,8.2752374800475)) ;
#55804 = CARTESIAN_POINT('Ctrl Pts',(26.6107569650772,-16.184347145014,8.2005937200553)) ;
#55805 = CARTESIAN_POINT('Ctrl Pts',(26.6144294302114,-16.1877442734701,8.12637020885662)) ;
#55806 = CARTESIAN_POINT('',(28.0358474093688,-15.9108618782029,8.54037520493671)) ;
#55807 = CARTESIAN_POINT('Ctrl Pts',(28.0358474093689,-15.9108618782028,8.54037520493676)) ;
#55808 = CARTESIAN_POINT('Ctrl Pts',(27.3158959072615,-16.0510971577111,8.33080653606366)) ;
#55809 = CARTESIAN_POINT('Ctrl Pts',(26.614429430238,-16.1877442737199,8.12637020918415)) ;
#55810 = CARTESIAN_POINT('',(28.4257404213013,-15.9108618782029,7.1361074896129)) ;
#55811 = CARTESIAN_POINT('Origin',(-2.92277791062251E-15,-15.9108618782028,
0.)) ;
#55812 = CARTESIAN_POINT('',(26.9943463529853,-16.1877442736409,6.75803311957223)) ;
#55813 = CARTESIAN_POINT('Ctrl Pts',(26.9943463530987,-16.1877442737199,6.75803311939104)) ;
#55814 = CARTESIAN_POINT('Ctrl Pts',(27.7008008740359,-16.0510971578292,6.9445041333834)) ;
#55815 = CARTESIAN_POINT('Ctrl Pts',(28.4257404213014,-15.9108618782028,7.13610748961287)) ;
#55816 = CARTESIAN_POINT('',(28.8379530854688,-15.9108618948274,5.22677683844473)) ;
#55817 = CARTESIAN_POINT('Ctrl Pts',(26.994346352907,-16.1877442734701,6.75803311965786)) ;
#55818 = CARTESIAN_POINT('Ctrl Pts',(27.0294657922942,-16.184347145014,6.69254081788165)) ;
#55819 = CARTESIAN_POINT('Ctrl Pts',(27.0669911785949,-16.1804174769264,6.62800567260791)) ;
#55820 = CARTESIAN_POINT('Ctrl Pts',(27.1067849032983,-16.1759680067789,6.56476090991527)) ;
#55821 = CARTESIAN_POINT('Ctrl Pts',(27.1465786280237,-16.171518536629,6.50151614718779)) ;
#55822 = CARTESIAN_POINT('Ctrl Pts',(27.1886404115476,-16.166549308068,6.43956233690494)) ;
#55823 = CARTESIAN_POINT('Ctrl Pts',(27.2327797121498,-16.1610860188908,6.37920362141187)) ;
#55824 = CARTESIAN_POINT('Ctrl Pts',(27.275072392574,-16.155851292919,6.32137008462396)) ;
#55825 = CARTESIAN_POINT('Ctrl Pts',(27.3192993767049,-16.1501596984486,6.26496343695771)) ;
#55826 = CARTESIAN_POINT('Ctrl Pts',(27.365258700168,-16.1440425621066,6.21022547120853)) ;
#55827 = CARTESIAN_POINT('Ctrl Pts',(27.4113129747325,-16.1379127878754,6.15537441784739)) ;
#55828 = CARTESIAN_POINT('Ctrl Pts',(27.4591064023066,-16.1313557844549,6.10219932109308)) ;
#55829 = CARTESIAN_POINT('Ctrl Pts',(27.508399212981,-16.1244124680045,6.05090705822831)) ;
#55830 = CARTESIAN_POINT('Ctrl Pts',(27.5455421596677,-16.1191805644222,6.0122574913044)) ;
#55831 = CARTESIAN_POINT('Ctrl Pts',(27.5835356403936,-16.1137295207044,5.97467624578577)) ;
#55832 = CARTESIAN_POINT('Ctrl Pts',(27.6222653824652,-16.108079933754,5.93823645287308)) ;
#55833 = CARTESIAN_POINT('Ctrl Pts',(27.6721710483487,-16.1008000918638,5.89128152798355)) ;
#55834 = CARTESIAN_POINT('Ctrl Pts',(27.7233073060428,-16.0931892946346,5.84621690572527)) ;
#55835 = CARTESIAN_POINT('Ctrl Pts',(27.7753889813127,-16.0853002129683,5.80318136994858)) ;
#55836 = CARTESIAN_POINT('Ctrl Pts',(27.8278953505494,-16.0773468007026,5.75979490589796)) ;
#55837 = CARTESIAN_POINT('Ctrl Pts',(27.881362158849,-16.0691106491237,5.71847095926792)) ;
#55838 = CARTESIAN_POINT('Ctrl Pts',(27.9354757476287,-16.0606518030576,5.67930337320214)) ;
#55839 = CARTESIAN_POINT('Ctrl Pts',(27.9797913206747,-16.053724548385,5.64722762179708)) ;
#55840 = CARTESIAN_POINT('Ctrl Pts',(28.0245401420056,-16.0466480826283,5.61659714963857)) ;
#55841 = CARTESIAN_POINT('Ctrl Pts',(28.0695427116236,-16.0394576303853,5.58743859879812)) ;
#55842 = CARTESIAN_POINT('Ctrl Pts',(28.1245853482227,-16.0306629892537,5.55177477934753)) ;
#55843 = CARTESIAN_POINT('Ctrl Pts',(28.1814199477719,-16.0214720150686,5.51739939557131)) ;
#55844 = CARTESIAN_POINT('Ctrl Pts',(28.2398605493166,-16.0119118209661,5.48459298879387)) ;
#55845 = CARTESIAN_POINT('Ctrl Pts',(28.297822505783,-16.0024299275609,5.45205527577939)) ;
#55846 = CARTESIAN_POINT('Ctrl Pts',(28.3573639622018,-15.9925848997542,5.42106133197323)) ;
#55847 = CARTESIAN_POINT('Ctrl Pts',(28.4182668577455,-15.9824119250011,5.39185029123897)) ;
#55848 = CARTESIAN_POINT('Ctrl Pts',(28.4682741786843,-15.9740589032138,5.36786512803923)) ;
#55849 = CARTESIAN_POINT('Ctrl Pts',(28.5191986261912,-15.9654849570548,5.34508146289537)) ;
#55850 = CARTESIAN_POINT('Ctrl Pts',(28.5709031781777,-15.9567135267634,5.32361140268334)) ;
#55851 = CARTESIAN_POINT('Ctrl Pts',(28.6356773135241,-15.9457249040785,5.29671426243865)) ;
#55852 = CARTESIAN_POINT('Ctrl Pts',(28.7016858787851,-15.9344245943003,5.27187587354305)) ;
#55853 = CARTESIAN_POINT('Ctrl Pts',(28.7686609676306,-15.9228603613544,5.24926585064139)) ;
#55854 = CARTESIAN_POINT('Ctrl Pts',(28.7916485147756,-15.9188912236552,5.24150551801081)) ;
#55855 = CARTESIAN_POINT('Ctrl Pts',(28.8147497046315,-15.914891048882,5.23400730323592)) ;
#55856 = CARTESIAN_POINT('Ctrl Pts',(28.8379530716378,-15.9108619275541,5.22677680590791)) ;
#55857 = CARTESIAN_POINT('',(28.9972957403971,-15.9108618818335,4.25483109005223)) ;
#55858 = CARTESIAN_POINT('Origin',(-2.92277791062251E-15,-15.9108618782028,
0.)) ;
#55859 = CARTESIAN_POINT('',(27.7391282412025,-16.1877442736409,2.21506457880764)) ;
#55860 = CARTESIAN_POINT('Ctrl Pts',(28.9972957168721,-15.9108618853164,4.25483107607865)) ;
#55861 = CARTESIAN_POINT('Ctrl Pts',(28.9399571848693,-15.9226008834119,4.21328148344468)) ;
#55862 = CARTESIAN_POINT('Ctrl Pts',(28.8841689131692,-15.9340937421155,4.16985249820661)) ;
#55863 = CARTESIAN_POINT('Ctrl Pts',(28.8301435051533,-15.9452906232646,4.12477814745126)) ;
#55864 = CARTESIAN_POINT('Ctrl Pts',(28.8116005516433,-15.9491336899665,4.10930743429519)) ;
#55865 = CARTESIAN_POINT('Ctrl Pts',(28.793264951962,-15.9529419398963,4.0936432064508)) ;
#55866 = CARTESIAN_POINT('Ctrl Pts',(28.775144267083,-15.9567135267634,4.0777958742614)) ;
#55867 = CARTESIAN_POINT('Ctrl Pts',(28.7238883953676,-15.9673817754481,4.03297037063621)) ;
#55868 = CARTESIAN_POINT('Ctrl Pts',(28.6743476946165,-15.9777576912908,3.98667107826351)) ;
#55869 = CARTESIAN_POINT('Ctrl Pts',(28.6266876215316,-15.9877997661729,3.93917051195709)) ;
#55870 = CARTESIAN_POINT('Ctrl Pts',(28.5786392390422,-15.9979236586407,3.89128293582399)) ;
#55871 = CARTESIAN_POINT('Ctrl Pts',(28.5325024992417,-16.0077081692741,3.84217487520988)) ;
#55872 = CARTESIAN_POINT('Ctrl Pts',(28.4884020773677,-16.0171189356801,3.79215308199961)) ;
#55873 = CARTESIAN_POINT('Ctrl Pts',(28.4523131970299,-16.0248200870134,3.75121854140485)) ;
#55874 = CARTESIAN_POINT('Ctrl Pts',(28.4175871575564,-16.0322710948773,3.70967273478831)) ;
#55875 = CARTESIAN_POINT('Ctrl Pts',(28.3842688584582,-16.0394576303854,3.6676940310985)) ;
#55876 = CARTESIAN_POINT('Ctrl Pts',(28.3435027255416,-16.0482506141109,3.61633158281616)) ;
#55877 = CARTESIAN_POINT('Ctrl Pts',(28.3037997694713,-16.0568730319549,3.56300318344106)) ;
#55878 = CARTESIAN_POINT('Ctrl Pts',(28.2654529933442,-16.0652608298864,3.50786380557492)) ;
#55879 = CARTESIAN_POINT('Ctrl Pts',(28.2274205492046,-16.0735798722808,3.45317641016946)) ;
#55880 = CARTESIAN_POINT('Ctrl Pts',(28.1907225500605,-16.0816680200508,3.39670786595972)) ;
#55881 = CARTESIAN_POINT('Ctrl Pts',(28.1556150486768,-16.0894673869309,3.33865062185837)) ;
#55882 = CARTESIAN_POINT('Ctrl Pts',(28.126767031269,-16.0958761674667,3.2909446808922)) ;
#55883 = CARTESIAN_POINT('Ctrl Pts',(28.0989924703388,-16.1020900207684,3.24216688644051)) ;
#55884 = CARTESIAN_POINT('Ctrl Pts',(28.0724153706577,-16.1080799337539,3.19244299664488)) ;
#55885 = CARTESIAN_POINT('Ctrl Pts',(28.0391392799602,-16.1155796568301,3.13018576442147)) ;
#55886 = CARTESIAN_POINT('Ctrl Pts',(28.0077364739579,-16.1227292229208,3.06643551831957)) ;
#55887 = CARTESIAN_POINT('Ctrl Pts',(27.9784005590081,-16.1294814162037,3.00144352849088)) ;
#55888 = CARTESIAN_POINT('Ctrl Pts',(27.9491226464934,-16.1362202591733,2.93658003963727)) ;
#55889 = CARTESIAN_POINT('Ctrl Pts',(27.9219037333767,-16.1425632136358,2.87048013698147)) ;
#55890 = CARTESIAN_POINT('Ctrl Pts',(27.8968931599413,-16.148471764915,2.80342126353177)) ;
#55891 = CARTESIAN_POINT('Ctrl Pts',(27.8780313192468,-16.1529277264407,2.75284850111858)) ;
#55892 = CARTESIAN_POINT('Ctrl Pts',(27.8604246005476,-16.1571367885212,2.70173094251072)) ;
#55893 = CARTESIAN_POINT('Ctrl Pts',(27.8441195317072,-16.1610860188909,2.65019569049381)) ;
#55894 = CARTESIAN_POINT('Ctrl Pts',(27.8215634137318,-16.1665493080681,2.57890281612689)) ;
#55895 = CARTESIAN_POINT('Ctrl Pts',(27.8014853776107,-16.171518536629,2.50676169950606)) ;
#55896 = CARTESIAN_POINT('Ctrl Pts',(27.7839688776935,-16.1759680067789,2.43412140235199)) ;
#55897 = CARTESIAN_POINT('Ctrl Pts',(27.766452377786,-16.1804174769265,2.36148110523793)) ;
#55898 = CARTESIAN_POINT('Ctrl Pts',(27.7514974970917,-16.184347145014,2.28834225690174)) ;
#55899 = CARTESIAN_POINT('Ctrl Pts',(27.7391282411555,-16.1877442734701,2.21506457870152)) ;
#55900 = CARTESIAN_POINT('',(29.2163130941136,-15.9108618782029,2.31382751933678)) ;
#55901 = CARTESIAN_POINT('Ctrl Pts',(29.2163130941136,-15.9108618782028,2.31382751933756)) ;
#55902 = CARTESIAN_POINT('Ctrl Pts',(28.4681425925364,-16.0510971570555,2.26392674105533)) ;
#55903 = CARTESIAN_POINT('Ctrl Pts',(27.7391282412521,-16.1877442737199,2.21506457901549)) ;
#55904 = CARTESIAN_POINT('',(29.2952145751572,-15.9108618782029,0.858575330421187)) ;
#55905 = CARTESIAN_POINT('Origin',(-2.92277791062251E-15,-15.9108618782028,
0.)) ;
#55906 = CARTESIAN_POINT('',(27.8160108909581,-16.1877442736409,0.79704754203402)) ;
#55907 = CARTESIAN_POINT('Ctrl Pts',(27.8160108910298,-16.1877442737199,0.797047541832666)) ;
#55908 = CARTESIAN_POINT('Ctrl Pts',(28.546034658842,-16.0510971568885,0.827292127995152)) ;
#55909 = CARTESIAN_POINT('Ctrl Pts',(29.2952145751573,-15.9108618782028,0.85857533042041)) ;
#55910 = CARTESIAN_POINT('',(29.2873405113753,-15.9108618818335,-1.09472993550084)) ;
#55911 = CARTESIAN_POINT('Ctrl Pts',(27.8160108909,-16.1877442734702,0.797047542134493)) ;
#55912 = CARTESIAN_POINT('Ctrl Pts',(27.8362303483673,-16.184347145014,0.725536772633904)) ;
#55913 = CARTESIAN_POINT('Ctrl Pts',(27.859005263401,-16.1804174769265,0.654443574381639)) ;
#55914 = CARTESIAN_POINT('Ctrl Pts',(27.8842728784575,-16.1759680067789,0.584122964577792)) ;
#55915 = CARTESIAN_POINT('Ctrl Pts',(27.909540493528,-16.171518536629,0.513802354735197)) ;
#55916 = CARTESIAN_POINT('Ctrl Pts',(27.9373006580581,-16.1665493080681,0.444254949988175)) ;
#55917 = CARTESIAN_POINT('Ctrl Pts',(27.9674326667007,-16.1610860188908,0.375818742840304)) ;
#55918 = CARTESIAN_POINT('Ctrl Pts',(27.996304066897,-16.155851292919,0.310245645875013)) ;
#55919 = CARTESIAN_POINT('Ctrl Pts',(28.0273712868368,-16.1501596984485,0.245650260037327)) ;
#55920 = CARTESIAN_POINT('Ctrl Pts',(28.0604890622642,-16.1440425621065,0.182312141511965)) ;
#55921 = CARTESIAN_POINT('Ctrl Pts',(28.0936752583953,-16.1379127878753,0.118843167620128)) ;
#55922 = CARTESIAN_POINT('Ctrl Pts',(28.1289202282347,-16.1313557844548,0.056637100912983)) ;
#55923 = CARTESIAN_POINT('Ctrl Pts',(28.1660342800607,-16.1244124680043,-0.00405247455977011)) ;
#55924 = CARTESIAN_POINT('Ctrl Pts',(28.1940003308787,-16.1191805644221,-0.0497830716863816)) ;
#55925 = CARTESIAN_POINT('Ctrl Pts',(28.2230266882454,-16.1137295207043,-0.0946531638453065)) ;
#55926 = CARTESIAN_POINT('Ctrl Pts',(28.2530174721459,-16.1080799337539,-0.138566764351555)) ;
#55927 = CARTESIAN_POINT('Ctrl Pts',(28.2916624504208,-16.1008000918637,-0.195152152154858)) ;
#55928 = CARTESIAN_POINT('Ctrl Pts',(28.3319156091424,-16.0931892946345,-0.250155972415166)) ;
#55929 = CARTESIAN_POINT('Ctrl Pts',(28.3735282757164,-16.0853002129681,-0.30338138194066)) ;
#55930 = CARTESIAN_POINT('Ctrl Pts',(28.4154802679428,-16.0773468007024,-0.357040811881018)) ;
#55931 = CARTESIAN_POINT('Ctrl Pts',(28.4588136249783,-16.0691106491234,-0.40889241092005)) ;
#55932 = CARTESIAN_POINT('Ctrl Pts',(28.5032421949055,-16.0606518030573,-0.458777102591018)) ;
#55933 = CARTESIAN_POINT('Ctrl Pts',(28.5396263560801,-16.0537245483848,-0.499629478998345)) ;
#55934 = CARTESIAN_POINT('Ctrl Pts',(28.5767443287514,-16.0466480826283,-0.539163501559296)) ;
#55935 = CARTESIAN_POINT('Ctrl Pts',(28.6144265367895,-16.0394576303854,-0.577314563885697)) ;
#55936 = CARTESIAN_POINT('Ctrl Pts',(28.6605156401652,-16.0306629892538,-0.623977122875787)) ;
#55937 = CARTESIAN_POINT('Ctrl Pts',(28.7086317869771,-16.0214720150689,-0.669766588165793)) ;
#55938 = CARTESIAN_POINT('Ctrl Pts',(28.7586536720263,-16.0119118209665,-0.714369001223339)) ;
#55939 = CARTESIAN_POINT('Ctrl Pts',(28.8082658636697,-16.0024299275614,-0.758606107885602)) ;
#55940 = CARTESIAN_POINT('Ctrl Pts',(28.8597524921807,-15.9925848997548,-0.801675083605944)) ;
#55941 = CARTESIAN_POINT('Ctrl Pts',(28.9129520015845,-15.9824119250019,-0.843295508705367)) ;
#55942 = CARTESIAN_POINT('Ctrl Pts',(28.9566340780589,-15.9740589032144,-0.877470007915371)) ;
#55943 = CARTESIAN_POINT('Ctrl Pts',(29.0014701257582,-15.965484957055,-0.910668254528474)) ;
#55944 = CARTESIAN_POINT('Ctrl Pts',(29.0473504257582,-15.9567135267634,-0.942751306966303)) ;
#55945 = CARTESIAN_POINT('Ctrl Pts',(29.1048280876747,-15.9457249040904,-0.98294413136516)) ;
#55946 = CARTESIAN_POINT('Ctrl Pts',(29.1639538899006,-15.9344245943248,-1.02139170282338)) ;
#55947 = CARTESIAN_POINT('Ctrl Pts',(29.2245026517423,-15.922860361392,-1.05787078025111)) ;
#55948 = CARTESIAN_POINT('Ctrl Pts',(29.245284593372,-15.9188912098109,-1.07039136753889)) ;
#55949 = CARTESIAN_POINT('Ctrl Pts',(29.2662338695707,-15.9148910209385,-1.08268039334433)) ;
#55950 = CARTESIAN_POINT('Ctrl Pts',(29.2873404864774,-15.9108618853164,-1.09472992415267)) ;
#55951 = CARTESIAN_POINT('',(29.2340179925284,-15.9108618818335,-2.07820592662307)) ;
#55952 = CARTESIAN_POINT('Origin',(-2.92277791062251E-15,-15.9108618782028,
0.)) ;
#55953 = CARTESIAN_POINT('',(27.5667762454386,-16.1877442736409,-3.7998150091926)) ;
#55954 = CARTESIAN_POINT('Ctrl Pts',(29.2340179665494,-15.9108618853164,-2.0782059352128)) ;
#55955 = CARTESIAN_POINT('Ctrl Pts',(29.1690880433416,-15.922600883412,-2.10645803199504)) ;
#55956 = CARTESIAN_POINT('Ctrl Pts',(29.1052681223567,-15.9340937421157,-2.1368788423665)) ;
#55957 = CARTESIAN_POINT('Ctrl Pts',(29.0428161453331,-15.9452906232649,-2.16928551410604)) ;
#55958 = CARTESIAN_POINT('Ctrl Pts',(29.0213809697546,-15.9491336899667,-2.18040834370659)) ;
#55959 = CARTESIAN_POINT('Ctrl Pts',(29.0001067002499,-15.9529419398964,-2.19176473867345)) ;
#55960 = CARTESIAN_POINT('Ctrl Pts',(28.9790029589372,-15.9567135267634,-2.20334615743714)) ;
#55961 = CARTESIAN_POINT('Ctrl Pts',(28.9193092627717,-15.9673817754482,-2.23610516839168)) ;
#55962 = CARTESIAN_POINT('Ctrl Pts',(28.8609738168107,-15.9777576912909,-2.27067222278905)) ;
#55963 = CARTESIAN_POINT('Ctrl Pts',(28.8042167921,-15.987799766173,-2.30681674536044)) ;
#55964 = CARTESIAN_POINT('Ctrl Pts',(28.7469973407702,-15.9979236586409,-2.34325575464003)) ;
#55965 = CARTESIAN_POINT('Ctrl Pts',(28.6913824708994,-16.0077081692743,-2.38129766082209)) ;
#55966 = CARTESIAN_POINT('Ctrl Pts',(28.6375598854752,-16.0171189356803,-2.42066968520106)) ;
#55967 = CARTESIAN_POINT('Ctrl Pts',(28.5935150268936,-16.0248200870135,-2.45288915649125)) ;
#55968 = CARTESIAN_POINT('Ctrl Pts',(28.5506697425885,-16.0322710948774,-2.48599857324384)) ;
#55969 = CARTESIAN_POINT('Ctrl Pts',(28.5091062263966,-16.0394576303854,-2.51983338874485)) ;
#55970 = CARTESIAN_POINT('Ctrl Pts',(28.4582517748961,-16.0482506141108,-2.56123149798998)) ;
#55971 = CARTESIAN_POINT('Ctrl Pts',(28.4080130223862,-16.0568730319548,-2.60477814707854)) ;
#55972 = CARTESIAN_POINT('Ctrl Pts',(28.3587094362426,-16.0652608298863,-2.65038497358669)) ;
#55973 = CARTESIAN_POINT('Ctrl Pts',(28.3098099960476,-16.0735798722807,-2.695617956819)) ;
#55974 = CARTESIAN_POINT('Ctrl Pts',(28.261830907923,-16.0816680200507,-2.74287731281456)) ;
#55975 = CARTESIAN_POINT('Ctrl Pts',(28.21506360909,-16.0894673869309,-2.79203013578472)) ;
#55976 = CARTESIAN_POINT('Ctrl Pts',(28.1766346751679,-16.0958761674667,-2.83241926736048)) ;
#55977 = CARTESIAN_POINT('Ctrl Pts',(28.1390236840916,-16.1020900207684,-2.87408595449453)) ;
#55978 = CARTESIAN_POINT('Ctrl Pts',(28.1023787757534,-16.1080799337539,-2.91693403656095)) ;
#55979 = CARTESIAN_POINT('Ctrl Pts',(28.0564971969472,-16.1155796568301,-2.97058235342623)) ;
#55980 = CARTESIAN_POINT('Ctrl Pts',(28.0121241526303,-16.1227292229208,-3.02609147917076)) ;
#55981 = CARTESIAN_POINT('Ctrl Pts',(27.969502738406,-16.1294814162037,-3.0832576378432)) ;
#55982 = CARTESIAN_POINT('Ctrl Pts',(27.9269655944633,-16.1362202591734,-3.14031076863114)) ;
#55983 = CARTESIAN_POINT('Ctrl Pts',(27.8861735192375,-16.1425632136359,-3.19901403056068)) ;
#55984 = CARTESIAN_POINT('Ctrl Pts',(27.8473320035648,-16.1484717649151,-3.2591285708333)) ;
#55985 = CARTESIAN_POINT('Ctrl Pts',(27.8180394932255,-16.1529277264407,-3.30446423196756)) ;
#55986 = CARTESIAN_POINT('Ctrl Pts',(27.789855645749,-16.1571367885212,-3.35060176639201)) ;
#55987 = CARTESIAN_POINT('Ctrl Pts',(27.7628532245448,-16.1610860188908,-3.39742704502891)) ;
#55988 = CARTESIAN_POINT('Ctrl Pts',(27.7254985954864,-16.1665493080681,-3.46220423300072)) ;
#55989 = CARTESIAN_POINT('Ctrl Pts',(27.690381765095,-16.171518536629,-3.52834254614104)) ;
#55990 = CARTESIAN_POINT('Ctrl Pts',(27.6576592745555,-16.175968006779,-3.59551902381645)) ;
#55991 = CARTESIAN_POINT('Ctrl Pts',(27.624936784034,-16.1804174769265,-3.66269550145486)) ;
#55992 = CARTESIAN_POINT('Ctrl Pts',(27.5946088497164,-16.184347145014,-3.73090954687479)) ;
#55993 = CARTESIAN_POINT('Ctrl Pts',(27.56677624537,-16.1877442734702,-3.79981500928618)) ;
#55994 = CARTESIAN_POINT('',(29.0306564501773,-15.9108618782029,-4.02091216943267)) ;
#55995 = CARTESIAN_POINT('Ctrl Pts',(29.0306564501773,-15.9108618782028,-4.02091216943256)) ;
#55996 = CARTESIAN_POINT('Ctrl Pts',(28.2892505645617,-16.0510971574954,-3.90881175282058)) ;
#55997 = CARTESIAN_POINT('Ctrl Pts',(27.5667762455317,-16.1877442737199,-3.79981500900026)) ;
#55998 = CARTESIAN_POINT('',(28.7948770547713,-15.9108618782029,-5.459102856983)) ;
#55999 = CARTESIAN_POINT('Origin',(-2.92277791062251E-15,-15.9108618782028,
0.)) ;
#56000 = CARTESIAN_POINT('',(27.3370296749455,-16.187744273641,-5.20120709271523)) ;
#56001 = CARTESIAN_POINT('Ctrl Pts',(27.3370296749724,-16.1877442737199,-5.20120709292722)) ;
#56002 = CARTESIAN_POINT('Ctrl Pts',(28.0564875803008,-16.0510971577385,-5.32860313832098)) ;
#56003 = CARTESIAN_POINT('Ctrl Pts',(28.7948770547713,-15.9108618782028,-5.45910285698312)) ;
#56004 = CARTESIAN_POINT('',(28.3672841893431,-15.9108618818335,-7.36504824030179)) ;
#56005 = CARTESIAN_POINT('Ctrl Pts',(27.3370296749104,-16.1877442734702,-5.20120709260465)) ;
#56006 = CARTESIAN_POINT('Ctrl Pts',(27.3414037110988,-16.184347145014,-5.27539256572612)) ;
#56007 = CARTESIAN_POINT('Ctrl Pts',(27.348363225151,-16.1804174769265,-5.34971957802101)) ;
#56008 = CARTESIAN_POINT('Ctrl Pts',(27.3579232449636,-16.1759680067789,-5.42382792137733)) ;
#56009 = CARTESIAN_POINT('Ctrl Pts',(27.3674832647814,-16.171518536629,-5.49793626477445)) ;
#56010 = CARTESIAN_POINT('Ctrl Pts',(27.3796437758774,-16.1665493080681,-5.57182530463607)) ;
#56011 = CARTESIAN_POINT('Ctrl Pts',(27.3943595533256,-16.1610860188908,-5.64513900245385)) ;
#56012 = CARTESIAN_POINT('Ctrl Pts',(27.4084596787088,-16.155851292919,-5.71538553446148)) ;
#56013 = CARTESIAN_POINT('Ctrl Pts',(27.4249144657817,-16.1501596984485,-5.78514925002124)) ;
#56014 = CARTESIAN_POINT('Ctrl Pts',(27.443642142802,-16.1440425621065,-5.85412590129558)) ;
#56015 = CARTESIAN_POINT('Ctrl Pts',(27.4624085108522,-16.1379127878753,-5.92324505703946)) ;
#56016 = CARTESIAN_POINT('Ctrl Pts',(27.4834570073389,-16.1313557844548,-5.99157340715721)) ;
#56017 = CARTESIAN_POINT('Ctrl Pts',(27.5066568885023,-16.1244124680043,-6.05882251814029)) ;
#56018 = CARTESIAN_POINT('Ctrl Pts',(27.5241383819977,-16.1191805644221,-6.1094958335742)) ;
#56019 = CARTESIAN_POINT('Ctrl Pts',(27.5428403757957,-16.1137295207043,-6.15955669673402)) ;
#56020 = CARTESIAN_POINT('Ctrl Pts',(27.5626898658027,-16.1080799337539,-6.20889075368092)) ;
#56021 = CARTESIAN_POINT('Ctrl Pts',(27.5882671602353,-16.1008000918637,-6.2724607345541)) ;
#56022 = CARTESIAN_POINT('Ctrl Pts',(27.6157550270204,-16.0931892946346,-6.33483183531309)) ;
#56023 = CARTESIAN_POINT('Ctrl Pts',(27.6449529228583,-16.0853002129682,-6.39575835759351)) ;
#56024 = CARTESIAN_POINT('Ctrl Pts',(27.6743889095439,-16.0773468007024,-6.4571816981176)) ;
#56025 = CARTESIAN_POINT('Ctrl Pts',(27.7055625957016,-16.0691106491234,-6.51713642642337)) ;
#56026 = CARTESIAN_POINT('Ctrl Pts',(27.738228716225,-16.0606518030573,-6.57540567095972)) ;
#56027 = CARTESIAN_POINT('Ctrl Pts',(27.7649801825905,-16.0537245483848,-6.62312446065317)) ;
#56028 = CARTESIAN_POINT('Ctrl Pts',(27.7927317114543,-16.0466480826283,-6.66971346666096)) ;
#56029 = CARTESIAN_POINT('Ctrl Pts',(27.8213315797461,-16.0394576303854,-6.71507313920121)) ;
#56030 = CARTESIAN_POINT('Ctrl Pts',(27.8563120746498,-16.0306629892537,-6.77055254833493)) ;
#56031 = CARTESIAN_POINT('Ctrl Pts',(27.8934599111776,-16.0214720150688,-6.82561503063382)) ;
#56032 = CARTESIAN_POINT('Ctrl Pts',(27.9327241119829,-16.0119118209663,-6.87992789070965)) ;
#56033 = CARTESIAN_POINT('Ctrl Pts',(27.9716667278631,-16.0024299275612,-6.9337959130789)) ;
#56034 = CARTESIAN_POINT('Ctrl Pts',(28.0126910709413,-15.9925848997546,-6.98692606327699)) ;
#56035 = CARTESIAN_POINT('Ctrl Pts',(28.0556996442737,-15.9824119250015,-7.03900974792234)) ;
#56036 = CARTESIAN_POINT('Ctrl Pts',(28.0910139509351,-15.9740589032141,-7.08177562154035)) ;
#56037 = CARTESIAN_POINT('Ctrl Pts',(28.1276651150658,-15.9654849570549,-7.12383613650684)) ;
#56038 = CARTESIAN_POINT('Ctrl Pts',(28.1655758512416,-15.9567135267634,-7.16503201329497)) ;
#56039 = CARTESIAN_POINT('Ctrl Pts',(28.2130694482099,-15.9457249040902,-7.21664115008039)) ;
#56040 = CARTESIAN_POINT('Ctrl Pts',(28.262547830676,-15.9344245943244,-7.26690013841677)) ;
#56041 = CARTESIAN_POINT('Ctrl Pts',(28.3138390727814,-15.9228603613914,-7.31554254927431)) ;
#56042 = CARTESIAN_POINT('Ctrl Pts',(28.3314435880026,-15.9188912098104,-7.33223791532878)) ;
#56043 = CARTESIAN_POINT('Ctrl Pts',(28.3492613044774,-15.9148910209383,-7.3487431056656)) ;
#56044 = CARTESIAN_POINT('Ctrl Pts',(28.3672841674668,-15.9108618853164,-7.36504822386662)) ;
#56045 = CARTESIAN_POINT('',(28.1037900289265,-15.9108618823941,-8.31406834816463)) ;
#56046 = CARTESIAN_POINT('Origin',(-2.92277791062251E-15,-15.9108618782028,
0.)) ;
#56047 = CARTESIAN_POINT('',(26.1054324307097,-16.1877442736409,-9.63701947055319)) ;
#56048 = CARTESIAN_POINT('Ctrl Pts',(28.1037899993503,-15.9108618900532,-8.3140683522349)) ;
#56049 = CARTESIAN_POINT('Ctrl Pts',(28.034304736139,-15.9226008880843,-8.32770191715421)) ;
#56050 = CARTESIAN_POINT('Ctrl Pts',(27.9654373146411,-15.9340937467164,-8.34369210999802)) ;
#56051 = CARTESIAN_POINT('Ctrl Pts',(27.8974789538808,-15.9452906277875,-8.36191580337098)) ;
#56052 = CARTESIAN_POINT('Ctrl Pts',(27.8741538504537,-15.9491336929544,-8.36817065601886)) ;
#56053 = CARTESIAN_POINT('Ctrl Pts',(27.8509356814767,-15.9529419413759,-8.37468820324564)) ;
#56054 = CARTESIAN_POINT('Ctrl Pts',(27.82783568028,-15.9567135267634,-8.38146217165719)) ;
#56055 = CARTESIAN_POINT('Ctrl Pts',(27.7624953705522,-15.9673817754483,-8.40062291499775)) ;
#56056 = CARTESIAN_POINT('Ctrl Pts',(27.698092879999,-15.9777576912911,-8.42184141437466)) ;
#56057 = CARTESIAN_POINT('Ctrl Pts',(27.6348927990567,-15.9877997661733,-8.44493981550727)) ;
#56058 = CARTESIAN_POINT('Ctrl Pts',(27.5711777968354,-15.9979236586412,-8.46822641035863)) ;
#56059 = CARTESIAN_POINT('Ctrl Pts',(27.5086852863975,-16.0077081692746,-8.49342336485628)) ;
#56060 = CARTESIAN_POINT('Ctrl Pts',(27.4476572216975,-16.0171189356807,-8.52030462830303)) ;
#56061 = CARTESIAN_POINT('Ctrl Pts',(27.3977158735079,-16.0248200870138,-8.54230248362045)) ;
#56062 = CARTESIAN_POINT('Ctrl Pts',(27.3487547422468,-16.0322710948775,-8.56542735098012)) ;
#56063 = CARTESIAN_POINT('Ctrl Pts',(27.3008894727844,-16.0394576303854,-8.58953619992411)) ;
#56064 = CARTESIAN_POINT('Ctrl Pts',(27.2423246003303,-16.048250614111,-8.61903424055521)) ;
#56065 = CARTESIAN_POINT('Ctrl Pts',(27.1838991596106,-16.0568730319551,-8.65076294644521)) ;
#56066 = CARTESIAN_POINT('Ctrl Pts',(27.1259441443405,-16.0652608298868,-8.68470469707721)) ;
#56067 = CARTESIAN_POINT('Ctrl Pts',(27.0684641915654,-16.0735798722812,-8.71836822411347)) ;
#56068 = CARTESIAN_POINT('Ctrl Pts',(27.011447463296,-16.0816680200512,-8.75420859693357)) ;
#56069 = CARTESIAN_POINT('Ctrl Pts',(26.9552071539288,-16.0894673869314,-8.79215866740018)) ;
#56070 = CARTESIAN_POINT('Ctrl Pts',(26.9089941977332,-16.095876167467,-8.82334243868145)) ;
#56071 = CARTESIAN_POINT('Ctrl Pts',(26.8633054246535,-16.1020900207686,-8.85594973051555)) ;
#56072 = CARTESIAN_POINT('Ctrl Pts',(26.8183061828456,-16.108079933754,-8.88991847615642)) ;
#56073 = CARTESIAN_POINT('Ctrl Pts',(26.7619644875617,-16.1155796568302,-8.93244934199296)) ;
#56074 = CARTESIAN_POINT('Ctrl Pts',(26.706696039165,-16.1227292229209,-8.97712180235449)) ;
#56075 = CARTESIAN_POINT('Ctrl Pts',(26.6527820556249,-16.1294814162038,-9.02378910382704)) ;
#56076 = CARTESIAN_POINT('Ctrl Pts',(26.5989746698281,-16.1362202591735,-9.07036413556367)) ;
#56077 = CARTESIAN_POINT('Ctrl Pts',(26.5465168245935,-16.142563213636,-9.11892585748311)) ;
#56078 = CARTESIAN_POINT('Ctrl Pts',(26.495660552787,-16.1484717649152,-9.169285175488)) ;
#56079 = CARTESIAN_POINT('Ctrl Pts',(26.4573070580305,-16.1529277264408,-9.20726389021547)) ;
#56080 = CARTESIAN_POINT('Ctrl Pts',(26.4198639271609,-16.1571367885212,-9.24626406062484)) ;
#56081 = CARTESIAN_POINT('Ctrl Pts',(26.3834267567978,-16.1610860188908,-9.28618986789499)) ;
#56082 = CARTESIAN_POINT('Ctrl Pts',(26.3330202775945,-16.166549308068,-9.34142246015669)) ;
#56083 = CARTESIAN_POINT('Ctrl Pts',(26.2845066768924,-16.171518536629,-9.39846541580138)) ;
#56084 = CARTESIAN_POINT('Ctrl Pts',(26.2381082630198,-16.1759680067789,-9.45703697656326)) ;
#56085 = CARTESIAN_POINT('Ctrl Pts',(26.1917098491729,-16.1804174769265,-9.51560853729283)) ;
#56086 = CARTESIAN_POINT('Ctrl Pts',(26.1474269617336,-16.184347145014,-9.57570816684701)) ;
#56087 = CARTESIAN_POINT('Ctrl Pts',(26.1054324306225,-16.1877442734701,-9.63701947062993)) ;
#56088 = CARTESIAN_POINT('',(27.4875585758881,-15.9108618782029,-10.1676384740821)) ;
#56089 = CARTESIAN_POINT('Ctrl Pts',(27.4875585758879,-15.9108618782028,-10.1676384740828)) ;
#56090 = CARTESIAN_POINT('Ctrl Pts',(26.7875846204384,-16.0510971581644,-9.89877855202715)) ;
#56091 = CARTESIAN_POINT('Ctrl Pts',(26.1054324308419,-16.1877442737199,-9.63701947038512)) ;
#56092 = CARTESIAN_POINT('',(26.9481230865112,-15.9108618782029,-11.5215194621522)) ;
#56093 = CARTESIAN_POINT('Origin',(-2.92277791062251E-15,-15.9108618782028,
0.)) ;
#56094 = CARTESIAN_POINT('',(25.5797993342585,-16.1877442736409,-10.9562590645367)) ;
#56095 = CARTESIAN_POINT('Ctrl Pts',(25.579799334239,-16.1877442737199,-10.9562590647496)) ;
#56096 = CARTESIAN_POINT('Ctrl Pts',(26.2550503277099,-16.0510971581193,-11.2353388432409)) ;
#56097 = CARTESIAN_POINT('Ctrl Pts',(26.9481230865116,-15.9108618782028,-11.5215194621516)) ;
#56098 = CARTESIAN_POINT('',(26.1208051708581,-15.9108618823941,-13.2909850543146)) ;
#56099 = CARTESIAN_POINT('Ctrl Pts',(25.579799334248,-16.1877442734701,-10.9562590644211)) ;
#56100 = CARTESIAN_POINT('Ctrl Pts',(25.568123424087,-16.184347145014,-11.0296504108912)) ;
#56101 = CARTESIAN_POINT('Ctrl Pts',(25.5589421180155,-16.1804174769264,-11.1037357887423)) ;
#56102 = CARTESIAN_POINT('Ctrl Pts',(25.5523475266828,-16.1759680067789,-11.178166641881)) ;
#56103 = CARTESIAN_POINT('Ctrl Pts',(25.5457529353466,-16.171518536629,-11.2525974950608)) ;
#56104 = CARTESIAN_POINT('Ctrl Pts',(25.541745181025,-16.166549308068,-11.3273732006547)) ;
#56105 = CARTESIAN_POINT('Ctrl Pts',(25.5403566338808,-16.1610860188908,-11.4021363221146)) ;
#56106 = CARTESIAN_POINT('Ctrl Pts',(25.5390261782592,-16.1558512929189,-11.4737716394019)) ;
#56107 = CARTESIAN_POINT('Ctrl Pts',(25.5400991249098,-16.1501596984484,-11.5454416108816)) ;
#56108 = CARTESIAN_POINT('Ctrl Pts',(25.5435610181598,-16.1440425621063,-11.616831523354)) ;
#56109 = CARTESIAN_POINT('Ctrl Pts',(25.5470300636165,-16.1379127878751,-11.6883689260482)) ;
#56110 = CARTESIAN_POINT('Ctrl Pts',(25.5528978824486,-16.1313557844545,-11.7596246018672)) ;
#56111 = CARTESIAN_POINT('Ctrl Pts',(25.5610987922911,-16.124412468004,-11.8302887546736)) ;
#56112 = CARTESIAN_POINT('Ctrl Pts',(25.5672783132574,-16.1191805644219,-11.8835353605034)) ;
#56113 = CARTESIAN_POINT('Ctrl Pts',(25.5747814590423,-16.1137295207042,-11.9364462043401)) ;
#56114 = CARTESIAN_POINT('Ctrl Pts',(25.583561515064,-16.1080799337539,-11.9888939120546)) ;
#56115 = CARTESIAN_POINT('Ctrl Pts',(25.594875159794,-16.1008000918636,-12.056476024346)) ;
#56116 = CARTESIAN_POINT('Ctrl Pts',(25.6083124325426,-16.0931892946343,-12.1232980022537)) ;
#56117 = CARTESIAN_POINT('Ctrl Pts',(25.6237302964865,-16.0853002129678,-12.1890767808231)) ;
#56118 = CARTESIAN_POINT('Ctrl Pts',(25.6392738836098,-16.0773468007019,-12.2553919447961)) ;
#56119 = CARTESIAN_POINT('Ctrl Pts',(25.6568302519724,-16.0691106491229,-12.3206463859086)) ;
#56120 = CARTESIAN_POINT('Ctrl Pts',(25.6762064916025,-16.0606518030567,-12.3845755781982)) ;
#56121 = CARTESIAN_POINT('Ctrl Pts',(25.6920743943232,-16.0537245483844,-12.4369295036055)) ;
#56122 = CARTESIAN_POINT('Ctrl Pts',(25.709161848733,-16.046648082628,-12.4883950429174)) ;
#56123 = CARTESIAN_POINT('Ctrl Pts',(25.7273420792229,-16.0394576303854,-12.5388423577954)) ;
#56124 = CARTESIAN_POINT('Ctrl Pts',(25.7495783165907,-16.0306629892537,-12.6005444615625)) ;
#56125 = CARTESIAN_POINT('Ctrl Pts',(25.7740208512851,-16.0214720150687,-12.6623053003954)) ;
#56126 = CARTESIAN_POINT('Ctrl Pts',(25.8006914174555,-16.0119118209662,-12.7237889985167)) ;
#56127 = CARTESIAN_POINT('Ctrl Pts',(25.8271435441353,-16.0024299275611,-12.784769127737)) ;
#56128 = CARTESIAN_POINT('Ctrl Pts',(25.8557873490937,-15.9925848997544,-12.8454761456396)) ;
#56129 = CARTESIAN_POINT('Ctrl Pts',(25.886593953266,-15.9824119250013,-12.9055877146238)) ;
#56130 = CARTESIAN_POINT('Ctrl Pts',(25.9118892323843,-15.974058903214,-12.9549452779303)) ;
#56131 = CARTESIAN_POINT('Ctrl Pts',(25.938641745247,-15.9654849570548,-13.0039013583173)) ;
#56132 = CARTESIAN_POINT('Ctrl Pts',(25.9668102537101,-15.9567135267634,-13.0522837860431)) ;
#56133 = CARTESIAN_POINT('Ctrl Pts',(26.0020990379238,-15.9457249040891,-13.1128960493439)) ;
#56134 = CARTESIAN_POINT('Ctrl Pts',(26.0396164464604,-15.9344245943221,-13.1726164001282)) ;
#56135 = CARTESIAN_POINT('Ctrl Pts',(26.079251847358,-15.9228603613878,-13.231147679351)) ;
#56136 = CARTESIAN_POINT('Ctrl Pts',(26.0928557632711,-15.9188912113635,-13.2512371595329)) ;
#56137 = CARTESIAN_POINT('Ctrl Pts',(26.1067087778732,-15.9148910240723,-13.2711867422769)) ;
#56138 = CARTESIAN_POINT('Ctrl Pts',(26.1208051521851,-15.9108618900532,-13.2909850310201)) ;
#56139 = CARTESIAN_POINT('',(25.6594598237771,-15.9108618960635,-14.1611741945452)) ;
#56140 = CARTESIAN_POINT('Origin',(-2.92277791062251E-15,-15.9108618782028,
0.)) ;
#56141 = CARTESIAN_POINT('',(23.4234276096246,-16.1877442736409,-15.0236076122497)) ;
#56142 = CARTESIAN_POINT('Ctrl Pts',(25.6594598224132,-15.9108619316234,-14.1611741563844)) ;
#56143 = CARTESIAN_POINT('Ctrl Pts',(25.5886682727421,-15.922600929087,-14.1595517042466)) ;
#56144 = CARTESIAN_POINT('Ctrl Pts',(25.5179735150173,-15.9340937870887,-14.1603636010547)) ;
#56145 = CARTESIAN_POINT('Ctrl Pts',(25.4476864284671,-15.9452906674734,-14.1635522014843)) ;
#56146 = CARTESIAN_POINT('Ctrl Pts',(25.4235621279405,-15.9491337191721,-14.1646466095583)) ;
#56147 = CARTESIAN_POINT('Ctrl Pts',(25.3994857899391,-15.9529419543585,-14.1660205563673)) ;
#56148 = CARTESIAN_POINT('Ctrl Pts',(25.3754697336308,-15.9567135267634,-14.1676703300568)) ;
#56149 = CARTESIAN_POINT('Ctrl Pts',(25.3075380506038,-15.9673817754482,-14.1723368707201)) ;
#56150 = CARTESIAN_POINT('Ctrl Pts',(25.2400799043394,-15.977757691291,-14.1792146616279)) ;
#56151 = CARTESIAN_POINT('Ctrl Pts',(25.1733919327092,-15.9877997661731,-14.1881868857565)) ;
#56152 = CARTESIAN_POINT('Ctrl Pts',(25.1061606222867,-15.997923658641,-14.1972322108852)) ;
#56153 = CARTESIAN_POINT('Ctrl Pts',(25.039712551615,-16.0077081692744,-14.2084060321102)) ;
#56154 = CARTESIAN_POINT('Ctrl Pts',(24.9743326121174,-16.0171189356805,-14.2215395966218)) ;
#56155 = CARTESIAN_POINT('Ctrl Pts',(24.9208299762537,-16.0248200870136,-14.2322872407014)) ;
#56156 = CARTESIAN_POINT('Ctrl Pts',(24.8680423661167,-16.0322710948774,-14.2443462655726)) ;
#56157 = CARTESIAN_POINT('Ctrl Pts',(24.8161134701842,-16.0394576303853,-14.2576018449788)) ;
#56158 = CARTESIAN_POINT('Ctrl Pts',(24.7525766051236,-16.0482506141109,-14.2738205213998)) ;
#56159 = CARTESIAN_POINT('Ctrl Pts',(24.6886963848685,-16.0568730319549,-14.2922476850668)) ;
#56160 = CARTESIAN_POINT('Ctrl Pts',(24.6247998525748,-16.0652608298865,-14.3129372812856)) ;
#56161 = CARTESIAN_POINT('Ctrl Pts',(24.5614270859275,-16.073579872281,-14.3334572830154)) ;
#56162 = CARTESIAN_POINT('Ctrl Pts',(24.498038756358,-16.081668020051,-14.3562028166603)) ;
#56163 = CARTESIAN_POINT('Ctrl Pts',(24.4349551708164,-16.0894673869312,-14.3811756315062)) ;
#56164 = CARTESIAN_POINT('Ctrl Pts',(24.3831190588151,-16.0958761674669,-14.4016959240075)) ;
#56165 = CARTESIAN_POINT('Ctrl Pts',(24.33148885998,-16.1020900207685,-14.4237191398173)) ;
#56166 = CARTESIAN_POINT('Ctrl Pts',(24.2802393992345,-16.108079933754,-14.4472202082416)) ;
#56167 = CARTESIAN_POINT('Ctrl Pts',(24.2160720625252,-16.1155796568302,-14.4766449270323)) ;
#56168 = CARTESIAN_POINT('Ctrl Pts',(24.1524925012697,-16.1227292229209,-14.5083918874139)) ;
#56169 = CARTESIAN_POINT('Ctrl Pts',(24.0898069063631,-16.1294814162038,-14.5423782205364)) ;
#56170 = CARTESIAN_POINT('Ctrl Pts',(24.0272452522698,-16.1362202591735,-14.5762973565018)) ;
#56171 = CARTESIAN_POINT('Ctrl Pts',(23.9655745075671,-16.142563213636,-14.6124468462664)) ;
#56172 = CARTESIAN_POINT('Ctrl Pts',(23.9050814623739,-16.1484717649152,-14.6506961962637)) ;
#56173 = CARTESIAN_POINT('Ctrl Pts',(23.8594603499876,-16.1529277264408,-14.6795421220946)) ;
#56174 = CARTESIAN_POINT('Ctrl Pts',(23.8145087349089,-16.1571367885212,-14.7095813238667)) ;
#56175 = CARTESIAN_POINT('Ctrl Pts',(23.7703405769757,-16.1610860188908,-14.7407407733971)) ;
#56176 = CARTESIAN_POINT('Ctrl Pts',(23.7092391985723,-16.1665493080681,-14.7838461553213)) ;
#56177 = CARTESIAN_POINT('Ctrl Pts',(23.6495972696092,-16.171518536629,-14.8291264882632)) ;
#56178 = CARTESIAN_POINT('Ctrl Pts',(23.5916924706681,-16.1759680067789,-14.876354391028)) ;
#56179 = CARTESIAN_POINT('Ctrl Pts',(23.5337876717589,-16.1804174769265,-14.9235822937668)) ;
#56180 = CARTESIAN_POINT('Ctrl Pts',(23.4776204497978,-16.184347145014,-14.9727573155733)) ;
#56181 = CARTESIAN_POINT('Ctrl Pts',(23.423427609523,-16.1877442734701,-15.0236076123058)) ;
#56182 = CARTESIAN_POINT('',(24.659173012817,-15.9108618782029,-15.8389373042029)) ;
#56183 = CARTESIAN_POINT('Ctrl Pts',(24.6591730128168,-15.9108618782028,-15.8389373042032)) ;
#56184 = CARTESIAN_POINT('Ctrl Pts',(24.0333609963471,-16.0510971579214,-15.4258894690935)) ;
#56185 = CARTESIAN_POINT('Ctrl Pts',(23.4234276097899,-16.1877442737199,-15.0236076121142)) ;
#56186 = CARTESIAN_POINT('',(23.8413048334143,-15.9108618782029,-17.045202622519)) ;
#56187 = CARTESIAN_POINT('Origin',(-2.92277791062251E-15,-15.9108618782028,
0.)) ;
#56188 = CARTESIAN_POINT('',(22.6264860066069,-16.1877442736409,-16.199008539506)) ;
#56189 = CARTESIAN_POINT('Ctrl Pts',(22.6264860065421,-16.1877442737199,-16.1990085397097)) ;
#56190 = CARTESIAN_POINT('Ctrl Pts',(23.2259561029842,-16.0510971583948,-16.6167225905446)) ;
#56191 = CARTESIAN_POINT('Ctrl Pts',(23.8413048334146,-15.9108618782028,-17.0452026225187)) ;
#56192 = CARTESIAN_POINT('',(22.6529462781943,-15.9108618960635,-18.595449925547)) ;
#56193 = CARTESIAN_POINT('Ctrl Pts',(22.6264860066214,-16.1877442734702,-16.1990085393908)) ;
#56194 = CARTESIAN_POINT('Ctrl Pts',(22.5993061026931,-16.184347145014,-16.2681740614178)) ;
#56195 = CARTESIAN_POINT('Ctrl Pts',(22.5744132841655,-16.1804174769265,-16.3385536548969)) ;
#56196 = CARTESIAN_POINT('Ctrl Pts',(22.551972437449,-16.1759680067789,-16.4098267138495)) ;
#56197 = CARTESIAN_POINT('Ctrl Pts',(22.5295315907202,-16.171518536629,-16.4810997728414)) ;
#56198 = CARTESIAN_POINT('Ctrl Pts',(22.5095429691188,-16.1665493080681,-16.5532657152816)) ;
#56199 = CARTESIAN_POINT('Ctrl Pts',(22.4921150243035,-16.1610860188908,-16.6259824199177)) ;
#56200 = CARTESIAN_POINT('Ctrl Pts',(22.4754161983031,-16.155851292919,-16.6956569346638)) ;
#56201 = CARTESIAN_POINT('Ctrl Pts',(22.4610571347385,-16.1501596984485,-16.7658819538511)) ;
#56202 = CARTESIAN_POINT('Ctrl Pts',(22.4490913699374,-16.1440425621065,-16.8363470145571)) ;
#56203 = CARTESIAN_POINT('Ctrl Pts',(22.4371008840904,-16.1379127878753,-16.9069576547587)) ;
#56204 = CARTESIAN_POINT('Ctrl Pts',(22.4275136525808,-16.1313557844548,-16.9778088200711)) ;
#56205 = CARTESIAN_POINT('Ctrl Pts',(22.4203321256725,-16.1244124680044,-17.048583837452)) ;
#56206 = CARTESIAN_POINT('Ctrl Pts',(22.4149207265774,-16.1191805644222,-17.101913981571)) ;
#56207 = CARTESIAN_POINT('Ctrl Pts',(22.4108741855918,-16.1137295207043,-17.1552007538358)) ;
#56208 = CARTESIAN_POINT('Ctrl Pts',(22.4081742619674,-16.1080799337539,-17.2083097157992)) ;
#56209 = CARTESIAN_POINT('Ctrl Pts',(22.4046952435411,-16.1008000918637,-17.2767438950482)) ;
#56210 = CARTESIAN_POINT('Ctrl Pts',(22.4034536103134,-16.0931892946346,-17.3448922286831)) ;
#56211 = CARTESIAN_POINT('Ctrl Pts',(22.4043705201805,-16.0853002129682,-17.4124475209615)) ;
#56212 = CARTESIAN_POINT('Ctrl Pts',(22.4052949068825,-16.0773468007024,-17.4805536850181)) ;
#56213 = CARTESIAN_POINT('Ctrl Pts',(22.4084130411773,-16.0691106491235,-17.5480566137945)) ;
#56214 = CARTESIAN_POINT('Ctrl Pts',(22.4135933884833,-16.0606518030574,-17.6146564958564)) ;
#56215 = CARTESIAN_POINT('Ctrl Pts',(22.4178357620649,-16.0537245483849,-17.6691975456164)) ;
#56216 = CARTESIAN_POINT('Ctrl Pts',(22.4234601516448,-16.0466480826283,-17.7231331468177)) ;
#56217 = CARTESIAN_POINT('Ctrl Pts',(22.4303706569622,-16.0394576303854,-17.7763092436615)) ;
#56218 = CARTESIAN_POINT('Ctrl Pts',(22.4388228950485,-16.0306629892537,-17.8413489202666)) ;
#56219 = CARTESIAN_POINT('Ctrl Pts',(22.449417222153,-16.0214720150687,-17.9069202474519)) ;
#56220 = CARTESIAN_POINT('Ctrl Pts',(22.4622470676566,-16.0119118209662,-17.9726998742285)) ;
#56221 = CARTESIAN_POINT('Ctrl Pts',(22.4749718330917,-16.0024299275611,-18.0379407472317)) ;
#56222 = CARTESIAN_POINT('Ctrl Pts',(22.4898957474453,-15.9925848997544,-18.1033860401522)) ;
#56223 = CARTESIAN_POINT('Ctrl Pts',(22.5070598998852,-15.9824119250013,-18.1687147433183)) ;
#56224 = CARTESIAN_POINT('Ctrl Pts',(22.5211533723229,-15.974058903214,-18.2223560915107)) ;
#56225 = CARTESIAN_POINT('Ctrl Pts',(22.5367563161497,-15.9654849570549,-18.2759186054106)) ;
#56226 = CARTESIAN_POINT('Ctrl Pts',(22.5538654687518,-15.9567135267634,-18.3292252755273)) ;
#56227 = CARTESIAN_POINT('Ctrl Pts',(22.5752993758999,-15.9457249040774,-18.396006503343)) ;
#56228 = CARTESIAN_POINT('Ctrl Pts',(22.5991015382038,-15.934424594298,-18.462395759412)) ;
#56229 = CARTESIAN_POINT('Ctrl Pts',(22.6252277906263,-15.9228603613509,-18.5280790495003)) ;
#56230 = CARTESIAN_POINT('Ctrl Pts',(22.6341949792813,-15.9188912249891,-18.5506232109889)) ;
#56231 = CARTESIAN_POINT('Ctrl Pts',(22.6434355147679,-15.9148910515742,-18.5730842951907)) ;
#56232 = CARTESIAN_POINT('Ctrl Pts',(22.652946242239,-15.9108619316234,-18.5954499384048)) ;
#56233 = CARTESIAN_POINT('',(22.0153220853233,-15.9108618949459,-19.3461191882741)) ;
#56234 = CARTESIAN_POINT('Origin',(-2.92277791062251E-15,-15.9108618782028,
0.)) ;
#56235 = CARTESIAN_POINT('',(19.6461693467839,-16.1877442736409,-19.7077085595375)) ;
#56236 = CARTESIAN_POINT('Ctrl Pts',(22.0153220904288,-15.9108619279123,-19.3461191530285)) ;
#56237 = CARTESIAN_POINT('Ctrl Pts',(21.9465343871962,-15.9226009254266,-19.3293165418211)) ;
#56238 = CARTESIAN_POINT('Ctrl Pts',(21.8773178998704,-15.9340937834848,-19.314912173237)) ;
#56239 = CARTESIAN_POINT('Ctrl Pts',(21.8079886315363,-15.9452906639308,-19.3029165795175)) ;
#56240 = CARTESIAN_POINT('Ctrl Pts',(21.7841930710607,-15.9491337168317,-19.2987993879957)) ;
#56241 = CARTESIAN_POINT('Ctrl Pts',(21.7603842591961,-15.9529419531996,-19.2949655104482)) ;
#56242 = CARTESIAN_POINT('Ctrl Pts',(21.7365750250461,-15.9567135267635,-19.2914139700575)) ;
#56243 = CARTESIAN_POINT('Ctrl Pts',(21.6692283787169,-15.9673817754483,-19.2813681057887)) ;
#56244 = CARTESIAN_POINT('Ctrl Pts',(21.6018688446853,-15.9777576912911,-19.2735835903689)) ;
#56245 = CARTESIAN_POINT('Ctrl Pts',(21.5348112378018,-15.9877997661733,-19.2680101062651)) ;
#56246 = CARTESIAN_POINT('Ctrl Pts',(21.4672072805305,-15.9979236586412,-19.2623912123214)) ;
#56247 = CARTESIAN_POINT('Ctrl Pts',(21.3999106875573,-16.0077081692748,-19.2590194248121)) ;
#56248 = CARTESIAN_POINT('Ctrl Pts',(21.3332359665677,-16.0171189356809,-19.2577911795092)) ;
#56249 = CARTESIAN_POINT('Ctrl Pts',(21.2786737668204,-16.0248200870139,-19.2567860644587)) ;
#56250 = CARTESIAN_POINT('Ctrl Pts',(21.2245279677896,-16.0322710948776,-19.2572153802409)) ;
#56251 = CARTESIAN_POINT('Ctrl Pts',(21.1709635828472,-16.0394576303854,-19.2589978739485)) ;
#56252 = CARTESIAN_POINT('Ctrl Pts',(21.105425638374,-16.0482506141109,-19.261178818876)) ;
#56253 = CARTESIAN_POINT('Ctrl Pts',(21.0390776066841,-16.0568730319549,-19.2654428066277)) ;
#56254 = CARTESIAN_POINT('Ctrl Pts',(20.9722272882007,-16.0652608298865,-19.2719128259091)) ;
#56255 = CARTESIAN_POINT('Ctrl Pts',(20.9059249478159,-16.073579872281,-19.2783298098581)) ;
#56256 = CARTESIAN_POINT('Ctrl Pts',(20.8391289847859,-16.0816680200509,-19.2869169484544)) ;
#56257 = CARTESIAN_POINT('Ctrl Pts',(20.7721518414175,-16.0894673869311,-19.2977448066129)) ;
#56258 = CARTESIAN_POINT('Ctrl Pts',(20.7171163725964,-16.0958761674669,-19.3066421142631)) ;
#56259 = CARTESIAN_POINT('Ctrl Pts',(20.661958918721,-16.1020900207685,-19.3170514729541)) ;
#56260 = CARTESIAN_POINT('Ctrl Pts',(20.6068556068631,-16.108079933754,-19.3289859803214)) ;
#56261 = CARTESIAN_POINT('Ctrl Pts',(20.5378630220768,-16.1155796568301,-19.3439286849187)) ;
#56262 = CARTESIAN_POINT('Ctrl Pts',(20.4689452575836,-16.1227292229207,-19.3612656927369)) ;
#56263 = CARTESIAN_POINT('Ctrl Pts',(20.4004191600592,-16.1294814162036,-19.3809818943453)) ;
#56264 = CARTESIAN_POINT('Ctrl Pts',(20.3320285510829,-16.1362202591732,-19.4006591134401)) ;
#56265 = CARTESIAN_POINT('Ctrl Pts',(20.264028562393,-16.1425632136357,-19.4227060610854)) ;
#56266 = CARTESIAN_POINT('Ctrl Pts',(20.1967273313737,-16.1484717649149,-19.4470569459802)) ;
#56267 = CARTESIAN_POINT('Ctrl Pts',(20.1459717938674,-16.1529277264406,-19.4654212794829)) ;
#56268 = CARTESIAN_POINT('Ctrl Pts',(20.0956135821392,-16.1571367885211,-19.4850949129296)) ;
#56269 = CARTESIAN_POINT('Ctrl Pts',(20.0457796906102,-16.1610860188908,-19.5060310234919)) ;
#56270 = CARTESIAN_POINT('Ctrl Pts',(19.9768404455517,-16.166549308068,-19.5349936353278)) ;
#56271 = CARTESIAN_POINT('Ctrl Pts',(19.9088589786387,-16.171518536629,-19.566394087524)) ;
#56272 = CARTESIAN_POINT('Ctrl Pts',(19.8421553586711,-16.1759680067789,-19.6000700080484)) ;
#56273 = CARTESIAN_POINT('Ctrl Pts',(19.7754517387401,-16.1804174769264,-19.6337459285543)) ;
#56274 = CARTESIAN_POINT('Ctrl Pts',(19.7100264991306,-16.184347145014,-19.6696969732477)) ;
#56275 = CARTESIAN_POINT('Ctrl Pts',(19.6461693466726,-16.1877442734701,-19.7077085595704)) ;
#56276 = CARTESIAN_POINT('',(20.6777519263696,-15.9108618782029,-20.7696250296925)) ;
#56277 = CARTESIAN_POINT('Ctrl Pts',(20.6777519263701,-15.9108618782028,-20.7696250296921)) ;
#56278 = CARTESIAN_POINT('Ctrl Pts',(20.1553641257598,-16.0510971569168,-20.231702942616)) ;
#56279 = CARTESIAN_POINT('Ctrl Pts',(19.6461693469744,-16.1877442737198,-19.7077085594409)) ;
#56280 = CARTESIAN_POINT('',(19.619693664013,-15.9108618782029,-21.7718710526404)) ;
#56281 = CARTESIAN_POINT('Origin',(-2.92277791062251E-15,-15.9108618782028,
0.)) ;
#56282 = CARTESIAN_POINT('',(18.6151833408189,-16.1877442736409,-20.6843103790742)) ;
#56283 = CARTESIAN_POINT('Ctrl Pts',(18.615183340712,-16.1877442737198,-20.6843103792592)) ;
#56284 = CARTESIAN_POINT('Ctrl Pts',(19.1108419892473,-16.0510971575107,-21.2211268617121)) ;
#56285 = CARTESIAN_POINT('Ctrl Pts',(19.6196936640126,-15.9108618782028,-21.7718710526408)) ;
#56286 = CARTESIAN_POINT('',(18.1258609279823,-15.9108618949459,-23.0304124971064)) ;
#56287 = CARTESIAN_POINT('Ctrl Pts',(18.6151833408578,-16.1877442734701,-20.6843103789648)) ;
#56288 = CARTESIAN_POINT('Ctrl Pts',(18.5737703452616,-16.184347145014,-20.7460159736105)) ;
#56289 = CARTESIAN_POINT('Ctrl Pts',(18.5343299748061,-16.1804174769264,-20.8093989111475)) ;
#56290 = CARTESIAN_POINT('Ctrl Pts',(18.497092181757,-16.1759680067789,-20.8741815268916)) ;
#56291 = CARTESIAN_POINT('Ctrl Pts',(18.4598543886874,-16.171518536629,-20.9389641426714)) ;
#56292 = CARTESIAN_POINT('Ctrl Pts',(18.4248195455368,-16.166549308068,-21.0051459226955)) ;
#56293 = CARTESIAN_POINT('Ctrl Pts',(18.39216711438,-16.1610860188908,-21.0724160582175)) ;
#56294 = CARTESIAN_POINT('Ctrl Pts',(18.3608807365454,-16.155851292919,-21.1368718675514)) ;
#56295 = CARTESIAN_POINT('Ctrl Pts',(18.3317610766189,-16.1501596984485,-21.2023682905993)) ;
#56296 = CARTESIAN_POINT('Ctrl Pts',(18.30492715963,-16.1440425621065,-21.2686136316174)) ;
#56297 = CARTESIAN_POINT('Ctrl Pts',(18.2780378042711,-16.1379127878753,-21.3349958342692)) ;
#56298 = CARTESIAN_POINT('Ctrl Pts',(18.2534438107098,-16.1313557844548,-21.4021295673313)) ;
#56299 = CARTESIAN_POINT('Ctrl Pts',(18.2312156472675,-16.1244124680044,-21.4697060881353)) ;
#56300 = CARTESIAN_POINT('Ctrl Pts',(18.2144663591183,-16.1191805644222,-21.5206261122753)) ;
#56301 = CARTESIAN_POINT('Ctrl Pts',(18.199059343121,-16.1137295207043,-21.5717971827197)) ;
#56302 = CARTESIAN_POINT('Ctrl Pts',(18.1850056852781,-16.1080799337539,-21.6230840828956)) ;
#56303 = CARTESIAN_POINT('Ctrl Pts',(18.1668966787307,-16.1008000918638,-21.6891704229405)) ;
#56304 = CARTESIAN_POINT('Ctrl Pts',(18.1510341969168,-16.0931892946346,-21.7554585719638)) ;
#56305 = CARTESIAN_POINT('Ctrl Pts',(18.1374072790211,-16.0853002129682,-21.8216315675676)) ;
#56306 = CARTESIAN_POINT('Ctrl Pts',(18.1236692420074,-16.0773468007025,-21.8883441631719)) ;
#56307 = CARTESIAN_POINT('Ctrl Pts',(18.1122033417405,-16.0691106491235,-21.9549392176873)) ;
#56308 = CARTESIAN_POINT('Ctrl Pts',(18.1029455694405,-16.0606518030575,-22.0210956530574)) ;
#56309 = CARTESIAN_POINT('Ctrl Pts',(18.0953640452087,-16.053724548385,-22.0752735482998)) ;
#56310 = CARTESIAN_POINT('Ctrl Pts',(18.0892623797524,-16.0466480826283,-22.129157242622)) ;
#56311 = CARTESIAN_POINT('Ctrl Pts',(18.0845800323485,-16.0394576303854,-22.1825756662427)) ;
#56312 = CARTESIAN_POINT('Ctrl Pts',(18.0788530538943,-16.0306629892537,-22.2479117326944)) ;
#56313 = CARTESIAN_POINT('Ctrl Pts',(18.0751037944482,-16.0214720150686,-22.3142275058505)) ;
#56314 = CARTESIAN_POINT('Ctrl Pts',(18.0734930099685,-16.0119118209661,-22.3812272790436)) ;
#56315 = CARTESIAN_POINT('Ctrl Pts',(18.0718954182698,-16.0024299275609,-22.4476783051183)) ;
#56316 = CARTESIAN_POINT('Ctrl Pts',(18.0724016163703,-15.9925848997542,-22.5148017238976)) ;
#56317 = CARTESIAN_POINT('Ctrl Pts',(18.0751207403865,-15.9824119250011,-22.5822928636936)) ;
#56318 = CARTESIAN_POINT('Ctrl Pts',(18.0773534110361,-15.9740589032138,-22.6377097869478)) ;
#56319 = CARTESIAN_POINT('Ctrl Pts',(18.081077209515,-15.9654849570548,-22.6933742107403)) ;
#56320 = CARTESIAN_POINT('Ctrl Pts',(18.0863270012958,-15.9567135267635,-22.7491125625987)) ;
#56321 = CARTESIAN_POINT('Ctrl Pts',(18.0929038056638,-15.9457249040785,-22.8189401388673)) ;
#56322 = CARTESIAN_POINT('Ctrl Pts',(18.1018777590367,-15.9344245943002,-22.8888940123242)) ;
#56323 = CARTESIAN_POINT('Ctrl Pts',(18.1132732284097,-15.9228603613543,-22.9586580355687)) ;
#56324 = CARTESIAN_POINT('Ctrl Pts',(18.1171844420595,-15.9188912237728,-22.9826028149406)) ;
#56325 = CARTESIAN_POINT('Ctrl Pts',(18.1213804711799,-15.9148910491191,-23.0065252208016)) ;
#56326 = CARTESIAN_POINT('Ctrl Pts',(18.125860892512,-15.9108619279123,-23.0304125002962)) ;
#56327 = CARTESIAN_POINT('',(17.3417723053832,-15.9108618962294,-23.6264611434763)) ;
#56328 = CARTESIAN_POINT('Origin',(-2.92277791062251E-15,-15.9108618782028,
0.)) ;
#56329 = CARTESIAN_POINT('',(14.9502780404355,-16.1877442736409,-23.4702989581266)) ;
#56330 = CARTESIAN_POINT('Ctrl Pts',(17.3417723204951,-15.9108619321403,-23.6264611079952)) ;
#56331 = CARTESIAN_POINT('Ctrl Pts',(17.2782049000365,-15.9226009295966,-23.595264010192)) ;
#56332 = CARTESIAN_POINT('Ctrl Pts',(17.2137031689819,-15.9340937875903,-23.5663169095397)) ;
#56333 = CARTESIAN_POINT('Ctrl Pts',(17.1485734783208,-15.9452906679664,-23.5396980233582)) ;
#56334 = CARTESIAN_POINT('Ctrl Pts',(17.1262193270725,-15.9491337194978,-23.5305617507654)) ;
#56335 = CARTESIAN_POINT('Ctrl Pts',(17.1037913301717,-15.9529419545198,-23.5216993195756)) ;
#56336 = CARTESIAN_POINT('Ctrl Pts',(17.0813022267581,-15.9567135267635,-23.5131125336849)) ;
#56337 = CARTESIAN_POINT('Ctrl Pts',(17.0176896714601,-15.9673817754481,-23.4888239979325)) ;
#56338 = CARTESIAN_POINT('Ctrl Pts',(16.9535784066094,-15.9777576912908,-23.4667411714743)) ;
#56339 = CARTESIAN_POINT('Ctrl Pts',(16.8892867036426,-15.9877997661728,-23.4468825890607)) ;
#56340 = CARTESIAN_POINT('Ctrl Pts',(16.8244711854299,-15.9979236586406,-23.4268622092806)) ;
#56341 = CARTESIAN_POINT('Ctrl Pts',(16.7594727840492,-16.007708169274,-23.4091024740735)) ;
#56342 = CARTESIAN_POINT('Ctrl Pts',(16.6946209174192,-16.01711893568,-23.3935698503413)) ;
#56343 = CARTESIAN_POINT('Ctrl Pts',(16.641550421604,-16.0248200870133,-23.380858974223)) ;
#56344 = CARTESIAN_POINT('Ctrl Pts',(16.5885782310602,-16.0322710948773,-23.369638506587)) ;
#56345 = CARTESIAN_POINT('Ctrl Pts',(16.5358829682124,-16.0394576303854,-23.3598645671712)) ;
#56346 = CARTESIAN_POINT('Ctrl Pts',(16.4714084257695,-16.0482506141109,-23.3479058020443)) ;
#56347 = CARTESIAN_POINT('Ctrl Pts',(16.4056949428662,-16.056873031955,-23.3378072345523)) ;
#56348 = CARTESIAN_POINT('Ctrl Pts',(16.3390166847862,-16.0652608298866,-23.3297551459858)) ;
#56349 = CARTESIAN_POINT('Ctrl Pts',(16.2728849944109,-16.0735798722809,-23.3217690611166)) ;
#56350 = CARTESIAN_POINT('Ctrl Pts',(16.2058047029135,-16.0816680200509,-23.3157962796076)) ;
#56351 = CARTESIAN_POINT('Ctrl Pts',(16.1380657785028,-16.089467386931,-23.3119728824655)) ;
#56352 = CARTESIAN_POINT('Ctrl Pts',(16.0824043502165,-16.0958761674667,-23.3088311770475)) ;
#56353 = CARTESIAN_POINT('Ctrl Pts',(16.0262987425406,-16.1020900207685,-23.3071399485763)) ;
#56354 = CARTESIAN_POINT('Ctrl Pts',(15.9699181491897,-16.108079933754,-23.3069498505863)) ;
#56355 = CARTESIAN_POINT('Ctrl Pts',(15.8993263329097,-16.1155796568302,-23.3067118367311)) ;
#56356 = CARTESIAN_POINT('Ctrl Pts',(15.8282928832485,-16.1227292229209,-23.3088282327695)) ;
#56357 = CARTESIAN_POINT('Ctrl Pts',(15.7571304872636,-16.1294814162039,-23.3133523951902)) ;
#56358 = CARTESIAN_POINT('Ctrl Pts',(15.686108792268,-16.1362202591736,-23.3178676125195)) ;
#56359 = CARTESIAN_POINT('Ctrl Pts',(15.6149591634837,-16.1425632136361,-23.3247811272778)) ;
#56360 = CARTESIAN_POINT('Ctrl Pts',(15.5439966773993,-16.1484717649153,-23.334094926757)) ;
#56361 = CARTESIAN_POINT('Ctrl Pts',(15.4904799872992,-16.1529277264409,-23.3411189721067)) ;
#56362 = CARTESIAN_POINT('Ctrl Pts',(15.437069872936,-16.1571367885212,-23.3495071199925)) ;
#56363 = CARTESIAN_POINT('Ctrl Pts',(15.3839004251958,-16.1610860188908,-23.3592409423245)) ;
#56364 = CARTESIAN_POINT('Ctrl Pts',(15.3103468359604,-16.1665493080681,-23.3727065245325)) ;
#56365 = CARTESIAN_POINT('Ctrl Pts',(15.2372045689343,-16.171518536629,-23.3887588457374)) ;
#56366 = CARTESIAN_POINT('Ctrl Pts',(15.1648211150739,-16.1759680067789,-23.407308135406)) ;
#56367 = CARTESIAN_POINT('Ctrl Pts',(15.0924376612533,-16.1804174769264,-23.4258574250643)) ;
#56368 = CARTESIAN_POINT('Ctrl Pts',(15.0208136154844,-16.184347145014,-23.4469034617514)) ;
#56369 = CARTESIAN_POINT('Ctrl Pts',(14.9502780403199,-16.1877442734702,-23.4702989581348)) ;
#56370 = CARTESIAN_POINT('',(15.7294621415156,-15.9108618782029,-24.7291481725744)) ;
#56371 = CARTESIAN_POINT('Ctrl Pts',(15.7294621415156,-15.9108618782028,-24.7291481725744)) ;
#56372 = CARTESIAN_POINT('Ctrl Pts',(15.3349248241001,-16.0510971573237,-24.0915044676574)) ;
#56373 = CARTESIAN_POINT('Ctrl Pts',(14.9502780406423,-16.1877442737198,-23.4702989580733)) ;
#56374 = CARTESIAN_POINT('',(14.4806874246062,-15.9108618782029,-25.4805109900364)) ;
#56375 = CARTESIAN_POINT('Origin',(-2.92277791062251E-15,-15.9108618782028,
0.)) ;
#56376 = CARTESIAN_POINT('',(13.7334553913052,-16.1877442736409,-24.2024368542756)) ;
#56377 = CARTESIAN_POINT('Ctrl Pts',(13.7334553911612,-16.1877442737199,-24.2024368544333)) ;
#56378 = CARTESIAN_POINT('Ctrl Pts',(14.102126141797,-16.0510971569896,-24.8332548261164)) ;
#56379 = CARTESIAN_POINT('Ctrl Pts',(14.4806874246063,-15.9108618782028,-25.4805109900364)) ;
#56380 = CARTESIAN_POINT('',(12.751230463362,-15.9108618962294,-26.3884985273164)) ;
#56381 = CARTESIAN_POINT('Ctrl Pts',(13.7334553913666,-16.1877442734702,-24.2024368541772)) ;
#56382 = CARTESIAN_POINT('Ctrl Pts',(13.6797457297494,-16.184347145014,-24.2537972364167)) ;
#56383 = CARTESIAN_POINT('Ctrl Pts',(13.6276019952533,-16.1804174769265,-24.3072198022979)) ;
#56384 = CARTESIAN_POINT('Ctrl Pts',(13.5773084536876,-16.1759680067789,-24.3624828117221)) ;
#56385 = CARTESIAN_POINT('Ctrl Pts',(13.5270149120943,-16.171518536629,-24.4177458211767)) ;
#56386 = CARTESIAN_POINT('Ctrl Pts',(13.4785720377215,-16.166549308068,-24.4748488523071)) ;
#56387 = CARTESIAN_POINT('Ctrl Pts',(13.4322219116136,-16.1610860188908,-24.5335269419437)) ;
#56388 = CARTESIAN_POINT('Ctrl Pts',(13.3878108982001,-16.155851292919,-24.5897501638582)) ;
#56389 = CARTESIAN_POINT('Ctrl Pts',(13.3452922448459,-16.1501596984486,-24.6474554508189)) ;
#56390 = CARTESIAN_POINT('Ctrl Pts',(13.3048448998038,-16.1440425621066,-24.7063835136293)) ;
#56391 = CARTESIAN_POINT('Ctrl Pts',(13.2643139913044,-16.1379127878754,-24.7654333207137)) ;
#56392 = CARTESIAN_POINT('Ctrl Pts',(13.2258632234961,-16.1313557844549,-24.825710522781)) ;
#56393 = CARTESIAN_POINT('Ctrl Pts',(13.1896277877376,-16.1244124680045,-24.8869287440011)) ;
#56394 = CARTESIAN_POINT('Ctrl Pts',(13.1623237886324,-16.1191805644222,-24.9330576844272)) ;
#56395 = CARTESIAN_POINT('Ctrl Pts',(13.1362767125676,-16.1137295207044,-24.9797203506699)) ;
#56396 = CARTESIAN_POINT('Ctrl Pts',(13.1115264539273,-16.1080799337539,-25.0267870706076)) ;
#56397 = CARTESIAN_POINT('Ctrl Pts',(13.0796342162779,-16.1008000918637,-25.0874354476383)) ;
#56398 = CARTESIAN_POINT('Ctrl Pts',(13.0498925978974,-16.0931892946345,-25.1487638518767)) ;
#56399 = CARTESIAN_POINT('Ctrl Pts',(13.0223590317742,-16.0853002129681,-25.210460375078)) ;
#56400 = CARTESIAN_POINT('Ctrl Pts',(12.9946009463867,-16.0773468007023,-25.2726599954059)) ;
#56401 = CARTESIAN_POINT('Ctrl Pts',(12.9690871443112,-16.0691106491233,-25.3352332649269)) ;
#56402 = CARTESIAN_POINT('Ctrl Pts',(12.9458241355485,-16.0606518030571,-25.3978528522157)) ;
#56403 = CARTESIAN_POINT('Ctrl Pts',(12.9267732171505,-16.0537245483847,-25.449134294772)) ;
#56404 = CARTESIAN_POINT('Ctrl Pts',(12.9092308037536,-16.0466480826282,-25.5004465405545)) ;
#56405 = CARTESIAN_POINT('Ctrl Pts',(12.8931745449892,-16.0394576303854,-25.5516095048324)) ;
#56406 = CARTESIAN_POINT('Ctrl Pts',(12.8735361371421,-16.0306629892538,-25.6141869192784)) ;
#56407 = CARTESIAN_POINT('Ctrl Pts',(12.8556186023503,-16.0214720150688,-25.6781462865562)) ;
#56408 = CARTESIAN_POINT('Ctrl Pts',(12.8396425063793,-16.0119118209664,-25.743233371235)) ;
#56409 = CARTESIAN_POINT('Ctrl Pts',(12.823797259159,-16.0024299275613,-25.8077873742565)) ;
#56410 = CARTESIAN_POINT('Ctrl Pts',(12.8098620717459,-15.9925848997546,-25.8734503024339)) ;
#56411 = CARTESIAN_POINT('Ctrl Pts',(12.7980090241213,-15.9824119250016,-25.9399480681732)) ;
#56412 = CARTESIAN_POINT('Ctrl Pts',(12.7882764957844,-15.9740589032142,-25.9945493327509)) ;
#56413 = CARTESIAN_POINT('Ctrl Pts',(12.7799470282373,-15.9654849570549,-26.049712859848)) ;
#56414 = CARTESIAN_POINT('Ctrl Pts',(12.7730919847679,-15.9567135267634,-26.1052766300655)) ;
#56415 = CARTESIAN_POINT('Ctrl Pts',(12.7645041622943,-15.9457249040773,-26.1748854949425)) ;
#56416 = CARTESIAN_POINT('Ctrl Pts',(12.7582302946523,-15.9344245942978,-26.2451330204268)) ;
#56417 = CARTESIAN_POINT('Ctrl Pts',(12.7543621414963,-15.9228603613505,-26.3157156886516)) ;
#56418 = CARTESIAN_POINT('Ctrl Pts',(12.7530344938471,-15.9188912251586,-26.3399414392269)) ;
#56419 = CARTESIAN_POINT('Ctrl Pts',(12.7519898122864,-15.9148910519162,-26.364206566251)) ;
#56420 = CARTESIAN_POINT('Ctrl Pts',(12.7512304249355,-15.9108619321403,-26.3884985240483)) ;
#56421 = CARTESIAN_POINT('',(11.8573408058245,-15.9108618828344,-26.8020561960657)) ;
#56422 = CARTESIAN_POINT('Origin',(-2.92277791062251E-15,-15.9108618782028,
0.)) ;
#56423 = CARTESIAN_POINT('',(9.55532834895734,-16.1877442736409,-26.1354442627971)) ;
#56424 = CARTESIAN_POINT('Ctrl Pts',(11.8573407877332,-15.9108618871751,-26.8020561755759)) ;
#56425 = CARTESIAN_POINT('Ctrl Pts',(11.8019659957108,-15.9226008852454,-26.7579233271853)) ;
#56426 = CARTESIAN_POINT('Ctrl Pts',(11.7451950535357,-15.934093743921,-26.7157870228874)) ;
#56427 = CARTESIAN_POINT('Ctrl Pts',(11.6873103354369,-15.9452906250395,-26.675789507789)) ;
#56428 = CARTESIAN_POINT('Ctrl Pts',(11.6674427673654,-15.949133691139,-26.6620613014505)) ;
#56429 = CARTESIAN_POINT('Ctrl Pts',(11.6474442112849,-15.9529419404769,-26.6485846614785)) ;
#56430 = CARTESIAN_POINT('Ctrl Pts',(11.6273267208508,-15.9567135267634,-26.635364088185)) ;
#56431 = CARTESIAN_POINT('Ctrl Pts',(11.5704227089682,-15.9673817754481,-26.5979685858856)) ;
#56432 = CARTESIAN_POINT('Ctrl Pts',(11.5125574847872,-15.9777576912908,-26.562620016811)) ;
#56433 = CARTESIAN_POINT('Ctrl Pts',(11.4540378943115,-15.9877997661729,-26.5294049013298)) ;
#56434 = CARTESIAN_POINT('Ctrl Pts',(11.3950415167503,-15.9979236586407,-26.4959191664206)) ;
#56435 = CARTESIAN_POINT('Ctrl Pts',(11.335380559969,-16.007708169274,-26.4646019089955)) ;
#56436 = CARTESIAN_POINT('Ctrl Pts',(11.2753839489031,-16.0171189356801,-26.4354911950566)) ;
#56437 = CARTESIAN_POINT('Ctrl Pts',(11.2262866744231,-16.0248200870134,-26.4116689043108)) ;
#56438 = CARTESIAN_POINT('Ctrl Pts',(11.1769650131244,-16.0322710948773,-26.3893233098529)) ;
#56439 = CARTESIAN_POINT('Ctrl Pts',(11.1276028442977,-16.0394576303854,-26.3684499558578)) ;
#56440 = CARTESIAN_POINT('Ctrl Pts',(11.0672064618319,-16.0482506141109,-26.3429106592426)) ;
#56441 = CARTESIAN_POINT('Ctrl Pts',(11.0052002171405,-16.0568730319549,-26.3189217342993)) ;
#56442 = CARTESIAN_POINT('Ctrl Pts',(10.9418118207047,-16.0652608298865,-26.2967240445969)) ;
#56443 = CARTESIAN_POINT('Ctrl Pts',(10.87894302468,-16.0735798722809,-26.274708311362)) ;
#56444 = CARTESIAN_POINT('Ctrl Pts',(10.8147150045907,-16.0816680200509,-26.2544548903729)) ;
#56445 = CARTESIAN_POINT('Ctrl Pts',(10.7493816959561,-16.089467386931,-26.2361590157312)) ;
#56446 = CARTESIAN_POINT('Ctrl Pts',(10.6956969747283,-16.0958761674668,-26.2211251998985)) ;
#56447 = CARTESIAN_POINT('Ctrl Pts',(10.6412666491104,-16.1020900207684,-26.2074124642288)) ;
#56448 = CARTESIAN_POINT('Ctrl Pts',(10.5862450681494,-16.1080799337539,-26.1951066496522)) ;
#56449 = CARTESIAN_POINT('Ctrl Pts',(10.51735481525,-16.11557965683,-26.1796990466079)) ;
#56450 = CARTESIAN_POINT('Ctrl Pts',(10.4475271255812,-16.1227292229206,-26.1664958705399)) ;
#56451 = CARTESIAN_POINT('Ctrl Pts',(10.3770559056829,-16.1294814162034,-26.155616448966)) ;
#56452 = CARTESIAN_POINT('Ctrl Pts',(10.3067240201933,-16.136220259173,-26.1447585379858)) ;
#56453 = CARTESIAN_POINT('Ctrl Pts',(10.2357516288819,-16.1425632136355,-26.1362153515903)) ;
#56454 = CARTESIAN_POINT('Ctrl Pts',(10.1644460147151,-16.1484717649146,-26.1300565627414)) ;
#56455 = CARTESIAN_POINT('Ctrl Pts',(10.1106705529661,-16.1529277264404,-26.1254118833843)) ;
#56456 = CARTESIAN_POINT('Ctrl Pts',(10.0567059335498,-16.157136788521,-26.1221223252373)) ;
#56457 = CARTESIAN_POINT('Ctrl Pts',(10.0026870738765,-16.1610860188908,-26.1201987166258)) ;
#56458 = CARTESIAN_POINT('Ctrl Pts',(9.92795842454788,-16.166549308068,-26.1175376335476)) ;
#56459 = CARTESIAN_POINT('Ctrl Pts',(9.85307540852308,-16.171518536629,-26.1174912350626)) ;
#56460 = CARTESIAN_POINT('Ctrl Pts',(9.77839669062397,-16.1759680067789,-26.1200465497064)) ;
#56461 = CARTESIAN_POINT('Ctrl Pts',(9.70371797276597,-16.1804174769265,-26.1226018643487)) ;
#56462 = CARTESIAN_POINT('Ctrl Pts',(9.62924418161368,-16.184347145014,-26.1277588037449)) ;
#56463 = CARTESIAN_POINT('Ctrl Pts',(9.55532834884255,-16.1877442734701,-26.1354442627804)) ;
#56464 = CARTESIAN_POINT('',(10.0456801889655,-15.9108618782028,-27.532363831381)) ;
#56465 = CARTESIAN_POINT('Ctrl Pts',(10.0456801889651,-15.9108618782028,-27.5323638313812)) ;
#56466 = CARTESIAN_POINT('Ctrl Pts',(9.79744148248229,-16.0510971574616,-26.8248140204399)) ;
#56467 = CARTESIAN_POINT('Ctrl Pts',(9.55532834917085,-16.1877442737199,-26.1354442627893)) ;
#56468 = CARTESIAN_POINT('',(8.66458033535308,-15.9108618782028,-27.9977105530921)) ;
#56469 = CARTESIAN_POINT('Origin',(-2.92277791062251E-15,-15.9108618782028,
0.)) ;
#56470 = CARTESIAN_POINT('',(8.209566331333,-16.1877442736409,-26.5888842812483)) ;
#56471 = CARTESIAN_POINT('Ctrl Pts',(8.20956633115831,-16.1877442737199,-26.5888842813713)) ;
#56472 = CARTESIAN_POINT('Ctrl Pts',(8.43401054640113,-16.0510971576296,-27.2842073897287)) ;
#56473 = CARTESIAN_POINT('Ctrl Pts',(8.66458033535351,-15.9108618782028,-27.997710553092)) ;
#56474 = CARTESIAN_POINT('',(6.78036653080776,-15.9108618828344,-28.5126880007908)) ;
#56475 = CARTESIAN_POINT('Ctrl Pts',(8.20956633141424,-16.1877442734701,-26.5888842811654)) ;
#56476 = CARTESIAN_POINT('Ctrl Pts',(8.14607140785912,-16.184347145014,-26.6274978966082)) ;
#56477 = CARTESIAN_POINT('Ctrl Pts',(8.08366249239415,-16.1804174769265,-26.6684621110277)) ;
#56478 = CARTESIAN_POINT('Ctrl Pts',(8.02266487241838,-16.1759680067789,-26.7116214772316)) ;
#56479 = CARTESIAN_POINT('Ctrl Pts',(7.96166725240905,-16.171518536629,-26.7547808434592)) ;
#56480 = CARTESIAN_POINT('Ctrl Pts',(7.90208148177934,-16.166549308068,-26.8001350514255)) ;
#56481 = CARTESIAN_POINT('Ctrl Pts',(7.84420094110269,-16.1610860188908,-26.8474773729212)) ;
#56482 = CARTESIAN_POINT('Ctrl Pts',(7.78874190173793,-16.155851292919,-26.8928390720476)) ;
#56483 = CARTESIAN_POINT('Ctrl Pts',(7.73481237993059,-16.1501596984485,-26.9400549878379)) ;
#56484 = CARTESIAN_POINT('Ctrl Pts',(7.68264287973525,-16.1440425621065,-26.9889103617178)) ;
#56485 = CARTESIAN_POINT('Ctrl Pts',(7.63036559832969,-16.1379127878753,-27.0378666698851)) ;
#56486 = CARTESIAN_POINT('Ctrl Pts',(7.57985597144212,-16.1313557844548,-27.0884688459826)) ;
#56487 = CARTESIAN_POINT('Ctrl Pts',(7.53130759207052,-16.1244124680044,-27.1404662716341)) ;
#56488 = CARTESIAN_POINT('Ctrl Pts',(7.49472558666167,-16.1191805644222,-27.1796471903599)) ;
#56489 = CARTESIAN_POINT('Ctrl Pts',(7.4592563828573,-16.1137295207043,-27.2196195579886)) ;
#56490 = CARTESIAN_POINT('Ctrl Pts',(7.42496681800598,-16.1080799337539,-27.260265310174)) ;
#56491 = CARTESIAN_POINT('Ctrl Pts',(7.38078259484197,-16.1008000918638,-27.3126398734855)) ;
#56492 = CARTESIAN_POINT('Ctrl Pts',(7.33855252491512,-16.0931892946346,-27.3661408849174)) ;
#56493 = CARTESIAN_POINT('Ctrl Pts',(7.29839974951543,-16.0853002129682,-27.4204760748612)) ;
#56494 = CARTESIAN_POINT('Ctrl Pts',(7.25791955297621,-16.0773468007025,-27.4752543347953)) ;
#56495 = CARTESIAN_POINT('Ctrl Pts',(7.21955084612071,-16.0691106491236,-27.5308799627835)) ;
#56496 = CARTESIAN_POINT('Ctrl Pts',(7.18337035333025,-16.0606518030575,-27.5870346796851)) ;
#56497 = CARTESIAN_POINT('Ctrl Pts',(7.15374084053614,-16.053724548385,-27.6330218062984)) ;
#56498 = CARTESIAN_POINT('Ctrl Pts',(7.12557794295134,-16.0466480826283,-27.6793632999596)) ;
#56499 = CARTESIAN_POINT('Ctrl Pts',(7.09889854564046,-16.0394576303854,-27.7258784815505)) ;
#56500 = CARTESIAN_POINT('Ctrl Pts',(7.06626697852494,-16.0306629892538,-27.7827711936417)) ;
#56501 = CARTESIAN_POINT('Ctrl Pts',(7.03501897240025,-16.0214720150688,-27.8413834861136)) ;
#56502 = CARTESIAN_POINT('Ctrl Pts',(7.00542458942953,-16.0119118209664,-27.9015144825385)) ;
#56503 = CARTESIAN_POINT('Ctrl Pts',(6.97607259283704,-16.0024299275613,-27.9611529890723)) ;
#56504 = CARTESIAN_POINT('Ctrl Pts',(6.94834761378586,-15.9925848997547,-28.0222851011058)) ;
#56505 = CARTESIAN_POINT('Ctrl Pts',(6.92247662985391,-15.9824119250017,-28.0846801311699)) ;
#56506 = CARTESIAN_POINT('Ctrl Pts',(6.90123398473867,-15.9740589032142,-28.1359126426234)) ;
#56507 = CARTESIAN_POINT('Ctrl Pts',(6.88124072781037,-15.965484957055,-28.1879958878066)) ;
#56508 = CARTESIAN_POINT('Ctrl Pts',(6.86260138330431,-15.9567135267634,-28.2407869762416)) ;
#56509 = CARTESIAN_POINT('Ctrl Pts',(6.83925049104925,-15.9457249040898,-28.306922296487)) ;
#56510 = CARTESIAN_POINT('Ctrl Pts',(6.81802216149098,-15.9344245943236,-28.3741787776958)) ;
#56511 = CARTESIAN_POINT('Ctrl Pts',(6.79907125636311,-15.9228603613902,-28.4422797236946)) ;
#56512 = CARTESIAN_POINT('Ctrl Pts',(6.79256680389258,-15.91889121042,-28.4656537717128)) ;
#56513 = CARTESIAN_POINT('Ctrl Pts',(6.78633023914337,-15.9148910221682,-28.4891271056646)) ;
#56514 = CARTESIAN_POINT('Ctrl Pts',(6.78036653281026,-15.9108618871751,-28.5126879735306)) ;
#56515 = CARTESIAN_POINT('',(5.8184729570234,-15.9108618818334,-28.7244167966786)) ;
#56516 = CARTESIAN_POINT('Origin',(-2.92277791062251E-15,-15.9108618782028,
0.)) ;
#56517 = CARTESIAN_POINT('',(3.71358212386679,-16.1877442736409,-27.5785252411991)) ;
#56518 = CARTESIAN_POINT('Ctrl Pts',(5.81847294179667,-15.9108618853164,-28.7244167739446)) ;
#56519 = CARTESIAN_POINT('Ctrl Pts',(5.77388003967716,-15.9226008834119,-28.6694117834359)) ;
#56520 = CARTESIAN_POINT('Ctrl Pts',(5.72749443064539,-15.9340937421156,-28.6160565279039)) ;
#56521 = CARTESIAN_POINT('Ctrl Pts',(5.67956130868255,-15.9452906232646,-28.5645506289581)) ;
#56522 = CARTESIAN_POINT('Ctrl Pts',(5.66310938939528,-15.9491336899665,-28.5468724378123)) ;
#56523 = CARTESIAN_POINT('Ctrl Pts',(5.64647546513558,-15.9529419398963,-28.529411773067)) ;
#56524 = CARTESIAN_POINT('Ctrl Pts',(5.62967034032204,-15.9567135267634,-28.5121756210024)) ;
#56525 = CARTESIAN_POINT('Ctrl Pts',(5.58213564020621,-15.9673817754481,-28.4634217242814)) ;
#56526 = CARTESIAN_POINT('Ctrl Pts',(5.53322217026505,-15.9777576912908,-28.416460272393)) ;
#56527 = CARTESIAN_POINT('Ctrl Pts',(5.48321100329122,-15.9877997661729,-28.3714417257282)) ;
#56528 = CARTESIAN_POINT('Ctrl Pts',(5.43279237142662,-15.9979236586408,-28.3260563914375)) ;
#56529 = CARTESIAN_POINT('Ctrl Pts',(5.38125853927543,-16.0077081692742,-28.2826459719449)) ;
#56530 = CARTESIAN_POINT('Ctrl Pts',(5.3289225586257,-16.0171189356802,-28.2413183524286)) ;
#56531 = CARTESIAN_POINT('Ctrl Pts',(5.28609423946784,-16.0248200870134,-28.2074985508943)) ;
#56532 = CARTESIAN_POINT('Ctrl Pts',(5.24272933347944,-16.0322710948773,-28.175072684776)) ;
#56533 = CARTESIAN_POINT('Ctrl Pts',(5.19900837882614,-16.0394576303854,-28.1440759310355)) ;
#56534 = CARTESIAN_POINT('Ctrl Pts',(5.1455142240551,-16.048250614111,-28.1061502920567)) ;
#56535 = CARTESIAN_POINT('Ctrl Pts',(5.09011456066198,-16.0568730319551,-28.0693927051302)) ;
#56536 = CARTESIAN_POINT('Ctrl Pts',(5.03297999683575,-16.0652608298868,-28.0340873535912)) ;
#56537 = CARTESIAN_POINT('Ctrl Pts',(4.97631377018983,-16.0735798722812,-27.9990714032078)) ;
#56538 = CARTESIAN_POINT('Ctrl Pts',(4.91794125234338,-16.0816680200512,-27.9654843701936)) ;
#56539 = CARTESIAN_POINT('Ctrl Pts',(4.85806847238345,-16.0894673869314,-27.933571512816)) ;
#56540 = CARTESIAN_POINT('Ctrl Pts',(4.80887069611335,-16.0958761674671,-27.9073485510887)) ;
#56541 = CARTESIAN_POINT('Ctrl Pts',(4.75866075408531,-16.1020900207686,-27.8822555005002)) ;
#56542 = CARTESIAN_POINT('Ctrl Pts',(4.70757093348884,-16.108079933754,-27.8584093755501)) ;
#56543 = CARTESIAN_POINT('Ctrl Pts',(4.64360347562769,-16.1155796568301,-27.8285526257106)) ;
#56544 = CARTESIAN_POINT('Ctrl Pts',(4.57824661111033,-16.1227292229208,-27.8006472433746)) ;
#56545 = CARTESIAN_POINT('Ctrl Pts',(4.51176172321611,-16.1294814162036,-27.7748729474675)) ;
#56546 = CARTESIAN_POINT('Ctrl Pts',(4.44540828802764,-16.1362202591733,-27.7491496120273)) ;
#56547 = CARTESIAN_POINT('Ctrl Pts',(4.37793172432457,-16.1425632136358,-27.725549194379)) ;
#56548 = CARTESIAN_POINT('Ctrl Pts',(4.30961715334096,-16.148471764915,-27.7042057953237)) ;
#56549 = CARTESIAN_POINT('Ctrl Pts',(4.25809740077133,-16.1529277264407,-27.6881095713047)) ;
#56550 = CARTESIAN_POINT('Ctrl Pts',(4.20610160193261,-16.1571367885211,-27.6732961232077)) ;
#56551 = CARTESIAN_POINT('Ctrl Pts',(4.15375919217086,-16.1610860188908,-27.6598050294532)) ;
#56552 = CARTESIAN_POINT('Ctrl Pts',(4.08134971133679,-16.166549308068,-27.6411417103761)) ;
#56553 = CARTESIAN_POINT('Ctrl Pts',(4.0082273929161,-16.171518536629,-27.6249987617427)) ;
#56554 = CARTESIAN_POINT('Ctrl Pts',(3.93474530482786,-16.1759680067789,-27.6114406176889)) ;
#56555 = CARTESIAN_POINT('Ctrl Pts',(3.86126321678012,-16.1804174769265,-27.5978824736426)) ;
#56556 = CARTESIAN_POINT('Ctrl Pts',(3.78742199194697,-16.184347145014,-27.5869091829933)) ;
#56557 = CARTESIAN_POINT('Ctrl Pts',(3.71358212375819,-16.1877442734702,-27.578525241158)) ;
#56558 = CARTESIAN_POINT('',(3.8921733957507,-15.9108618782028,-29.0481967574568)) ;
#56559 = CARTESIAN_POINT('Ctrl Pts',(3.89217339575145,-15.9108618782028,-29.0481967574567)) ;
#56560 = CARTESIAN_POINT('Ctrl Pts',(3.80184066662191,-16.0510971574376,-28.3038250840197)) ;
#56561 = CARTESIAN_POINT('Ctrl Pts',(3.71358212407717,-16.1877442737199,-27.5785252412372)) ;
#56562 = CARTESIAN_POINT('',(2.4433270996089,-15.9108618782028,-29.2057682879055)) ;
#56563 = CARTESIAN_POINT('Origin',(-2.92277791062251E-15,-15.9108618782028,
0.)) ;
#56564 = CARTESIAN_POINT('',(2.30180707398557,-16.187744273641,-27.7320650306519)) ;
#56565 = CARTESIAN_POINT('Ctrl Pts',(2.30180707378832,-16.1877442737199,-27.7320650307344)) ;
#56566 = CARTESIAN_POINT('Ctrl Pts',(2.37152999322547,-16.0510971577989,-28.4593807420696)) ;
#56567 = CARTESIAN_POINT('Ctrl Pts',(2.44332709960815,-15.9108618782028,-29.2057682879056)) ;
#56568 = CARTESIAN_POINT('',(0.492460230914681,-15.9108618818334,-29.3036555873477)) ;
#56569 = CARTESIAN_POINT('Ctrl Pts',(2.30180707408278,-16.1877442734702,-27.7320650305885)) ;
#56570 = CARTESIAN_POINT('Ctrl Pts',(2.23149584064573,-16.184347145014,-27.7561263494924)) ;
#56571 = CARTESIAN_POINT('Ctrl Pts',(2.16173991573636,-16.1804174769264,-27.7827167713124)) ;
#56572 = CARTESIAN_POINT('Ctrl Pts',(2.09289039826652,-16.1759680067789,-27.8117544103006)) ;
#56573 = CARTESIAN_POINT('Ctrl Pts',(2.02404088075871,-16.171518536629,-27.8407920493047)) ;
#56574 = CARTESIAN_POINT('Ctrl Pts',(1.95609837828191,-16.166549308068,-27.87227672175)) ;
#56575 = CARTESIAN_POINT('Ctrl Pts',(1.88939385278888,-16.1610860188908,-27.9060696007688)) ;
#56576 = CARTESIAN_POINT('Ctrl Pts',(1.82547999051558,-16.155851292919,-27.9384487144716)) ;
#56577 = CARTESIAN_POINT('Ctrl Pts',(1.76266128475666,-16.1501596984486,-27.9729674953457)) ;
#56578 = CARTESIAN_POINT('Ctrl Pts',(1.7012090172553,-16.1440425621066,-28.009465757311)) ;
#56579 = CARTESIAN_POINT('Ctrl Pts',(1.63962979052034,-16.1379127878754,-28.0460394240019)) ;
#56580 = CARTESIAN_POINT('Ctrl Pts',(1.57942307856946,-16.1313557844549,-28.0846004726154)) ;
#56581 = CARTESIAN_POINT('Ctrl Pts',(1.52083182384675,-16.1244124680045,-28.1249457608655)) ;
#56582 = CARTESIAN_POINT('Ctrl Pts',(1.47668234604868,-16.1191805644222,-28.1553466016784)) ;
#56583 = CARTESIAN_POINT('Ctrl Pts',(1.43344951505291,-16.1137295207044,-28.1867596072095)) ;
#56584 = CARTESIAN_POINT('Ctrl Pts',(1.39122398593246,-16.1080799337539,-28.2190838414456)) ;
#56585 = CARTESIAN_POINT('Ctrl Pts',(1.33681378242112,-16.1008000918637,-28.2607356146682)) ;
#56586 = CARTESIAN_POINT('Ctrl Pts',(1.28406989208191,-16.0931892946345,-28.3039075854619)) ;
#56587 = CARTESIAN_POINT('Ctrl Pts',(1.23317540655631,-16.0853002129681,-28.3483407890563)) ;
#56588 = CARTESIAN_POINT('Ctrl Pts',(1.18186590786466,-16.0773468007023,-28.3931363180443)) ;
#56589 = CARTESIAN_POINT('Ctrl Pts',(1.13243637431771,-16.0691106491233,-28.4392133119591)) ;
#56590 = CARTESIAN_POINT('Ctrl Pts',(1.08503015713038,-16.0606518030572,-28.4862774263233)) ;
#56591 = CARTESIAN_POINT('Ctrl Pts',(1.0462074930285,-16.0537245483848,-28.5248199300628)) ;
#56592 = CARTESIAN_POINT('Ctrl Pts',(1.008740977047,-16.0466480826282,-28.5640237948626)) ;
#56593 = CARTESIAN_POINT('Ctrl Pts',(0.972685940156643,-16.0394576303854,
-28.6037161955719)) ;
#56594 = CARTESIAN_POINT('Ctrl Pts',(0.928587029583222,-16.0306629892537,
-28.652263965323)) ;
#56595 = CARTESIAN_POINT('Ctrl Pts',(0.885469674162133,-16.0214720150687,
-28.7027885373364)) ;
#56596 = CARTESIAN_POINT('Ctrl Pts',(0.843640804647336,-16.0119118209662,
-28.7551517869456)) ;
#56597 = CARTESIAN_POINT('Ctrl Pts',(0.802154525420636,-16.002429927561,-28.8070861667102)) ;
#56598 = CARTESIAN_POINT('Ctrl Pts',(0.761936143937485,-15.9925848997543,
-28.860828992985)) ;
#56599 = CARTESIAN_POINT('Ctrl Pts',(0.723256922153069,-15.9824119250012,
-28.9162037651156)) ;
#56600 = CARTESIAN_POINT('Ctrl Pts',(0.691497442736168,-15.9740589032139,
-28.9616719481493)) ;
#56601 = CARTESIAN_POINT('Ctrl Pts',(0.660775258900229,-15.9654849570548,
-29.0082395567595)) ;
#56602 = CARTESIAN_POINT('Ctrl Pts',(0.631223168391031,-15.9567135267634,
-29.055789510789)) ;
#56603 = CARTESIAN_POINT('Ctrl Pts',(0.59420106811579,-15.9457249040904,-29.1153588724087)) ;
#56604 = CARTESIAN_POINT('Ctrl Pts',(0.559010889735018,-15.9344245943247,
-29.1764794711086)) ;
#56605 = CARTESIAN_POINT('Ctrl Pts',(0.525863355899135,-15.9228603613919,
-29.2389143704133)) ;
#56606 = CARTESIAN_POINT('Ctrl Pts',(0.514486242769484,-15.9188912098108,
-29.2603436844656)) ;
#56607 = CARTESIAN_POINT('Ctrl Pts',(0.503349410828287,-15.9148910209385,
-29.2819275511905)) ;
#56608 = CARTESIAN_POINT('Ctrl Pts',(0.492460240898269,-15.9108618853164,
-29.3036555618719)) ;
#56609 = CARTESIAN_POINT('Origin',(-2.92277791062251E-15,-15.9108618782028,
0.)) ;
#56610 = CARTESIAN_POINT('Origin',(-1.76151330856832E-15,-9.58923182202279,
0.)) ;
#56611 = CARTESIAN_POINT('',(1.01645642765342E-15,-2.97427793106409,-25.5228270052942)) ;
#56612 = CARTESIAN_POINT('',(-1.30824146500192E-16,-9.58923182202279,-26.6311750163962)) ;
#56613 = CARTESIAN_POINT('',(2.75950304786523,-2.97427793637248,-25.3732110958861)) ;
#56614 = CARTESIAN_POINT('Origin',(-5.46365993374796E-16,-2.97427793741672,
0.)) ;
#56615 = CARTESIAN_POINT('',(2.98582626636667,-16.2025431678319,-27.5780838874313)) ;
#56616 = CARTESIAN_POINT('Ctrl Pts',(2.98582626636861,-16.2025431678318,-27.5780838874311)) ;
#56617 = CARTESIAN_POINT('Ctrl Pts',(2.98552181236654,-16.1852171611512,-27.5751968800475)) ;
#56618 = CARTESIAN_POINT('Ctrl Pts',(2.98521730416944,-16.167887657688,-27.5723092892116)) ;
#56619 = CARTESIAN_POINT('Ctrl Pts',(2.9479315159664,-14.0459096732034,-27.2187269791237)) ;
#56620 = CARTESIAN_POINT('Ctrl Pts',(2.90606163823145,-11.6569178621466,-26.8206408073361)) ;
#56621 = CARTESIAN_POINT('Ctrl Pts',(2.86542833808716,-9.31987893565106,-26.4311762695601)) ;
#56622 = CARTESIAN_POINT('Ctrl Pts',(2.83991825733066,-7.8564133077769,-26.1872986972926)) ;
#56623 = CARTESIAN_POINT('Ctrl Pts',(2.7972066419062,-5.36133051494367,-25.7714235433997)) ;
#56624 = CARTESIAN_POINT('Ctrl Pts',(2.7799975101858,-4.34397548535831,-25.6018305106833)) ;
#56625 = CARTESIAN_POINT('Ctrl Pts',(2.76445921051843,-3.37503715194868,-25.4402158918861)) ;
#56626 = CARTESIAN_POINT('Ctrl Pts',(2.76096814266673,-3.14436060309406,-25.4017174269074)) ;
#56627 = CARTESIAN_POINT('Ctrl Pts',(2.75967493119254,-3.02949077923723,-25.3824979545439)) ;
#56628 = CARTESIAN_POINT('Ctrl Pts',(2.75955256053887,-3.01786690009984,-25.3805521788679)) ;
#56629 = CARTESIAN_POINT('Ctrl Pts',(2.75941568018604,-3.00170199339844,-25.3778426381123)) ;
#56630 = CARTESIAN_POINT('Ctrl Pts',(2.75936689772594,-2.99510037673092,-25.3767353094954)) ;
#56631 = CARTESIAN_POINT('Ctrl Pts',(2.75933336756686,-2.98631509723413,-25.375258288366)) ;
#56632 = CARTESIAN_POINT('Ctrl Pts',(2.75931662463871,-2.98020409896568,-25.3742301638833)) ;
#56633 = CARTESIAN_POINT('Ctrl Pts',(2.75939097519427,-2.97566130081685,-25.3734564362549)) ;
#56634 = CARTESIAN_POINT('Ctrl Pts',(2.7594225130813,-2.97461345302792,-25.3732764024227)) ;
#56635 = CARTESIAN_POINT('Ctrl Pts',(2.7594800824429,-2.97437347879031,-25.3732296962218)) ;
#56636 = CARTESIAN_POINT('Ctrl Pts',(2.75949154295653,-2.97432570636421,-25.3732203982688)) ;
#56637 = CARTESIAN_POINT('Ctrl Pts',(2.75950300346898,-2.97427793394,-25.3732111003045)) ;
#56638 = CARTESIAN_POINT('',(3.01245352594498,-16.2025431678319,-27.5751879984371)) ;
#56639 = CARTESIAN_POINT('Origin',(-0.0970287445296982,-21.5586464785792,
0.892164572691303)) ;
#56640 = CARTESIAN_POINT('Ctrl Pts',(2.75950309456866,-2.97427793462802,-25.3732110905128)) ;
#56641 = CARTESIAN_POINT('Ctrl Pts',(2.75951141791194,-2.97432669170439,-25.3732184027943)) ;
#56642 = CARTESIAN_POINT('Ctrl Pts',(2.75951974125522,-2.97437544878077,-25.3732257150757)) ;
#56643 = CARTESIAN_POINT('Ctrl Pts',(2.75988939774605,-2.97654084904765,-25.3735504682689)) ;
#56644 = CARTESIAN_POINT('Ctrl Pts',(2.76054593631754,-3.00035443887309,-25.3774925990095)) ;
#56645 = CARTESIAN_POINT('Ctrl Pts',(2.76768271304796,-3.25662181914454,-25.4199076371643)) ;
#56646 = CARTESIAN_POINT('Ctrl Pts',(2.80101276140845,-4.98861101441761,-25.708191593734)) ;
#56647 = CARTESIAN_POINT('Ctrl Pts',(2.85987603015594,-8.03277302580515,-26.2148517658915)) ;
#56648 = CARTESIAN_POINT('Ctrl Pts',(2.96783636940418,-13.8113507317231,-27.177029718695)) ;
#56649 = CARTESIAN_POINT('Ctrl Pts',(3.01245352594286,-16.2025431678266,-27.5751879984364)) ;
#56650 = CARTESIAN_POINT('',(8.14947771659192,-2.97427793708563,-24.1867879500451)) ;
#56651 = CARTESIAN_POINT('Origin',(-5.46365993374796E-16,-2.97427793741672,
0.)) ;
#56652 = CARTESIAN_POINT('',(8.84449214097205,-16.2025431678319,-26.2914592246876)) ;
#56653 = CARTESIAN_POINT('Ctrl Pts',(8.8444921409701,-16.2025431678318,-26.2914592246882)) ;
#56654 = CARTESIAN_POINT('Ctrl Pts',(8.84368137315711,-16.1872403113959,-26.2890267531794)) ;
#56655 = CARTESIAN_POINT('Ctrl Pts',(8.84287052996823,-16.1719359305085,-26.2865940375341)) ;
#56656 = CARTESIAN_POINT('Ctrl Pts',(8.73054679496111,-14.051850633938,-25.9495945481204)) ;
#56657 = CARTESIAN_POINT('Ctrl Pts',(8.60409127671067,-11.6630949900927,-25.5698538329076)) ;
#56658 = CARTESIAN_POINT('Ctrl Pts',(8.48066779311721,-9.32575037806886,-25.1981813327223)) ;
#56659 = CARTESIAN_POINT('Ctrl Pts',(8.40325559611451,-7.86092828798006,-24.9652738433449)) ;
#56660 = CARTESIAN_POINT('Ctrl Pts',(8.27203747702655,-5.36388181438923,-24.5679912751739)) ;
#56661 = CARTESIAN_POINT('Ctrl Pts',(8.21874191386539,-4.34594047228758,-24.4059695641208)) ;
#56662 = CARTESIAN_POINT('Ctrl Pts',(8.1687574984097,-3.37573518131635,-24.2512722575224)) ;
#56663 = CARTESIAN_POINT('Ctrl Pts',(8.15704769885815,-3.14458998495216,-24.2143496755378)) ;
#56664 = CARTESIAN_POINT('Ctrl Pts',(8.15164435056689,-3.02954097345787,-24.1958288135939)) ;
#56665 = CARTESIAN_POINT('Ctrl Pts',(8.15110606607062,-3.01790731507202,-24.1939532713909)) ;
#56666 = CARTESIAN_POINT('Ctrl Pts',(8.15038939015159,-3.00173216030816,-24.1913348682466)) ;
#56667 = CARTESIAN_POINT('Ctrl Pts',(8.15010371261148,-2.9951315069744,-24.1902640829975)) ;
#56668 = CARTESIAN_POINT('Ctrl Pts',(8.14975280318563,-2.98633297379899,-24.1888266765532)) ;
#56669 = CARTESIAN_POINT('Ctrl Pts',(8.14951604066345,-2.98023844423496,-24.187828896103)) ;
#56670 = CARTESIAN_POINT('Ctrl Pts',(8.14942093279696,-2.97566575016659,-24.1870524576967)) ;
#56671 = CARTESIAN_POINT('Ctrl Pts',(8.14941248312575,-2.9745868821094,-24.1868645533682)) ;
#56672 = CARTESIAN_POINT('Ctrl Pts',(8.14945763957049,-2.97437302162435,-24.1868115263829)) ;
#56673 = CARTESIAN_POINT('Ctrl Pts',(8.14946767807719,-2.97432547935386,-24.1867997382152)) ;
#56674 = CARTESIAN_POINT('Ctrl Pts',(8.14947771658388,-2.97427793708336,-24.1867879500474)) ;
#56675 = CARTESIAN_POINT('',(8.86987433948411,-16.2025431678319,-26.2829069662563)) ;
#56676 = CARTESIAN_POINT('Origin',(-0.286549277334569,-21.5586464785792,0.850447948841961)) ;
#56677 = CARTESIAN_POINT('Ctrl Pts',(8.14947771672321,-2.97427793642345,-24.1867879498838)) ;
#56678 = CARTESIAN_POINT('Ctrl Pts',(8.14949133329423,-2.97432588904375,-24.1867918402822)) ;
#56679 = CARTESIAN_POINT('Ctrl Pts',(8.14950494986526,-2.97437384166406,-24.1867957306806)) ;
#56680 = CARTESIAN_POINT('Ctrl Pts',(8.14976489484414,-2.97528927351905,-24.1868699997108)) ;
#56681 = CARTESIAN_POINT('Ctrl Pts',(8.15057001316975,-2.98748334132594,-24.1887547193953)) ;
#56682 = CARTESIAN_POINT('Ctrl Pts',(8.1554153766091,-3.05983249654133,-24.1999139580347)) ;
#56683 = CARTESIAN_POINT('Ctrl Pts',(8.17321910187599,-3.37814096324511,-24.250194325778)) ;
#56684 = CARTESIAN_POINT('Ctrl Pts',(8.25150376159725,-4.77686335530337,-24.4711209579954)) ;
#56685 = CARTESIAN_POINT('Ctrl Pts',(8.51332551264261,-9.61051733687626,-25.2375264361977)) ;
#56686 = CARTESIAN_POINT('Ctrl Pts',(8.64483231029231,-12.0381142500592,-25.6224325826173)) ;
#56687 = CARTESIAN_POINT('Ctrl Pts',(8.76313990580416,-14.2266207751237,-25.9695132217007)) ;
#56688 = CARTESIAN_POINT('Ctrl Pts',(8.86987433948527,-16.2025431678314,-26.2829069662558)) ;
#56689 = CARTESIAN_POINT('',(13.15839190919,-2.97427793741672,-21.8694174764822)) ;
#56690 = CARTESIAN_POINT('Origin',(-5.46365993374796E-16,-2.97427793741672,
0.)) ;
#56691 = CARTESIAN_POINT('',(14.2895993930077,-16.2025431678318,-23.7754751494576)) ;
#56692 = CARTESIAN_POINT('Ctrl Pts',(14.2895993930102,-16.2025431678314,-23.7754751494561)) ;
#56693 = CARTESIAN_POINT('Ctrl Pts',(14.288479812531,-16.1895116831815,-23.7736005749326)) ;
#56694 = CARTESIAN_POINT('Ctrl Pts',(14.287359600215,-16.176472803045,-23.7717249344438)) ;
#56695 = CARTESIAN_POINT('Ctrl Pts',(14.1053987293089,-14.0585050844697,-23.4670553231882)) ;
#56696 = CARTESIAN_POINT('Ctrl Pts',(13.9002890366153,-11.6700134946164,-23.1234150926258)) ;
#56697 = CARTESIAN_POINT('Ctrl Pts',(13.6998225204247,-9.33232681203563,-22.7869156532154)) ;
#56698 = CARTESIAN_POINT('Ctrl Pts',(13.5740212516687,-7.86598567644115,-22.5758763480535)) ;
#56699 = CARTESIAN_POINT('Ctrl Pts',(13.3602778229174,-5.36674011566134,-22.2157738106669)) ;
#56700 = CARTESIAN_POINT('Ctrl Pts',(13.2733417726211,-4.34814220965037,-22.0689027346577)) ;
#56701 = CARTESIAN_POINT('Ctrl Pts',(13.1911487884526,-3.37651773132946,-21.9283631278092)) ;
#56702 = CARTESIAN_POINT('Ctrl Pts',(13.1717308858037,-3.1448473048907,-21.8947451711901)) ;
#56703 = CARTESIAN_POINT('Ctrl Pts',(13.16245590613,-3.02959726689373,-21.8777895079707)) ;
#56704 = CARTESIAN_POINT('Ctrl Pts',(13.1615260986429,-3.01795254848073,-21.876071921995)) ;
#56705 = CARTESIAN_POINT('Ctrl Pts',(13.1602624142991,-3.00176697334617,-21.8736672944438)) ;
#56706 = CARTESIAN_POINT('Ctrl Pts',(13.1597534264871,-2.99516934250607,-21.8726834277241)) ;
#56707 = CARTESIAN_POINT('Ctrl Pts',(13.1591004799476,-2.98635587386225,-21.8713528885411)) ;
#56708 = CARTESIAN_POINT('Ctrl Pts',(13.1586561623224,-2.98028108276681,-21.8704323482376)) ;
#56709 = CARTESIAN_POINT('Ctrl Pts',(13.1584155616641,-2.97606013386572,-21.8697517396796)) ;
#56710 = CARTESIAN_POINT('Ctrl Pts',(13.1582567494634,-2.97516487197257,-21.8696722323615)) ;
#56711 = CARTESIAN_POINT('Ctrl Pts',(13.1583774170714,-2.97437303709565,-21.8694447921021)) ;
#56712 = CARTESIAN_POINT('Ctrl Pts',(13.1583846631407,-2.97432548753967,-21.8694311343495)) ;
#56713 = CARTESIAN_POINT('Ctrl Pts',(13.1583919092032,-2.97427793798588,-21.8694174765856)) ;
#56714 = CARTESIAN_POINT('',(14.3125496870687,-16.2025431678319,-23.7616664156855)) ;
#56715 = CARTESIAN_POINT('Origin',(-0.46267108440793,-21.5586464785791,0.768965324109772)) ;
#56716 = CARTESIAN_POINT('Ctrl Pts',(13.1583919092032,-2.97427793798589,-21.8694174765856)) ;
#56717 = CARTESIAN_POINT('Ctrl Pts',(13.1584053694963,-2.97432607419128,-21.8694187904502)) ;
#56718 = CARTESIAN_POINT('Ctrl Pts',(13.1584188297894,-2.97437421039667,-21.8694201043147)) ;
#56719 = CARTESIAN_POINT('Ctrl Pts',(13.1586774926046,-2.97529923084781,-21.8694453524952)) ;
#56720 = CARTESIAN_POINT('Ctrl Pts',(13.1597050744733,-2.98568920246521,-21.8708587537663)) ;
#56721 = CARTESIAN_POINT('Ctrl Pts',(13.1706903685768,-3.09726433021604,-21.8860667553059)) ;
#56722 = CARTESIAN_POINT('Ctrl Pts',(13.2279185476989,-3.74807332618725,-21.9788942538091)) ;
#56723 = CARTESIAN_POINT('Ctrl Pts',(13.4698566107615,-6.49929376644458,-22.3713043467384)) ;
#56724 = CARTESIAN_POINT('Ctrl Pts',(14.2415308001386,-15.3848269920527,-23.6444991319492)) ;
#56725 = CARTESIAN_POINT('Ctrl Pts',(14.3125496870575,-16.2025431677232,-23.761666415671)) ;
#56726 = CARTESIAN_POINT('',(17.5520343204297,-2.97427793976807,-18.5294573485322)) ;
#56727 = CARTESIAN_POINT('Origin',(-5.46365993374796E-16,-2.97427793741672,
0.)) ;
#56728 = CARTESIAN_POINT('',(19.0665408591787,-16.2025431678318,-20.1477762807808)) ;
#56729 = CARTESIAN_POINT('Ctrl Pts',(19.0665408591778,-16.2025431678318,-20.1477762807817)) ;
#56730 = CARTESIAN_POINT('Ctrl Pts',(19.0652008544727,-16.190873531221,-20.1463523789925)) ;
#56731 = CARTESIAN_POINT('Ctrl Pts',(19.0638614007779,-16.1792086722493,-20.1449290578845)) ;
#56732 = CARTESIAN_POINT('Ctrl Pts',(18.8208071414155,-14.0625257526841,-19.886655527428)) ;
#56733 = CARTESIAN_POINT('Ctrl Pts',(18.5466384510028,-11.6741934639051,-19.5951615140958)) ;
#56734 = CARTESIAN_POINT('Ctrl Pts',(18.2784972693573,-9.33630026618093,-19.3095987195106)) ;
#56735 = CARTESIAN_POINT('Ctrl Pts',(18.1101644799581,-7.86904147552841,-19.1304250740684)) ;
#56736 = CARTESIAN_POINT('Ctrl Pts',(17.8238542141176,-5.36846742573192,-18.8245280395046)) ;
#56737 = CARTESIAN_POINT('Ctrl Pts',(17.7073320841991,-4.34947290227263,-18.6997311217121)) ;
#56738 = CARTESIAN_POINT('Ctrl Pts',(17.5967504477281,-3.37699090265648,-18.580041634387)) ;
#56739 = CARTESIAN_POINT('Ctrl Pts',(17.5705234637249,-3.14500297466746,-18.5513449311427)) ;
#56740 = CARTESIAN_POINT('Ctrl Pts',(17.5578067836975,-3.02963134974649,-18.5367643290789)) ;
#56741 = CARTESIAN_POINT('Ctrl Pts',(17.5565287224273,-3.01797986529181,-18.5352859406662)) ;
#56742 = CARTESIAN_POINT('Ctrl Pts',(17.5547769763625,-3.00178832029484,-18.5332084551072)) ;
#56743 = CARTESIAN_POINT('Ctrl Pts',(17.554068640032,-2.99519322179253,-18.5323573519155)) ;
#56744 = CARTESIAN_POINT('Ctrl Pts',(17.5531439282108,-2.98637087130639,-18.5311971856173)) ;
#56745 = CARTESIAN_POINT('Ctrl Pts',(17.5525133237871,-2.98030797966027,-18.530395278245)) ;
#56746 = CARTESIAN_POINT('Ctrl Pts',(17.5521302611564,-2.97607197580719,-18.5297805121099)) ;
#56747 = CARTESIAN_POINT('Ctrl Pts',(17.5519437475032,-2.97516258420107,-18.5297473096757)) ;
#56748 = CARTESIAN_POINT('Ctrl Pts',(17.5520246374274,-2.97437252356484,-18.5294883496527)) ;
#56749 = CARTESIAN_POINT('Ctrl Pts',(17.5520294791351,-2.97432523401781,-18.5294728494395)) ;
#56750 = CARTESIAN_POINT('Ctrl Pts',(17.5520343208427,-2.97427794447078,-18.5294573492263)) ;
#56751 = CARTESIAN_POINT('',(19.0859861185406,-16.2025431678319,-20.1293567527132)) ;
#56752 = CARTESIAN_POINT('Origin',(-0.617158905796344,-21.5586464785791,0.651526735465783)) ;
#56753 = CARTESIAN_POINT('Ctrl Pts',(17.5520343208427,-2.97427794447078,-18.5294573492263)) ;
#56754 = CARTESIAN_POINT('Ctrl Pts',(17.5520469269176,-2.97432632302893,-18.5294565733482)) ;
#56755 = CARTESIAN_POINT('Ctrl Pts',(17.5520595329925,-2.97437470158707,-18.5294557974702)) ;
#56756 = CARTESIAN_POINT('Ctrl Pts',(17.5526934119907,-2.9768073503034,-18.529416783517)) ;
#56757 = CARTESIAN_POINT('Ctrl Pts',(17.5528034283629,-2.979337953762,-18.529896605461)) ;
#56758 = CARTESIAN_POINT('Ctrl Pts',(17.557220828315,-3.01332285628473,-18.5335555575299)) ;
#56759 = CARTESIAN_POINT('Ctrl Pts',(17.5725224009764,-3.14289186108968,-18.5489642157879)) ;
#56760 = CARTESIAN_POINT('Ctrl Pts',(17.6982486755249,-4.20803765545581,-18.6756937040713)) ;
#56761 = CARTESIAN_POINT('Ctrl Pts',(18.2934730507535,-9.35158026128418,-19.2989393579036)) ;
#56762 = CARTESIAN_POINT('Ctrl Pts',(18.5832196153222,-11.8548215072816,-19.6021969277266)) ;
#56763 = CARTESIAN_POINT('Ctrl Pts',(18.8490355543646,-14.153188423186,-19.8808400851401)) ;
#56764 = CARTESIAN_POINT('Ctrl Pts',(19.0859861185426,-16.2025431678314,-20.1293567527112)) ;
#56765 = CARTESIAN_POINT('',(21.1249631147115,-2.97427793656,-14.323080387656)) ;
#56766 = CARTESIAN_POINT('Origin',(-5.46365993374796E-16,-2.97427793741672,
0.)) ;
#56767 = CARTESIAN_POINT('',(22.9519520657137,-16.2025431678319,-15.5779897858583)) ;
#56768 = CARTESIAN_POINT('Ctrl Pts',(22.9519520657139,-16.2025431678317,-15.5779897858579)) ;
#56769 = CARTESIAN_POINT('Ctrl Pts',(22.9502335499534,-16.1901238028483,-15.5768164009677)) ;
#56770 = CARTESIAN_POINT('Ctrl Pts',(22.948514579347,-16.1777011355868,-15.5756427009756)) ;
#56771 = CARTESIAN_POINT('Ctrl Pts',(22.6555236061391,-14.0603095790929,-15.3755899261384)) ;
#56772 = CARTESIAN_POINT('Ctrl Pts',(22.3250901464934,-11.6718894994608,-15.1498406568082)) ;
#56773 = CARTESIAN_POINT('Ctrl Pts',(22.0018462798773,-9.33411011491888,-14.9286071448455)) ;
#56774 = CARTESIAN_POINT('Ctrl Pts',(21.7990020106076,-7.86735711472142,-14.7898567783282)) ;
#56775 = CARTESIAN_POINT('Ctrl Pts',(21.4537280604868,-5.36751530138658,-14.5527288153069)) ;
#56776 = CARTESIAN_POINT('Ctrl Pts',(21.3131328026182,-4.3487393845648,-14.4559189764242)) ;
#56777 = CARTESIAN_POINT('Ctrl Pts',(21.1794721847679,-3.37673005063584,-14.3628442350099)) ;
#56778 = CARTESIAN_POINT('Ctrl Pts',(21.147713535865,-3.14491714238785,-14.340473172792)) ;
#56779 = CARTESIAN_POINT('Ctrl Pts',(21.132168877764,-3.02961254565857,-14.3289737413805)) ;
#56780 = CARTESIAN_POINT('Ctrl Pts',(21.1306033981186,-3.0179648009679,-14.3278050250569)) ;
#56781 = CARTESIAN_POINT('Ctrl Pts',(21.1284464644897,-3.00177655927346,-14.3261529979161)) ;
#56782 = CARTESIAN_POINT('Ctrl Pts',(21.127571548738,-2.99518006149376,-14.3254739090271)) ;
#56783 = CARTESIAN_POINT('Ctrl Pts',(21.1264197256475,-2.98636260828327,-14.3245401250765)) ;
#56784 = CARTESIAN_POINT('Ctrl Pts',(21.1256306236549,-2.98029306927367,-14.3238918025835)) ;
#56785 = CARTESIAN_POINT('Ctrl Pts',(21.125125531062,-2.97606537332734,-14.3233745101534)) ;
#56786 = CARTESIAN_POINT('Ctrl Pts',(21.1249429849765,-2.9751639433579,-14.3233746085866)) ;
#56787 = CARTESIAN_POINT('Ctrl Pts',(21.1249609586001,-2.97437281839512,-14.3231118962033)) ;
#56788 = CARTESIAN_POINT('Ctrl Pts',(21.1249620364161,-2.97432537736582,-14.3230961422498)) ;
#56789 = CARTESIAN_POINT('Ctrl Pts',(21.1249631142322,-2.97427793633651,-14.3230803882963)) ;
#56790 = CARTESIAN_POINT('',(22.9669830516602,-16.2025431678319,-15.5558207401564)) ;
#56791 = CARTESIAN_POINT('Origin',(-0.742789062672596,-21.5586464785791,0.503623480791383)) ;
#56792 = CARTESIAN_POINT('Ctrl Pts',(21.1249631142997,-2.97427793336231,-14.3230803873086)) ;
#56793 = CARTESIAN_POINT('Ctrl Pts',(21.1249757103847,-2.97432613941351,-14.3230762021838)) ;
#56794 = CARTESIAN_POINT('Ctrl Pts',(21.1249883064698,-2.97437434546471,-14.323072017059)) ;
#56795 = CARTESIAN_POINT('Ctrl Pts',(21.1252387195819,-2.97533269302076,-14.3229888158006)) ;
#56796 = CARTESIAN_POINT('Ctrl Pts',(21.1267571463958,-2.98566592142204,-14.3238344593653)) ;
#56797 = CARTESIAN_POINT('Ctrl Pts',(21.1441719217104,-3.10455043621784,-14.3336445177555)) ;
#56798 = CARTESIAN_POINT('Ctrl Pts',(21.2437508331783,-3.81759438301236,-14.3996676280851)) ;
#56799 = CARTESIAN_POINT('Ctrl Pts',(21.6375804487957,-6.63755433615676,-14.6607579010562)) ;
#56800 = CARTESIAN_POINT('Ctrl Pts',(22.8541348968827,-15.3906124573063,-15.479844027184)) ;
#56801 = CARTESIAN_POINT('Ctrl Pts',(22.9669830516443,-16.2025431677233,-15.5558207401474)) ;
#56802 = CARTESIAN_POINT('',(23.7101121129195,-2.97427793806634,-9.44697210723373)) ;
#56803 = CARTESIAN_POINT('Origin',(-5.46365993374796E-16,-2.97427793741672,
0.)) ;
#56804 = CARTESIAN_POINT('',(25.7641555029171,-16.2025431678319,-10.2797938022428)) ;
#56805 = CARTESIAN_POINT('Ctrl Pts',(25.7641555029177,-16.2025431678319,-10.2797938022413)) ;
#56806 = CARTESIAN_POINT('Ctrl Pts',(25.7618588421009,-16.1877688223624,-10.2788700351982)) ;
#56807 = CARTESIAN_POINT('Ctrl Pts',(25.7595617877488,-16.1729919326657,-10.2779461041504)) ;
#56808 = CARTESIAN_POINT('Ctrl Pts',(25.4300733391726,-14.0533996634013,-10.1454170231319)) ;
#56809 = CARTESIAN_POINT('Ctrl Pts',(25.0587933387861,-11.6647055250785,-9.99596160917884)) ;
#56810 = CARTESIAN_POINT('Ctrl Pts',(24.6956035468433,-9.32728125403024,-9.84940980079011)) ;
#56811 = CARTESIAN_POINT('Ctrl Pts',(24.4679197096846,-7.86210552892475,-9.75760726356454)) ;
#56812 = CARTESIAN_POINT('Ctrl Pts',(24.0800976015277,-5.36454711209344,-9.60038948428051)) ;
#56813 = CARTESIAN_POINT('Ctrl Pts',(23.9220842020473,-4.34645292073481,-9.53610920565715)) ;
#56814 = CARTESIAN_POINT('Ctrl Pts',(23.7717692171093,-3.37591727900287,-9.4740358356347)) ;
#56815 = CARTESIAN_POINT('Ctrl Pts',(23.7360285131927,-3.14464984801546,-9.45904965421893)) ;
#56816 = CARTESIAN_POINT('Ctrl Pts',(23.7184073683066,-3.02955407834925,-9.45117461641968)) ;
#56817 = CARTESIAN_POINT('Ctrl Pts',(23.7166290266303,-3.0179178504392,-9.45037050831506)) ;
#56818 = CARTESIAN_POINT('Ctrl Pts',(23.7141690200475,-3.00174015894501,-9.44922145101896)) ;
#56819 = CARTESIAN_POINT('Ctrl Pts',(23.7131680376703,-2.99514001169015,-9.44874601721026)) ;
#56820 = CARTESIAN_POINT('Ctrl Pts',(23.711844782819,-2.98633794415978,-9.44808267590362)) ;
#56821 = CARTESIAN_POINT('Ctrl Pts',(23.7109317473047,-2.98024818549774,-9.44761755137845)) ;
#56822 = CARTESIAN_POINT('Ctrl Pts',(23.7102769572539,-2.97566596594098,-9.44718670224653)) ;
#56823 = CARTESIAN_POINT('Ctrl Pts',(23.71012721905,-2.97457957456447,-9.44707073648006)) ;
#56824 = CARTESIAN_POINT('Ctrl Pts',(23.7101168677483,-2.97437287975886,-9.44700315107804)) ;
#56825 = CARTESIAN_POINT('Ctrl Pts',(23.7101144904349,-2.97432540956222,-9.44698762919633)) ;
#56826 = CARTESIAN_POINT('Ctrl Pts',(23.7101121131215,-2.97427793936558,-9.44697210731461)) ;
#56827 = CARTESIAN_POINT('',(25.7740693832514,-16.2025431678319,-10.2549118388444)) ;
#56828 = CARTESIAN_POINT('Origin',(-0.833687228529012,-21.5586464785791,0.332171351892473)) ;
#56829 = CARTESIAN_POINT('Ctrl Pts',(23.7101121131215,-2.97427793936557,-9.44697210731464)) ;
#56830 = CARTESIAN_POINT('Ctrl Pts',(23.7101245644293,-2.97432536598929,-9.44696232568401)) ;
#56831 = CARTESIAN_POINT('Ctrl Pts',(23.7101370157242,-2.97437279261535,-9.44695254404822)) ;
#56832 = CARTESIAN_POINT('Ctrl Pts',(23.710141161062,-2.974388582092,-9.4469492875036)) ;
#56833 = CARTESIAN_POINT('Ctrl Pts',(23.7103474475408,-2.97517432156201,-9.44678723047638)) ;
#56834 = CARTESIAN_POINT('Ctrl Pts',(23.7104505646161,-2.976087915043,-9.4469419856964)) ;
#56835 = CARTESIAN_POINT('Ctrl Pts',(23.7105996529263,-2.97697407685809,-9.44696894400583)) ;
#56836 = CARTESIAN_POINT('Ctrl Pts',(23.7106181044487,-2.97708375034319,-9.44697228043005)) ;
#56837 = CARTESIAN_POINT('Ctrl Pts',(23.7106365725645,-2.97719377294972,-9.44697573324589)) ;
#56838 = CARTESIAN_POINT('Ctrl Pts',(23.7106549402653,-2.97730340753796,-9.44697926243895)) ;
#56839 = CARTESIAN_POINT('Ctrl Pts',(23.7122516294942,-2.98683385276827,-9.44728605230987)) ;
#56840 = CARTESIAN_POINT('Ctrl Pts',(23.717151258952,-3.01773210335417,-9.44897572128477)) ;
#56841 = CARTESIAN_POINT('Ctrl Pts',(23.7194721219178,-3.03238727965577,-9.44978480081932)) ;
#56842 = CARTESIAN_POINT('Ctrl Pts',(23.7514418208435,-3.23426114336774,-9.46092980571913)) ;
#56843 = CARTESIAN_POINT('Ctrl Pts',(23.8661184658587,-3.96778714974358,-9.50516074375344)) ;
#56844 = CARTESIAN_POINT('Ctrl Pts',(24.0044670674295,-4.85383245444821,-9.55902094396787)) ;
#56845 = CARTESIAN_POINT('Ctrl Pts',(24.1732653666677,-5.93489101798971,-9.62473545130367)) ;
#56846 = CARTESIAN_POINT('Ctrl Pts',(24.3773019647013,-7.24299428982599,-9.70478555188628)) ;
#56847 = CARTESIAN_POINT('Ctrl Pts',(24.5093215665893,-8.08953550083095,-9.75664790617047)) ;
#56848 = CARTESIAN_POINT('Ctrl Pts',(24.5789706735296,-8.53614220537689,-9.7840087420468)) ;
#56849 = CARTESIAN_POINT('Ctrl Pts',(24.6285750786978,-8.85428404324401,-9.80352538383069)) ;
#56850 = CARTESIAN_POINT('Ctrl Pts',(24.6423854231622,-8.94284901749011,-9.8089550279813)) ;
#56851 = CARTESIAN_POINT('Ctrl Pts',(24.9521304391092,-10.9292266513597,-9.93073368588121)) ;
#56852 = CARTESIAN_POINT('Ctrl Pts',(25.3061682654494,-13.2004672662886,-10.0702956267967)) ;
#56853 = CARTESIAN_POINT('Ctrl Pts',(25.6253338879632,-15.2482357967354,-10.1962203605316)) ;
#56854 = CARTESIAN_POINT('Ctrl Pts',(25.6758923865101,-15.5726194238176,-10.2161678893959)) ;
#56855 = CARTESIAN_POINT('Ctrl Pts',(25.7255757904938,-15.8913954202363,-10.2357733156429)) ;
#56856 = CARTESIAN_POINT('Ctrl Pts',(25.7740693832509,-16.2025431678319,-10.2549118388455)) ;
#56857 = CARTESIAN_POINT('',(25.1866026330875,-2.97427793670427,-4.12913383088527)) ;
#56858 = CARTESIAN_POINT('Origin',(-5.46365993374796E-16,-2.97427793741672,
0.)) ;
#56859 = CARTESIAN_POINT('',(27.3716556636073,-16.2025431678319,-4.50092608560063)) ;
#56860 = CARTESIAN_POINT('Ctrl Pts',(27.3716556636072,-16.202543167832,-4.50092608560152)) ;
#56861 = CARTESIAN_POINT('Ctrl Pts',(27.3688793881231,-16.1857433178334,-4.50046163223941)) ;
#56862 = CARTESIAN_POINT('Ctrl Pts',(27.3661036374749,-16.1689466370182,-4.49999725972657)) ;
#56863 = CARTESIAN_POINT('Ctrl Pts',(27.0155166994629,-14.0474667172661,-4.44134451708904)) ;
#56864 = CARTESIAN_POINT('Ctrl Pts',(26.620749614247,-11.6585368364515,-4.37519069607536)) ;
#56865 = CARTESIAN_POINT('Ctrl Pts',(26.2345972311031,-9.32141776663148,-4.31014806193477)) ;
#56866 = CARTESIAN_POINT('Ctrl Pts',(25.9927255660653,-7.85759660531187,-4.26947436137525)) ;
#56867 = CARTESIAN_POINT('Ctrl Pts',(25.5804974344147,-5.36199912641347,-4.19935656741213)) ;
#56868 = CARTESIAN_POINT('Ctrl Pts',(25.4124567326006,-4.34449041885194,-4.17056329497325)) ;
#56869 = CARTESIAN_POINT('Ctrl Pts',(25.2525211642905,-3.37522003995815,-4.14228952629787)) ;
#56870 = CARTESIAN_POINT('Ctrl Pts',(25.2144717382874,-3.14442068985397,-4.13535037988208)) ;
#56871 = CARTESIAN_POINT('Ctrl Pts',(25.1955991210527,-3.02950392542895,-4.13145320038075)) ;
#56872 = CARTESIAN_POINT('Ctrl Pts',(25.1936911107792,-3.01787749425057,-4.13105048247988)) ;
#56873 = CARTESIAN_POINT('Ctrl Pts',(25.1910432510912,-3.00170978382865,-4.13045741104492)) ;
#56874 = CARTESIAN_POINT('Ctrl Pts',(25.1899632323033,-2.99510816665471,-4.13020818293691)) ;
#56875 = CARTESIAN_POINT('Ctrl Pts',(25.1885305246722,-2.98631952130879,-4.1298452372347)) ;
#56876 = CARTESIAN_POINT('Ctrl Pts',(25.1875359969717,-2.98021222223683,-4.12958648357871)) ;
#56877 = CARTESIAN_POINT('Ctrl Pts',(25.1868092668585,-2.97566275848799,-4.12930762945622)) ;
#56878 = CARTESIAN_POINT('Ctrl Pts',(25.1866429189275,-2.97460667468206,-4.12922855990008)) ;
#56879 = CARTESIAN_POINT('Ctrl Pts',(25.186614318913,-2.97437337060343,-4.12916138794003)) ;
#56880 = CARTESIAN_POINT('Ctrl Pts',(25.1866084692863,-2.9743256524054,-4.12914764911027)) ;
#56881 = CARTESIAN_POINT('Ctrl Pts',(25.186602619648,-2.97427793420933,-4.1291339102786)) ;
#56882 = CARTESIAN_POINT('',(27.3759888763025,-16.2025431678319,-4.47449465746573)) ;
#56883 = CARTESIAN_POINT('Origin',(-0.885603106156239,-21.5586464785792,0.145187259760998)) ;
#56884 = CARTESIAN_POINT('Ctrl Pts',(25.1866026463618,-2.97427793634941,-4.12913374954807)) ;
#56885 = CARTESIAN_POINT('Ctrl Pts',(25.1866118621959,-2.97432675308219,-4.12912809313557)) ;
#56886 = CARTESIAN_POINT('Ctrl Pts',(25.18662107803,-2.97437556981498,-4.12912243672306)) ;
#56887 = CARTESIAN_POINT('Ctrl Pts',(25.1870320563893,-2.97655254268123,-4.12887019008873)) ;
#56888 = CARTESIAN_POINT('Ctrl Pts',(25.1905243613001,-2.9974640474975,-4.12922534632092)) ;
#56889 = CARTESIAN_POINT('Ctrl Pts',(25.2327027816895,-3.25009986877477,-4.13359396024206)) ;
#56890 = CARTESIAN_POINT('Ctrl Pts',(25.5150428575483,-4.95577965796636,-4.17790529570596)) ;
#56891 = CARTESIAN_POINT('Ctrl Pts',(26.0181996523211,-7.99518172117798,-4.25658117072354)) ;
#56892 = CARTESIAN_POINT('Ctrl Pts',(26.9837924566198,-13.8318142714633,-4.41151055827675)) ;
#56893 = CARTESIAN_POINT('Ctrl Pts',(27.3759888763017,-16.2025431678263,-4.47449465746506)) ;
#56894 = CARTESIAN_POINT('',(25.4853955792416,-2.97427793781143,1.38177804637892)) ;
#56895 = CARTESIAN_POINT('Origin',(-5.46365993374796E-16,-2.97427793741672,
0.)) ;
#56896 = CARTESIAN_POINT('',(27.6992876268763,-16.2025431678319,1.48839993237836)) ;
#56897 = CARTESIAN_POINT('Ctrl Pts',(27.6992876268763,-16.2025431678319,1.48839993237756)) ;
#56898 = CARTESIAN_POINT('Ctrl Pts',(27.6963977131487,-16.1852729916106,1.4882527002794)) ;
#56899 = CARTESIAN_POINT('Ctrl Pts',(27.6935087726697,-16.1680086338848,1.48810552502117)) ;
#56900 = CARTESIAN_POINT('Ctrl Pts',(27.3384366271439,-14.0460917074,1.47001749405664)) ;
#56901 = CARTESIAN_POINT('Ctrl Pts',(26.9386687046014,-11.6571071306621,1.44976102534322)) ;
#56902 = CARTESIAN_POINT('Ctrl Pts',(26.5475739404773,-9.32005883264334,1.43027240288789)) ;
#56903 = CARTESIAN_POINT('Ctrl Pts',(26.3026659929641,-7.85655164084812,1.41800263993642)) ;
#56904 = CARTESIAN_POINT('Ctrl Pts',(25.8850783273247,-5.36140867819081,1.39786817314536)) ;
#56905 = CARTESIAN_POINT('Ctrl Pts',(25.7147993278214,-4.34403568258248,1.38986570156608)) ;
#56906 = CARTESIAN_POINT('Ctrl Pts',(25.552574008522,-3.37505853191685,1.38309950148959)) ;
#56907 = CARTESIAN_POINT('Ctrl Pts',(25.5139405992457,-3.14436762797809,1.38169771258376)) ;
#56908 = CARTESIAN_POINT('Ctrl Pts',(25.4946783799856,-3.02949230886718,1.38144689609332)) ;
#56909 = CARTESIAN_POINT('Ctrl Pts',(25.492728784212,-3.01786813878313,1.38143004544643)) ;
#56910 = CARTESIAN_POINT('Ctrl Pts',(25.4900157460364,-3.00170287001805,1.3814400553632)) ;
#56911 = CARTESIAN_POINT('Ctrl Pts',(25.4889073884696,-2.99510118203702,1.38145129303794)) ;
#56912 = CARTESIAN_POINT('Ctrl Pts',(25.4874306594782,-2.98631555202997,1.38149777525331)) ;
#56913 = CARTESIAN_POINT('Ctrl Pts',(25.4864031753873,-2.98020478534521,1.38153671577505)) ;
#56914 = CARTESIAN_POINT('Ctrl Pts',(25.4856345023826,-2.9756613593825,1.38165284654919)) ;
#56915 = CARTESIAN_POINT('Ctrl Pts',(25.4854562944026,-2.97461265172528,1.38169410945281)) ;
#56916 = CARTESIAN_POINT('Ctrl Pts',(25.4854129102212,-2.97437347068115,1.38175405510917)) ;
#56917 = CARTESIAN_POINT('Ctrl Pts',(25.4854042460737,-2.97432570444335,1.38176602670364)) ;
#56918 = CARTESIAN_POINT('Ctrl Pts',(25.4853955819149,-2.97427793820744,1.38177799829751)) ;
#56919 = CARTESIAN_POINT('',(27.6978375557248,-16.2025431678319,1.51514492105661)) ;
#56920 = CARTESIAN_POINT('Origin',(-0.896109166816728,-21.5586464785791,-0.0485856272728391)) ;
#56921 = CARTESIAN_POINT('Ctrl Pts',(25.4853955766927,-2.97427793899426,1.38177809705115)) ;
#56922 = CARTESIAN_POINT('Ctrl Pts',(25.4854033747212,-2.97432678020061,1.38178542694295)) ;
#56923 = CARTESIAN_POINT('Ctrl Pts',(25.4854111727497,-2.97437562140695,1.38179275683474)) ;
#56924 = CARTESIAN_POINT('Ctrl Pts',(25.4861536393221,-2.97902589460994,1.38249065113243)) ;
#56925 = CARTESIAN_POINT('Ctrl Pts',(25.4869504275186,-2.98368443800432,1.38221223700358)) ;
#56926 = CARTESIAN_POINT('Ctrl Pts',(25.4972660985915,-3.04564095439207,1.38369682324666)) ;
#56927 = CARTESIAN_POINT('Ctrl Pts',(25.5376066632687,-3.28698876069824,1.38659344204126)) ;
#56928 = CARTESIAN_POINT('Ctrl Pts',(25.751738340196,-4.56809667345973,1.40200013610528)) ;
#56929 = CARTESIAN_POINT('Ctrl Pts',(26.5774290539577,-9.50442793797728,1.45022142307887)) ;
#56930 = CARTESIAN_POINT('Ctrl Pts',(26.9887013828208,-11.9632015308957,1.47427793563209)) ;
#56931 = CARTESIAN_POINT('Ctrl Pts',(27.3622462521282,-14.1963338960462,1.49585140007546)) ;
#56932 = CARTESIAN_POINT('Ctrl Pts',(27.6978375557247,-16.2025431678314,1.51514492105782)) ;
#56933 = CARTESIAN_POINT('',(24.5925339350698,-2.97427793675404,6.82802848946651)) ;
#56934 = CARTESIAN_POINT('Origin',(-5.46365993374796E-16,-2.97427793741672,
0.)) ;
#56935 = CARTESIAN_POINT('',(22.5497250682996,-2.97427793653627,11.9551076002299)) ;
#56936 = CARTESIAN_POINT('Origin',(-5.46365993374796E-16,-2.97427793741672,
0.)) ;
#56937 = CARTESIAN_POINT('',(24.5142296821797,-16.2025431678319,12.9814641887756)) ;
#56938 = CARTESIAN_POINT('Ctrl Pts',(24.5142296821792,-16.2025431678315,12.9814641887765)) ;
#56939 = CARTESIAN_POINT('Ctrl Pts',(24.5122080448287,-16.1889101644085,12.9804008194301)) ;
#56940 = CARTESIAN_POINT('Ctrl Pts',(24.5101851232767,-16.1752685151775,12.9793367797034)) ;
#56941 = CARTESIAN_POINT('Ctrl Pts',(24.1960275789333,-14.05673727217,12.8140933509909)) ;
#56942 = CARTESIAN_POINT('Ctrl Pts',(23.8417764769763,-11.6681756019773,12.627883389876)) ;
#56943 = CARTESIAN_POINT('Ctrl Pts',(23.4949308862975,-9.33057976211665,12.4459358417275)) ;
#56944 = CARTESIAN_POINT('Ctrl Pts',(23.2774501530511,-7.86464213425622,12.3317760355887)) ;
#56945 = CARTESIAN_POINT('Ctrl Pts',(22.9063904996838,-5.36598072794395,12.1378872505747)) ;
#56946 = CARTESIAN_POINT('Ctrl Pts',(22.7550540299499,-4.34755722511546,12.0590438033061)) ;
#56947 = CARTESIAN_POINT('Ctrl Pts',(22.6103266209746,-3.37630976879788,11.9846094037368)) ;
#56948 = CARTESIAN_POINT('Ctrl Pts',(22.5757274743488,-3.14477890327531,11.9670507629476)) ;
#56949 = CARTESIAN_POINT('Ctrl Pts',(22.5583025731781,-3.0295822976008,11.9587113092107)) ;
#56950 = CARTESIAN_POINT('Ctrl Pts',(22.5565376094953,-3.01794053203936,11.9578760760157)) ;
#56951 = CARTESIAN_POINT('Ctrl Pts',(22.5540684899263,-3.0017576190999,11.9567446344546)) ;
#56952 = CARTESIAN_POINT('Ctrl Pts',(22.5530583529934,-2.99515899568192,11.9562895998487)) ;
#56953 = CARTESIAN_POINT('Ctrl Pts',(22.5516950135079,-2.98634952387366,11.9557099462857)) ;
#56954 = CARTESIAN_POINT('Ctrl Pts',(22.5507509201939,-2.98026930995719,11.9553157774299)) ;
#56955 = CARTESIAN_POINT('Ctrl Pts',(22.5500592500757,-2.9760549690666,11.955112918444)) ;
#56956 = CARTESIAN_POINT('Ctrl Pts',(22.549968984505,-2.97516557803826,11.9549650384074)) ;
#56957 = CARTESIAN_POINT('Ctrl Pts',(22.549751253269,-2.97437322618191,11.955092295629)) ;
#56958 = CARTESIAN_POINT('Ctrl Pts',(22.5497381608798,-2.97432558130056,11.9550999477284)) ;
#56959 = CARTESIAN_POINT('Ctrl Pts',(22.5497250684906,-2.97427793641922,11.9551075998279)) ;
#56960 = CARTESIAN_POINT('',(24.5016837039789,-16.2025431678319,13.0051284140257)) ;
#56961 = CARTESIAN_POINT('Origin',(-0.792886077760343,-21.5586464785791,-0.420361594016718)) ;
#56962 = CARTESIAN_POINT('Ctrl Pts',(22.5497250680389,-2.97427793477537,11.9551076000919)) ;
#56963 = CARTESIAN_POINT('Ctrl Pts',(22.5497269705711,-2.97432600972966,11.9551212081462)) ;
#56964 = CARTESIAN_POINT('Ctrl Pts',(22.5497288731033,-2.97437408468395,11.9551348162005)) ;
#56965 = CARTESIAN_POINT('Ctrl Pts',(22.5497645661837,-2.97527601066585,11.9553901145756)) ;
#56966 = CARTESIAN_POINT('Ctrl Pts',(22.5512523836686,-2.98580920545014,11.9563515605873)) ;
#56967 = CARTESIAN_POINT('Ctrl Pts',(22.5664879099537,-3.09354746925243,11.9661527335954)) ;
#56968 = CARTESIAN_POINT('Ctrl Pts',(22.6569327161989,-3.70814168940487,12.0153986349189)) ;
#56969 = CARTESIAN_POINT('Ctrl Pts',(23.0555175961015,-6.41664653573796,12.2324312219111)) ;
#56970 = CARTESIAN_POINT('Ctrl Pts',(24.3803519333028,-15.3815014745936,12.9402943899549)) ;
#56971 = CARTESIAN_POINT('Ctrl Pts',(24.5016837039635,-16.202543167723,13.0051284140159)) ;
#56972 = CARTESIAN_POINT('',(19.452530284046,-2.97427793908284,16.5231281529567)) ;
#56973 = CARTESIAN_POINT('Origin',(-5.46365993374796E-16,-2.97427793741672,
0.)) ;
#56974 = CARTESIAN_POINT('',(21.1504695437725,-16.2025431678318,17.9477995161824)) ;
#56975 = CARTESIAN_POINT('Ctrl Pts',(21.1504695437711,-16.2025431678318,17.947799516184)) ;
#56976 = CARTESIAN_POINT('Ctrl Pts',(21.148968900584,-16.190824464327,17.9465332633256)) ;
#56977 = CARTESIAN_POINT('Ctrl Pts',(21.1474684155399,-16.1791070126478,17.945267148275)) ;
#56978 = CARTESIAN_POINT('Ctrl Pts',(20.8764086676346,-14.0623748796458,17.7165466823383)) ;
#56979 = CARTESIAN_POINT('Ctrl Pts',(20.5704981887938,-11.674036593923,17.4585606095428)) ;
#56980 = CARTESIAN_POINT('Ctrl Pts',(20.2708383068535,-9.33615114017493,17.2062735872375)) ;
#56981 = CARTESIAN_POINT('Ctrl Pts',(20.082818488219,-7.86892678806865,17.0478916631225)) ;
#56982 = CARTESIAN_POINT('Ctrl Pts',(19.761875934007,-5.3684025943473,16.778567618261)) ;
#56983 = CARTESIAN_POINT('Ctrl Pts',(19.6309555628547,-4.349422954631,16.6689743597236)) ;
#56984 = CARTESIAN_POINT('Ctrl Pts',(19.5054589643214,-3.37697313855551,16.5650382345451)) ;
#56985 = CARTESIAN_POINT('Ctrl Pts',(19.4753859819799,-3.1449971286427,16.5404046002665)) ;
#56986 = CARTESIAN_POINT('Ctrl Pts',(19.4601388940641,-3.02963007022637,16.528496426528)) ;
#56987 = CARTESIAN_POINT('Ctrl Pts',(19.4585935139585,-3.0179788392836,16.527300304782)) ;
#56988 = CARTESIAN_POINT('Ctrl Pts',(19.4564242764873,-3.00178759363925,16.5256636322884)) ;
#56989 = CARTESIAN_POINT('Ctrl Pts',(19.4555360690703,-2.99519247023055,16.5250024107204)) ;
#56990 = CARTESIAN_POINT('Ctrl Pts',(19.4543275962744,-2.98637053452838,16.5241419079155)) ;
#56991 = CARTESIAN_POINT('Ctrl Pts',(19.4534925911232,-2.98030667154562,16.5235555486211)) ;
#56992 = CARTESIAN_POINT('Ctrl Pts',(19.4528580640734,-2.97607130659674,16.5232064063515)) ;
#56993 = CARTESIAN_POINT('Ctrl Pts',(19.4528144225956,-2.97516258009942,16.523022595322)) ;
#56994 = CARTESIAN_POINT('Ctrl Pts',(19.4525606694781,-2.97437254331412,16.5231168652152)) ;
#56995 = CARTESIAN_POINT('Ctrl Pts',(19.4525454769748,-2.97432524286461,16.5231225092668)) ;
#56996 = CARTESIAN_POINT('Ctrl Pts',(19.4525302844714,-2.9742779424151,16.5231281533183)) ;
#56997 = CARTESIAN_POINT('',(21.1331297746478,-16.2025431678318,17.9682134705435)) ;
#56998 = CARTESIAN_POINT('Origin',(-0.683983524963516,-21.5586464785791,-0.580980842721111)) ;
#56999 = CARTESIAN_POINT('Ctrl Pts',(19.4525302844714,-2.9742779424151,16.5231281533183)) ;
#57000 = CARTESIAN_POINT('Ctrl Pts',(19.4525255622681,-2.97432450011737,16.5231457624397)) ;
#57001 = CARTESIAN_POINT('Ctrl Pts',(19.4525208400648,-2.97437105781963,16.5231633715611)) ;
#57002 = CARTESIAN_POINT('Ctrl Pts',(19.4524565452229,-2.9750049610918,16.5234031273721)) ;
#57003 = CARTESIAN_POINT('Ctrl Pts',(19.4526315145313,-2.9757780922962,16.5233972335742)) ;
#57004 = CARTESIAN_POINT('Ctrl Pts',(19.4535415058967,-2.98456713021951,16.5246006215295)) ;
#57005 = CARTESIAN_POINT('Ctrl Pts',(19.4570077244971,-3.01292535222663,16.5278593349976)) ;
#57006 = CARTESIAN_POINT('Ctrl Pts',(19.48457703876,-3.23724786189985,16.5534596918303)) ;
#57007 = CARTESIAN_POINT('Ctrl Pts',(19.5819054214816,-4.00652715930706,16.6379749412941)) ;
#57008 = CARTESIAN_POINT('Ctrl Pts',(19.8512530910474,-6.12954829805385,16.8703386896818)) ;
#57009 = CARTESIAN_POINT('Ctrl Pts',(20.03438465427,-7.56992759765112,17.0275276590373)) ;
#57010 = CARTESIAN_POINT('Ctrl Pts',(20.2755054134284,-9.46557599994605,17.2342758017243)) ;
#57011 = CARTESIAN_POINT('Ctrl Pts',(20.353310307754,-10.076892225596,17.3008930715163)) ;
#57012 = CARTESIAN_POINT('Ctrl Pts',(20.6176064477318,-12.1539254231473,17.5273016927547)) ;
#57013 = CARTESIAN_POINT('Ctrl Pts',(20.8875535671149,-14.2741505136447,17.7582360672092)) ;
#57014 = CARTESIAN_POINT('Ctrl Pts',(21.133129774648,-16.2025431678318,17.9682134705432)) ;
#57015 = CARTESIAN_POINT('',(15.445756803441,-2.97427793744554,20.3185455967131)) ;
#57016 = CARTESIAN_POINT('Origin',(-5.46365993374796E-16,-2.97427793741672,
0.)) ;
#57017 = CARTESIAN_POINT('',(16.7977369565509,-16.2025431678319,22.0749156857653)) ;
#57018 = CARTESIAN_POINT('Ctrl Pts',(16.797736956552,-16.2025431678319,22.0749156857645)) ;
#57019 = CARTESIAN_POINT('Ctrl Pts',(16.7965330820174,-16.1907211336376,22.0733426945111)) ;
#57020 = CARTESIAN_POINT('Ctrl Pts',(16.7953292286977,-16.1788993343194,22.0717697365644)) ;
#57021 = CARTESIAN_POINT('Ctrl Pts',(16.5797648994147,-14.0620696072946,21.7901138157647)) ;
#57022 = CARTESIAN_POINT('Ctrl Pts',(16.3364645751062,-11.6737192459128,21.4723960063734)) ;
#57023 = CARTESIAN_POINT('Ctrl Pts',(16.0980463971873,-9.3358494693627,21.1615914035746)) ;
#57024 = CARTESIAN_POINT('Ctrl Pts',(15.9484768950245,-7.86869477940399,20.9665029328927)) ;
#57025 = CARTESIAN_POINT('Ctrl Pts',(15.6929447704673,-5.36827143841294,20.6344957971552)) ;
#57026 = CARTESIAN_POINT('Ctrl Pts',(15.5886476126233,-4.34932190866538,20.4993247717653)) ;
#57027 = CARTESIAN_POINT('Ctrl Pts',(15.4884348833676,-3.3769371970094,20.3708492157565)) ;
#57028 = CARTESIAN_POINT('Ctrl Pts',(15.4643629708558,-3.14498529561199,20.3403298909891)) ;
#57029 = CARTESIAN_POINT('Ctrl Pts',(15.4520332309067,-3.0296274890746,20.3254236572053)) ;
#57030 = CARTESIAN_POINT('Ctrl Pts',(15.4507811640484,-3.0179767598727,20.3239233549216)) ;
#57031 = CARTESIAN_POINT('Ctrl Pts',(15.44901451832,-3.00178590816239,20.3218586775132)) ;
#57032 = CARTESIAN_POINT('Ctrl Pts',(15.4482891915348,-2.99519054213983,20.3210219470156)) ;
#57033 = CARTESIAN_POINT('Ctrl Pts',(15.4472940203856,-2.98636924589745,20.3199218611091)) ;
#57034 = CARTESIAN_POINT('Ctrl Pts',(15.4466045047521,-2.98030468072635,20.3191696239606)) ;
#57035 = CARTESIAN_POINT('Ctrl Pts',(15.4460599816571,-2.97607045456207,20.3186923930545)) ;
#57036 = CARTESIAN_POINT('Ctrl Pts',(15.4460558392151,-2.97516281294533,20.3185045129636)) ;
#57037 = CARTESIAN_POINT('Ctrl Pts',(15.4457887885214,-2.97437258257387,20.3185412020118)) ;
#57038 = CARTESIAN_POINT('Ctrl Pts',(15.4457727963274,-2.97432526003727,20.3185433991146)) ;
#57039 = CARTESIAN_POINT('Ctrl Pts',(15.4457568041244,-2.97427793750316,20.3185455962057)) ;
#57040 = CARTESIAN_POINT('',(16.7764141848447,-16.2025431678319,22.09112483541)) ;
#57041 = CARTESIAN_POINT('Origin',(-0.54309866273249,-21.5586464785792,-0.714434072933713)) ;
#57042 = CARTESIAN_POINT('Ctrl Pts',(15.4457568041244,-2.97427793750316,20.3185455962057)) ;
#57043 = CARTESIAN_POINT('Ctrl Pts',(15.4457539152905,-2.97432629596546,20.3185579701203)) ;
#57044 = CARTESIAN_POINT('Ctrl Pts',(15.4457510264566,-2.97437465442775,20.3185703440349)) ;
#57045 = CARTESIAN_POINT('Ctrl Pts',(15.445605609725,-2.97680889943481,20.3191932161949)) ;
#57046 = CARTESIAN_POINT('Ctrl Pts',(15.4460664305379,-2.97934517843716,20.3193767133853)) ;
#57047 = CARTESIAN_POINT('Ctrl Pts',(15.4489469102806,-3.01314182309645,20.3243001217788)) ;
#57048 = CARTESIAN_POINT('Ctrl Pts',(15.461523981169,-3.14117529750347,20.341686154419)) ;
#57049 = CARTESIAN_POINT('Ctrl Pts',(15.5658036103066,-4.20201593204481,20.4856872188289)) ;
#57050 = CARTESIAN_POINT('Ctrl Pts',(16.0849048047097,-9.34914178729712,21.1743789821445)) ;
#57051 = CARTESIAN_POINT('Ctrl Pts',(16.3373613204017,-11.853076400732,21.5094631536216)) ;
#57052 = CARTESIAN_POINT('Ctrl Pts',(16.5694362224003,-14.1525004571554,21.816998218385)) ;
#57053 = CARTESIAN_POINT('Ctrl Pts',(16.7764141848436,-16.2025431678314,22.0911248354107)) ;
#57054 = CARTESIAN_POINT('',(10.7167569009779,-2.97427793741672,23.1638904314851)) ;
#57055 = CARTESIAN_POINT('Origin',(-5.46365993374796E-16,-2.97427793741672,
0.)) ;
#57056 = CARTESIAN_POINT('',(11.6595608585889,-16.2025431678318,25.169833332384)) ;
#57057 = CARTESIAN_POINT('Ctrl Pts',(11.6595608585918,-16.2025431678318,25.1698333323826)) ;
#57058 = CARTESIAN_POINT('Ctrl Pts',(11.6585530880691,-16.1883190110886,25.1676735901348)) ;
#57059 = CARTESIAN_POINT('Ctrl Pts',(11.6575457015777,-16.1741003377176,25.1655146825256)) ;
#57060 = CARTESIAN_POINT('Ctrl Pts',(11.5074098720457,-14.0550300026374,24.8437636611566)) ;
#57061 = CARTESIAN_POINT('Ctrl Pts',(11.338077613478,-11.6664005728183,24.4811293179889)) ;
#57062 = CARTESIAN_POINT('Ctrl Pts',(11.1720722581951,-9.32889248177215,24.1263935292874)) ;
#57063 = CARTESIAN_POINT('Ctrl Pts',(11.068051484594,-7.863344578113,23.9039571658016)) ;
#57064 = CARTESIAN_POINT('Ctrl Pts',(10.8900298857863,-5.3652473681901,23.525133601664)) ;
#57065 = CARTESIAN_POINT('Ctrl Pts',(10.8172778670904,-4.34699231213758,23.3708075548896)) ;
#57066 = CARTESIAN_POINT('Ctrl Pts',(10.7471329839059,-3.37610897168059,23.2240208229558)) ;
#57067 = CARTESIAN_POINT('Ctrl Pts',(10.7302245680935,-3.1447128703852,23.1891243965598)) ;
#57068 = CARTESIAN_POINT('Ctrl Pts',(10.7214034046739,-3.02956783168136,23.1719480498592)) ;
#57069 = CARTESIAN_POINT('Ctrl Pts',(10.7205040011658,-3.01792892294217,23.1702154461329)) ;
#57070 = CARTESIAN_POINT('Ctrl Pts',(10.7192232634546,-3.00174867959296,23.1678208698723)) ;
#57071 = CARTESIAN_POINT('Ctrl Pts',(10.7186943984944,-2.99514921220744,23.166847191043)) ;
#57072 = CARTESIAN_POINT('Ctrl Pts',(10.717960123488,-2.98634352741144,23.1655612451486)) ;
#57073 = CARTESIAN_POINT('Ctrl Pts',(10.7174466464294,-2.9802583336125,23.1646753895135)) ;
#57074 = CARTESIAN_POINT('Ctrl Pts',(10.7169801109564,-2.97566543965881,23.1640433166783)) ;
#57075 = CARTESIAN_POINT('Ctrl Pts',(10.7168553875118,-2.97457165285031,23.1638990908922)) ;
#57076 = CARTESIAN_POINT('Ctrl Pts',(10.7167886800643,-2.9743727123176,23.1638932257357)) ;
#57077 = CARTESIAN_POINT('Ctrl Pts',(10.7167727904227,-2.97432532489865,23.1638918286617)) ;
#57078 = CARTESIAN_POINT('Ctrl Pts',(10.7167569007811,-2.9742779374797,23.1638904315878)) ;
#57079 = CARTESIAN_POINT('',(11.6352521133992,-16.2025431678318,25.1810797554983)) ;
#57080 = CARTESIAN_POINT('Origin',(-0.376819110642892,-21.5586464785792,-0.814481159932352)) ;
#57081 = CARTESIAN_POINT('Ctrl Pts',(10.7167569006248,-2.97427793701361,23.1638904315741)) ;
#57082 = CARTESIAN_POINT('Ctrl Pts',(10.7167499840165,-2.97432596370162,23.1639024979641)) ;
#57083 = CARTESIAN_POINT('Ctrl Pts',(10.7167430674081,-2.97437399038964,23.1639145643541)) ;
#57084 = CARTESIAN_POINT('Ctrl Pts',(10.7166124790537,-2.97528075362364,23.1641423826623)) ;
#57085 = CARTESIAN_POINT('Ctrl Pts',(10.717256330779,-2.98644231985364,23.1659050928526)) ;
#57086 = CARTESIAN_POINT('Ctrl Pts',(10.7232995481034,-3.09146650890056,23.1824981979959)) ;
#57087 = CARTESIAN_POINT('Ctrl Pts',(10.7638322197368,-3.68205504702985,23.272777034556)) ;
#57088 = CARTESIAN_POINT('Ctrl Pts',(10.947704709346,-6.36122868516908,23.6823230437698)) ;
#57089 = CARTESIAN_POINT('Ctrl Pts',(11.5777447190413,-15.3793271372196,25.0557078381133)) ;
#57090 = CARTESIAN_POINT('Ctrl Pts',(11.6352521133898,-16.2025431677228,25.1810797554824)) ;
#57091 = CARTESIAN_POINT('',(5.48671463442036,-2.97427793619619,24.9261040060569)) ;
#57092 = CARTESIAN_POINT('Origin',(-5.46365993374796E-16,-2.97427793741672,
0.)) ;
#57093 = CARTESIAN_POINT('',(-5.12525029468365E-8,-2.97427793862301,25.5228270065607)) ;
#57094 = CARTESIAN_POINT('Origin',(-5.46365993374796E-16,-2.97427793741672,
0.)) ;
#57095 = CARTESIAN_POINT('',(0.0133921350610688,-16.2025431678318,27.7392445831865)) ;
#57096 = CARTESIAN_POINT('Ctrl Pts',(0.0133921350608421,-16.2025431678318,
27.7392445831865)) ;
#57097 = CARTESIAN_POINT('Ctrl Pts',(0.0133827205563863,-16.1853207396188,
27.7363589370385)) ;
#57098 = CARTESIAN_POINT('Ctrl Pts',(0.0133732997516836,-16.1680999693416,
27.7334735686804)) ;
#57099 = CARTESIAN_POINT('Ctrl Pts',(0.0122116115369291,-14.0462236600739,
27.3779497062717)) ;
#57100 = CARTESIAN_POINT('Ctrl Pts',(0.0107953830161923,-11.6572443672643,
26.97767230005)) ;
#57101 = CARTESIAN_POINT('Ctrl Pts',(0.00908199061164238,-9.32018928178254,
26.5860948800897)) ;
#57102 = CARTESIAN_POINT('Ctrl Pts',(0.00807469792554111,-7.85665194902709,
26.3408767894379)) ;
#57103 = CARTESIAN_POINT('Ctrl Pts',(0.00557187555144761,-5.36146535513246,
25.9228041835425)) ;
#57104 = CARTESIAN_POINT('Ctrl Pts',(0.0043438896367992,-4.34407933277878,
25.7523394851314)) ;
#57105 = CARTESIAN_POINT('Ctrl Pts',(0.00231744706143683,-3.37507403506501,
25.5899810524667)) ;
#57106 = CARTESIAN_POINT('Ctrl Pts',(0.0016255918363982,-3.14437272175176,
25.551326666984)) ;
#57107 = CARTESIAN_POINT('Ctrl Pts',(0.000833185359603188,-3.02949341768707,
25.5320784508113)) ;
#57108 = CARTESIAN_POINT('Ctrl Pts',(0.000744461577372581,-3.01786903750215,
25.5301307668094)) ;
#57109 = CARTESIAN_POINT('Ctrl Pts',(0.000587585115252702,-3.00170356762241,
25.527422215767)) ;
#57110 = CARTESIAN_POINT('Ctrl Pts',(0.000516359911024086,-2.99510191775345,
25.5263160984832)) ;
#57111 = CARTESIAN_POINT('Ctrl Pts',(0.000389995404236694,-2.9863159414149,
25.52484399371)) ;
#57112 = CARTESIAN_POINT('Ctrl Pts',(0.000295494913282459,-2.98020577737517,
25.5238202256846)) ;
#57113 = CARTESIAN_POINT('Ctrl Pts',(0.000137918756552516,-2.97566162983232,
25.5230588462965)) ;
#57114 = CARTESIAN_POINT('Ctrl Pts',(8.70400132779651E-5,-2.97461210268643,
25.5228829962964)) ;
#57115 = CARTESIAN_POINT('Ctrl Pts',(2.48813437772203E-5,-2.97437346419653,
25.5228430120269)) ;
#57116 = CARTESIAN_POINT('Ctrl Pts',(1.24407261809522E-5,-2.97432570239241,
25.5228350094584)) ;
#57117 = CARTESIAN_POINT('Ctrl Pts',(1.08584684169698E-10,-2.9742779405883,
25.52282700689)) ;
#57118 = CARTESIAN_POINT('',(-0.0133921350595798,-16.2025431678318,27.7392445831865)) ;
#57119 = CARTESIAN_POINT('Origin',(0.,-21.5586464785791,-0.89742531835827)) ;
#57120 = CARTESIAN_POINT('Ctrl Pts',(-1.04424683376919E-7,-2.97427794148292,
25.5228270070399)) ;
#57121 = CARTESIAN_POINT('Ctrl Pts',(-6.9948999599768E-6,-2.97432678358026,
25.5228351906136)) ;
#57122 = CARTESIAN_POINT('Ctrl Pts',(-1.38853752365767E-5,-2.9743756256776,
25.5228433741872)) ;
#57123 = CARTESIAN_POINT('Ctrl Pts',(-0.000671733076929959,-2.97903868013909,
25.5236246766248)) ;
#57124 = CARTESIAN_POINT('Ctrl Pts',(-0.000349894671792411,-2.98370976889989,
25.5244073252225)) ;
#57125 = CARTESIAN_POINT('Ctrl Pts',(-0.00127721170310683,-3.0459772111706,
25.5348403374966)) ;
#57126 = CARTESIAN_POINT('Ctrl Pts',(-0.00198813524755864,-3.28900867603421,
25.5755606587986)) ;
#57127 = CARTESIAN_POINT('Ctrl Pts',(-0.00577579228133441,-4.57301664693183,
25.7906983042822)) ;
#57128 = CARTESIAN_POINT('Ctrl Pts',(-0.00922328543825932,-9.50679819544934,
26.6173615102215)) ;
#57129 = CARTESIAN_POINT('Ctrl Pts',(-0.0109779254506447,-11.9648785601619,
27.0292169145927)) ;
#57130 = CARTESIAN_POINT('Ctrl Pts',(-0.012295824988902,-14.1970078152399,
27.4032138392471)) ;
#57131 = CARTESIAN_POINT('Ctrl Pts',(-0.0133921350608563,-16.2025431678313,
27.7392445831864)) ;
#57132 = CARTESIAN_POINT('',(-5.48671360278494,-2.97427793932974,24.926104233655)) ;
#57133 = CARTESIAN_POINT('Origin',(-5.46365993374796E-16,-2.97427793741672,
0.)) ;
#57134 = CARTESIAN_POINT('',(-5.9500385847868,-16.2025431678319,27.0935953729783)) ;
#57135 = CARTESIAN_POINT('Ctrl Pts',(-5.95003858478663,-16.2025431678314,
27.0935953729783)) ;
#57136 = CARTESIAN_POINT('Ctrl Pts',(-5.93287872287226,-15.7189595649501,
27.0144076436256)) ;
#57137 = CARTESIAN_POINT('Ctrl Pts',(-5.91524350319025,-15.221824220667,26.9329995753094)) ;
#57138 = CARTESIAN_POINT('Ctrl Pts',(-5.84492153936488,-13.2386274094556,
26.6082360433019)) ;
#57139 = CARTESIAN_POINT('Ctrl Pts',(-5.79005095651472,-11.6894126530758,
26.3545265310519)) ;
#57140 = CARTESIAN_POINT('Ctrl Pts',(-5.73090391748631,-10.0154554223458,
26.0803571843471)) ;
#57141 = CARTESIAN_POINT('Ctrl Pts',(-5.72326138326653,-9.79907595711066,
26.0449167916378)) ;
#57142 = CARTESIAN_POINT('Ctrl Pts',(-5.71470558583829,-9.55673624964,26.0052236145411)) ;
#57143 = CARTESIAN_POINT('Ctrl Pts',(-5.71390057186316,-9.53393434274454,
26.0014888551816)) ;
#57144 = CARTESIAN_POINT('Ctrl Pts',(-5.70139110462718,-9.17956028534485,
25.943445032905)) ;
#57145 = CARTESIAN_POINT('Ctrl Pts',(-5.6614752520146,-8.04994044340242,25.7584305573157)) ;
#57146 = CARTESIAN_POINT('Ctrl Pts',(-5.58189130805735,-5.78271924794518,
25.3869777597823)) ;
#57147 = CARTESIAN_POINT('Ctrl Pts',(-5.54324092011608,-4.67645412098992,
25.2056915431067)) ;
#57148 = CARTESIAN_POINT('Ctrl Pts',(-5.51469385636707,-3.84233733089944,
25.0688719125288)) ;
#57149 = CARTESIAN_POINT('Ctrl Pts',(-5.51222100231848,-3.76985007295875,
25.0569801203902)) ;
#57150 = CARTESIAN_POINT('Ctrl Pts',(-5.50324787511175,-3.50579051812552,
25.013652489226)) ;
#57151 = CARTESIAN_POINT('Ctrl Pts',(-5.49776736515089,-3.34217420314569,
24.9867883866358)) ;
#57152 = CARTESIAN_POINT('Ctrl Pts',(-5.49131928366058,-3.14397212208866,
24.9542036358068)) ;
#57153 = CARTESIAN_POINT('Ctrl Pts',(-5.48943105222872,-3.0840140701563,24.9443327026901)) ;
#57154 = CARTESIAN_POINT('Ctrl Pts',(-5.48781659384092,-3.02914875405639,
24.9352752309949)) ;
#57155 = CARTESIAN_POINT('Ctrl Pts',(-5.48742247974211,-3.01553314732883,
24.933026052041)) ;
#57156 = CARTESIAN_POINT('Ctrl Pts',(-5.48690349060606,-2.99517799299728,
24.9296481052891)) ;
#57157 = CARTESIAN_POINT('Ctrl Pts',(-5.48675589318455,-2.99005670072696,
24.9288019711253)) ;
#57158 = CARTESIAN_POINT('Ctrl Pts',(-5.48665234506065,-2.97915009782824,
24.9269535988966)) ;
#57159 = CARTESIAN_POINT('Ctrl Pts',(-5.48668297585237,-2.97671402055501,
24.9265289164305)) ;
#57160 = CARTESIAN_POINT('Ctrl Pts',(-5.48671360402347,-2.97427794328177,
24.9261042337966)) ;
#57161 = CARTESIAN_POINT('',(-5.97619665355032,-16.2025431678318,27.0878375466411)) ;
#57162 = CARTESIAN_POINT('Origin',(0.192919915744003,-21.5586464785792,-0.876444013123368)) ;
#57163 = CARTESIAN_POINT('Ctrl Pts',(-5.48671360403907,-2.97427794326962,
24.9261042338674)) ;
#57164 = CARTESIAN_POINT('Ctrl Pts',(-5.4867544422091,-2.97466563176781,24.9261617575856)) ;
#57165 = CARTESIAN_POINT('Ctrl Pts',(-5.48679114024367,-2.9751949691749,24.9262444942833)) ;
#57166 = CARTESIAN_POINT('Ctrl Pts',(-5.48794225379729,-2.98815252649866,
24.9282141483353)) ;
#57167 = CARTESIAN_POINT('Ctrl Pts',(-5.48820355368734,-3.0009526412213,24.9303526539106)) ;
#57168 = CARTESIAN_POINT('Ctrl Pts',(-5.4917702937201,-3.08233977560006,24.9435305502341)) ;
#57169 = CARTESIAN_POINT('Ctrl Pts',(-5.49591359064664,-3.18658700036627,
24.9605034752394)) ;
#57170 = CARTESIAN_POINT('Ctrl Pts',(-5.50101843278592,-3.31684853906785,
24.9817278336455)) ;
#57171 = CARTESIAN_POINT('Ctrl Pts',(-5.50255804554906,-3.35653277590054,
24.9881972734115)) ;
#57172 = CARTESIAN_POINT('Ctrl Pts',(-5.50440219560687,-3.40414624973906,
24.9959600406285)) ;
#57173 = CARTESIAN_POINT('Ctrl Pts',(-5.5047590081922,-3.41339294985133,24.9974678889237)) ;
#57174 = CARTESIAN_POINT('Ctrl Pts',(-5.54132990195816,-4.36100762295681,
25.1519933426862)) ;
#57175 = CARTESIAN_POINT('Ctrl Pts',(-5.63758587198842,-6.96806954423069,
25.5780803406581)) ;
#57176 = CARTESIAN_POINT('Ctrl Pts',(-5.72482181396427,-9.33961765357979,
25.9657474153764)) ;
#57177 = CARTESIAN_POINT('Ctrl Pts',(-5.74458877632446,-9.87816198815649,
26.0537904891407)) ;
#57178 = CARTESIAN_POINT('Ctrl Pts',(-5.75033083195084,-10.0345661355023,
26.0793596823434)) ;
#57179 = CARTESIAN_POINT('Ctrl Pts',(-5.75109550216058,-10.0553952782751,
26.0827648693305)) ;
#57180 = CARTESIAN_POINT('Ctrl Pts',(-5.82459880453683,-12.0576523218942,
26.4100981603903)) ;
#57181 = CARTESIAN_POINT('Ctrl Pts',(-5.90433700445679,-14.2366140340412,
26.7663749738318)) ;
#57182 = CARTESIAN_POINT('Ctrl Pts',(-5.97619665355194,-16.2025431678313,
27.0878375466407)) ;
#57183 = CARTESIAN_POINT('',(-10.716756900978,-2.97427793741671,23.1638904314851)) ;
#57184 = CARTESIAN_POINT('Origin',(-5.46365993374796E-16,-2.97427793741672,
0.)) ;
#57185 = CARTESIAN_POINT('',(-11.6352521133983,-16.2025431678318,25.1810797554987)) ;
#57186 = CARTESIAN_POINT('Ctrl Pts',(-11.6352521133968,-16.2025431678318,
25.1810797554994)) ;
#57187 = CARTESIAN_POINT('Ctrl Pts',(-11.6342584581205,-16.1883190325504,
25.1789134868053)) ;
#57188 = CARTESIAN_POINT('Ctrl Pts',(-11.6332651881032,-16.1741003483714,
25.1767480462244)) ;
#57189 = CARTESIAN_POINT('Ctrl Pts',(-11.4852346439277,-14.0550299934948,
24.8540230124763)) ;
#57190 = CARTESIAN_POINT('Ctrl Pts',(-11.3184718899869,-11.6664005713927,
24.4901998913042)) ;
#57191 = CARTESIAN_POINT('Ctrl Pts',(-11.1555753225574,-9.32889248183853,
24.1340258244603)) ;
#57192 = CARTESIAN_POINT('Ctrl Pts',(-11.0533843889444,-7.86334458038693,
23.910742887255)) ;
#57193 = CARTESIAN_POINT('Ctrl Pts',(-10.8799081843125,-5.36524737160743,
23.5298164000503)) ;
#57194 = CARTESIAN_POINT('Ctrl Pts',(-10.8093853863934,-4.34699231493492,
23.3744590058058)) ;
#57195 = CARTESIAN_POINT('Ctrl Pts',(-10.7429209444356,-3.37610897447703,
23.2259695204405)) ;
#57196 = CARTESIAN_POINT('Ctrl Pts',(-10.7272704888776,-3.14471287330663,
23.1904910996795)) ;
#57197 = CARTESIAN_POINT('Ctrl Pts',(-10.7198900306606,-3.02956785456265,
23.1726482154596)) ;
#57198 = CARTESIAN_POINT('Ctrl Pts',(-10.7191517661507,-3.01792892777941,
23.1708410575628)) ;
#57199 = CARTESIAN_POINT('Ctrl Pts',(-10.718155837799,-3.0017485997851,23.1683146988345)) ;
#57200 = CARTESIAN_POINT('Ctrl Pts',(-10.7177561124938,-2.99514906175769,
23.1672812605971)) ;
#57201 = CARTESIAN_POINT('Ctrl Pts',(-10.7172513792382,-2.98634347416415,
23.1658891353251)) ;
#57202 = CARTESIAN_POINT('Ctrl Pts',(-10.7169086091624,-2.98025788613349,
23.1649242294489)) ;
#57203 = CARTESIAN_POINT('Ctrl Pts',(-10.7167289165089,-2.97566524671235,
23.1641594959843)) ;
#57204 = CARTESIAN_POINT('Ctrl Pts',(-10.716699744908,-2.97457162490568,23.1639710936711)) ;
#57205 = CARTESIAN_POINT('Ctrl Pts',(-10.7167384565843,-2.97437271210288,
23.1639164615673)) ;
#57206 = CARTESIAN_POINT('Ctrl Pts',(-10.7167476789213,-2.97432532480766,
23.1639034464702)) ;
#57207 = CARTESIAN_POINT('Ctrl Pts',(-10.7167569012583,-2.97427793751245,
23.1638904313731)) ;
#57208 = CARTESIAN_POINT('',(-11.6595608585908,-16.2025431678319,25.1698333323831)) ;
#57209 = CARTESIAN_POINT('Origin',(0.376819110642888,-21.5586464785791,-0.81448115993236)) ;
#57210 = CARTESIAN_POINT('Ctrl Pts',(-10.7167569012583,-2.97427793751246,
23.163890431373)) ;
#57211 = CARTESIAN_POINT('Ctrl Pts',(-10.7167705770044,-2.97432596381794,
23.1638929706548)) ;
#57212 = CARTESIAN_POINT('Ctrl Pts',(-10.7167842527504,-2.97437399012343,
23.1638955099365)) ;
#57213 = CARTESIAN_POINT('Ctrl Pts',(-10.7170423164564,-2.97528025486022,
23.1639434266246)) ;
#57214 = CARTESIAN_POINT('Ctrl Pts',(-10.7179683584633,-2.98643371533908,
23.1655740852485)) ;
#57215 = CARTESIAN_POINT('Ctrl Pts',(-10.7267027186728,-3.0914576706438,23.1809220919597)) ;
#57216 = CARTESIAN_POINT('Ctrl Pts',(-10.7692656529469,-3.6819918304019,23.2702515899602)) ;
#57217 = CARTESIAN_POINT('Ctrl Pts',(-10.9623645657162,-6.36109345723266,
23.6755157069365)) ;
#57218 = CARTESIAN_POINT('Ctrl Pts',(-11.6012362667214,-15.3793218860576,
25.0448385213858)) ;
#57219 = CARTESIAN_POINT('Ctrl Pts',(-11.6595608585848,-16.2025431677229,
25.1698333323657)) ;
#57220 = CARTESIAN_POINT('',(-15.4457568027361,-2.97427793608127,20.3185455969618)) ;
#57221 = CARTESIAN_POINT('Origin',(-5.46365993374796E-16,-2.97427793741672,
0.)) ;
#57222 = CARTESIAN_POINT('',(-16.7764141848438,-16.2025431678318,22.0911248354107)) ;
#57223 = CARTESIAN_POINT('Ctrl Pts',(-16.7764141848437,-16.2025431678318,
22.0911248354107)) ;
#57224 = CARTESIAN_POINT('Ctrl Pts',(-16.7752198634206,-16.190713841179,22.0895430472459)) ;
#57225 = CARTESIAN_POINT('Ctrl Pts',(-16.7740266741282,-16.1788957010685,
22.0879627528603)) ;
#57226 = CARTESIAN_POINT('Ctrl Pts',(-16.5603070515992,-14.0620696485942,
21.8049052958167)) ;
#57227 = CARTESIAN_POINT('Ctrl Pts',(-16.3192597867892,-11.6737192528371,
21.4854747478875)) ;
#57228 = CARTESIAN_POINT('Ctrl Pts',(-16.0835676324059,-9.33584946938956,
21.1725978744201)) ;
#57229 = CARTESIAN_POINT('Ctrl Pts',(-15.9356042182785,-7.86869477874113,
20.97628848721)) ;
#57230 = CARTESIAN_POINT('Ctrl Pts',(-15.6840608298526,-5.36827143780728,
20.6412491931078)) ;
#57231 = CARTESIAN_POINT('Ctrl Pts',(-15.5817192347535,-4.34932190857903,
20.5045915876768)) ;
#57232 = CARTESIAN_POINT('Ctrl Pts',(-15.4847363587165,-3.37693719727565,
20.3736607611576)) ;
#57233 = CARTESIAN_POINT('Ctrl Pts',(-15.4617693823315,-3.1449852959358,20.3423014857958)) ;
#57234 = CARTESIAN_POINT('Ctrl Pts',(-15.4507050345335,-3.02962747694642,
20.3264333232862)) ;
#57235 = CARTESIAN_POINT('Ctrl Pts',(-15.4495943826826,-3.01797675837514,
20.324825522346)) ;
#57236 = CARTESIAN_POINT('Ctrl Pts',(-15.4480775917176,-3.00178591878239,
20.3225709128349)) ;
#57237 = CARTESIAN_POINT('Ctrl Pts',(-15.4474654051385,-2.99519054883672,
20.321648174563)) ;
#57238 = CARTESIAN_POINT('Ctrl Pts',(-15.4466716458739,-2.98636916407357,
20.3203949606915)) ;
#57239 = CARTESIAN_POINT('Ctrl Pts',(-15.4461313364807,-2.98030508165379,
20.3195294015113)) ;
#57240 = CARTESIAN_POINT('Ctrl Pts',(-15.4458171571932,-2.97607071487635,
20.3188770382006)) ;
#57241 = CARTESIAN_POINT('Ctrl Pts',(-15.4456372043608,-2.97516294137418,
20.3188227779353)) ;
#57242 = CARTESIAN_POINT('Ctrl Pts',(-15.4457440117809,-2.97437258105023,
20.3185752400619)) ;
#57243 = CARTESIAN_POINT('Ctrl Pts',(-15.4457504068511,-2.97432525840346,
20.3185604187873)) ;
#57244 = CARTESIAN_POINT('Ctrl Pts',(-15.4457568019214,-2.97427793575669,
20.3185455975128)) ;
#57245 = CARTESIAN_POINT('',(-16.7977369565509,-16.2025431678318,22.0749156857653)) ;
#57246 = CARTESIAN_POINT('Origin',(0.543098662732483,-21.5586464785792,-0.71443407293372)) ;
#57247 = CARTESIAN_POINT('Ctrl Pts',(-15.4457568025556,-2.97427793106408,
20.3185455960431)) ;
#57248 = CARTESIAN_POINT('Ctrl Pts',(-15.4457694984367,-2.9743262894881,20.3185461227573)) ;
#57249 = CARTESIAN_POINT('Ctrl Pts',(-15.4457821943179,-2.97437464791213,
20.3185466494715)) ;
#57250 = CARTESIAN_POINT('Ctrl Pts',(-15.4464212757398,-2.97680889962313,
20.3185731630504)) ;
#57251 = CARTESIAN_POINT('Ctrl Pts',(-15.4464747921446,-2.97934518644453,
20.3190662866477)) ;
#57252 = CARTESIAN_POINT('Ctrl Pts',(-15.4504481397431,-3.01314189784647,
20.323158932543)) ;
#57253 = CARTESIAN_POINT('Ctrl Pts',(-15.4638357589392,-3.14117566784154,
20.3399288645903)) ;
#57254 = CARTESIAN_POINT('Ctrl Pts',(-15.5746903197145,-4.20201721913459,
20.4789319888574)) ;
#57255 = CARTESIAN_POINT('Ctrl Pts',(-16.0994049025687,-9.34914228273644,
21.1633563985944)) ;
#57256 = CARTESIAN_POINT('Ctrl Pts',(-16.3547359668196,-11.8530767546699,
21.4962553652859)) ;
#57257 = CARTESIAN_POINT('Ctrl Pts',(-16.588974741721,-14.1525006000269,21.8021454522111)) ;
#57258 = CARTESIAN_POINT('Ctrl Pts',(-16.7977369565519,-16.2025431678313,
22.0749156857645)) ;
#57259 = CARTESIAN_POINT('',(-19.4525302835701,-2.97427793904102,16.5231281535061)) ;
#57260 = CARTESIAN_POINT('Origin',(-5.46365993374796E-16,-2.97427793741672,
0.)) ;
#57261 = CARTESIAN_POINT('',(-21.1331297746477,-16.2025431678318,17.9682134705436)) ;
#57262 = CARTESIAN_POINT('Ctrl Pts',(-21.1331297746474,-16.2025431678318,
17.9682134705439)) ;
#57263 = CARTESIAN_POINT('Ctrl Pts',(-21.1316374631217,-16.1908247582476,
17.9669374849658)) ;
#57264 = CARTESIAN_POINT('Ctrl Pts',(-21.1301452569594,-16.1791071590717,
17.965661585088)) ;
#57265 = CARTESIAN_POINT('Ctrl Pts',(-20.8605852292292,-14.0623748808398,
17.7351754744795)) ;
#57266 = CARTESIAN_POINT('Ctrl Pts',(-20.5565069219806,-11.6740365940616,
17.4750324022608)) ;
#57267 = CARTESIAN_POINT('Ctrl Pts',(-20.259063823058,-9.33615114006502,17.2201355811663)) ;
#57268 = CARTESIAN_POINT('Ctrl Pts',(-20.0723501178403,-7.86892678670822,
17.0602159811398)) ;
#57269 = CARTESIAN_POINT('Ctrl Pts',(-19.7546512798608,-5.36840259178783,
16.7870731379981)) ;
#57270 = CARTESIAN_POINT('Ctrl Pts',(-19.6253211866005,-4.34942295199821,
16.6756076595711)) ;
#57271 = CARTESIAN_POINT('Ctrl Pts',(-19.5024511712846,-3.37697313538146,
16.5685792814353)) ;
#57272 = CARTESIAN_POINT('Ctrl Pts',(-19.473276780477,-3.14499712523272,16.5428877433583)) ;
#57273 = CARTESIAN_POINT('Ctrl Pts',(-19.4590587751061,-3.02963007194482,
16.5297680413151)) ;
#57274 = CARTESIAN_POINT('Ctrl Pts',(-19.4576283953209,-3.01797883744602,
16.5284365298052)) ;
#57275 = CARTESIAN_POINT('Ctrl Pts',(-19.4556623320526,-3.00178752696938,
16.5265606453689)) ;
#57276 = CARTESIAN_POINT('Ctrl Pts',(-19.4548661148076,-2.9951923179276,16.5257911024352)) ;
#57277 = CARTESIAN_POINT('Ctrl Pts',(-19.4538214301102,-2.98637030522913,
16.5247377534462)) ;
#57278 = CARTESIAN_POINT('Ctrl Pts',(-19.4531077541231,-2.98030684070767,
16.524008657544)) ;
#57279 = CARTESIAN_POINT('Ctrl Pts',(-19.4526605493631,-2.97607144563206,
16.5234389746291)) ;
#57280 = CARTESIAN_POINT('Ctrl Pts',(-19.4524720868882,-2.97516264973382,
16.5234256419414)) ;
#57281 = CARTESIAN_POINT('Ctrl Pts',(-19.4525240609173,-2.97437254348245,
16.5231599642006)) ;
#57282 = CARTESIAN_POINT('Ctrl Pts',(-19.4525271723989,-2.9743252428848,16.5231440591025)) ;
#57283 = CARTESIAN_POINT('Ctrl Pts',(-19.4525302838691,-2.97427794228964,
16.5231281539948)) ;
#57284 = CARTESIAN_POINT('',(-21.1504695437717,-16.2025431678318,17.9477995161833)) ;
#57285 = CARTESIAN_POINT('Origin',(0.683983524963512,-21.5586464785791,-0.580980842721122)) ;
#57286 = CARTESIAN_POINT('Ctrl Pts',(-19.4525302838691,-2.97427794228965,
16.5231281539948)) ;
#57287 = CARTESIAN_POINT('Ctrl Pts',(-19.4525427535086,-2.97432631415661,
16.5231259928427)) ;
#57288 = CARTESIAN_POINT('Ctrl Pts',(-19.452555223148,-2.97437468602357,16.5231238316906)) ;
#57289 = CARTESIAN_POINT('Ctrl Pts',(-19.4531824648511,-2.97680786400913,
16.5230151224743)) ;
#57290 = CARTESIAN_POINT('Ctrl Pts',(-19.4533427230956,-2.97934036345287,
16.523481894319)) ;
#57291 = CARTESIAN_POINT('Ctrl Pts',(-19.458120904464,-3.01326272602979,16.5266361147738)) ;
#57292 = CARTESIAN_POINT('Ctrl Pts',(-19.4749326989184,-3.14232006038648,
16.5402453876941)) ;
#57293 = CARTESIAN_POINT('Ctrl Pts',(-19.6134421521223,-4.20603554880853,
16.65248228589)) ;
#57294 = CARTESIAN_POINT('Ctrl Pts',(-20.2727144713711,-9.35077018734797,
17.2078483873162)) ;
#57295 = CARTESIAN_POINT('Ctrl Pts',(-20.593580039196,-11.8542418942229,17.4780259333328)) ;
#57296 = CARTESIAN_POINT('Ctrl Pts',(-20.8880093579677,-14.1529599452982,
17.726333838428)) ;
#57297 = CARTESIAN_POINT('Ctrl Pts',(-21.1504695437716,-16.2025431678313,
17.9477995161832)) ;
#57298 = CARTESIAN_POINT('',(-22.5497250681625,-2.97427793560092,11.9551076001539)) ;
#57299 = CARTESIAN_POINT('Origin',(-5.46365993374796E-16,-2.97427793741672,
0.)) ;
#57300 = CARTESIAN_POINT('',(-24.5016837039787,-16.2025431678318,13.005128414026)) ;
#57301 = CARTESIAN_POINT('Ctrl Pts',(-24.5016837039782,-16.2025431678318,
13.0051284140269)) ;
#57302 = CARTESIAN_POINT('Ctrl Pts',(-24.4996676420489,-16.1889006495292,
13.0040511248088)) ;
#57303 = CARTESIAN_POINT('Ctrl Pts',(-24.4976524169855,-16.1752637798932,
13.0029742776455)) ;
#57304 = CARTESIAN_POINT('Ctrl Pts',(-24.1845818021322,-14.0567372972925,
12.8356823852449)) ;
#57305 = CARTESIAN_POINT('Ctrl Pts',(-23.8316567265512,-11.6681756060599,
12.6469712655301)) ;
#57306 = CARTESIAN_POINT('Ctrl Pts',(-23.4864154829261,-9.33057976204126,
12.4619975963323)) ;
#57307 = CARTESIAN_POINT('Ctrl Pts',(-23.269879341362,-7.86464212508095,12.34605621553)) ;
#57308 = CARTESIAN_POINT('Ctrl Pts',(-22.9011691865421,-5.36600381543967,
12.1477438959469)) ;
#57309 = CARTESIAN_POINT('Ctrl Pts',(-22.7509867332351,-4.34760394628317,
12.0667321657766)) ;
#57310 = CARTESIAN_POINT('Ctrl Pts',(-22.6081554098183,-3.37633177831297,
11.9887125870729)) ;
#57311 = CARTESIAN_POINT('Ctrl Pts',(-22.5742032273907,-3.14478388077979,
11.9699275781758)) ;
#57312 = CARTESIAN_POINT('Ctrl Pts',(-22.5575213999732,-3.02958227422016,
11.9601847498191)) ;
#57313 = CARTESIAN_POINT('Ctrl Pts',(-22.5558396144626,-3.01794052653865,
11.9591926323437)) ;
#57314 = CARTESIAN_POINT('Ctrl Pts',(-22.5535174978171,-3.00175763485085,
11.9577839214564)) ;
#57315 = CARTESIAN_POINT('Ctrl Pts',(-22.5525739903808,-2.99515898007651,
11.9572031990715)) ;
#57316 = CARTESIAN_POINT('Ctrl Pts',(-22.55132911353,-2.98634939833744,11.9564000619532)) ;
#57317 = CARTESIAN_POINT('Ctrl Pts',(-22.5504731163466,-2.9802696426833,11.95583989009)) ;
#57318 = CARTESIAN_POINT('Ctrl Pts',(-22.549917036684,-2.97605518832563,11.9553812397866)) ;
#57319 = CARTESIAN_POINT('Ctrl Pts',(-22.549743958395,-2.97516568496484,11.9553895210276)) ;
#57320 = CARTESIAN_POINT('Ctrl Pts',(-22.5497270953284,-2.97437322186437,
11.9551378608054)) ;
#57321 = CARTESIAN_POINT('Ctrl Pts',(-22.5497260814769,-2.97432557691684,
11.9551227303367)) ;
#57322 = CARTESIAN_POINT('Ctrl Pts',(-22.5497250676253,-2.97427793196933,
11.9551075998681)) ;
#57323 = CARTESIAN_POINT('',(-24.5142296821799,-16.2025431678318,12.9814641887753)) ;
#57324 = CARTESIAN_POINT('Origin',(0.792886077760343,-21.5586464785791,-0.420361594016722)) ;
#57325 = CARTESIAN_POINT('Ctrl Pts',(-22.5497250676253,-2.97427793196933,
11.9551075998681)) ;
#57326 = CARTESIAN_POINT('Ctrl Pts',(-22.5497352940808,-2.97432684211101,
11.9551058060875)) ;
#57327 = CARTESIAN_POINT('Ctrl Pts',(-22.5497455205363,-2.97437575225269,
11.9551040123068)) ;
#57328 = CARTESIAN_POINT('Ctrl Pts',(-22.5499048520773,-2.97513778835108,
11.9550760646145)) ;
#57329 = CARTESIAN_POINT('Ctrl Pts',(-22.5500439827512,-2.97596782595578,
11.9551105442205)) ;
#57330 = CARTESIAN_POINT('Ctrl Pts',(-22.5514940525204,-2.98473527704851,
11.9555115761301)) ;
#57331 = CARTESIAN_POINT('Ctrl Pts',(-22.5558837380948,-3.01362289847503,
11.9575649728667)) ;
#57332 = CARTESIAN_POINT('Ctrl Pts',(-22.5895429583672,-3.23583015028412,
11.9735614046487)) ;
#57333 = CARTESIAN_POINT('Ctrl Pts',(-22.7007162739326,-3.98248101845175,
12.0309463354103)) ;
#57334 = CARTESIAN_POINT('Ctrl Pts',(-22.9981001655269,-5.9830848446617,12.185645166953)) ;
#57335 = CARTESIAN_POINT('Ctrl Pts',(-23.1944779036023,-7.30595314390739,
12.2884330665384)) ;
#57336 = CARTESIAN_POINT('Ctrl Pts',(-23.4213140715843,-8.83439078112419,
12.4073031199904)) ;
#57337 = CARTESIAN_POINT('Ctrl Pts',(-23.4860190491741,-9.27052278052022,
12.4412627181695)) ;
#57338 = CARTESIAN_POINT('Ctrl Pts',(-23.8053430784459,-11.4225775147922,
12.6087526144909)) ;
#57339 = CARTESIAN_POINT('Ctrl Pts',(-24.1472874488276,-13.7281025785756,
12.7884729898918)) ;
#57340 = CARTESIAN_POINT('Ctrl Pts',(-24.4735167425919,-15.9279951058929,
12.9600499578252)) ;
#57341 = CARTESIAN_POINT('Ctrl Pts',(-24.4939674190775,-16.0659036750085,
12.9708063576517)) ;
#57342 = CARTESIAN_POINT('Ctrl Pts',(-24.5142296821805,-16.2025431678318,
12.981464188774)) ;
#57343 = CARTESIAN_POINT('',(-24.592552107853,-2.97439688780173,6.82803753488347)) ;
#57344 = CARTESIAN_POINT('Origin',(-5.46365993374796E-16,-2.97427793741672,
0.)) ;
#57345 = CARTESIAN_POINT('',(-26.7245661349767,-16.2025431678318,7.43393800703095)) ;
#57346 = CARTESIAN_POINT('Ctrl Pts',(-26.7245661349768,-16.2025431678313,
7.43393800703048)) ;
#57347 = CARTESIAN_POINT('Ctrl Pts',(-26.6689832159522,-15.8579457768539,
7.41830998820638)) ;
#57348 = CARTESIAN_POINT('Ctrl Pts',(-26.6124202750428,-15.5072677851224,
7.40240343975473)) ;
#57349 = CARTESIAN_POINT('Ctrl Pts',(-26.3507918514815,-13.8852011858705,
7.3288117644863)) ;
#57350 = CARTESIAN_POINT('Ctrl Pts',(-26.1359705189235,-12.5532595769792,
7.26833999538627)) ;
#57351 = CARTESIAN_POINT('Ctrl Pts',(-25.877434070244,-10.95010355525,7.19545563196677)) ;
#57352 = CARTESIAN_POINT('Ctrl Pts',(-25.8274200724287,-10.6399639551473,
7.18135091155874)) ;
#57353 = CARTESIAN_POINT('Ctrl Pts',(-25.7535520225924,-10.1818898397547,
7.16051008425751)) ;
#57354 = CARTESIAN_POINT('Ctrl Pts',(-25.7125628705679,-9.92770194704203,
7.1489430778947)) ;
#57355 = CARTESIAN_POINT('Ctrl Pts',(-25.6721063124177,-9.6768097016269,7.13752188896885)) ;
#57356 = CARTESIAN_POINT('Ctrl Pts',(-25.6516451009408,-9.54991748949785,
7.13174456271593)) ;
#57357 = CARTESIAN_POINT('Ctrl Pts',(-25.6480238982615,-9.52746023152702,
7.13072208912283)) ;
#57358 = CARTESIAN_POINT('Ctrl Pts',(-25.5859834329005,-9.14270729296583,
7.11320283416776)) ;
#57359 = CARTESIAN_POINT('Ctrl Pts',(-25.3739725568845,-7.8279579923284,7.05337615177815)) ;
#57360 = CARTESIAN_POINT('Ctrl Pts',(-25.0488113106629,-5.81059539629016,
6.96103715749616)) ;
#57361 = CARTESIAN_POINT('Ctrl Pts',(-24.9410807235872,-5.14207211743425,
6.93035492624889)) ;
#57362 = CARTESIAN_POINT('Ctrl Pts',(-24.766903337543,-4.06065733928159,6.88040057681779)) ;
#57363 = CARTESIAN_POINT('Ctrl Pts',(-24.6971464703163,-3.62728003610139,
6.86022009636915)) ;
#57364 = CARTESIAN_POINT('Ctrl Pts',(-24.630044306151,-3.20962006541524,6.84032192534756)) ;
#57365 = CARTESIAN_POINT('Ctrl Pts',(-24.6139309219069,-3.10915131540964,
6.83543402113868)) ;
#57366 = CARTESIAN_POINT('Ctrl Pts',(-24.6021451332267,-3.03535094781093,
6.83166179919274)) ;
#57367 = CARTESIAN_POINT('Ctrl Pts',(-24.6002338489497,-3.02336908310285,
6.83104144184553)) ;
#57368 = CARTESIAN_POINT('Ctrl Pts',(-24.5972607462002,-3.0046695511412,6.83003816803247)) ;
#57369 = CARTESIAN_POINT('Ctrl Pts',(-24.5961100776802,-2.99742051577194,
6.82964246735651)) ;
#57370 = CARTESIAN_POINT('Ctrl Pts',(-24.5946263153786,-2.98801463919662,
6.82909564333515)) ;
#57371 = CARTESIAN_POINT('Ctrl Pts',(-24.59337944986,-2.97996100765901,6.82854250312845)) ;
#57372 = CARTESIAN_POINT('Ctrl Pts',(-24.5925577081587,-2.97451596139029,
6.82809194035633)) ;
#57373 = CARTESIAN_POINT('Ctrl Pts',(-24.5925713143705,-2.97451583818675,
6.82804285739138)) ;
#57374 = CARTESIAN_POINT('',(-26.7317316862594,-16.2025431678318,7.40813002376167)) ;
#57375 = CARTESIAN_POINT('Origin',(0.864714158790679,-21.5586464785792,-0.240086704374452)) ;
#57376 = CARTESIAN_POINT('Ctrl Pts',(-24.5925713143603,-2.97451583818853,
6.82804285738853)) ;
#57377 = CARTESIAN_POINT('Ctrl Pts',(-24.5925806259886,-2.97456488239044,
6.82804003606991)) ;
#57378 = CARTESIAN_POINT('Ctrl Pts',(-24.5925899376168,-2.97461392659235,
6.82803721475129)) ;
#57379 = CARTESIAN_POINT('Ctrl Pts',(-24.5937332774705,-2.98063587992714,
6.82769079563499)) ;
#57380 = CARTESIAN_POINT('Ctrl Pts',(-24.5945770239903,-2.98636186716204,
6.82823805211795)) ;
#57381 = CARTESIAN_POINT('Ctrl Pts',(-24.6080089005343,-3.06781746902136,
6.83087603583482)) ;
#57382 = CARTESIAN_POINT('Ctrl Pts',(-24.6568415415074,-3.36899802404575,
6.84362461449725)) ;
#57383 = CARTESIAN_POINT('Ctrl Pts',(-24.6710163121772,-3.45642106171283,
6.84732431020992)) ;
#57384 = CARTESIAN_POINT('Ctrl Pts',(-24.6728723965344,-3.46786980995301,
6.84780959155663)) ;
#57385 = CARTESIAN_POINT('Ctrl Pts',(-24.8318196304806,-4.44835604177014,
6.88940695397689)) ;
#57386 = CARTESIAN_POINT('Ctrl Pts',(-25.2480074862592,-7.02233073853014,
7.00250108447751)) ;
#57387 = CARTESIAN_POINT('Ctrl Pts',(-25.628103213734,-9.37363014663993,7.10612690748992)) ;
#57388 = CARTESIAN_POINT('Ctrl Pts',(-25.7147409830227,-9.90964877679412,
7.12979161674918)) ;
#57389 = CARTESIAN_POINT('Ctrl Pts',(-25.7418193097697,-10.0771773232176,
7.13718657805486)) ;
#57390 = CARTESIAN_POINT('Ctrl Pts',(-25.7451959194303,-10.0980678317341,
7.13810874883747)) ;
#57391 = CARTESIAN_POINT('Ctrl Pts',(-26.0669352634096,-12.0886187181864,
7.22598029792739)) ;
#57392 = CARTESIAN_POINT('Ctrl Pts',(-26.4160920844778,-14.2492145131363,
7.32160128400388)) ;
#57393 = CARTESIAN_POINT('Ctrl Pts',(-26.7317316862593,-16.2025431678313,
7.40813002376179)) ;
#57394 = CARTESIAN_POINT('',(-25.4853955845497,-2.97427793815454,1.38177794953793)) ;
#57395 = CARTESIAN_POINT('Origin',(-5.46365993374796E-16,-2.97427793741672,
0.)) ;
#57396 = CARTESIAN_POINT('',(-27.6978375557248,-16.2025431678318,1.51514492105713)) ;
#57397 = CARTESIAN_POINT('Ctrl Pts',(-27.6978375557247,-16.2025431678318,
1.51514492105922)) ;
#57398 = CARTESIAN_POINT('Ctrl Pts',(-27.6949483747658,-16.1852712613029,
1.51497881880076)) ;
#57399 = CARTESIAN_POINT('Ctrl Pts',(-27.6920606024541,-16.1680077735078,
1.51481279026704)) ;
#57400 = CARTESIAN_POINT('Ctrl Pts',(-27.3371143876217,-14.0460917001996,
1.49440474478063)) ;
#57401 = CARTESIAN_POINT('Ctrl Pts',(-26.9374998132548,-11.6571071294358,
1.47131995388038)) ;
#57402 = CARTESIAN_POINT('Ctrl Pts',(-26.5465905728723,-9.32005883265994,
1.4484095511999)) ;
#57403 = CARTESIAN_POINT('Ctrl Pts',(-26.3017916915238,-7.8565516409229,1.43412818138653)) ;
#57404 = CARTESIAN_POINT('Ctrl Pts',(-25.8844750239149,-5.3614086784368,1.40899545055731)) ;
#57405 = CARTESIAN_POINT('Ctrl Pts',(-25.7143289878448,-4.34403568291514,
1.39854061302158)) ;
#57406 = CARTESIAN_POINT('Ctrl Pts',(-25.5523230854378,-3.37505853243338,
1.3877275070587)) ;
#57407 = CARTESIAN_POINT('Ctrl Pts',(-25.5137645868328,-3.14436762856298,
1.38494407232914)) ;
#57408 = CARTESIAN_POINT('Ctrl Pts',(-25.4945881657819,-3.02949231117301,
1.38311080631034)) ;
#57409 = CARTESIAN_POINT('Ctrl Pts',(-25.4926481764263,-3.01786813916945,
1.38291676976861)) ;
#57410 = CARTESIAN_POINT('Ctrl Pts',(-25.4899521301898,-3.00170290476441,
1.38261348814891)) ;
#57411 = CARTESIAN_POINT('Ctrl Pts',(-25.4888514934502,-2.99510126826416,
1.38248248287018)) ;
#57412 = CARTESIAN_POINT('Ctrl Pts',(-25.4873884466953,-2.98631563827613,
1.38227661114065)) ;
#57413 = CARTESIAN_POINT('Ctrl Pts',(-25.486371196431,-2.98020487444517,1.38212680866863)) ;
#57414 = CARTESIAN_POINT('Ctrl Pts',(-25.4856195768672,-2.97566139772543,
1.38192825014818)) ;
#57415 = CARTESIAN_POINT('Ctrl Pts',(-25.4854468698752,-2.97461266012032,
1.38186796062895)) ;
#57416 = CARTESIAN_POINT('Ctrl Pts',(-25.4854102201195,-2.9743734717481,1.38180367418922)) ;
#57417 = CARTESIAN_POINT('Ctrl Pts',(-25.4854029011111,-2.97432570548941,
1.38179083609563)) ;
#57418 = CARTESIAN_POINT('Ctrl Pts',(-25.4853955821027,-2.97427793923073,
1.38177799800203)) ;
#57419 = CARTESIAN_POINT('',(-27.6992876268763,-16.2025431678318,1.48839993237876)) ;
#57420 = CARTESIAN_POINT('Origin',(0.896109166816714,-21.5586464785791,-0.0485856272728462)) ;
#57421 = CARTESIAN_POINT('Ctrl Pts',(-25.4853955876312,-2.97427794002965,
1.38177789850702)) ;
#57422 = CARTESIAN_POINT('Ctrl Pts',(-25.4854041324089,-2.97432678140872,
1.38177145595585)) ;
#57423 = CARTESIAN_POINT('Ctrl Pts',(-25.4854126771865,-2.97437562278778,
1.38176501340469)) ;
#57424 = CARTESIAN_POINT('Ctrl Pts',(-25.4862266854511,-2.9790284397228,1.38115127129212)) ;
#57425 = CARTESIAN_POINT('Ctrl Pts',(-25.4869891119617,-2.983689485392,1.38151436532657)) ;
#57426 = CARTESIAN_POINT('Ctrl Pts',(-25.4974120488345,-3.04568905696004,
1.38115379950162)) ;
#57427 = CARTESIAN_POINT('Ctrl Pts',(-25.5378627351659,-3.2872365214572,1.38263725546573)) ;
#57428 = CARTESIAN_POINT('Ctrl Pts',(-25.7524643697489,-4.5686999147475,1.39047624847401)) ;
#57429 = CARTESIAN_POINT('Ctrl Pts',(-26.5784759569267,-9.50471724369494,
1.4318077909381)) ;
#57430 = CARTESIAN_POINT('Ctrl Pts',(-26.9899241868522,-11.9634061746525,
1.45235798347176)) ;
#57431 = CARTESIAN_POINT('Ctrl Pts',(-27.363591331709,-14.1964160924647,1.47129725231825)) ;
#57432 = CARTESIAN_POINT('Ctrl Pts',(-27.6992876268763,-16.2025431678313,
1.48839993237614)) ;
#57433 = CARTESIAN_POINT('',(-25.1866026070031,-2.97427793714977,-4.12913399045467)) ;
#57434 = CARTESIAN_POINT('Origin',(-5.46365993374796E-16,-2.97427793741672,
0.)) ;
#57435 = CARTESIAN_POINT('',(-27.3759888763025,-16.2025431678318,-4.47449465746571)) ;
#57436 = CARTESIAN_POINT('Ctrl Pts',(-27.3759888763025,-16.2025431678318,
-4.4744946574655)) ;
#57437 = CARTESIAN_POINT('Ctrl Pts',(-27.3732094220677,-16.1857420647624,
-4.47404829586599)) ;
#57438 = CARTESIAN_POINT('Ctrl Pts',(-27.3704308025602,-16.1689460141171,
-4.47360207526417)) ;
#57439 = CARTESIAN_POINT('Ctrl Pts',(-27.0194681712013,-14.0474667151253,
-4.41724160356195)) ;
#57440 = CARTESIAN_POINT('Ctrl Pts',(-26.6242428750162,-11.658536835958,-4.35388274751894)) ;
#57441 = CARTESIAN_POINT('Ctrl Pts',(-26.2375361320519,-9.32141776666402,
-4.29222155923528)) ;
#57442 = CARTESIAN_POINT('Ctrl Pts',(-25.9953385064225,-7.85759660285274,
-4.25353612774431)) ;
#57443 = CARTESIAN_POINT('Ctrl Pts',(-25.5823004912435,-5.36199912354941,
-4.18835840434003)) ;
#57444 = CARTESIAN_POINT('Ctrl Pts',(-25.4138624515631,-4.34449041737206,
-4.16198878709876)) ;
#57445 = CARTESIAN_POINT('Ctrl Pts',(-25.2532711456091,-3.37522003933381,
-4.13771484198824)) ;
#57446 = CARTESIAN_POINT('Ctrl Pts',(-25.2149978063456,-3.14442068934507,
-4.13214150615795)) ;
#57447 = CARTESIAN_POINT('Ctrl Pts',(-25.1958687361614,-3.02950392952988,
-4.12980862521967)) ;
#57448 = CARTESIAN_POINT('Ctrl Pts',(-25.1939320152815,-3.01787749563495,
-4.12958103145751)) ;
#57449 = CARTESIAN_POINT('Ctrl Pts',(-25.1912333983801,-3.00170981125287,
-4.1292975922956)) ;
#57450 = CARTESIAN_POINT('Ctrl Pts',(-25.1901303432712,-2.99510823617433,
-4.12918892312608)) ;
#57451 = CARTESIAN_POINT('Ctrl Pts',(-25.1886567289002,-2.98631949906856,
-4.12907540246666)) ;
#57452 = CARTESIAN_POINT('Ctrl Pts',(-25.1876317161037,-2.98021264730425,
-4.1290030629297)) ;
#57453 = CARTESIAN_POINT('Ctrl Pts',(-25.1868539544775,-2.97566296777208,
-4.12903526378729)) ;
#57454 = CARTESIAN_POINT('Ctrl Pts',(-25.1866710372384,-2.97460670643535,
-4.12905707867674)) ;
#57455 = CARTESIAN_POINT('Ctrl Pts',(-25.1866224802819,-2.97437337212036,
-4.12911160736365)) ;
#57456 = CARTESIAN_POINT('Ctrl Pts',(-25.1866125500831,-2.97432565381897,
-4.12912275881491)) ;
#57457 = CARTESIAN_POINT('Ctrl Pts',(-25.1866026198728,-2.97427793551953,
-4.12913391026427)) ;
#57458 = CARTESIAN_POINT('',(-27.3716556636072,-16.2025431678318,-4.50092608560145)) ;
#57459 = CARTESIAN_POINT('Origin',(0.885603106156221,-21.5586464785792,0.145187259760995)) ;
#57460 = CARTESIAN_POINT('Ctrl Pts',(-25.1866025936503,-2.97427793771224,
-4.12913407248572)) ;
#57461 = CARTESIAN_POINT('Ctrl Pts',(-25.1866095211381,-2.97432675457791,
-4.12914237450595)) ;
#57462 = CARTESIAN_POINT('Ctrl Pts',(-25.1866164486258,-2.97437557144357,
-4.12915067652617)) ;
#57463 = CARTESIAN_POINT('Ctrl Pts',(-25.1869254243862,-2.97655287275656,
-4.12952095838038)) ;
#57464 = CARTESIAN_POINT('Ctrl Pts',(-25.1903482932883,-2.99746421379417,
-4.13029948590828)) ;
#57465 = CARTESIAN_POINT('Ctrl Pts',(-25.2317140552067,-3.25010212170233,
-4.13962725825562)) ;
#57466 = CARTESIAN_POINT('Ctrl Pts',(-25.5134259808611,-4.95579873516529,
-4.18778756473923)) ;
#57467 = CARTESIAN_POINT('Ctrl Pts',(-26.0153659193611,-7.99520368216468,
-4.27388892128809)) ;
#57468 = CARTESIAN_POINT('Ctrl Pts',(-26.9798765474653,-13.831802071856,-4.43538391273868)) ;
#57469 = CARTESIAN_POINT('Ctrl Pts',(-27.3716556636063,-16.2025431678262,
-4.500926085601)) ;
#57470 = CARTESIAN_POINT('',(-23.7101121128184,-2.97427793741671,-9.44697210719331)) ;
#57471 = CARTESIAN_POINT('Origin',(-5.46365993374796E-16,-2.97427793741672,
0.)) ;
#57472 = CARTESIAN_POINT('',(-25.7740693832513,-16.2025431678318,-10.2549118388445)) ;
#57473 = CARTESIAN_POINT('Ctrl Pts',(-25.7740693832516,-16.2025431678318,
-10.2549118388438)) ;
#57474 = CARTESIAN_POINT('Ctrl Pts',(-25.7717662057054,-16.1877653700843,
-10.254002864804)) ;
#57475 = CARTESIAN_POINT('Ctrl Pts',(-25.7694634381093,-16.1729902152862,
-10.2530940582596)) ;
#57476 = CARTESIAN_POINT('Ctrl Pts',(-25.4391163992136,-14.0533996573025,
-10.1227206511024)) ;
#57477 = CARTESIAN_POINT('Ctrl Pts',(-25.0667883861616,-11.6647055239092,
-9.97589555283087)) ;
#57478 = CARTESIAN_POINT('Ctrl Pts',(-24.702330635356,-9.32728125401795,-9.83252608174547)) ;
#57479 = CARTESIAN_POINT('Ctrl Pts',(-24.473900641258,-7.86210553169967,-9.74259625848603)) ;
#57480 = CARTESIAN_POINT('Ctrl Pts',(-24.0842249574383,-5.36454711554133,
-9.59003060362382)) ;
#57481 = CARTESIAN_POINT('Ctrl Pts',(-23.925302428713,-4.34645292280116,-9.52803206672356)) ;
#57482 = CARTESIAN_POINT('Ctrl Pts',(-23.7734866041964,-3.37591728035413,
-9.46972551968006)) ;
#57483 = CARTESIAN_POINT('Ctrl Pts',(-23.7372330254185,-3.14464984931574,
-9.45602655707944)) ;
#57484 = CARTESIAN_POINT('Ctrl Pts',(-23.7190244883969,-3.02955404144013,
-9.44962574507765)) ;
#57485 = CARTESIAN_POINT('Ctrl Pts',(-23.7171804403966,-3.01791784367858,
-9.44898656105867)) ;
#57486 = CARTESIAN_POINT('Ctrl Pts',(-23.7146042867674,-3.00174019075879,
-9.4481290283292)) ;
#57487 = CARTESIAN_POINT('Ctrl Pts',(-23.7135506216482,-2.99514003796932,
-9.44778581572707)) ;
#57488 = CARTESIAN_POINT('Ctrl Pts',(-23.7121337604259,-2.98633794087801,
-9.44735739531497)) ;
#57489 = CARTESIAN_POINT('Ctrl Pts',(-23.7111510567275,-2.98024831805525,
-9.44706718623769)) ;
#57490 = CARTESIAN_POINT('Ctrl Pts',(-23.7103793731646,-2.9756660058921,-9.44692967577819)) ;
#57491 = CARTESIAN_POINT('Ctrl Pts',(-23.7101909070959,-2.97457957271177,
-9.44691089066687)) ;
#57492 = CARTESIAN_POINT('Ctrl Pts',(-23.7101369135214,-2.97437287773465,
-9.44695283905479)) ;
#57493 = CARTESIAN_POINT('Ctrl Pts',(-23.7101245131969,-2.97432540755282,
-9.44696247304605)) ;
#57494 = CARTESIAN_POINT('Ctrl Pts',(-23.7101121128723,-2.97427793737098,
-9.4469721070373)) ;
#57495 = CARTESIAN_POINT('',(-25.7641555029173,-16.2025431678318,-10.2797938022424)) ;
#57496 = CARTESIAN_POINT('Origin',(0.833687228529012,-21.5586464785791,0.33217135189247)) ;
#57497 = CARTESIAN_POINT('Ctrl Pts',(-23.7101121127218,-2.97427793679491,
-9.44697210715423)) ;
#57498 = CARTESIAN_POINT('Ctrl Pts',(-23.7101153152554,-2.97432592122196,
-9.44698579066765)) ;
#57499 = CARTESIAN_POINT('Ctrl Pts',(-23.7101185177891,-2.974373905649,-9.44699947418107)) ;
#57500 = CARTESIAN_POINT('Ctrl Pts',(-23.7101786105686,-2.97527429200802,
-9.44725623350041)) ;
#57501 = CARTESIAN_POINT('Ctrl Pts',(-23.7119047187706,-2.98673786471755,
-9.44811328134859)) ;
#57502 = CARTESIAN_POINT('Ctrl Pts',(-23.7231965051006,-3.0618162915894,-9.4537590304828)) ;
#57503 = CARTESIAN_POINT('Ctrl Pts',(-23.7746504249845,-3.39437532880271,
-9.47516001099938)) ;
#57504 = CARTESIAN_POINT('Ctrl Pts',(-23.9939151254337,-4.81167572162242,
-9.56642109048687)) ;
#57505 = CARTESIAN_POINT('Ctrl Pts',(-24.7425357318122,-9.62933838762751,
-9.868352084219)) ;
#57506 = CARTESIAN_POINT('Ctrl Pts',(-25.118894856561,-12.051377463681,-10.0201542187415)) ;
#57507 = CARTESIAN_POINT('Ctrl Pts',(-25.4578393533391,-14.2320211893607,
-10.1565867698155)) ;
#57508 = CARTESIAN_POINT('Ctrl Pts',(-25.764155502917,-16.2025431678313,-10.279793802243)) ;
#57509 = CARTESIAN_POINT('',(-21.124963114758,-2.97427793718828,-14.323080387775)) ;
#57510 = CARTESIAN_POINT('Origin',(-5.46365993374796E-16,-2.97427793741672,
0.)) ;
#57511 = CARTESIAN_POINT('',(-22.9669830516588,-16.2025431678318,-15.5558207401585)) ;
#57512 = CARTESIAN_POINT('Ctrl Pts',(-22.9669830516587,-16.2025431678316,
-15.5558207401585)) ;
#57513 = CARTESIAN_POINT('Ctrl Pts',(-22.9652569821592,-16.1901242777138,
-15.5546586379788)) ;
#57514 = CARTESIAN_POINT('Ctrl Pts',(-22.9635303524359,-16.1777013719743,
-15.5534961631374)) ;
#57515 = CARTESIAN_POINT('Ctrl Pts',(-22.6692388096402,-14.0603095716988,
-15.355361512148)) ;
#57516 = CARTESIAN_POINT('Ctrl Pts',(-22.3372169635415,-11.6718894981187,
-15.131954939375)) ;
#57517 = CARTESIAN_POINT('Ctrl Pts',(-22.0120512929729,-9.33411011503439,
-14.913555876619)) ;
#57518 = CARTESIAN_POINT('Ctrl Pts',(-21.8080750291336,-7.86735711606076,
-14.7764750775493)) ;
#57519 = CARTESIAN_POINT('Ctrl Pts',(-21.4599896090463,-5.36751530388756,
-14.5434937228485)) ;
#57520 = CARTESIAN_POINT('Ctrl Pts',(-21.3180158530842,-4.34873938710956,
-14.4487170165588)) ;
#57521 = CARTESIAN_POINT('Ctrl Pts',(-21.1820786906682,-3.37673005385096,
-14.3589999273775)) ;
#57522 = CARTESIAN_POINT('Ctrl Pts',(-21.149541406992,-3.1449171459073,-14.3377772656239)) ;
#57523 = CARTESIAN_POINT('Ctrl Pts',(-21.1331050331298,-3.02961255818415,
-14.3275930192541)) ;
#57524 = CARTESIAN_POINT('Ctrl Pts',(-21.1314398779441,-3.01796480514944,
-14.3265713108627)) ;
#57525 = CARTESIAN_POINT('Ctrl Pts',(-21.1291068134075,-3.00177651940637,
-14.3251790442246)) ;
#57526 = CARTESIAN_POINT('Ctrl Pts',(-21.1281521135327,-2.99518000535374,
-14.3246176232549)) ;
#57527 = CARTESIAN_POINT('Ctrl Pts',(-21.1268583161178,-2.98636255210082,
-14.3238932357542)) ;
#57528 = CARTESIAN_POINT('Ctrl Pts',(-21.1259639730245,-2.98029308314374,
-14.3234001531875)) ;
#57529 = CARTESIAN_POINT('Ctrl Pts',(-21.1252964678625,-2.9760653941696,-14.3231224034572)) ;
#57530 = CARTESIAN_POINT('Ctrl Pts',(-21.1252289897392,-2.97516395667663,
-14.3229527870938)) ;
#57531 = CARTESIAN_POINT('Ctrl Pts',(-21.1249915865035,-2.97437281950653,
-14.3230667237568)) ;
#57532 = CARTESIAN_POINT('Ctrl Pts',(-21.1249773504602,-2.97432537843874,
-14.3230735560448)) ;
#57533 = CARTESIAN_POINT('Ctrl Pts',(-21.1249631144169,-2.97427793737095,
-14.3230803883327)) ;
#57534 = CARTESIAN_POINT('',(-22.9519520657146,-16.2025431678318,-15.577989785857)) ;
#57535 = CARTESIAN_POINT('Origin',(0.742789062672589,-21.5586464785791,0.503623480791376)) ;
#57536 = CARTESIAN_POINT('Ctrl Pts',(-21.124963114225,-2.9742779367314,-14.3230803884248)) ;
#57537 = CARTESIAN_POINT('Ctrl Pts',(-21.1249638884685,-2.97432614272334,
-14.3230936391942)) ;
#57538 = CARTESIAN_POINT('Ctrl Pts',(-21.1249646627119,-2.97437434871528,
-14.3231068899635)) ;
#57539 = CARTESIAN_POINT('Ctrl Pts',(-21.1249800549334,-2.97533270010394,
-14.32337031973)) ;
#57540 = CARTESIAN_POINT('Ctrl Pts',(-21.1263277956509,-2.98566687891167,
-14.3244679902124)) ;
#57541 = CARTESIAN_POINT('Ctrl Pts',(-21.1418861653829,-3.10454524903057,
-14.3370142074003)) ;
#57542 = CARTESIAN_POINT('Ctrl Pts',(-21.2400732682184,-3.81755457323848,
-14.4050797447424)) ;
#57543 = CARTESIAN_POINT('Ctrl Pts',(-21.6283862075553,-6.63747712966605,
-14.6742953410927)) ;
#57544 = CARTESIAN_POINT('Ctrl Pts',(-22.8396016024952,-15.3906091490516,
-15.5012780450194)) ;
#57545 = CARTESIAN_POINT('Ctrl Pts',(-22.9519520656995,-16.2025431677232,
-15.5779897858469)) ;
#57546 = CARTESIAN_POINT('',(-17.5520343210229,-2.97427793967815,-18.5294573479495)) ;
#57547 = CARTESIAN_POINT('Origin',(-5.46365993374796E-16,-2.97427793741672,
0.)) ;
#57548 = CARTESIAN_POINT('',(-19.0859861185405,-16.2025431678318,-20.1293567527133)) ;
#57549 = CARTESIAN_POINT('Ctrl Pts',(-19.0859861185421,-16.2025431678318,
-20.1293567527118)) ;
#57550 = CARTESIAN_POINT('Ctrl Pts',(-19.0846371298263,-16.1908759391215,
-20.1279419167462)) ;
#57551 = CARTESIAN_POINT('Ctrl Pts',(-19.0832882729851,-16.179209871745,-20.1265272238852)) ;
#57552 = CARTESIAN_POINT('Ctrl Pts',(-18.8385520769211,-14.0625257558835,
-19.8698466324083)) ;
#57553 = CARTESIAN_POINT('Ctrl Pts',(-18.5623287580252,-11.6741934643914,
-19.5802988659292)) ;
#57554 = CARTESIAN_POINT('Ctrl Pts',(-18.2917016367397,-9.33630026614505,
-19.297090878332)) ;
#57555 = CARTESIAN_POINT('Ctrl Pts',(-18.1219041184186,-7.86904147581327,
-19.1193046978973)) ;
#57556 = CARTESIAN_POINT('Ctrl Pts',(-17.8319562334904,-5.3684674257714,-18.8168533991059)) ;
#57557 = CARTESIAN_POINT('Ctrl Pts',(-17.7136507220211,-4.34947290189771,
-18.6937457899545)) ;
#57558 = CARTESIAN_POINT('Ctrl Pts',(-17.6001235387096,-3.37699090193947,
-18.5768464727248)) ;
#57559 = CARTESIAN_POINT('Ctrl Pts',(-17.5728888219343,-3.14500297387669,
-18.5491043446499)) ;
#57560 = CARTESIAN_POINT('Ctrl Pts',(-17.5590180714718,-3.02963135488066,
-18.5356169375373)) ;
#57561 = CARTESIAN_POINT('Ctrl Pts',(-17.5576110433959,-3.01797986462699,
-18.5342607116337)) ;
#57562 = CARTESIAN_POINT('Ctrl Pts',(-17.5556314417978,-3.00178831577416,
-18.5323990614106)) ;
#57563 = CARTESIAN_POINT('Ctrl Pts',(-17.5548199352069,-2.99519321590349,
-18.5316456859648)) ;
#57564 = CARTESIAN_POINT('Ctrl Pts',(-17.5537115426901,-2.98637094041825,
-18.530659528573)) ;
#57565 = CARTESIAN_POINT('Ctrl Pts',(-17.5529448973719,-2.98030761516333,
-18.5299863859087)) ;
#57566 = CARTESIAN_POINT('Ctrl Pts',(-17.5523517824303,-2.97607173941054,
-18.5295706214556)) ;
#57567 = CARTESIAN_POINT('Ctrl Pts',(-17.5523287283435,-2.97516246709807,
-18.5293826094285)) ;
#57568 = CARTESIAN_POINT('Ctrl Pts',(-17.5520658014124,-2.97437252302452,
-18.5294493569053)) ;
#57569 = CARTESIAN_POINT('Ctrl Pts',(-17.5520500614881,-2.97432523361278,
-18.5294533526932)) ;
#57570 = CARTESIAN_POINT('Ctrl Pts',(-17.5520343215638,-2.97427794420103,
-18.529457348481)) ;
#57571 = CARTESIAN_POINT('',(-19.066540859179,-16.2025431678318,-20.1477762807805)) ;
#57572 = CARTESIAN_POINT('Origin',(0.617158905796334,-21.5586464785791,0.651526735465776)) ;
#57573 = CARTESIAN_POINT('Ctrl Pts',(-17.5520343215638,-2.97427794420103,
-18.529457348481)) ;
#57574 = CARTESIAN_POINT('Ctrl Pts',(-17.5520328590378,-2.97432632137793,
-18.5294698987708)) ;
#57575 = CARTESIAN_POINT('Ctrl Pts',(-17.5520313965119,-2.97437469855482,
-18.5294824490605)) ;
#57576 = CARTESIAN_POINT('Ctrl Pts',(-17.5519578549723,-2.97680729268956,
-18.5301135268382)) ;
#57577 = CARTESIAN_POINT('Ctrl Pts',(-17.5524313112944,-2.97933811808545,
-18.5302491313957)) ;
#57578 = CARTESIAN_POINT('Ctrl Pts',(-17.5558459413838,-3.01332488184634,
-18.5348583870864)) ;
#57579 = CARTESIAN_POINT('Ctrl Pts',(-17.570404533859,-3.14290217484017,-18.5509727463816)) ;
#57580 = CARTESIAN_POINT('Ctrl Pts',(-17.6901444286037,-4.20807339287134,
-18.6833787023212)) ;
#57581 = CARTESIAN_POINT('Ctrl Pts',(-18.2802487121423,-9.35159400823905,
-19.3114692894703)) ;
#57582 = CARTESIAN_POINT('Ctrl Pts',(-18.5673745153853,-11.854831316873,-19.6172084675867)) ;
#57583 = CARTESIAN_POINT('Ctrl Pts',(-18.8312173562081,-14.1531923295863,
-19.8977192805209)) ;
#57584 = CARTESIAN_POINT('Ctrl Pts',(-19.066540859178,-16.2025431678313,-20.1477762807813)) ;
#57585 = CARTESIAN_POINT('',(-13.1583919092399,-2.97427793887167,-21.8694174767368)) ;
#57586 = CARTESIAN_POINT('Origin',(-5.46365993374796E-16,-2.97427793741672,
0.)) ;
#57587 = CARTESIAN_POINT('',(-14.312549687069,-16.2025431678318,-23.7616664156853)) ;
#57588 = CARTESIAN_POINT('Ctrl Pts',(-14.3125496870692,-16.2025431678318,
-23.7616664156852)) ;
#57589 = CARTESIAN_POINT('Ctrl Pts',(-14.3114173894645,-16.1895058181297,
-23.7597983459377)) ;
#57590 = CARTESIAN_POINT('Ctrl Pts',(-14.3102852112603,-16.1764698839562,
-23.7579304811446)) ;
#57591 = CARTESIAN_POINT('Ctrl Pts',(-14.1263382038808,-14.0585051121798,
-23.4544564647785)) ;
#57592 = CARTESIAN_POINT('Ctrl Pts',(-13.9188030305551,-11.6700134993328,
-23.1122755929955)) ;
#57593 = CARTESIAN_POINT('Ctrl Pts',(-13.715401930735,-9.33232681200154,-22.7775418330419)) ;
#57594 = CARTESIAN_POINT('Ctrl Pts',(-13.5878725388209,-7.86598567539764,
-22.5675423048878)) ;
#57595 = CARTESIAN_POINT('Ctrl Pts',(-13.3698368359399,-5.36674011422468,
-22.2100223430801)) ;
#57596 = CARTESIAN_POINT('Ctrl Pts',(-13.2807960510996,-4.34814220861965,
-22.0644176439079)) ;
#57597 = CARTESIAN_POINT('Ctrl Pts',(-13.1951275032717,-3.37651773024291,
-21.9259692143185)) ;
#57598 = CARTESIAN_POINT('Ctrl Pts',(-13.1745211431796,-3.14484730369312,
-21.8930663287957)) ;
#57599 = CARTESIAN_POINT('Ctrl Pts',(-13.1638850913661,-3.02959728845171,
-21.8769295999609)) ;
#57600 = CARTESIAN_POINT('Ctrl Pts',(-13.1628031114733,-3.01795255159799,
-21.8753035694779)) ;
#57601 = CARTESIAN_POINT('Ctrl Pts',(-13.1612705151022,-3.00176698296443,
-21.8730607421964)) ;
#57602 = CARTESIAN_POINT('Ctrl Pts',(-13.1606396748887,-2.99516939089294,
-21.8721501992151)) ;
#57603 = CARTESIAN_POINT('Ctrl Pts',(-13.1597699751221,-2.98635593952167,
-21.8709500794992)) ;
#57604 = CARTESIAN_POINT('Ctrl Pts',(-13.1591647786055,-2.98028104303356,
-21.8701263162042)) ;
#57605 = CARTESIAN_POINT('Ctrl Pts',(-13.1586761512808,-2.97606009736442,
-21.869594940972)) ;
#57606 = CARTESIAN_POINT('Ctrl Pts',(-13.1586802925452,-2.9751648529284,-21.8694173912168)) ;
#57607 = CARTESIAN_POINT('Ctrl Pts',(-13.158422831361,-2.97437304087061,-21.8694174679499)) ;
#57608 = CARTESIAN_POINT('Ctrl Pts',(-13.1584073704168,-2.97432549132609,
-21.8694174725579)) ;
#57609 = CARTESIAN_POINT('Ctrl Pts',(-13.1583919094726,-2.97427794178158,
-21.8694174771658)) ;
#57610 = CARTESIAN_POINT('',(-14.2895993930079,-16.2025431678318,-23.7754751494576)) ;
#57611 = CARTESIAN_POINT('Origin',(0.462671084407919,-21.5586464785791,0.768965324109761)) ;
#57612 = CARTESIAN_POINT('Ctrl Pts',(-13.1583919094726,-2.97427794178157,
-21.8694174771658)) ;
#57613 = CARTESIAN_POINT('Ctrl Pts',(-13.1583867628863,-2.97432607736403,
-21.8694299862965)) ;
#57614 = CARTESIAN_POINT('Ctrl Pts',(-13.1583816162999,-2.9743742129465,-21.8694424954271)) ;
#57615 = CARTESIAN_POINT('Ctrl Pts',(-13.1582827830485,-2.97529859190629,
-21.8696827164154)) ;
#57616 = CARTESIAN_POINT('Ctrl Pts',(-13.1590495899011,-2.98568101501634,
-21.8712515447568)) ;
#57617 = CARTESIAN_POINT('Ctrl Pts',(-13.1673405936747,-3.09725857703815,
-21.8880811230034)) ;
#57618 = CARTESIAN_POINT('Ctrl Pts',(-13.2225454665839,-3.7480304421894,-21.9821187438248)) ;
#57619 = CARTESIAN_POINT('Ctrl Pts',(-13.4559147992043,-6.49920651633227,
-22.379675795358)) ;
#57620 = CARTESIAN_POINT('Ctrl Pts',(-14.2193462265786,-15.3848234289498,
-23.6578464502457)) ;
#57621 = CARTESIAN_POINT('Ctrl Pts',(-14.2895993929987,-16.2025431677231,
-23.7754751494418)) ;
#57622 = CARTESIAN_POINT('',(-8.14947771652619,-2.97427793741671,-24.1867879501258)) ;
#57623 = CARTESIAN_POINT('Origin',(-5.46365993374796E-16,-2.97427793741672,
0.)) ;
#57624 = CARTESIAN_POINT('',(-8.8698743394829,-16.2025431678319,-26.2829069662568)) ;
#57625 = CARTESIAN_POINT('Ctrl Pts',(-8.8698743394858,-16.2025431678319,-26.2829069662558)) ;
#57626 = CARTESIAN_POINT('Ctrl Pts',(-8.8690475992033,-16.1872381291413,-26.2804794906608)) ;
#57627 = CARTESIAN_POINT('Ctrl Pts',(-8.8682209482893,-16.1719348447295,-26.2780522951228)) ;
#57628 = CARTESIAN_POINT('Ctrl Pts',(-8.75369775126741,-14.0518506209721,
-25.9417940804283)) ;
#57629 = CARTESIAN_POINT('Ctrl Pts',(-8.62455882373438,-11.6630949877703,
-25.5629575129557)) ;
#57630 = CARTESIAN_POINT('Ctrl Pts',(-8.49788878968684,-9.32575037810072,
-25.1923789033979)) ;
#57631 = CARTESIAN_POINT('Ctrl Pts',(-8.41856649585192,-7.8609282885068,-24.9601150006645)) ;
#57632 = CARTESIAN_POINT('Ctrl Pts',(-8.28260316417309,-5.36388181533702,
-24.5644312808462)) ;
#57633 = CARTESIAN_POINT('Ctrl Pts',(-8.22698003060744,-4.34594047322709,
-24.4031938195724)) ;
#57634 = CARTESIAN_POINT('Ctrl Pts',(-8.17315345603937,-3.37573518238573,
-24.2497910871311)) ;
#57635 = CARTESIAN_POINT('Ctrl Pts',(-8.16013095169145,-3.14458998608287,
-24.213310806901)) ;
#57636 = CARTESIAN_POINT('Ctrl Pts',(-8.15322417016401,-3.02954094887778,
-24.1952965060488)) ;
#57637 = CARTESIAN_POINT('Ctrl Pts',(-8.15251766614579,-3.01790731126877,
-24.1934776472756)) ;
#57638 = CARTESIAN_POINT('Ctrl Pts',(-8.15150361548596,-3.00173213555065,
-24.1909594376427)) ;
#57639 = CARTESIAN_POINT('Ctrl Pts',(-8.15108302267982,-2.99513137012668,
-24.1899340908212)) ;
#57640 = CARTESIAN_POINT('Ctrl Pts',(-8.15049249698612,-2.98633283447704,
-24.1885774200603)) ;
#57641 = CARTESIAN_POINT('Ctrl Pts',(-8.15007714725426,-2.98023825569031,
-24.1876398039442)) ;
#57642 = CARTESIAN_POINT('Ctrl Pts',(-8.14968298797736,-2.97566568479222,
-24.1869641494673)) ;
#57643 = CARTESIAN_POINT('Ctrl Pts',(-8.1495760041458,-2.97458686961963,-24.1868094545128)) ;
#57644 = CARTESIAN_POINT('Ctrl Pts',(-8.14950796797829,-2.97437302247926,
-24.1867945689326)) ;
#57645 = CARTESIAN_POINT('Ctrl Pts',(-8.14949284226742,-2.97432548027622,
-24.1867912595821)) ;
#57646 = CARTESIAN_POINT('Ctrl Pts',(-8.14947771655654,-2.97427793807318,
-24.1867879502316)) ;
#57647 = CARTESIAN_POINT('',(-8.84449214097162,-16.2025431678319,-26.2914592246877)) ;
#57648 = CARTESIAN_POINT('Origin',(0.286549277334558,-21.5586464785791,0.850447948841961)) ;
#57649 = CARTESIAN_POINT('Ctrl Pts',(-8.14947771655655,-2.97427793807318,
-24.1867879502316)) ;
#57650 = CARTESIAN_POINT('Ctrl Pts',(-8.14946923078658,-2.97432589067353,
-24.1867992877722)) ;
#57651 = CARTESIAN_POINT('Ctrl Pts',(-8.14946074501662,-2.97437384327389,
-24.1868106253128)) ;
#57652 = CARTESIAN_POINT('Ctrl Pts',(-8.14929875494501,-2.97528923989621,
-24.1870270545849)) ;
#57653 = CARTESIAN_POINT('Ctrl Pts',(-8.14979835399925,-2.98748257149445,
-24.1890145855308)) ;
#57654 = CARTESIAN_POINT('Ctrl Pts',(-8.15269430516147,-3.05983243148465,
-24.2008307822515)) ;
#57655 = CARTESIAN_POINT('Ctrl Pts',(-8.16894924936113,-3.37814059840374,
-24.2516329420915)) ;
#57656 = CARTESIAN_POINT('Ctrl Pts',(-8.24032645255946,-4.7768625642409,-24.4748868920346)) ;
#57657 = CARTESIAN_POINT('Ctrl Pts',(-8.4957008254956,-9.61051691549516,-25.243464810217)) ;
#57658 = CARTESIAN_POINT('Ctrl Pts',(-8.62394445730424,-12.0381139511629,
-25.6294704668798)) ;
#57659 = CARTESIAN_POINT('Ctrl Pts',(-8.7398048631378,-14.2266206439564,-25.9773756898256)) ;
#57660 = CARTESIAN_POINT('Ctrl Pts',(-8.84449214096946,-16.2025431678314,
-26.2914592246884)) ;
#57661 = CARTESIAN_POINT('',(-2.75950295924795,-2.97427793707758,-25.3732111056427)) ;
#57662 = CARTESIAN_POINT('Origin',(-5.46365993374796E-16,-2.97427793741672,
0.)) ;
#57663 = CARTESIAN_POINT('',(-3.01245352594241,-16.2025431678319,-27.5751879984373)) ;
#57664 = CARTESIAN_POINT('Ctrl Pts',(-3.01245352594352,-16.2025431678319,
-27.5751879984372)) ;
#57665 = CARTESIAN_POINT('Ctrl Pts',(-3.01213020923632,-16.185215473181,-27.5723027580066)) ;
#57666 = CARTESIAN_POINT('Ctrl Pts',(-3.01180686736354,-16.1678868184851,
-27.5694173585072)) ;
#57667 = CARTESIAN_POINT('Ctrl Pts',(-2.97221120494068,-14.0459096503381,
-27.2160863999648)) ;
#57668 = CARTESIAN_POINT('Ctrl Pts',(-2.92752542896347,-11.6569178583153,
-26.8183064787745)) ;
#57669 = CARTESIAN_POINT('Ctrl Pts',(-2.88348538207021,-9.31987893564895,
-26.4292124476807)) ;
#57670 = CARTESIAN_POINT('Ctrl Pts',(-2.85597258225044,-7.85641330793526,
-26.1855526842642)) ;
#57671 = CARTESIAN_POINT('Ctrl Pts',(-2.80828475893858,-5.36133051516146,
-25.7702187256031)) ;
#57672 = CARTESIAN_POINT('Ctrl Pts',(-2.78863406182219,-4.34397548551647,
-25.6008912291156)) ;
#57673 = CARTESIAN_POINT('Ctrl Pts',(-2.76906671893031,-3.37503715205337,
-25.4397147951663)) ;
#57674 = CARTESIAN_POINT('Ctrl Pts',(-2.76420013559178,-3.14436060318559,
-25.4013659265098)) ;
#57675 = CARTESIAN_POINT('Ctrl Pts',(-2.76133149427244,-3.02949078756967,
-25.3823177938562)) ;
#57676 = CARTESIAN_POINT('Ctrl Pts',(-2.76103271954395,-3.0178669010488,-25.3803912020351)) ;
#57677 = CARTESIAN_POINT('Ctrl Pts',(-2.76058392755013,-3.00170195861387,
-25.3777155776922)) ;
#57678 = CARTESIAN_POINT('Ctrl Pts',(-2.76039352479921,-2.9951002807134,-25.3766236408899)) ;
#57679 = CARTESIAN_POINT('Ctrl Pts',(-2.76010875449308,-2.98631499743371,
-25.3751739431355)) ;
#57680 = CARTESIAN_POINT('Ctrl Pts',(-2.75990408935368,-2.98020400131968,
-25.3741662567881)) ;
#57681 = CARTESIAN_POINT('Ctrl Pts',(-2.75966514631604,-2.97566119972773,
-25.373426601311)) ;
#57682 = CARTESIAN_POINT('Ctrl Pts',(-2.75959564554254,-2.97461343441426,
-25.3732575699952)) ;
#57683 = CARTESIAN_POINT('Ctrl Pts',(-2.75952938647569,-2.97437348082648,
-25.3732243344283)) ;
#57684 = CARTESIAN_POINT('Ctrl Pts',(-2.75951619495104,-2.97432570844283,
-25.3732177175531)) ;
#57685 = CARTESIAN_POINT('Ctrl Pts',(-2.75950300342517,-2.97427793606106,
-25.3732111006667)) ;
#57686 = CARTESIAN_POINT('',(-2.98582626636701,-16.2025431678319,-27.5780838874313)) ;
#57687 = CARTESIAN_POINT('Origin',(0.0970287445296876,-21.5586464785792,0.892164572691307)) ;
#57688 = CARTESIAN_POINT('Ctrl Pts',(-2.75950291268683,-2.97427793673757,
-25.3732111106492)) ;
#57689 = CARTESIAN_POINT('Ctrl Pts',(-2.75949693136208,-2.97432677662352,
-25.3732199926138)) ;
#57690 = CARTESIAN_POINT('Ctrl Pts',(-2.75949095003733,-2.97437561650947,
-25.3732288745783)) ;
#57691 = CARTESIAN_POINT('Ctrl Pts',(-2.75892375064498,-2.97900702423292,
-25.3740711369728)) ;
#57692 = CARTESIAN_POINT('Ctrl Pts',(-2.75932604494419,-2.98364704831612,
-25.3748094127723)) ;
#57693 = CARTESIAN_POINT('Ctrl Pts',(-2.75952661218359,-3.04515584041083,
-25.3851542688191)) ;
#57694 = CARTESIAN_POINT('Ctrl Pts',(-2.76315465789757,-3.28410263517818,
-25.4250316993994)) ;
#57695 = CARTESIAN_POINT('Ctrl Pts',(-2.78251290289041,-4.56104030220253,
-25.6381409650497)) ;
#57696 = CARTESIAN_POINT('Ctrl Pts',(-2.86857365834589,-9.50103938481345,
-26.4613669104021)) ;
#57697 = CARTESIAN_POINT('Ctrl Pts',(-2.91138738464896,-11.9608037313374,
-26.8712784094001)) ;
#57698 = CARTESIAN_POINT('Ctrl Pts',(-2.95055606709738,-14.1953706426329,
-27.2436316384425)) ;
#57699 = CARTESIAN_POINT('Ctrl Pts',(-2.98582626636797,-16.2025431678314,
-27.5780838874311)) ;
#57700 = CARTESIAN_POINT('Origin',(-5.46365993374796E-16,-2.97427793741672,
0.)) ;
#57701 = CARTESIAN_POINT('',(26.7317316862594,-16.2025431678319,7.40813002376185)) ;
#57702 = CARTESIAN_POINT('Ctrl Pts',(26.7317316862594,-16.2025431678314,7.40813002376151)) ;
#57703 = CARTESIAN_POINT('Ctrl Pts',(26.6708612250771,-15.8258476727767,7.39144313065645)) ;
#57704 = CARTESIAN_POINT('Ctrl Pts',(26.6087613235262,-15.4415494924405,7.37442275828496)) ;
#57705 = CARTESIAN_POINT('Ctrl Pts',(26.3177228462478,-13.6405242351605,7.29467562226099)) ;
#57706 = CARTESIAN_POINT('Ctrl Pts',(26.0771464558663,-12.1518647220656,7.22881355838971)) ;
#57707 = CARTESIAN_POINT('Ctrl Pts',(25.792202821699,-10.3888908916882,7.15094619732042)) ;
#57708 = CARTESIAN_POINT('Ctrl Pts',(25.7373039946257,-10.0492376710507,7.13595081080411)) ;
#57709 = CARTESIAN_POINT('Ctrl Pts',(25.6751992047838,-9.66501669817754,7.11899639910692)) ;
#57710 = CARTESIAN_POINT('Ctrl Pts',(25.6670200785919,-9.61441555997111,7.11676371273239)) ;
#57711 = CARTESIAN_POINT('Ctrl Pts',(25.655407176928,-9.54257140038981,7.11359397120237)) ;
#57712 = CARTESIAN_POINT('Ctrl Pts',(25.6520195340659,-9.52161349076768,7.11266932544962)) ;
#57713 = CARTESIAN_POINT('Ctrl Pts',(25.5946244020356,-9.16653613429363,7.09700475867469)) ;
#57714 = CARTESIAN_POINT('Ctrl Pts',(25.4026983078924,-7.97911008179591,7.04458112870836)) ;
#57715 = CARTESIAN_POINT('Ctrl Pts',(25.0403950796436,-5.73851073762623,6.94620342034088)) ;
#57716 = CARTESIAN_POINT('Ctrl Pts',(24.876091691589,-4.72268532357717,6.90176444040087)) ;
#57717 = CARTESIAN_POINT('Ctrl Pts',(24.6906989359728,-3.57769528729753,6.85238733933921)) ;
#57718 = CARTESIAN_POINT('Ctrl Pts',(24.6384207630783,-3.25519700220501,6.83869725874935)) ;
#57719 = CARTESIAN_POINT('Ctrl Pts',(24.6073454773866,-3.06433572454096,6.83108487113129)) ;
#57720 = CARTESIAN_POINT('Ctrl Pts',(24.6038284005659,-3.04276136762821,6.83024032654945)) ;
#57721 = CARTESIAN_POINT('Ctrl Pts',(24.5986470322512,-3.01110082456801,6.82907309089495)) ;
#57722 = CARTESIAN_POINT('Ctrl Pts',(24.5972152123349,-3.00236268573874,6.8287573880774)) ;
#57723 = CARTESIAN_POINT('Ctrl Pts',(24.5949512353083,-2.9886302619033,6.82831094889558)) ;
#57724 = CARTESIAN_POINT('Ctrl Pts',(24.5937055045486,-2.98105415711827,6.82805278954538)) ;
#57725 = CARTESIAN_POINT('Ctrl Pts',(24.5927170642124,-2.9753008951146,6.82800959104032)) ;
#57726 = CARTESIAN_POINT('Ctrl Pts',(24.5926019604562,-2.97464733466745,6.82801483559427)) ;
#57727 = CARTESIAN_POINT('Ctrl Pts',(24.5925339353042,-2.9742779365593,6.82802848779065)) ;
#57728 = CARTESIAN_POINT('',(26.724566134977,-16.2025431678319,7.43393800702995)) ;
#57729 = CARTESIAN_POINT('Origin',(-0.864714158790687,-21.5586464785792,-0.240086704374448)) ;
#57730 = CARTESIAN_POINT('Ctrl Pts',(24.5925339349735,-2.97427793447466,6.82802848788166)) ;
#57731 = CARTESIAN_POINT('Ctrl Pts',(24.5922903959867,-2.97295544059358,6.82807736481932)) ;
#57732 = CARTESIAN_POINT('Ctrl Pts',(24.5926502825679,-2.97527517096814,6.8282340058834)) ;
#57733 = CARTESIAN_POINT('Ctrl Pts',(24.5947125268534,-2.98908868346097,6.8294578061479)) ;
#57734 = CARTESIAN_POINT('Ctrl Pts',(24.5969055942541,-3.00247119052961,6.82994048762188)) ;
#57735 = CARTESIAN_POINT('Ctrl Pts',(24.6100866411951,-3.08518510694711,6.834269953955)) ;
#57736 = CARTESIAN_POINT('Ctrl Pts',(24.6266891374417,-3.18867973050429,6.83929132521917)) ;
#57737 = CARTESIAN_POINT('Ctrl Pts',(24.6520865382055,-3.34683414658513,6.84686946441176)) ;
#57738 = CARTESIAN_POINT('Ctrl Pts',(24.6617947563325,-3.40723155602974,6.84973021442313)) ;
#57739 = CARTESIAN_POINT('Ctrl Pts',(24.6690099532311,-3.45211719949212,6.85185507493831)) ;
#57740 = CARTESIAN_POINT('Ctrl Pts',(24.6704849089357,-3.46129178275174,6.85228875962351)) ;
#57741 = CARTESIAN_POINT('Ctrl Pts',(24.8262885492609,-4.43038592304249,6.89807351378244)) ;
#57742 = CARTESIAN_POINT('Ctrl Pts',(25.2411322159244,-7.00390438792483,7.01572324021616)) ;
#57743 = CARTESIAN_POINT('Ctrl Pts',(25.621524497974,-9.36314461801283,7.12325426676193)) ;
#57744 = CARTESIAN_POINT('Ctrl Pts',(25.7085353751157,-9.90272468153527,7.14780567066282)) ;
#57745 = CARTESIAN_POINT('Ctrl Pts',(25.7365170082255,-10.0762492014801,7.15570246432779)) ;
#57746 = CARTESIAN_POINT('Ctrl Pts',(25.7399002083209,-10.0972296242141,7.15665721132822)) ;
#57747 = CARTESIAN_POINT('Ctrl Pts',(26.0610066170549,-12.0885198967075,7.24727146087783)) ;
#57748 = CARTESIAN_POINT('Ctrl Pts',(26.409490678682,-14.249170043393,7.3453495476889)) ;
#57749 = CARTESIAN_POINT('Ctrl Pts',(26.7245661349771,-16.2025431678314,7.43393800702949)) ;
#57750 = CARTESIAN_POINT('',(5.97619665355046,-16.2025431678319,27.0878375466411)) ;
#57751 = CARTESIAN_POINT('Ctrl Pts',(5.97619665355081,-16.2025431678314,27.0878375466409)) ;
#57752 = CARTESIAN_POINT('Ctrl Pts',(5.96072272453984,-15.779208956766,27.0186152627304)) ;
#57753 = CARTESIAN_POINT('Ctrl Pts',(5.94488045825097,-15.3459135704608,26.9477650900312)) ;
#57754 = CARTESIAN_POINT('Ctrl Pts',(5.89489453658278,-13.9792379428408,26.7242972853165)) ;
#57755 = CARTESIAN_POINT('Ctrl Pts',(5.85987132786771,-13.0223166999358,26.5678345002262)) ;
#57756 = CARTESIAN_POINT('Ctrl Pts',(5.80809434291493,-11.6092032550686,26.3367939418112)) ;
#57757 = CARTESIAN_POINT('Ctrl Pts',(5.79109467281383,-11.1454992507822,26.2609815488546)) ;
#57758 = CARTESIAN_POINT('Ctrl Pts',(5.76604719586049,-10.4627424983602,26.149359334853)) ;
#57759 = CARTESIAN_POINT('Ctrl Pts',(5.75780507218401,-10.2381528735791,26.1126423647602)) ;
#57760 = CARTESIAN_POINT('Ctrl Pts',(5.74405261756366,-9.86355741108647,26.0514029061754)) ;
#57761 = CARTESIAN_POINT('Ctrl Pts',(5.73849711874685,-9.71227520462928,26.0266713826372)) ;
#57762 = CARTESIAN_POINT('Ctrl Pts',(5.73219963076735,-9.54083766529388,25.9986452802693)) ;
#57763 = CARTESIAN_POINT('Ctrl Pts',(5.73142304793564,-9.51969691584835,25.9951892553716)) ;
#57764 = CARTESIAN_POINT('Ctrl Pts',(5.71641614781068,-9.11120429329879,25.9284104333817)) ;
#57765 = CARTESIAN_POINT('Ctrl Pts',(5.65974887270405,-7.56784943123937,25.6761017421969)) ;
#57766 = CARTESIAN_POINT('Ctrl Pts',(5.57709597367415,-5.33563589821568,25.3113304772533)) ;
#57767 = CARTESIAN_POINT('Ctrl Pts',(5.54998071858407,-4.60671916329358,25.1922440851709)) ;
#57768 = CARTESIAN_POINT('Ctrl Pts',(5.51727804656527,-3.73938880523472,25.0506409639444)) ;
#57769 = CARTESIAN_POINT('Ctrl Pts',(5.50753615464755,-3.48384628708339,25.0089437563574)) ;
#57770 = CARTESIAN_POINT('Ctrl Pts',(5.49667474050161,-3.20573594642881,24.9636211780588)) ;
#57771 = CARTESIAN_POINT('Ctrl Pts',(5.49367323791136,-3.13044865534939,24.9513653690511)) ;
#57772 = CARTESIAN_POINT('Ctrl Pts',(5.49016340863078,-3.04571930373455,24.9376015459661)) ;
#57773 = CARTESIAN_POINT('Ctrl Pts',(5.48924355592997,-3.02334616904155,24.9339656258311)) ;
#57774 = CARTESIAN_POINT('Ctrl Pts',(5.48776174140018,-2.9921585742524,24.9289411704213)) ;
#57775 = CARTESIAN_POINT('Ctrl Pts',(5.48756020827974,-2.98773607317881,24.9282267950638)) ;
#57776 = CARTESIAN_POINT('Ctrl Pts',(5.48695179424486,-2.97700394873062,24.9265194850504)) ;
#57777 = CARTESIAN_POINT('Ctrl Pts',(5.48680471756041,-2.97502954371886,24.9262131248547)) ;
#57778 = CARTESIAN_POINT('Ctrl Pts',(5.48671463550852,-2.97427793387919,24.9261040052127)) ;
#57779 = CARTESIAN_POINT('',(5.95003858478611,-16.2025431678319,27.0935953729785)) ;
#57780 = CARTESIAN_POINT('Origin',(-0.192919915744,-21.5586464785792,-0.876444013123365)) ;
#57781 = CARTESIAN_POINT('Ctrl Pts',(5.48671463550852,-2.97427793387919,24.9261040052127)) ;
#57782 = CARTESIAN_POINT('Ctrl Pts',(5.48655343436942,-2.97293293385127,24.9259087364526)) ;
#57783 = CARTESIAN_POINT('Ctrl Pts',(5.48657474615765,-2.97550366968052,24.9263450877106)) ;
#57784 = CARTESIAN_POINT('Ctrl Pts',(5.48650656002357,-2.98896306265492,24.9286692261902)) ;
#57785 = CARTESIAN_POINT('Ctrl Pts',(5.4870581876998,-3.00225028492091,24.9308273952644)) ;
#57786 = CARTESIAN_POINT('Ctrl Pts',(5.48940856559024,-3.08513378934106,24.9445297544016)) ;
#57787 = CARTESIAN_POINT('Ctrl Pts',(5.49278640846088,-3.18963983843306,24.9617155731815)) ;
#57788 = CARTESIAN_POINT('Ctrl Pts',(5.49706224508616,-3.31975443705721,24.9830972000661)) ;
#57789 = CARTESIAN_POINT('Ctrl Pts',(5.49838046279082,-3.35939593234685,24.9896080397158)) ;
#57790 = CARTESIAN_POINT('Ctrl Pts',(5.49982593417466,-3.4027865871652,24.996734084582)) ;
#57791 = CARTESIAN_POINT('Ctrl Pts',(5.50011019121751,-3.41129002097857,24.9981303867991)) ;
#57792 = CARTESIAN_POINT('Ctrl Pts',(5.53157664010535,-4.35245512534218,25.1526729085225)) ;
#57793 = CARTESIAN_POINT('Ctrl Pts',(5.6231120523299,-6.95923681319167,25.5797509022431)) ;
#57794 = CARTESIAN_POINT('Ctrl Pts',(5.70685056811174,-9.33462644072451,25.9688468798497)) ;
#57795 = CARTESIAN_POINT('Ctrl Pts',(5.72594006926732,-9.87490507692204,26.0573366155415)) ;
#57796 = CARTESIAN_POINT('Ctrl Pts',(5.73156501003844,-10.0341421448734,26.0834176111344)) ;
#57797 = CARTESIAN_POINT('Ctrl Pts',(5.7322996806034,-10.054939175098,26.0868238922277)) ;
#57798 = CARTESIAN_POINT('Ctrl Pts',(5.80304552537078,-12.0575349767993,26.4148222638508)) ;
#57799 = CARTESIAN_POINT('Ctrl Pts',(5.88027610174045,-14.2365603955804,26.7716619766563)) ;
#57800 = CARTESIAN_POINT('Ctrl Pts',(5.9500385847868,-16.2025431678314,27.0935953729783)) ;
#57801 = CARTESIAN_POINT('Origin',(-3.29835915403229E-15,-17.9554309391014,
0.)) ;
#57802 = CARTESIAN_POINT('',(0.494365359100647,-15.9320789705494,-29.3036235215755)) ;
#57803 = CARTESIAN_POINT('',(0.492460255574504,-15.9108622559522,-29.3036555995867)) ;
#57804 = CARTESIAN_POINT('Origin',(-3.92942532412469E-15,-21.3907951629292,
0.)) ;
#57805 = CARTESIAN_POINT('',(5.81660547648255,-15.9320789705494,-28.7247950268312)) ;
#57806 = CARTESIAN_POINT('Origin',(-3.92942532412469E-15,-21.3907951629292,
0.)) ;
#57807 = CARTESIAN_POINT('',(5.81660547648253,-15.9320789705494,-28.7247950268311)) ;
#57808 = CARTESIAN_POINT('',(6.78222025653935,-15.9320789748381,-28.5122470677388)) ;
#57809 = CARTESIAN_POINT('',(6.7803665240703,-15.9108618774105,-28.5126880067314)) ;
#57810 = CARTESIAN_POINT('Origin',(-3.92942532412469E-15,-21.3907951629292,
0.)) ;
#57811 = CARTESIAN_POINT('',(11.8555982263102,-15.9320789748381,-26.8028269993353)) ;
#57812 = CARTESIAN_POINT('Origin',(-3.92942532412469E-15,-21.3907951629292,
0.)) ;
#57813 = CARTESIAN_POINT('',(11.8555981836618,-15.932078964213,-26.8028269424543)) ;
#57814 = CARTESIAN_POINT('',(12.7529460606102,-15.932078986503,-26.3876695044702)) ;
#57815 = CARTESIAN_POINT('',(12.7512304233236,-15.9108618549279,-26.3884982701394)) ;
#57816 = CARTESIAN_POINT('Origin',(-3.92942532412469E-15,-21.3907951629292,
0.)) ;
#57817 = CARTESIAN_POINT('',(17.3402362534815,-15.932078986503,-23.6275885730099)) ;
#57818 = CARTESIAN_POINT('Origin',(-3.92942532412469E-15,-21.3907951629292,
0.)) ;
#57819 = CARTESIAN_POINT('',(17.3402360849801,-15.9320789502307,-23.627588425548)) ;
#57820 = CARTESIAN_POINT('',(18.1273581983811,-15.9320789854432,-23.0292340460187)) ;
#57821 = CARTESIAN_POINT('',(18.1258608416401,-15.9108618569292,-23.0304122763961)) ;
#57822 = CARTESIAN_POINT('Origin',(-3.92942532412468E-15,-21.3907951629292,
0.)) ;
#57823 = CARTESIAN_POINT('',(22.0140643019504,-15.9320789854432,-19.3475504627412)) ;
#57824 = CARTESIAN_POINT('Origin',(-3.92942532412468E-15,-21.3907951629292,
0.)) ;
#57825 = CARTESIAN_POINT('',(22.0140641187248,-15.93207895158,-19.3475503621096)) ;
#57826 = CARTESIAN_POINT('',(22.6541552108272,-15.9320789866943,-18.5939771612252)) ;
#57827 = CARTESIAN_POINT('',(22.6529461354171,-15.9108618551723,-18.595449711334)) ;
#57828 = CARTESIAN_POINT('Origin',(-3.92942532412469E-15,-21.3907951629292,
0.)) ;
#57829 = CARTESIAN_POINT('',(25.6585391321031,-15.9320789866943,-14.1628423910863)) ;
#57830 = CARTESIAN_POINT('Origin',(-3.92942532412469E-15,-21.3907951629292,
0.)) ;
#57831 = CARTESIAN_POINT('',(25.6585389138341,-15.9320789500595,-14.1628423304031)) ;
#57832 = CARTESIAN_POINT('',(26.1216692307926,-15.9320789708932,-13.2892868445522)) ;
#57833 = CARTESIAN_POINT('',(26.1208051637602,-15.9108618761819,-13.290985048708)) ;
#57834 = CARTESIAN_POINT('Origin',(-3.92942532412469E-15,-21.3907951629292,
0.)) ;
#57835 = CARTESIAN_POINT('',(28.103249474609,-15.9320789708932,-8.31589545434586)) ;
#57836 = CARTESIAN_POINT('Origin',(-3.92942532412469E-15,-21.3907951629292,
0.)) ;
#57837 = CARTESIAN_POINT('',(28.1032494677604,-15.9320789699703,-8.31589545421927)) ;
#57838 = CARTESIAN_POINT('',(28.3677629681468,-15.9320789705494,-7.36320397554968)) ;
#57839 = CARTESIAN_POINT('',(28.3672842077332,-15.9108622559523,-7.3650482198151)) ;
#57840 = CARTESIAN_POINT('Origin',(-3.9294253241247E-15,-21.3907951629292,
0.)) ;
#57841 = CARTESIAN_POINT('',(29.2338828322227,-15.9320789705494,-2.08010652476853)) ;
#57842 = CARTESIAN_POINT('Origin',(-3.9294253241247E-15,-21.3907951629292,
0.)) ;
#57843 = CARTESIAN_POINT('',(29.2338828322227,-15.9320789705494,-2.08010652476853)) ;
#57844 = CARTESIAN_POINT('',(29.287411634191,-15.9320789705494,-1.09282586534355)) ;
#57845 = CARTESIAN_POINT('',(29.2873405249314,-15.9108622559522,-1.09472991153979)) ;
#57846 = CARTESIAN_POINT('Origin',(-3.92942532412469E-15,-21.3907951629292,
0.)) ;
#57847 = CARTESIAN_POINT('',(28.9975723124842,-15.9320789705494,4.25294587136481)) ;
#57848 = CARTESIAN_POINT('Origin',(-3.92942532412469E-15,-21.3907951629292,
0.)) ;
#57849 = CARTESIAN_POINT('',(28.9975723124842,-15.9320789705494,4.2529458713648)) ;
#57850 = CARTESIAN_POINT('',(28.837613004449,-15.9320790002153,5.22865180923071)) ;
#57851 = CARTESIAN_POINT('',(28.8379528519801,-15.9108618570888,5.22677686529081)) ;
#57852 = CARTESIAN_POINT('Origin',(-3.9294253241247E-15,-21.3907951629292,
0.)) ;
#57853 = CARTESIAN_POINT('',(27.4053672544904,-15.9320790002153,10.387134791801)) ;
#57854 = CARTESIAN_POINT('Origin',(-3.9294253241247E-15,-21.3907951629292,
0.)) ;
#57855 = CARTESIAN_POINT('',(27.4053669090694,-15.9320789327933,10.3871345576338)) ;
#57856 = CARTESIAN_POINT('',(27.0394003853433,-15.932078979868,11.3056431141676)) ;
#57857 = CARTESIAN_POINT('',(27.0401351051488,-15.9108618606822,11.3038851399891)) ;
#57858 = CARTESIAN_POINT('Origin',(-3.92942532412469E-15,-21.3907951629292,
0.)) ;
#57859 = CARTESIAN_POINT('',(24.531718174094,-15.932078979868,16.0356335344338)) ;
#57860 = CARTESIAN_POINT('Origin',(-3.92942532412469E-15,-21.3907951629292,
0.)) ;
#57861 = CARTESIAN_POINT('',(24.5317180654997,-15.9320789564852,16.0356334188635)) ;
#57862 = CARTESIAN_POINT('',(23.9768550750891,-15.9320789856441,16.8539952692808)) ;
#57863 = CARTESIAN_POINT('',(23.9779505086143,-15.9108618566337,16.8524363191949)) ;
#57864 = CARTESIAN_POINT('Origin',(-3.92942532412468E-15,-21.3907951629292,
0.)) ;
#57865 = CARTESIAN_POINT('',(20.5109930276199,-15.9320789856441,20.9343235106773)) ;
#57866 = CARTESIAN_POINT('Origin',(-3.92942532412468E-15,-21.3907951629292,
0.)) ;
#57867 = CARTESIAN_POINT('',(20.5109929157274,-15.9320789513242,20.9343233307748)) ;
#57868 = CARTESIAN_POINT('',(19.7931787380933,-15.9320789860435,21.6142733149332)) ;
#57869 = CARTESIAN_POINT('',(19.7945836826822,-15.910861856046,21.6129862941042)) ;
#57870 = CARTESIAN_POINT('Origin',(-3.9294253241247E-15,-21.3907951629292,
0.)) ;
#57871 = CARTESIAN_POINT('',(15.5311966688983,-15.9320789860435,24.8541478534821)) ;
#57872 = CARTESIAN_POINT('Origin',(-3.9294253241247E-15,-21.3907951629292,
0.)) ;
#57873 = CARTESIAN_POINT('',(15.5311965964273,-15.9320789508155,24.8541476484462)) ;
#57874 = CARTESIAN_POINT('',(14.6839955520831,-15.9320789746107,25.3638920378233)) ;
#57875 = CARTESIAN_POINT('',(14.6856444121027,-15.9108618692113,25.3629372329525)) ;
#57876 = CARTESIAN_POINT('Origin',(-3.92942532412469E-15,-21.3907951629292,
0.)) ;
#57877 = CARTESIAN_POINT('',(9.82517875536679,-15.9320789746107,27.6118200614346)) ;
#57878 = CARTESIAN_POINT('Origin',(-3.92942532412469E-15,-21.3907951629292,
0.)) ;
#57879 = CARTESIAN_POINT('',(9.82517874764536,-15.9320789645514,27.61181999456)) ;
#57880 = CARTESIAN_POINT('',(8.88820398548747,-15.9320790345093,27.9275227055374)) ;
#57881 = CARTESIAN_POINT('',(8.89001959178239,-15.9108618212313,27.9269444452518)) ;
#57882 = CARTESIAN_POINT('Origin',(-3.9294253241247E-15,-21.3907951629292,
0.)) ;
#57883 = CARTESIAN_POINT('',(3.65974695538204,-15.9320790345093,29.078393125799)) ;
#57884 = CARTESIAN_POINT('Origin',(-3.9294253241247E-15,-21.3907951629292,
0.)) ;
#57885 = CARTESIAN_POINT('',(3.65974705260781,-15.9320788891238,29.0783922312664)) ;
#57886 = CARTESIAN_POINT('',(2.6768116432333,-15.9320789705494,29.1852947223283)) ;
#57887 = CARTESIAN_POINT('',(2.67870904720401,-15.9108622559523,29.1851206343735)) ;
#57888 = CARTESIAN_POINT('Origin',(-3.92942532412468E-15,-21.3907951629292,
0.)) ;
#57889 = CARTESIAN_POINT('',(-2.6768116432333,-15.9320789705494,29.1852947223283)) ;
#57890 = CARTESIAN_POINT('Origin',(-3.92942532412468E-15,-21.3907951629292,
0.)) ;
#57891 = CARTESIAN_POINT('',(-2.67681164323326,-15.9320789705494,29.1852947223282)) ;
#57892 = CARTESIAN_POINT('',(-3.65974695538209,-15.9320790345093,29.078393125799)) ;
#57893 = CARTESIAN_POINT('',(-3.65785635054521,-15.9108618212313,29.0786306642735)) ;
#57894 = CARTESIAN_POINT('Origin',(-3.9294253241247E-15,-21.3907951629292,
0.)) ;
#57895 = CARTESIAN_POINT('',(-8.88820398548748,-15.9320790345093,27.9275227055374)) ;
#57896 = CARTESIAN_POINT('Origin',(-3.9294253241247E-15,-21.3907951629292,
0.)) ;
#57897 = CARTESIAN_POINT('',(-8.88820352164328,-15.9320788891238,27.9275219345056)) ;
#57898 = CARTESIAN_POINT('',(-9.8251787553669,-15.9320789746107,27.6118200614345)) ;
#57899 = CARTESIAN_POINT('',(-9.82338358996211,-15.9108618692113,27.6124586323977)) ;
#57900 = CARTESIAN_POINT('Origin',(-3.92942532412469E-15,-21.3907951629292,
0.)) ;
#57901 = CARTESIAN_POINT('',(-14.6839955520832,-15.9320789746107,25.3638920378232)) ;
#57902 = CARTESIAN_POINT('Origin',(-3.92942532412469E-15,-21.3907951629292,
0.)) ;
#57903 = CARTESIAN_POINT('',(-14.6839955061126,-15.9320789645514,25.3638919886445)) ;
#57904 = CARTESIAN_POINT('',(-15.5311966688983,-15.9320789860435,24.8541478534821)) ;
#57905 = CARTESIAN_POINT('',(-15.5295806974965,-15.9108618560459,24.8551572732861)) ;
#57906 = CARTESIAN_POINT('Origin',(-3.9294253241247E-15,-21.3907951629292,
0.)) ;
#57907 = CARTESIAN_POINT('',(-19.7931787380933,-15.9320789860435,21.6142733149332)) ;
#57908 = CARTESIAN_POINT('Origin',(-3.9294253241247E-15,-21.3907951629292,
0.)) ;
#57909 = CARTESIAN_POINT('',(-19.7931785599191,-15.9320789508155,21.6142731902508)) ;
#57910 = CARTESIAN_POINT('',(-20.5109930276199,-15.9320789856441,20.9343235106773)) ;
#57911 = CARTESIAN_POINT('',(-20.5096318357506,-15.9108618566336,20.935656723591)) ;
#57912 = CARTESIAN_POINT('Origin',(-3.92942532412468E-15,-21.3907951629292,
0.)) ;
#57913 = CARTESIAN_POINT('',(-23.9768550750892,-15.9320789856441,16.8539952692808)) ;
#57914 = CARTESIAN_POINT('Origin',(-3.92942532412468E-15,-21.3907951629292,
0.)) ;
#57915 = CARTESIAN_POINT('',(-23.9768548794545,-15.9320789513242,16.8539951879673)) ;
#57916 = CARTESIAN_POINT('',(-24.531718174094,-15.932078979868,16.0356335344337)) ;
#57917 = CARTESIAN_POINT('',(-24.5306754334589,-15.9108618606822,16.0372282063037)) ;
#57918 = CARTESIAN_POINT('Origin',(-3.92942532412469E-15,-21.3907951629292,
0.)) ;
#57919 = CARTESIAN_POINT('',(-27.0394003853434,-15.932078979868,11.3056431141676)) ;
#57920 = CARTESIAN_POINT('Origin',(-3.92942532412469E-15,-21.3907951629292,
0.)) ;
#57921 = CARTESIAN_POINT('',(-27.0394002287454,-15.9320789564852,11.3056430891418)) ;
#57922 = CARTESIAN_POINT('',(-27.4053672544904,-15.9320790002153,10.387134791801)) ;
#57923 = CARTESIAN_POINT('',(-27.404691820706,-15.9108618570887,10.3889165606763)) ;
#57924 = CARTESIAN_POINT('Origin',(-3.92942532412469E-15,-21.3907951629292,
0.)) ;
#57925 = CARTESIAN_POINT('',(-28.837613004449,-15.9320790002153,5.22865180923068)) ;
#57926 = CARTESIAN_POINT('Origin',(-3.92942532412469E-15,-21.3907951629292,
0.)) ;
#57927 = CARTESIAN_POINT('',(-28.8376125877467,-15.9320789327933,5.22865183179534)) ;
#57928 = CARTESIAN_POINT('',(-28.9975723124843,-15.9320789705494,4.25294587136478)) ;
#57929 = CARTESIAN_POINT('',(-28.9972957564644,-15.9108622559522,4.25483106769728)) ;
#57930 = CARTESIAN_POINT('Origin',(-3.92942532412469E-15,-21.3907951629292,
0.)) ;
#57931 = CARTESIAN_POINT('',(-29.287411634191,-15.9320789705494,-1.09282586534359)) ;
#57932 = CARTESIAN_POINT('Origin',(-3.92942532412469E-15,-21.3907951629292,
0.)) ;
#57933 = CARTESIAN_POINT('',(-29.287411634191,-15.9320789705494,-1.09282586534359)) ;
#57934 = CARTESIAN_POINT('',(-29.2338828322227,-15.9320789705494,-2.08010652476856)) ;
#57935 = CARTESIAN_POINT('',(-29.2340180034144,-15.9108622559522,-2.07820595190936)) ;
#57936 = CARTESIAN_POINT('Origin',(-3.9294253241247E-15,-21.3907951629292,
0.)) ;
#57937 = CARTESIAN_POINT('',(-28.3677629681468,-15.9320789705494,-7.36320397554972)) ;
#57938 = CARTESIAN_POINT('Origin',(-3.9294253241247E-15,-21.3907951629292,
0.)) ;
#57939 = CARTESIAN_POINT('',(-28.3677629681468,-15.9320789705494,-7.3632039755497)) ;
#57940 = CARTESIAN_POINT('',(-28.103249474609,-15.9320789708932,-8.31589545434591)) ;
#57941 = CARTESIAN_POINT('',(-28.1037900199178,-15.9108618761818,-8.31406834735388)) ;
#57942 = CARTESIAN_POINT('Origin',(-3.92942532412469E-15,-21.3907951629292,
0.)) ;
#57943 = CARTESIAN_POINT('',(-26.1216692307926,-15.9320789708932,-13.2892868445522)) ;
#57944 = CARTESIAN_POINT('Origin',(-3.92942532412469E-15,-21.3907951629292,
0.)) ;
#57945 = CARTESIAN_POINT('',(-26.1216692257335,-15.9320789699703,-13.2892868399344)) ;
#57946 = CARTESIAN_POINT('',(-25.658539132103,-15.9320789866943,-14.1628423910863)) ;
#57947 = CARTESIAN_POINT('',(-25.6594595719309,-15.9108618551722,-14.161174141197)) ;
#57948 = CARTESIAN_POINT('Origin',(-3.92942532412469E-15,-21.3907951629292,
0.)) ;
#57949 = CARTESIAN_POINT('',(-22.6541552108272,-15.9320789866943,-18.5939771612253)) ;
#57950 = CARTESIAN_POINT('Origin',(-3.92942532412469E-15,-21.3907951629292,
0.)) ;
#57951 = CARTESIAN_POINT('',(-22.6541550736643,-15.9320789500595,-18.5939769809197)) ;
#57952 = CARTESIAN_POINT('',(-22.0140643019503,-15.9320789854432,-19.3475504627413)) ;
#57953 = CARTESIAN_POINT('',(-22.0153218696111,-15.9108618569291,-19.3461190901096)) ;
#57954 = CARTESIAN_POINT('Origin',(-3.92942532412468E-15,-21.3907951629291,
0.)) ;
#57955 = CARTESIAN_POINT('',(-18.1273581983811,-15.9320789854432,-23.0292340460188)) ;
#57956 = CARTESIAN_POINT('Origin',(-3.92942532412468E-15,-21.3907951629291,
0.)) ;
#57957 = CARTESIAN_POINT('',(-18.1273581078167,-15.93207895158,-23.0292338576138)) ;
#57958 = CARTESIAN_POINT('',(-17.3402362534815,-15.932078986503,-23.6275885730099)) ;
#57959 = CARTESIAN_POINT('',(-17.3417720969185,-15.9108618549278,-23.6264609876381)) ;
#57960 = CARTESIAN_POINT('Origin',(-3.92942532412468E-15,-21.3907951629292,
0.)) ;
#57961 = CARTESIAN_POINT('',(-12.7529460606102,-15.932078986503,-26.3876695044702)) ;
#57962 = CARTESIAN_POINT('Origin',(-3.92942532412468E-15,-21.3907951629292,
0.)) ;
#57963 = CARTESIAN_POINT('',(-12.7529460092534,-15.9320789502307,-26.3876692865248)) ;
#57964 = CARTESIAN_POINT('',(-11.8555982263102,-15.9320789748381,-26.8028269993354)) ;
#57965 = CARTESIAN_POINT('',(-11.8573408147833,-15.9108618774106,-26.8020561967176)) ;
#57966 = CARTESIAN_POINT('Origin',(-3.92942532412469E-15,-21.3907951629292,
0.)) ;
#57967 = CARTESIAN_POINT('',(-6.78222025653932,-15.9320789748381,-28.5122470677388)) ;
#57968 = CARTESIAN_POINT('Origin',(-3.92942532412469E-15,-21.3907951629292,
0.)) ;
#57969 = CARTESIAN_POINT('',(-6.78222025606846,-15.932078964213,-28.5122469966465)) ;
#57970 = CARTESIAN_POINT('',(-5.81660547648251,-15.9320789705494,-28.7247950268312)) ;
#57971 = CARTESIAN_POINT('',(-5.8184729355711,-15.9108622559522,-28.7244168139326)) ;
#57972 = CARTESIAN_POINT('Origin',(-3.9294253241247E-15,-21.3907951629292,
0.)) ;
#57973 = CARTESIAN_POINT('',(-0.494365359100612,-15.9320789705494,-29.3036235215755)) ;
#57974 = CARTESIAN_POINT('Origin',(-3.9294253241247E-15,-21.3907951629292,
0.)) ;
#57975 = CARTESIAN_POINT('',(-0.494365359100623,-15.9320789705494,-29.3036235215755)) ;
#57976 = CARTESIAN_POINT('',(-1.87947417050994E-15,-20.,-29.3077933083081)) ;
#57977 = CARTESIAN_POINT('',(-8.68211344379605E-15,-17.9554309391014,-29.3077933083081)) ;
#57978 = CARTESIAN_POINT('Origin',(-3.67394039744206E-15,-20.,0.)) ;
#57979 = CARTESIAN_POINT('Origin',(-1.4236519040088E-15,-7.75,0.)) ;
#57980 = CARTESIAN_POINT('',(1.88995598193963E-15,1.11022302462516E-15,-30.8653235080594)) ;
#57981 = CARTESIAN_POINT('Origin',(-3.47179281571763E-31,-1.88995598193962E-15,
0.)) ;
#57982 = CARTESIAN_POINT('',(-7.61344957909942E-16,-15.5,-34.0685435652414)) ;
#57983 = CARTESIAN_POINT('',(5.6437440768064E-16,-7.75,-32.4669335366504)) ;
#57984 = CARTESIAN_POINT('Origin',(-2.8473038080176E-15,-15.5,0.)) ;
#57985 = CARTESIAN_POINT('',(-0.0148206788859343,-15.0366437072152,33.9727834182319)) ;
#57986 = CARTESIAN_POINT('',(9.58677831405906E-9,-1.901536240759,31.2582937677921)) ;
#57987 = CARTESIAN_POINT('Ctrl Pts',(-0.0148206796830926,-15.0366437072144,
33.9727834182323)) ;
#57988 = CARTESIAN_POINT('Ctrl Pts',(-0.0147761934970794,-14.9636265798866,
33.9576937635085)) ;
#57989 = CARTESIAN_POINT('Ctrl Pts',(-0.014731452265485,-14.8904290787823,
33.9425668329)) ;
#57990 = CARTESIAN_POINT('Ctrl Pts',(-0.01434327996254,-14.2574947912553,
33.8117651948258)) ;
#57991 = CARTESIAN_POINT('Ctrl Pts',(-0.0139852279340405,-13.6878788033261,
33.6940488603458)) ;
#57992 = CARTESIAN_POINT('Ctrl Pts',(-0.0132371778195199,-12.5352441626078,
33.4558464085617)) ;
#57993 = CARTESIAN_POINT('Ctrl Pts',(-0.0128472164427587,-11.9522255098215,
33.3353602912582)) ;
#57994 = CARTESIAN_POINT('Ctrl Pts',(-0.012031151377517,-10.7794869194086,
33.093003175074)) ;
#57995 = CARTESIAN_POINT('Ctrl Pts',(-0.0116051245489098,-10.1897669817304,
32.9711321761835)) ;
#57996 = CARTESIAN_POINT('Ctrl Pts',(-0.0109330916398328,-9.30518714838486,
32.7883256929664)) ;
#57997 = CARTESIAN_POINT('Ctrl Pts',(-0.0107035427670526,-9.01032721998394,
32.727390201878)) ;
#57998 = CARTESIAN_POINT('Ctrl Pts',(-0.0102317470018941,-8.42144506509216,
32.6056923384334)) ;
#57999 = CARTESIAN_POINT('Ctrl Pts',(-0.00998950899209841,-8.12742283859438,
32.5449299660763)) ;
#58000 = CARTESIAN_POINT('Ctrl Pts',(-0.00949001810971001,-7.54105375785668,
32.4237514523057)) ;
#58001 = CARTESIAN_POINT('Ctrl Pts',(-0.00923278420232808,-7.24870690362007,
32.363335310893)) ;
#58002 = CARTESIAN_POINT('Ctrl Pts',(-0.00869987323933532,-6.66652623865879,
32.2430223714091)) ;
#58003 = CARTESIAN_POINT('Ctrl Pts',(-0.00842423445942805,-6.37669242790047,
32.183125573331)) ;
#58004 = CARTESIAN_POINT('Ctrl Pts',(-0.00799293179098999,-5.94445474907251,
32.0937997182736)) ;
#58005 = CARTESIAN_POINT('Ctrl Pts',(-0.00784617116632075,-5.8007943635198,
32.0641109905068)) ;
#58006 = CARTESIAN_POINT('Ctrl Pts',(-0.00754567856593524,-5.51441598220198,
32.0049282884094)) ;
#58007 = CARTESIAN_POINT('Ctrl Pts',(-0.00739194776214034,-5.37169798643552,
31.9754343140794)) ;
#58008 = CARTESIAN_POINT('Ctrl Pts',(-0.00707620189734833,-5.0873090933607,
31.9166627578568)) ;
#58009 = CARTESIAN_POINT('Ctrl Pts',(-0.00691419331811431,-4.94563819605463,
31.887385175965)) ;
#58010 = CARTESIAN_POINT('Ctrl Pts',(-0.00658008599236392,-4.66344820909719,
31.8290680437289)) ;
#58011 = CARTESIAN_POINT('Ctrl Pts',(-0.00640800046290111,-4.52292911943078,
31.8000284933815)) ;
#58012 = CARTESIAN_POINT('Ctrl Pts',(-0.00605114898957075,-4.24314745782051,
31.7422090635241)) ;
#58013 = CARTESIAN_POINT('Ctrl Pts',(-0.0058664094908114,-4.10388488678362,
31.7134291842014)) ;
#58014 = CARTESIAN_POINT('Ctrl Pts',(-0.00548031482479414,-3.82672097435253,
31.6561507360658)) ;
#58015 = CARTESIAN_POINT('Ctrl Pts',(-0.00527901892921338,-3.68881963287913,
31.6276521672366)) ;
#58016 = CARTESIAN_POINT('Ctrl Pts',(-0.00495976082686647,-3.48306707796744,
31.5851315268619)) ;
#58017 = CARTESIAN_POINT('Ctrl Pts',(-0.00485042867486194,-3.41466613604316,
31.570995848916)) ;
#58018 = CARTESIAN_POINT('Ctrl Pts',(-0.00462466717946779,-3.27824382794845,
31.5428029358115)) ;
#58019 = CARTESIAN_POINT('Ctrl Pts',(-0.00450823986138664,-3.2102224617746,
31.5287457006532)) ;
#58020 = CARTESIAN_POINT('Ctrl Pts',(-0.00426647698023381,-3.07457239569776,
31.5007123783991)) ;
#58021 = CARTESIAN_POINT('Ctrl Pts',(-0.00414115714718083,-3.00694369580828,
31.4867362913064)) ;
#58022 = CARTESIAN_POINT('Ctrl Pts',(-0.00387889601227492,-2.87209205434656,
31.4588679707746)) ;
#58023 = CARTESIAN_POINT('Ctrl Pts',(-0.00374199348527815,-2.80486911270198,
31.4449757373206)) ;
#58024 = CARTESIAN_POINT('Ctrl Pts',(-0.00346465861919957,-2.67661413836906,
31.4184706781625)) ;
#58025 = CARTESIAN_POINT('Ctrl Pts',(-0.0033186339604559,-2.61231067593153,
31.4051817816902)) ;
#58026 = CARTESIAN_POINT('Ctrl Pts',(-0.00307592509832223,-2.51355910906303,
31.3847738705318)) ;
#58027 = CARTESIAN_POINT('Ctrl Pts',(-0.00299104803530146,-2.48025919132693,
31.3778921390891)) ;
#58028 = CARTESIAN_POINT('Ctrl Pts',(-0.00281217424207543,-2.41327667158013,
31.3640495910111)) ;
#58029 = CARTESIAN_POINT('Ctrl Pts',(-0.00271819528239995,-2.37959406952389,
31.3570887743664)) ;
#58030 = CARTESIAN_POINT('Ctrl Pts',(-0.00251912676833825,-2.31222895652059,
31.3431671599055)) ;
#58031 = CARTESIAN_POINT('Ctrl Pts',(-0.00241408123887382,-2.27854645923592,
31.3362063649129)) ;
#58032 = CARTESIAN_POINT('Ctrl Pts',(-0.00224540359278948,-2.22830986861511,
31.3258245156846)) ;
#58033 = CARTESIAN_POINT('Ctrl Pts',(-0.00218730809007332,-2.21161219769834,
31.3223737898337)) ;
#58034 = CARTESIAN_POINT('Ctrl Pts',(-0.0020665726407671,-2.17836041986871,
31.3155020069411)) ;
#58035 = CARTESIAN_POINT('Ctrl Pts',(-0.00200393495611065,-2.16180631294789,
31.3120809498982)) ;
#58036 = CARTESIAN_POINT('Ctrl Pts',(-0.00187287329576513,-2.12888951005409,
31.3052783926287)) ;
#58037 = CARTESIAN_POINT('Ctrl Pts',(-0.00180446694445819,-2.11252681791942,
31.3018968931955)) ;
#58038 = CARTESIAN_POINT('Ctrl Pts',(-0.00165981089476397,-2.08004069522962,
31.2951833399147)) ;
#58039 = CARTESIAN_POINT('Ctrl Pts',(-0.00158360917355472,-2.06391726446957,
31.291851286025)) ;
#58040 = CARTESIAN_POINT('Ctrl Pts',(-0.00146057179251287,-2.03994745220908,
31.2868977058982)) ;
#58041 = CARTESIAN_POINT('Ctrl Pts',(-0.00141807818111219,-2.03199340463373,
31.2852539294864)) ;
#58042 = CARTESIAN_POINT('Ctrl Pts',(-0.00132928283223824,-2.01616307091637,
31.281982446771)) ;
#58043 = CARTESIAN_POINT('Ctrl Pts',(-0.00128298191126172,-2.00828678476986,
31.280354740467)) ;
#58044 = CARTESIAN_POINT('Ctrl Pts',(-0.00118517612253733,-1.99261795861226,
31.2771166347607)) ;
#58045 = CARTESIAN_POINT('Ctrl Pts',(-0.00113369979187007,-1.98482541877565,
31.2755062353946)) ;
#58046 = CARTESIAN_POINT('Ctrl Pts',(-0.00105070864777337,-1.97320391184726,
31.2731045450879)) ;
#58047 = CARTESIAN_POINT('Ctrl Pts',(-0.00102207037490944,-1.96934129344584,
31.2723062997975)) ;
#58048 = CARTESIAN_POINT('Ctrl Pts',(-0.000962302516201868,-1.9616392413869,
31.2707146005552)) ;
#58049 = CARTESIAN_POINT('Ctrl Pts',(-0.000931174692610054,-1.9577998077162,
31.2699211466007)) ;
#58050 = CARTESIAN_POINT('Ctrl Pts',(-0.000865532982845733,-1.9501397428687,
31.2683381243983)) ;
#58051 = CARTESIAN_POINT('Ctrl Pts',(-0.000829293872646199,-1.94611557964085,
31.2675064943974)) ;
#58052 = CARTESIAN_POINT('Ctrl Pts',(-0.000748920269517818,-1.93787585622421,
31.2658036804696)) ;
#58053 = CARTESIAN_POINT('Ctrl Pts',(-0.000704858395548698,-1.93366029535625,
31.2649324964023)) ;
#58054 = CARTESIAN_POINT('Ctrl Pts',(-0.000630605424405322,-1.92733721691345,
31.2636257746236)) ;
#58055 = CARTESIAN_POINT('Ctrl Pts',(-0.000604477929136395,-1.92522958117288,
31.2631902124922)) ;
#58056 = CARTESIAN_POINT('Ctrl Pts',(-0.000548532542702596,-1.92103837449027,
31.2623240614392)) ;
#58057 = CARTESIAN_POINT('Ctrl Pts',(-0.000518750289895745,-1.91895480309204,
31.2618934724234)) ;
#58058 = CARTESIAN_POINT('Ctrl Pts',(-0.000469852903473204,-1.91586546722132,
31.2612550330144)) ;
#58059 = CARTESIAN_POINT('Ctrl Pts',(-0.000452838239228457,-1.91484169594687,
31.2610434613515)) ;
#58060 = CARTESIAN_POINT('Ctrl Pts',(-0.000416879002336717,-1.91280916054715,
31.2606234193898)) ;
#58061 = CARTESIAN_POINT('Ctrl Pts',(-0.000397937068286648,-1.9118003963771,
31.2604149490818)) ;
#58062 = CARTESIAN_POINT('Ctrl Pts',(-0.000357192200659911,-1.9098008749712,
31.2600017297628)) ;
#58063 = CARTESIAN_POINT('Ctrl Pts',(-0.000335428304312129,-1.90881011956137,
31.2597969811292)) ;
#58064 = CARTESIAN_POINT('Ctrl Pts',(-0.000299075801589961,-1.90733975547413,
31.259493116992)) ;
#58065 = CARTESIAN_POINT('Ctrl Pts',(-0.000286330749186815,-1.90685226278536,
31.2593923721857)) ;
#58066 = CARTESIAN_POINT('Ctrl Pts',(-0.000258978203130866,-1.90588291853958,
31.2591920483642)) ;
#58067 = CARTESIAN_POINT('Ctrl Pts',(-0.000244394768655416,-1.90540106633159,
31.2590924692146)) ;
#58068 = CARTESIAN_POINT('Ctrl Pts',(-0.000219952978457789,-1.90467591230858,
31.2589426095278)) ;
#58069 = CARTESIAN_POINT('Ctrl Pts',(-0.000210792012095635,-1.90441732984955,
31.2588891711064)) ;
#58070 = CARTESIAN_POINT('Ctrl Pts',(-0.000190504227060032,-1.9038880529221,
31.2587797912063)) ;
#58071 = CARTESIAN_POINT('Ctrl Pts',(-0.000179382359458563,-1.90361735827164,
31.2587238496901)) ;
#58072 = CARTESIAN_POINT('Ctrl Pts',(-0.000154443127708429,-1.90307628163011,
31.2586120312716)) ;
#58073 = CARTESIAN_POINT('Ctrl Pts',(-0.000140721200959569,-1.90280593840711,
31.2585561623812)) ;
#58074 = CARTESIAN_POINT('Ctrl Pts',(-1.07819935174354E-5,-1.90163368866297,
31.2583139062895)) ;
#58075 = CARTESIAN_POINT('Ctrl Pts',(-5.38608092278449E-6,-1.90158500930527,
31.2583038462567)) ;
#58076 = CARTESIAN_POINT('Ctrl Pts',(9.83167186641764E-9,-1.90153632994757,
31.2582937862238)) ;
#58077 = CARTESIAN_POINT('',(0.0148206788852317,-15.0366437072152,33.9727834182319)) ;
#58078 = CARTESIAN_POINT('Origin',(0.,-21.6462763158693,-1.36594255531499)) ;
#58079 = CARTESIAN_POINT('Ctrl Pts',(9.83167186641764E-9,-1.90153632994757,
31.2582937862238)) ;
#58080 = CARTESIAN_POINT('Ctrl Pts',(5.40498507600443E-6,-1.90158500938597,
31.2583038462733)) ;
#58081 = CARTESIAN_POINT('Ctrl Pts',(1.08001384804997E-5,-1.90163368882437,
31.2583139063229)) ;
#58082 = CARTESIAN_POINT('Ctrl Pts',(0.000140721346216588,-1.90280594305982,
31.2585561633427)) ;
#58083 = CARTESIAN_POINT('Ctrl Pts',(0.000154443545858063,-1.90307628603679,
31.2586120321823)) ;
#58084 = CARTESIAN_POINT('Ctrl Pts',(0.000179382728467112,-1.90361736221603,
31.2587238505053)) ;
#58085 = CARTESIAN_POINT('Ctrl Pts',(0.000190504320645866,-1.90388805664502,
31.2587797919757)) ;
#58086 = CARTESIAN_POINT('Ctrl Pts',(0.00021079206978046,-1.90441733312078,
31.2588891717824)) ;
#58087 = CARTESIAN_POINT('Ctrl Pts',(0.000219952985965777,-1.90467591536023,
31.2589426101585)) ;
#58088 = CARTESIAN_POINT('Ctrl Pts',(0.000244394767151704,-1.90540106911698,
31.2590924697902)) ;
#58089 = CARTESIAN_POINT('Ctrl Pts',(0.000258978255278715,-1.90588292126836,
31.2591920489281)) ;
#58090 = CARTESIAN_POINT('Ctrl Pts',(0.000286330784955126,-1.90685226540366,
31.2593923727268)) ;
#58091 = CARTESIAN_POINT('Ctrl Pts',(0.000299075816320136,-1.9073397580372,
31.2594931175217)) ;
#58092 = CARTESIAN_POINT('Ctrl Pts',(0.000335428305529032,-1.90881012195651,
31.2597969816242)) ;
#58093 = CARTESIAN_POINT('Ctrl Pts',(0.000357192224140643,-1.90980087725246,
31.2600017302343)) ;
#58094 = CARTESIAN_POINT('Ctrl Pts',(0.000397937081915845,-1.91180039842972,
31.260414949506)) ;
#58095 = CARTESIAN_POINT('Ctrl Pts',(0.000416879027904655,-1.91280916248412,
31.2606234197901)) ;
#58096 = CARTESIAN_POINT('Ctrl Pts',(0.000452838258712398,-1.9148416976513,
31.2610434617038)) ;
#58097 = CARTESIAN_POINT('Ctrl Pts',(0.000469852938162042,-1.9158654688083,
31.2612550333424)) ;
#58098 = CARTESIAN_POINT('Ctrl Pts',(0.000518750313335333,-1.91895480432564,
31.2618934726783)) ;
#58099 = CARTESIAN_POINT('Ctrl Pts',(0.000548532557564341,-1.92103837548551,
31.2623240616449)) ;
#58100 = CARTESIAN_POINT('Ctrl Pts',(0.000604477934722621,-1.92522958168858,
31.2631902125987)) ;
#58101 = CARTESIAN_POINT('Ctrl Pts',(0.000630605459915997,-1.92733721718753,
31.2636257746802)) ;
#58102 = CARTESIAN_POINT('Ctrl Pts',(0.00070485841900451,-1.93366029490678,
31.2649324963094)) ;
#58103 = CARTESIAN_POINT('Ctrl Pts',(0.000748920258238895,-1.93787585529259,
31.2658036802771)) ;
#58104 = CARTESIAN_POINT('Ctrl Pts',(0.000829293852258837,-1.94611557776626,
31.26750649401)) ;
#58105 = CARTESIAN_POINT('Ctrl Pts',(0.000865532986477288,-1.9501397405333,
31.2683381239156)) ;
#58106 = CARTESIAN_POINT('Ctrl Pts',(0.000931174692604608,-1.95779980495566,
31.2699211460302)) ;
#58107 = CARTESIAN_POINT('Ctrl Pts',(0.000962302480328251,-1.96163923864022,
31.2707145999876)) ;
#58108 = CARTESIAN_POINT('Ctrl Pts',(0.00102207033992775,-1.9693412907264,
31.2723062992355)) ;
#58109 = CARTESIAN_POINT('Ctrl Pts',(0.00105070862597898,-1.97320390914139,
31.2731045445287)) ;
#58110 = CARTESIAN_POINT('Ctrl Pts',(0.00113369977366347,-1.98482541611087,
31.2755062348439)) ;
#58111 = CARTESIAN_POINT('Ctrl Pts',(0.00118517610350443,-1.99261795597505,
31.2771166342157)) ;
#58112 = CARTESIAN_POINT('Ctrl Pts',(0.0012829818947538,-2.00828678218809,
31.2803547399334)) ;
#58113 = CARTESIAN_POINT('Ctrl Pts',(0.00132928283070744,-2.01616306836236,
31.2819824462432)) ;
#58114 = CARTESIAN_POINT('Ctrl Pts',(0.00141807818099176,-2.03199340213575,
31.2852539289702)) ;
#58115 = CARTESIAN_POINT('Ctrl Pts',(0.00146057177435883,-2.03994744973935,
31.2868977053878)) ;
#58116 = CARTESIAN_POINT('Ctrl Pts',(0.00158360915669288,-2.06391726208467,
31.2918512855321)) ;
#58117 = CARTESIAN_POINT('Ctrl Pts',(0.001659810895993,-2.08004069290168,
31.2951833394336)) ;
#58118 = CARTESIAN_POINT('Ctrl Pts',(0.00180446694663054,-2.11252681570644,
31.3018968927381)) ;
#58119 = CARTESIAN_POINT('Ctrl Pts',(0.00187287328849277,-2.12888950789906,
31.3052783921833)) ;
#58120 = CARTESIAN_POINT('Ctrl Pts',(0.00200393494937599,-2.16180631090932,
31.3120809494769)) ;
#58121 = CARTESIAN_POINT('Ctrl Pts',(0.00206657262782834,-2.17836041788876,
31.3155020065319)) ;
#58122 = CARTESIAN_POINT('Ctrl Pts',(0.00218730807792908,-2.21161219583605,
31.3223737894488)) ;
#58123 = CARTESIAN_POINT('Ctrl Pts',(0.00224540358654324,-2.22830986681189,
31.3258245153119)) ;
#58124 = CARTESIAN_POINT('Ctrl Pts',(0.00241408123334814,-2.27854645761049,
31.336206364577)) ;
#58125 = CARTESIAN_POINT('Ctrl Pts',(0.00251912676155658,-2.31222895501437,
31.3431671595943)) ;
#58126 = CARTESIAN_POINT('Ctrl Pts',(0.00271819527582991,-2.37959406825606,
31.3570887741044)) ;
#58127 = CARTESIAN_POINT('Ctrl Pts',(0.00281217424613174,-2.41327667043147,
31.3640495907737)) ;
#58128 = CARTESIAN_POINT('Ctrl Pts',(0.00299104804018365,-2.48025919041532,
31.3778921389007)) ;
#58129 = CARTESIAN_POINT('Ctrl Pts',(0.00307592509813755,-2.51355910826926,
31.3847738703678)) ;
#58130 = CARTESIAN_POINT('Ctrl Pts',(0.00331863396146083,-2.61231067548724,
31.4051817815983)) ;
#58131 = CARTESIAN_POINT('Ctrl Pts',(0.00346465861835736,-2.67661413815233,
31.4184706781177)) ;
#58132 = CARTESIAN_POINT('Ctrl Pts',(0.0037419934849328,-2.80486911270198,
31.4449757373206)) ;
#58133 = CARTESIAN_POINT('Ctrl Pts',(0.00387889601224861,-2.87209205434656,
31.4588679707746)) ;
#58134 = CARTESIAN_POINT('Ctrl Pts',(0.00414115714715684,-3.00694369580827,
31.4867362913064)) ;
#58135 = CARTESIAN_POINT('Ctrl Pts',(0.0042664769804943,-3.07457239569777,
31.5007123783991)) ;
#58136 = CARTESIAN_POINT('Ctrl Pts',(0.00450823986163544,-3.2102224617746,
31.5287457006532)) ;
#58137 = CARTESIAN_POINT('Ctrl Pts',(0.00462466717990583,-3.27824382794846,
31.5428029358115)) ;
#58138 = CARTESIAN_POINT('Ctrl Pts',(0.00485042867526996,-3.41466613604315,
31.570995848916)) ;
#58139 = CARTESIAN_POINT('Ctrl Pts',(0.00495976082741732,-3.48306707796744,
31.5851315268619)) ;
#58140 = CARTESIAN_POINT('Ctrl Pts',(0.00527901892971909,-3.68881963287913,
31.6276521672366)) ;
#58141 = CARTESIAN_POINT('Ctrl Pts',(0.00548031481950349,-3.82672097435253,
31.6561507360658)) ;
#58142 = CARTESIAN_POINT('Ctrl Pts',(0.00586640948546941,-4.10388488678362,
31.7134291842014)) ;
#58143 = CARTESIAN_POINT('Ctrl Pts',(0.0060511489907128,-4.2431474578205,
31.7422090635241)) ;
#58144 = CARTESIAN_POINT('Ctrl Pts',(0.00640800046407745,-4.52292911943078,
31.8000284933815)) ;
#58145 = CARTESIAN_POINT('Ctrl Pts',(0.00658008599084795,-4.66344820909719,
31.8290680437289)) ;
#58146 = CARTESIAN_POINT('Ctrl Pts',(0.00691419331657868,-4.94563819605463,
31.887385175965)) ;
#58147 = CARTESIAN_POINT('Ctrl Pts',(0.0070762018962943,-5.08730909336069,
31.9166627578568)) ;
#58148 = CARTESIAN_POINT('Ctrl Pts',(0.00739194776104187,-5.37169798643551,
31.9754343140794)) ;
#58149 = CARTESIAN_POINT('Ctrl Pts',(0.00754567856520655,-5.51441598220197,
32.0049282884094)) ;
#58150 = CARTESIAN_POINT('Ctrl Pts',(0.00784617116563057,-5.80079436351979,
32.0641109905068)) ;
#58151 = CARTESIAN_POINT('Ctrl Pts',(0.00799293179047366,-5.94445474907251,
32.0937997182736)) ;
#58152 = CARTESIAN_POINT('Ctrl Pts',(0.00842423445892503,-6.37669242790047,
32.183125573331)) ;
#58153 = CARTESIAN_POINT('Ctrl Pts',(0.00869987323869593,-6.66652623865878,
32.2430223714091)) ;
#58154 = CARTESIAN_POINT('Ctrl Pts',(0.00923278420170785,-7.24870690362006,
32.363335310893)) ;
#58155 = CARTESIAN_POINT('Ctrl Pts',(0.00949001810909513,-7.54105375785668,
32.4237514523057)) ;
#58156 = CARTESIAN_POINT('Ctrl Pts',(0.00998950899150371,-8.12742283859435,
32.5449299660763)) ;
#58157 = CARTESIAN_POINT('Ctrl Pts',(0.0102317469989513,-8.42144506509215,
32.6056923384334)) ;
#58158 = CARTESIAN_POINT('Ctrl Pts',(0.0107035427641363,-9.01032721998393,
32.727390201878)) ;
#58159 = CARTESIAN_POINT('Ctrl Pts',(0.0109330916392549,-9.30518714838485,
32.7883256929664)) ;
#58160 = CARTESIAN_POINT('Ctrl Pts',(0.011605124548404,-10.1897669817304,
32.9711321761835)) ;
#58161 = CARTESIAN_POINT('Ctrl Pts',(0.0120311513767769,-10.7794869194086,
33.093003175074)) ;
#58162 = CARTESIAN_POINT('Ctrl Pts',(0.0128472164422006,-11.9522255098215,
33.3353602912582)) ;
#58163 = CARTESIAN_POINT('Ctrl Pts',(0.0132371778185301,-12.5352441626078,
33.4558464085617)) ;
#58164 = CARTESIAN_POINT('Ctrl Pts',(0.0139852279330011,-13.6878788033261,
33.6940488603458)) ;
#58165 = CARTESIAN_POINT('Ctrl Pts',(0.0143432799612731,-14.2574947912552,
33.8117651948258)) ;
#58166 = CARTESIAN_POINT('Ctrl Pts',(0.0147314522641499,-14.8904290787823,
33.9425668329)) ;
#58167 = CARTESIAN_POINT('Ctrl Pts',(0.0147761934957339,-14.9636265798866,
33.9576937635085)) ;
#58168 = CARTESIAN_POINT('Ctrl Pts',(0.014820679681735,-15.0366437072144,
33.9727834182323)) ;
#58169 = CARTESIAN_POINT('',(14.2782523899403,-15.0366437072153,30.8266401270693)) ;
#58170 = CARTESIAN_POINT('',(14.2513506240286,-15.0366437072153,30.8390862093169)) ;
#58171 = CARTESIAN_POINT('Origin',(-0.573544392334149,-21.6462763158694,-1.23969588788643)) ;
#58172 = CARTESIAN_POINT('',(13.1250168957584,-1.901536243719,28.3692590808765)) ;
#58173 = CARTESIAN_POINT('Ctrl Pts',(13.1250169039853,-1.90153633586757,28.369259098053)) ;
#58174 = CARTESIAN_POINT('Ctrl Pts',(13.1250269478319,-1.90158489539068,28.3692655085023)) ;
#58175 = CARTESIAN_POINT('Ctrl Pts',(13.1251996720784,-1.90241997455468,28.3693757491368)) ;
#58176 = CARTESIAN_POINT('Ctrl Pts',(13.1252567763422,-1.90282053169335,28.3694405386005)) ;
#58177 = CARTESIAN_POINT('Ctrl Pts',(13.1252930337436,-1.90309401349771,28.3694860372096)) ;
#58178 = CARTESIAN_POINT('Ctrl Pts',(13.1253632958455,-1.90364136769095,28.3695781655761)) ;
#58179 = CARTESIAN_POINT('Ctrl Pts',(13.1253972100022,-1.9039152012528,28.3696248283824)) ;
#58180 = CARTESIAN_POINT('Ctrl Pts',(13.1254621893454,-1.90445061351417,28.3697166815804)) ;
#58181 = CARTESIAN_POINT('Ctrl Pts',(13.1254932500133,-1.90471219239629,28.3697618741041)) ;
#58182 = CARTESIAN_POINT('Ctrl Pts',(13.1255792249785,-1.9054458353377,28.3698891517338)) ;
#58183 = CARTESIAN_POINT('Ctrl Pts',(13.1256348435025,-1.90593335789139,28.3699744310004)) ;
#58184 = CARTESIAN_POINT('Ctrl Pts',(13.1257449190649,-1.90691410886923,28.3701468261471)) ;
#58185 = CARTESIAN_POINT('Ctrl Pts',(13.1257993541738,-1.90740733794508,28.3702339523212)) ;
#58186 = CARTESIAN_POINT('Ctrl Pts',(13.1259616328036,-1.90889500365118,28.3704976225806)) ;
#58187 = CARTESIAN_POINT('Ctrl Pts',(13.1260684852153,-1.90989741674749,28.3706764414799)) ;
#58188 = CARTESIAN_POINT('Ctrl Pts',(13.1262812303969,-1.91192046485291,28.3710386724698)) ;
#58189 = CARTESIAN_POINT('Ctrl Pts',(13.1263870873956,-1.91294109803394,28.3712221006936)) ;
#58190 = CARTESIAN_POINT('Ctrl Pts',(13.1265983616806,-1.91499754756168,28.3715926178508)) ;
#58191 = CARTESIAN_POINT('Ctrl Pts',(13.1267037766399,-1.91603336395173,28.3717797078706)) ;
#58192 = CARTESIAN_POINT('Ctrl Pts',(13.1270196437705,-1.91915904650413,28.3723453045198)) ;
#58193 = CARTESIAN_POINT('Ctrl Pts',(13.1272297591902,-1.92126713079265,28.3727281152986)) ;
#58194 = CARTESIAN_POINT('Ctrl Pts',(13.1276487985653,-1.92550764503829,28.3734998317072)) ;
#58195 = CARTESIAN_POINT('Ctrl Pts',(13.1278576900239,-1.92764007545159,28.3738887524756)) ;
#58196 = CARTESIAN_POINT('Ctrl Pts',(13.1284806092693,-1.93403753795706,28.3750572910872)) ;
#58197 = CARTESIAN_POINT('Ctrl Pts',(13.1288909375366,-1.93830268824026,28.3758386474229)) ;
#58198 = CARTESIAN_POINT('Ctrl Pts',(13.1296877148954,-1.94663933648012,28.3773683122489)) ;
#58199 = CARTESIAN_POINT('Ctrl Pts',(13.1300740977459,-1.95071083511603,28.3781166515402)) ;
#58200 = CARTESIAN_POINT('Ctrl Pts',(13.1308065738439,-1.95846141420779,28.379542614647)) ;
#58201 = CARTESIAN_POINT('Ctrl Pts',(13.1311721109147,-1.96234642274043,28.3802581335656)) ;
#58202 = CARTESIAN_POINT('Ctrl Pts',(13.1319029492433,-1.97013989960687,28.3816946224065)) ;
#58203 = CARTESIAN_POINT('Ctrl Pts',(13.1322682488701,-1.974048367954,28.3824155930864)) ;
#58204 = CARTESIAN_POINT('Ctrl Pts',(13.1333644330489,-1.98580782403353,28.3845861267117)) ;
#58205 = CARTESIAN_POINT('Ctrl Pts',(13.1340956458595,-1.99369286238981,28.3860432912726)) ;
#58206 = CARTESIAN_POINT('Ctrl Pts',(13.1355607255424,-2.00954767943326,28.3889756882594)) ;
#58207 = CARTESIAN_POINT('Ctrl Pts',(13.1362945663458,-2.01751745794586,28.3904509327061)) ;
#58208 = CARTESIAN_POINT('Ctrl Pts',(13.1377656003264,-2.03353569925263,28.3934177874007)) ;
#58209 = CARTESIAN_POINT('Ctrl Pts',(13.138502792754,-2.04158416205131,28.394909397996)) ;
#58210 = CARTESIAN_POINT('Ctrl Pts',(13.1407197670541,-2.06583849778387,28.399406540668)) ;
#58211 = CARTESIAN_POINT('Ctrl Pts',(13.1422050381934,-2.08215331459392,28.4024343401622)) ;
#58212 = CARTESIAN_POINT('Ctrl Pts',(13.1451895153445,-2.11502504894364,28.4085386196463)) ;
#58213 = CARTESIAN_POINT('Ctrl Pts',(13.1466886775721,-2.13158196668823,28.4116151199393)) ;
#58214 = CARTESIAN_POINT('Ctrl Pts',(13.1496985589263,-2.16488949245127,28.4178068779039)) ;
#58215 = CARTESIAN_POINT('Ctrl Pts',(13.151209261612,-2.1816400966306,28.4209221423076)) ;
#58216 = CARTESIAN_POINT('Ctrl Pts',(13.1542391277507,-2.21528657271386,28.427181834879)) ;
#58217 = CARTESIAN_POINT('Ctrl Pts',(13.1557582891559,-2.23218244462569,28.4303262639956)) ;
#58218 = CARTESIAN_POINT('Ctrl Pts',(13.1603232595078,-2.28301534196996,28.439789169183)) ;
#58219 = CARTESIAN_POINT('Ctrl Pts',(13.1633766205547,-2.31709764872116,28.4461372325071)) ;
#58220 = CARTESIAN_POINT('Ctrl Pts',(13.1694732902846,-2.38526238067128,28.4588380368451)) ;
#58221 = CARTESIAN_POINT('Ctrl Pts',(13.1725165575778,-2.41934479220568,28.4651907938965)) ;
#58222 = CARTESIAN_POINT('Ctrl Pts',(13.1785611978818,-2.48712238762728,28.4778275168357)) ;
#58223 = CARTESIAN_POINT('Ctrl Pts',(13.1815625546765,-2.52081757156001,28.4841114902361)) ;
#58224 = CARTESIAN_POINT('Ctrl Pts',(13.1904549255812,-2.6207413071602,28.5027505372084)) ;
#58225 = CARTESIAN_POINT('Ctrl Pts',(13.1962343453641,-2.68580804227443,28.5148926888216)) ;
#58226 = CARTESIAN_POINT('Ctrl Pts',(13.20775574064,-2.81566304839315,28.5391309080581)) ;
#58227 = CARTESIAN_POINT('Ctrl Pts',(13.2137900707651,-2.88376182393009,28.5518455351887)) ;
#58228 = CARTESIAN_POINT('Ctrl Pts',(13.2258838404761,-3.02037041957963,28.5773567693237)) ;
#58229 = CARTESIAN_POINT('Ctrl Pts',(13.2319432444941,-3.08888023976489,28.5901533928)) ;
#58230 = CARTESIAN_POINT('Ctrl Pts',(13.2440884526074,-3.22629766229947,28.6158250026112)) ;
#58231 = CARTESIAN_POINT('Ctrl Pts',(13.2501742422778,-3.29520526463518,28.6286999956163)) ;
#58232 = CARTESIAN_POINT('Ctrl Pts',(13.2623727032053,-3.43340499038686,28.6545251021062)) ;
#58233 = CARTESIAN_POINT('Ctrl Pts',(13.268485372607,-3.50269711380624,28.6674752164491)) ;
#58234 = CARTESIAN_POINT('Ctrl Pts',(13.2868637167533,-3.71113037540774,28.7064337048146)) ;
#58235 = CARTESIAN_POINT('Ctrl Pts',(13.2991698265153,-3.85082840427815,28.7325501781858)) ;
#58236 = CARTESIAN_POINT('Ctrl Pts',(13.3238866282531,-4.13160342647603,28.7850487366164)) ;
#58237 = CARTESIAN_POINT('Ctrl Pts',(13.336297265978,-4.27268041988289,28.8114308467927)) ;
#58238 = CARTESIAN_POINT('Ctrl Pts',(13.3612174575322,-4.55610729697891,28.8644391466752)) ;
#58239 = CARTESIAN_POINT('Ctrl Pts',(13.373726987082,-4.69845717975854,28.8910653474071)) ;
#58240 = CARTESIAN_POINT('Ctrl Pts',(13.3988381015789,-4.98432375945421,28.9445408484739)) ;
#58241 = CARTESIAN_POINT('Ctrl Pts',(13.4114396744345,-5.12784045638525,28.9713901544063)) ;
#58242 = CARTESIAN_POINT('Ctrl Pts',(13.436727309626,-5.41593459099438,29.0252912128394)) ;
#58243 = CARTESIAN_POINT('Ctrl Pts',(13.4494133660345,-5.56051202867017,29.0523429680818)) ;
#58244 = CARTESIAN_POINT('Ctrl Pts',(13.4748619542698,-5.85062157186436,29.1066284795457)) ;
#58245 = CARTESIAN_POINT('Ctrl Pts',(13.4876244850246,-5.99615367738409,29.1338622362626)) ;
#58246 = CARTESIAN_POINT('Ctrl Pts',(13.5260143312979,-6.43402288686051,29.2158060422649)) ;
#58247 = CARTESIAN_POINT('Ctrl Pts',(13.5517439698395,-6.7276328790384,29.2707585944021)) ;
#58248 = CARTESIAN_POINT('Ctrl Pts',(13.6034073853403,-7.31739864832443,29.3811489411672)) ;
#58249 = CARTESIAN_POINT('Ctrl Pts',(13.6293411273095,-7.6135544254662,29.436586751991)) ;
#58250 = CARTESIAN_POINT('Ctrl Pts',(13.6813422113443,-8.20756317967979,29.5477870239103)) ;
#58251 = CARTESIAN_POINT('Ctrl Pts',(13.7074095360699,-8.50541615674834,29.6035494930274)) ;
#58252 = CARTESIAN_POINT('Ctrl Pts',(13.759606248396,-9.10197072662847,29.7152389516399)) ;
#58253 = CARTESIAN_POINT('Ctrl Pts',(13.7857356278777,-9.40067231944697,29.7711659448926)) ;
#58254 = CARTESIAN_POINT('Ctrl Pts',(13.8641086058114,-10.2967771460885,29.9389539496253)) ;
#58255 = CARTESIAN_POINT('Ctrl Pts',(13.916337185494,-10.8941804126697,30.0508219169838)) ;
#58256 = CARTESIAN_POINT('Ctrl Pts',(14.0201724215159,-12.0821983504006,30.2732997895653)) ;
#58257 = CARTESIAN_POINT('Ctrl Pts',(14.071779007624,-12.6728130216019,30.3839097272913)) ;
#58258 = CARTESIAN_POINT('Ctrl Pts',(14.1753539738539,-13.8584258096385,30.6059603498131)) ;
#58259 = CARTESIAN_POINT('Ctrl Pts',(14.2272846073097,-14.4529998121294,30.7173219252823)) ;
#58260 = CARTESIAN_POINT('Ctrl Pts',(14.2782523900528,-15.0366437072152,30.8266401270172)) ;
#58261 = CARTESIAN_POINT('Ctrl Pts',(14.2513506239141,-15.0366437072152,30.8390862093698)) ;
#58262 = CARTESIAN_POINT('Ctrl Pts',(14.2498487196638,-15.0192244618052,30.8358146216817)) ;
#58263 = CARTESIAN_POINT('Ctrl Pts',(14.2483459834305,-15.0017954802462,30.8325412019439)) ;
#58264 = CARTESIAN_POINT('Ctrl Pts',(14.1979681755858,-14.4175024637988,30.7228022408249)) ;
#58265 = CARTESIAN_POINT('Ctrl Pts',(14.1482238960184,-13.8404650786097,30.6144223190429)) ;
#58266 = CARTESIAN_POINT('Ctrl Pts',(14.0475863486083,-12.6728130223236,30.3951024433868)) ;
#58267 = CARTESIAN_POINT('Ctrl Pts',(13.9966930472133,-12.0821983512294,30.2841625050364)) ;
#58268 = CARTESIAN_POINT('Ctrl Pts',(13.8943503623223,-10.894180413714,30.0609941048191)) ;
#58269 = CARTESIAN_POINT('Ctrl Pts',(13.842900908589,-10.2967771472412,29.9487656754368)) ;
#58270 = CARTESIAN_POINT('Ctrl Pts',(13.7657568491019,-9.40067232076225,29.7804091125241)) ;
#58271 = CARTESIAN_POINT('Ctrl Pts',(13.7400472188986,-9.10197072799794,29.7242879225883)) ;
#58272 = CARTESIAN_POINT('Ctrl Pts',(13.6887131872663,-8.50541615822605,29.6121993454108)) ;
#58273 = CARTESIAN_POINT('Ctrl Pts',(13.6630887777184,-8.20756318121152,29.5562319619242)) ;
#58274 = CARTESIAN_POINT('Ctrl Pts',(13.6120009385489,-7.61355442710567,29.4446091779631)) ;
#58275 = CARTESIAN_POINT('Ctrl Pts',(13.5865374915885,-7.31739865001763,29.388953785511)) ;
#58276 = CARTESIAN_POINT('Ctrl Pts',(13.5358483446611,-6.72763288083859,29.27811269413)) ;
#58277 = CARTESIAN_POINT('Ctrl Pts',(13.5106226096945,-6.43402288871397,29.222927011386)) ;
#58278 = CARTESIAN_POINT('Ctrl Pts',(13.4730212100658,-5.99615367931698,29.1406184311406)) ;
#58279 = CARTESIAN_POINT('Ctrl Pts',(13.4605269614545,-5.85062157382364,29.1132605538929)) ;
#58280 = CARTESIAN_POINT('Ctrl Pts',(13.4356276714686,-5.5605120306821,29.0587209100092)) ;
#58281 = CARTESIAN_POINT('Ctrl Pts',(13.4232226290259,-5.41593459303255,29.0315391438679)) ;
#58282 = CARTESIAN_POINT('Ctrl Pts',(13.3985121557589,-5.12784045847568,28.977371061906)) ;
#58283 = CARTESIAN_POINT('Ctrl Pts',(13.3862067190029,-4.98432376157065,28.9503847488305)) ;
#58284 = CARTESIAN_POINT('Ctrl Pts',(13.3617063123363,-4.69845718192687,28.8966267042463)) ;
#58285 = CARTESIAN_POINT('Ctrl Pts',(13.3495113303281,-4.55610729917304,28.869854978331)) ;
#58286 = CARTESIAN_POINT('Ctrl Pts',(13.3252434057812,-4.27268042212843,28.8165449076082)) ;
#58287 = CARTESIAN_POINT('Ctrl Pts',(13.3131704391221,-4.13160342874717,28.790006574167)) ;
#58288 = CARTESIAN_POINT('Ctrl Pts',(13.2891593483905,-3.85082840660023,28.7371815190693)) ;
#58289 = CARTESIAN_POINT('Ctrl Pts',(13.2772211700524,-3.71113037775515,28.7108948225007)) ;
#58290 = CARTESIAN_POINT('Ctrl Pts',(13.2594263764353,-3.50269711619146,28.6716663549198)) ;
#58291 = CARTESIAN_POINT('Ctrl Pts',(13.2535135490082,-3.43340499278465,28.658623783837)) ;
#58292 = CARTESIAN_POINT('Ctrl Pts',(13.2417277490737,-3.29520526705806,28.6326077600474)) ;
#58293 = CARTESIAN_POINT('Ctrl Pts',(13.2358547747125,-3.22629766473483,28.6196343081985)) ;
#58294 = CARTESIAN_POINT('Ctrl Pts',(13.2241514889807,-3.08888024222519,28.5937582433277)) ;
#58295 = CARTESIAN_POINT('Ctrl Pts',(13.2183211631902,-3.02037042205235,28.5808556369805)) ;
#58296 = CARTESIAN_POINT('Ctrl Pts',(13.2067068091968,-2.88376182642761,28.5551226015214)) ;
#58297 = CARTESIAN_POINT('Ctrl Pts',(13.2009227454198,-2.81566305090302,28.5422921888514)) ;
#58298 = CARTESIAN_POINT('Ctrl Pts',(13.1899080877081,-2.68580804467985,28.5178195278291)) ;
#58299 = CARTESIAN_POINT('Ctrl Pts',(13.1843953175679,-2.62074130944303,28.5055540109265)) ;
#58300 = CARTESIAN_POINT('Ctrl Pts',(13.1759461421688,-2.52081757365458,28.4867099198361)) ;
#58301 = CARTESIAN_POINT('Ctrl Pts',(13.1730997733076,-2.48712238965837,28.4803542413676)) ;
#58302 = CARTESIAN_POINT('Ctrl Pts',(13.1673817598006,-2.41934479410906,28.4675664047515)) ;
#58303 = CARTESIAN_POINT('Ctrl Pts',(13.1645100989313,-2.38526238251044,28.4611342540995)) ;
#58304 = CARTESIAN_POINT('Ctrl Pts',(13.1587769281494,-2.3170976504319,28.4482652772108)) ;
#58305 = CARTESIAN_POINT('Ctrl Pts',(13.1559153792237,-2.2830153436165,28.4418284721351)) ;
#58306 = CARTESIAN_POINT('Ctrl Pts',(13.1516584111466,-2.23218244617646,28.4322230698995)) ;
#58307 = CARTESIAN_POINT('Ctrl Pts',(13.1502453308303,-2.21528657423275,28.4290295624378)) ;
#58308 = CARTESIAN_POINT('Ctrl Pts',(13.1474359244531,-2.18164009808608,28.4226678743052)) ;
#58309 = CARTESIAN_POINT('Ctrl Pts',(13.1460395963361,-2.16488949387522,28.4194996945841)) ;
#58310 = CARTESIAN_POINT('Ctrl Pts',(13.1432690292635,-2.13158196804943,28.4131972180285)) ;
#58311 = CARTESIAN_POINT('Ctrl Pts',(13.1418947745461,-2.11502505027367,28.4100629293605)) ;
#58312 = CARTESIAN_POINT('Ctrl Pts',(13.1391744339186,-2.08215331586202,28.4038364472936)) ;
#58313 = CARTESIAN_POINT('Ctrl Pts',(13.1378283041887,-2.06583849902119,28.4007442741215)) ;
#58314 = CARTESIAN_POINT('Ctrl Pts',(13.1358359914392,-2.04158416324294,28.3961431919376)) ;
#58315 = CARTESIAN_POINT('Ctrl Pts',(13.135176390713,-2.0335357004291,28.3946156835952)) ;
#58316 = CARTESIAN_POINT('Ctrl Pts',(13.1338674938624,-2.01751745909216,28.3915738162696)) ;
#58317 = CARTESIAN_POINT('Ctrl Pts',(13.1332181969884,-2.00954768056451,28.3900594576326)) ;
#58318 = CARTESIAN_POINT('Ctrl Pts',(13.1319317077644,-1.99369286349119,28.3870444358944)) ;
#58319 = CARTESIAN_POINT('Ctrl Pts',(13.1312944893827,-1.98580782512015,28.3855437848765)) ;
#58320 = CARTESIAN_POINT('Ctrl Pts',(13.1303498456158,-1.97404836901842,28.3833031411859)) ;
#58321 = CARTESIAN_POINT('Ctrl Pts',(13.1300368390763,-1.97013990066385,28.3825579771459)) ;
#58322 = CARTESIAN_POINT('Ctrl Pts',(13.1294151364984,-1.96234642378273,28.3810709967266)) ;
#58323 = CARTESIAN_POINT('Ctrl Pts',(13.1291064388203,-1.95846141524282,28.3803291811031)) ;
#58324 = CARTESIAN_POINT('Ctrl Pts',(13.128493818823,-1.95071083608938,28.3788477666453)) ;
#58325 = CARTESIAN_POINT('Ctrl Pts',(13.1281736019689,-1.9466393373964,28.3780688156913)) ;
#58326 = CARTESIAN_POINT('Ctrl Pts',(13.1275235722031,-1.93830268903959,28.3764712581725)) ;
#58327 = CARTESIAN_POINT('Ctrl Pts',(13.1271936929168,-1.93403753869634,28.3756526821611)) ;
#58328 = CARTESIAN_POINT('Ctrl Pts',(13.1267063464949,-1.92764007610111,28.3744214208619)) ;
#58329 = CARTESIAN_POINT('Ctrl Pts',(13.1265451593027,-1.92550764565787,28.3740104297428)) ;
#58330 = CARTESIAN_POINT('Ctrl Pts',(13.1262282666799,-1.92126713135282,28.3731914552007)) ;
#58331 = CARTESIAN_POINT('Ctrl Pts',(13.1260725287054,-1.91915904703525,28.3727834867303)) ;
#58332 = CARTESIAN_POINT('Ctrl Pts',(13.1258459404436,-1.91603336443895,28.3721765852679)) ;
#58333 = CARTESIAN_POINT('Ctrl Pts',(13.1257715916756,-1.91499754803343,28.371975122494)) ;
#58334 = CARTESIAN_POINT('Ctrl Pts',(13.1256259736314,-1.91294109847689,28.3715742295187)) ;
#58335 = CARTESIAN_POINT('Ctrl Pts',(13.1255547020259,-1.91192046528262,28.3713748003851)) ;
#58336 = CARTESIAN_POINT('Ctrl Pts',(13.1254163516264,-1.90989741714894,28.3709781506974)) ;
#58337 = CARTESIAN_POINT('Ctrl Pts',(13.1253492373508,-1.90889500403652,28.370780946975)) ;
#58338 = CARTESIAN_POINT('Ctrl Pts',(13.1252533348394,-1.90740733830955,28.3704865678484)) ;
#58339 = CARTESIAN_POINT('Ctrl Pts',(13.1252221711284,-1.90691410922708,28.3703886751776)) ;
#58340 = CARTESIAN_POINT('Ctrl Pts',(13.1251620394976,-1.90593335823539,28.3701931735045)) ;
#58341 = CARTESIAN_POINT('Ctrl Pts',(13.1251330495881,-1.90544583567611,28.3700955745277)) ;
#58342 = CARTESIAN_POINT('Ctrl Pts',(13.1250917024319,-1.90471219292145,28.3699476499174)) ;
#58343 = CARTESIAN_POINT('Ctrl Pts',(13.1250773667852,-1.90445061424685,28.3698947196222)) ;
#58344 = CARTESIAN_POINT('Ctrl Pts',(13.1250494265139,-1.90391520239999,28.3697857304192)) ;
#58345 = CARTESIAN_POINT('Ctrl Pts',(13.1250358172642,-1.90364136904213,28.369729673609)) ;
#58346 = CARTESIAN_POINT('Ctrl Pts',(13.1250110872508,-1.90309401527264,28.3696164799516)) ;
#58347 = CARTESIAN_POINT('Ctrl Pts',(13.1249998825665,-1.90282053368396,28.3695593907705)) ;
#58348 = CARTESIAN_POINT('Ctrl Pts',(13.1250156134575,-1.90163370102003,28.3692818656094)) ;
#58349 = CARTESIAN_POINT('Ctrl Pts',(13.1250162587214,-1.9015850184438,28.3692704818312)) ;
#58350 = CARTESIAN_POINT('Ctrl Pts',(13.1250169039853,-1.90153633586757,28.369259098053)) ;
#58351 = CARTESIAN_POINT('',(25.9023611320436,-15.0366437072153,21.982218282509)) ;
#58352 = CARTESIAN_POINT('',(25.8831717248497,-15.0366437072153,22.0048097991466)) ;
#58353 = CARTESIAN_POINT('Origin',(-1.04106958514518,-21.6462763158693,-0.884292476110772)) ;
#58354 = CARTESIAN_POINT('',(23.8238854240696,-1.9015362404957,20.2361906635364)) ;
#58355 = CARTESIAN_POINT('Ctrl Pts',(23.8238854382361,-1.90153632942096,20.2361906752451)) ;
#58356 = CARTESIAN_POINT('Ctrl Pts',(23.8238972397902,-1.90158489009019,20.236192282953)) ;
#58357 = CARTESIAN_POINT('Ctrl Pts',(23.8241008025455,-1.90242250380941,20.2362200140004)) ;
#58358 = CARTESIAN_POINT('Ctrl Pts',(23.8241800405353,-1.90282422716847,20.2362549662449)) ;
#58359 = CARTESIAN_POINT('Ctrl Pts',(23.8242321897855,-1.90309850455843,20.2362811264257)) ;
#58360 = CARTESIAN_POINT('Ctrl Pts',(23.8243349160092,-1.90364745004718,20.2363354225369)) ;
#58361 = CARTESIAN_POINT('Ctrl Pts',(23.8243854246561,-1.90392207929595,20.2363636265058)) ;
#58362 = CARTESIAN_POINT('Ctrl Pts',(23.8244832306668,-1.90445904680028,20.2364198915188)) ;
#58363 = CARTESIAN_POINT('Ctrl Pts',(23.8245305247551,-1.90472138524212,20.2364479564785)) ;
#58364 = CARTESIAN_POINT('Ctrl Pts',(23.824662358658,-1.90545718058384,20.2365276307242)) ;
#58365 = CARTESIAN_POINT('Ctrl Pts',(23.8247488851777,-1.90594614106352,20.2365818501438)) ;
#58366 = CARTESIAN_POINT('Ctrl Pts',(23.8249216560831,-1.90692978464094,20.2366924479152)) ;
#58367 = CARTESIAN_POINT('Ctrl Pts',(23.8250078848634,-1.90742446839044,20.2367488448471)) ;
#58368 = CARTESIAN_POINT('Ctrl Pts',(23.8252666035088,-1.90891652156313,20.2369205519908)) ;
#58369 = CARTESIAN_POINT('Ctrl Pts',(23.8254391508834,-1.9099218908987,20.237038348235)) ;
#58370 = CARTESIAN_POINT('Ctrl Pts',(23.8257853090816,-1.91195090507058,20.2372785226529)) ;
#58371 = CARTESIAN_POINT('Ctrl Pts',(23.8259588941782,-1.91297454807863,20.2374009305311)) ;
#58372 = CARTESIAN_POINT('Ctrl Pts',(23.8263072074963,-1.9150370619197,20.2376492615341)) ;
#58373 = CARTESIAN_POINT('Ctrl Pts',(23.8264819340572,-1.91607593279612,20.2377751866276)) ;
#58374 = CARTESIAN_POINT('Ctrl Pts',(23.8270075940328,-1.91921083239654,20.2381570567528)) ;
#58375 = CARTESIAN_POINT('Ctrl Pts',(23.8273600354879,-1.92132513283609,20.2384170590922)) ;
#58376 = CARTESIAN_POINT('Ctrl Pts',(23.8280664039129,-1.92557815084124,20.23894310934)) ;
#58377 = CARTESIAN_POINT('Ctrl Pts',(23.8284203077438,-1.9277168688624,20.2392091846352)) ;
#58378 = CARTESIAN_POINT('Ctrl Pts',(23.8294793530247,-1.93413319420295,20.2400106041034)) ;
#58379 = CARTESIAN_POINT('Ctrl Pts',(23.8301818629063,-1.93841091972006,20.2405490841293)) ;
#58380 = CARTESIAN_POINT('Ctrl Pts',(23.8315512366694,-1.94677214683963,20.2416060095999)) ;
#58381 = CARTESIAN_POINT('Ctrl Pts',(23.8322180532724,-1.95085564912166,20.2421245109221)) ;
#58382 = CARTESIAN_POINT('Ctrl Pts',(23.8334852560765,-1.95862918241561,20.2431141173015)) ;
#58383 = CARTESIAN_POINT('Ctrl Pts',(23.8341192980611,-1.96252574910842,20.243611530175)) ;
#58384 = CARTESIAN_POINT('Ctrl Pts',(23.8353894653667,-1.97034241205852,20.2446114143533)) ;
#58385 = CARTESIAN_POINT('Ctrl Pts',(23.8360255895339,-1.97426250832905,20.2451138870204)) ;
#58386 = CARTESIAN_POINT('Ctrl Pts',(23.837937434196,-1.98605694944873,20.2466281194029)) ;
#58387 = CARTESIAN_POINT('Ctrl Pts',(23.8392166575569,-1.99396544619106,20.2476466572173)) ;
#58388 = CARTESIAN_POINT('Ctrl Pts',(23.8417851342223,-2.00986743205398,20.2496990560114)) ;
#58389 = CARTESIAN_POINT('Ctrl Pts',(23.843074368885,-2.01786092099999,20.2507329388821)) ;
#58390 = CARTESIAN_POINT('Ctrl Pts',(23.8456627856708,-2.03392681721801,20.2528141859325)) ;
#58391 = CARTESIAN_POINT('Ctrl Pts',(23.8469619672685,-2.04199922449445,20.2538615507317)) ;
#58392 = CARTESIAN_POINT('Ctrl Pts',(23.8508738250851,-2.06632571772129,20.2570216762299)) ;
#58393 = CARTESIAN_POINT('Ctrl Pts',(23.8535008798689,-2.0826890716089,20.2591523897619)) ;
#58394 = CARTESIAN_POINT('Ctrl Pts',(23.858788182709,-2.11565860024936,20.2634522521349)) ;
#58395 = CARTESIAN_POINT('Ctrl Pts',(23.8614483995056,-2.13226477520709,20.2656214378429)) ;
#58396 = CARTESIAN_POINT('Ctrl Pts',(23.8667956808139,-2.1656713915056,20.2699902155389)) ;
#58397 = CARTESIAN_POINT('Ctrl Pts',(23.869482733217,-2.18247182900697,20.2721898205565)) ;
#58398 = CARTESIAN_POINT('Ctrl Pts',(23.8748768260301,-2.21621840381591,20.2766120092876)) ;
#58399 = CARTESIAN_POINT('Ctrl Pts',(23.8775838649755,-2.23316454113134,20.2788345947272)) ;
#58400 = CARTESIAN_POINT('Ctrl Pts',(23.8857242748928,-2.28414866676852,20.2855261523041)) ;
#58401 = CARTESIAN_POINT('Ctrl Pts',(23.8911769860505,-2.31833236849097,20.2900188701501)) ;
#58402 = CARTESIAN_POINT('Ctrl Pts',(23.902075238584,-2.38669989038716,20.2990127845743)) ;
#58403 = CARTESIAN_POINT('Ctrl Pts',(23.9075207490885,-2.42088369689579,20.3035140131346)) ;
#58404 = CARTESIAN_POINT('Ctrl Pts',(23.9183446729951,-2.48886293005225,20.3124714841742)) ;
#58405 = CARTESIAN_POINT('Ctrl Pts',(23.9237230748093,-2.52265835674563,20.3169277403104)) ;
#58406 = CARTESIAN_POINT('Ctrl Pts',(23.9396669654899,-2.62287936398345,20.3301497626395)) ;
#58407 = CARTESIAN_POINT('Ctrl Pts',(23.9500412146539,-2.6881396713304,20.3387686942727)) ;
#58408 = CARTESIAN_POINT('Ctrl Pts',(23.9707393778284,-2.81840077289416,20.3559829746962)) ;
#58409 = CARTESIAN_POINT('Ctrl Pts',(23.9815899155693,-2.88672198231194,20.3650182794143)) ;
#58410 = CARTESIAN_POINT('Ctrl Pts',(24.0033483989575,-3.02377678830098,20.3831529455601)) ;
#58411 = CARTESIAN_POINT('Ctrl Pts',(24.014256319173,-3.09251038494502,20.3922523369516)) ;
#58412 = CARTESIAN_POINT('Ctrl Pts',(24.03612921706,-3.23037665966399,20.410511341564)) ;
#58413 = CARTESIAN_POINT('Ctrl Pts',(24.0470941844152,-3.29950933772532,20.4196709669254)) ;
#58414 = CARTESIAN_POINT('Ctrl Pts',(24.0690802477411,-3.43816047088516,20.4380472859567)) ;
#58415 = CARTESIAN_POINT('Ctrl Pts',(24.0801013423862,-3.50767892598712,20.4472639811866)) ;
#58416 = CARTESIAN_POINT('Ctrl Pts',(24.1132469194986,-3.71679300160785,20.474995535766)) ;
#58417 = CARTESIAN_POINT('Ctrl Pts',(24.1354537658879,-3.85694733178598,20.4935917805061)) ;
#58418 = CARTESIAN_POINT('Ctrl Pts',(24.1800745931133,-4.13863946071678,20.5309820442909)) ;
#58419 = CARTESIAN_POINT('Ctrl Pts',(24.2024885351756,-4.28017725954893,20.5497761090088)) ;
#58420 = CARTESIAN_POINT('Ctrl Pts',(24.2475093203922,-4.56452990514295,20.5875447978751)) ;
#58421 = CARTESIAN_POINT('Ctrl Pts',(24.2701161461079,-4.70734475099467,20.6065194422633)) ;
#58422 = CARTESIAN_POINT('Ctrl Pts',(24.3155076113059,-4.99414506800992,20.6446330803387)) ;
#58423 = CARTESIAN_POINT('Ctrl Pts',(24.3382922421449,-5.13813053918853,20.6637720842065)) ;
#58424 = CARTESIAN_POINT('Ctrl Pts',(24.384023726511,-5.42716568699795,20.702198825054)) ;
#58425 = CARTESIAN_POINT('Ctrl Pts',(24.4069705758003,-5.57221536362646,20.7214865670219)) ;
#58426 = CARTESIAN_POINT('Ctrl Pts',(24.453010585758,-5.86327250296127,20.7601955450431)) ;
#58427 = CARTESIAN_POINT('Ctrl Pts',(24.4761037456608,-6.0092799656689,20.7796167819971)) ;
#58428 = CARTESIAN_POINT('Ctrl Pts',(24.5455785124947,-6.44857940435679,20.8380582440759)) ;
#58429 = CARTESIAN_POINT('Ctrl Pts',(24.5921554554228,-6.74314842620376,20.8772561613807)) ;
#58430 = CARTESIAN_POINT('Ctrl Pts',(24.6856996519804,-7.33484057012121,20.9560078084074)) ;
#58431 = CARTESIAN_POINT('Ctrl Pts',(24.7326668806052,-7.63196369222536,20.9955615675779)) ;
#58432 = CARTESIAN_POINT('Ctrl Pts',(24.82685976589,-8.22791267989474,21.0749083918998)) ;
#58433 = CARTESIAN_POINT('Ctrl Pts',(24.8740854101562,-8.52673854545668,21.1147014716412)) ;
#58434 = CARTESIAN_POINT('Ctrl Pts',(24.9686625303249,-9.12524166409269,21.1944112711994)) ;
#58435 = CARTESIAN_POINT('Ctrl Pts',(25.0160140004293,-9.42491891717367,21.2343279978436)) ;
#58436 = CARTESIAN_POINT('Ctrl Pts',(25.1580575855592,-10.3239507246136,21.3540909375572)) ;
#58437 = CARTESIAN_POINT('Ctrl Pts',(25.2527389752251,-10.9233053117369,21.4339497879505)) ;
#58438 = CARTESIAN_POINT('Ctrl Pts',(25.4410055391706,-12.1152037164723,21.5927839145526)) ;
#58439 = CARTESIAN_POINT('Ctrl Pts',(25.5345906632723,-12.7077475341359,21.6717592498504)) ;
#58440 = CARTESIAN_POINT('Ctrl Pts',(25.7201261119685,-13.8825790586843,21.8283605922029)) ;
#58441 = CARTESIAN_POINT('Ctrl Pts',(25.8120639293555,-14.4647882730915,21.9059762674555)) ;
#58442 = CARTESIAN_POINT('Ctrl Pts',(25.9023611320477,-15.0366437072153,21.9822182825043)) ;
#58443 = CARTESIAN_POINT('Ctrl Pts',(25.8831717248466,-15.0366437072153,22.0048097991503)) ;
#58444 = CARTESIAN_POINT('Ctrl Pts',(25.8826584335355,-15.0333766938331,22.0043711940518)) ;
#58445 = CARTESIAN_POINT('Ctrl Pts',(25.8821450893183,-15.0301093425198,22.0039325433645)) ;
#58446 = CARTESIAN_POINT('Ctrl Pts',(25.7922804814445,-14.458135719157,21.9271435098704)) ;
#58447 = CARTESIAN_POINT('Ctrl Pts',(25.701329838895,-13.8792135356312,21.8494149308997)) ;
#58448 = CARTESIAN_POINT('Ctrl Pts',(25.5173038766047,-12.7077475344918,21.6921108285546)) ;
#58449 = CARTESIAN_POINT('Ctrl Pts',(25.4242285328903,-12.1152037168811,21.612535333405)) ;
#58450 = CARTESIAN_POINT('Ctrl Pts',(25.237028663492,-10.923305312252,21.4524453969325)) ;
#58451 = CARTESIAN_POINT('Ctrl Pts',(25.1429040876147,-10.323950725182,21.3719310146869)) ;
#58452 = CARTESIAN_POINT('Ctrl Pts',(25.0017387475006,-9.42491891782229,21.2511341250345)) ;
#58453 = CARTESIAN_POINT('Ctrl Pts',(24.9546872475854,-9.12524166476805,21.2108642461908)) ;
#58454 = CARTESIAN_POINT('Ctrl Pts',(24.8607266279542,-8.52673854618542,21.1304286461072)) ;
#58455 = CARTESIAN_POINT('Ctrl Pts',(24.8138175024392,-8.22791268065011,21.090262931693)) ;
#58456 = CARTESIAN_POINT('Ctrl Pts',(24.7202772386849,-7.63196369303388,21.0101477819253)) ;
#58457 = CARTESIAN_POINT('Ctrl Pts',(24.6736460880534,-7.33484057095624,20.970198361162)) ;
#58458 = CARTESIAN_POINT('Ctrl Pts',(24.5807981071967,-6.74314842709155,20.8906270656642)) ;
#58459 = CARTESIAN_POINT('Ctrl Pts',(24.5345812519569,-6.44857940527084,20.8510052203684)) ;
#58460 = CARTESIAN_POINT('Ctrl Pts',(24.4656699006792,-6.00927996662213,20.7919004542311)) ;
#58461 = CARTESIAN_POINT('Ctrl Pts',(24.4427684514381,-5.86327250392753,20.7722535180421)) ;
#58462 = CARTESIAN_POINT('Ctrl Pts',(24.3971209605381,-5.57221536461865,20.73308243087)) ;
#58463 = CARTESIAN_POINT('Ctrl Pts',(24.3743749181146,-5.42716568800309,20.7135582807878)) ;
#58464 = CARTESIAN_POINT('Ctrl Pts',(24.3290558602293,-5.13813054021944,20.6746459939591)) ;
#58465 = CARTESIAN_POINT('Ctrl Pts',(24.306482840531,-4.99414506905368,20.6552578622012)) ;
#58466 = CARTESIAN_POINT('Ctrl Pts',(24.2615277697454,-4.707344752064,20.616630460914)) ;
#58467 = CARTESIAN_POINT('Ctrl Pts',(24.2391457100099,-4.56452990622502,20.5973912015613)) ;
#58468 = CARTESIAN_POINT('Ctrl Pts',(24.1945910136002,-4.28017726065633,20.5590737905393)) ;
#58469 = CARTESIAN_POINT('Ctrl Pts',(24.1724183597702,-4.1386394618368,20.539995659358)) ;
#58470 = CARTESIAN_POINT('Ctrl Pts',(24.1283018092702,-3.85694733293112,20.5020117151243)) ;
#58471 = CARTESIAN_POINT('Ctrl Pts',(24.1063578737995,-3.71679300276549,20.4831059477265)) ;
#58472 = CARTESIAN_POINT('Ctrl Pts',(24.0736292825901,-3.50767892716341,20.4548834793968)) ;
#58473 = CARTESIAN_POINT('Ctrl Pts',(24.062750988598,-3.43816047206766,20.4454986662434)) ;
#58474 = CARTESIAN_POINT('Ctrl Pts',(24.0410598003719,-3.29950933892018,20.4267751934111)) ;
#58475 = CARTESIAN_POINT('Ctrl Pts',(24.0302469048117,-3.23037666086501,20.417436535294)) ;
#58476 = CARTESIAN_POINT('Ctrl Pts',(24.0086897936963,-3.09251038615833,20.3988057577573)) ;
#58477 = CARTESIAN_POINT('Ctrl Pts',(23.9979455678243,-3.02377678952043,20.3895136504882)) ;
#58478 = CARTESIAN_POINT('Ctrl Pts',(23.9765296674114,-2.8867219835436,20.3709756644882)) ;
#58479 = CARTESIAN_POINT('Ctrl Pts',(23.9658579674197,-2.81840077413193,20.3617298156971)) ;
#58480 = CARTESIAN_POINT('Ctrl Pts',(23.9455218687335,-2.68813967234734,20.3440892799348)) ;
#58481 = CARTESIAN_POINT('Ctrl Pts',(23.9353381116194,-2.62287936476213,20.3352460836472)) ;
#58482 = CARTESIAN_POINT('Ctrl Pts',(23.9197108347794,-2.52265835715845,20.321651314572)) ;
#58483 = CARTESIAN_POINT('Ctrl Pts',(23.9144431544326,-2.48886293034172,20.317064707008)) ;
#58484 = CARTESIAN_POINT('Ctrl Pts',(23.9038525683769,-2.42088369693709,20.3078325293342)) ;
#58485 = CARTESIAN_POINT('Ctrl Pts',(23.8985296510698,-2.38669989030367,20.3031869728647)) ;
#58486 = CARTESIAN_POINT('Ctrl Pts',(23.8878910766815,-2.31833236815792,20.2938873416141)) ;
#58487 = CARTESIAN_POINT('Ctrl Pts',(23.8825753930318,-2.28414866631064,20.2892333024744)) ;
#58488 = CARTESIAN_POINT('Ctrl Pts',(23.8746550147401,-2.23316454048736,20.2822827035826)) ;
#58489 = CARTESIAN_POINT('Ctrl Pts',(23.8720237583063,-2.21621840311006,20.2799709000535)) ;
#58490 = CARTESIAN_POINT('Ctrl Pts',(23.8667871580548,-2.18247182817792,20.2753632967057)) ;
#58491 = CARTESIAN_POINT('Ctrl Pts',(23.8641818127718,-2.16567139061522,20.2730674986103)) ;
#58492 = CARTESIAN_POINT('Ctrl Pts',(23.8590054932055,-2.13226477419477,20.2684974491529)) ;
#58493 = CARTESIAN_POINT('Ctrl Pts',(23.8564345080252,-2.11565859917642,20.2662232118455)) ;
#58494 = CARTESIAN_POINT('Ctrl Pts',(23.8513358993637,-2.08268907041563,20.2617012014733)) ;
#58495 = CARTESIAN_POINT('Ctrl Pts',(23.8488082445528,-2.06632571646822,20.2594534652275)) ;
#58496 = CARTESIAN_POINT('Ctrl Pts',(23.8450568807162,-2.04199922315259,20.2561043915805)) ;
#58497 = CARTESIAN_POINT('Ctrl Pts',(23.8438131291648,-2.03392681584675,20.2549917694768)) ;
#58498 = CARTESIAN_POINT('Ctrl Pts',(23.8413405401307,-2.01786091957008,20.2527741594364)) ;
#58499 = CARTESIAN_POINT('Ctrl Pts',(23.8401117021167,-2.00986743059477,20.2516691721247)) ;
#58500 = CARTESIAN_POINT('Ctrl Pts',(23.8376708072609,-1.99396544467382,20.2494665723942)) ;
#58501 = CARTESIAN_POINT('Ctrl Pts',(23.8364587318387,-1.98605694790282,20.2483689819058)) ;
#58502 = CARTESIAN_POINT('Ctrl Pts',(23.8346551451098,-1.97426250674009,20.2467272984177)) ;
#58503 = CARTESIAN_POINT('Ctrl Pts',(23.834056378304,-1.97034241045512,20.2461808452601)) ;
#58504 = CARTESIAN_POINT('Ctrl Pts',(23.8328641758709,-1.9625257474765,20.245089173729)) ;
#58505 = CARTESIAN_POINT('Ctrl Pts',(23.8322707390673,-1.9586291807694,20.2445439567363)) ;
#58506 = CARTESIAN_POINT('Ctrl Pts',(23.8310891586813,-1.95085564771088,20.2434535479286)) ;
#58507 = CARTESIAN_POINT('Ctrl Pts',(23.8304696089611,-1.94677214569123,20.2428793998139)) ;
#58508 = CARTESIAN_POINT('Ctrl Pts',(23.8292050669332,-1.93841091910833,20.2416990570549)) ;
#58509 = CARTESIAN_POINT('Ctrl Pts',(23.8285600271676,-1.93413319386599,20.2410929180656)) ;
#58510 = CARTESIAN_POINT('Ctrl Pts',(23.8275978307824,-1.92771686893724,20.2401774793944)) ;
#58511 = CARTESIAN_POINT('Ctrl Pts',(23.8272780053549,-1.92557815105288,20.2398712839446)) ;
#58512 = CARTESIAN_POINT('Ctrl Pts',(23.8266446073645,-1.92132513332065,20.239259326347)) ;
#58513 = CARTESIAN_POINT('Ctrl Pts',(23.8263310115037,-1.91921083301692,20.238953591482)) ;
#58514 = CARTESIAN_POINT('Ctrl Pts',(23.8258691296441,-1.91607593361768,20.2384966360183)) ;
#58515 = CARTESIAN_POINT('Ctrl Pts',(23.8257165958113,-1.91503706280771,20.2383445836466)) ;
#58516 = CARTESIAN_POINT('Ctrl Pts',(23.8254151853864,-1.912974549099,20.2380410343312)) ;
#58517 = CARTESIAN_POINT('Ctrl Pts',(23.8252663071272,-1.91195090615706,20.2378895393365)) ;
#58518 = CARTESIAN_POINT('Ctrl Pts',(23.8249732944991,-1.90992189211548,20.2375867971581)) ;
#58519 = CARTESIAN_POINT('Ctrl Pts',(23.8248291348807,-1.90891652284042,20.237435580283)) ;
#58520 = CARTESIAN_POINT('Ctrl Pts',(23.8246178337073,-1.90742446976331,20.237208049006)) ;
#58521 = CARTESIAN_POINT('Ctrl Pts',(23.8245482295593,-1.90692978604951,20.2371320800555)) ;
#58522 = CARTESIAN_POINT('Ctrl Pts',(23.8244111375301,-1.90594614253486,20.2369794778838)) ;
#58523 = CARTESIAN_POINT('Ctrl Pts',(23.8243436339605,-1.90545718208726,20.2369028629261)) ;
#58524 = CARTESIAN_POINT('Ctrl Pts',(23.8242436809488,-1.90472138673829,20.2367856555915)) ;
#58525 = CARTESIAN_POINT('Ctrl Pts',(23.8242083343078,-1.90445904825293,20.2367435249956)) ;
#58526 = CARTESIAN_POINT('Ctrl Pts',(23.8241369872358,-1.90392208066598,20.2366561100854)) ;
#58527 = CARTESIAN_POINT('Ctrl Pts',(23.8241009834238,-1.90364745137547,20.2366108296914)) ;
#58528 = CARTESIAN_POINT('Ctrl Pts',(23.8240307833116,-1.90309850580222,20.2365182408545)) ;
#58529 = CARTESIAN_POINT('Ctrl Pts',(23.823996530879,-1.9028242283647,20.236471010896)) ;
#58530 = CARTESIAN_POINT('Ctrl Pts',(23.8238938369784,-1.90163369618714,20.2362118689699)) ;
#58531 = CARTESIAN_POINT('Ctrl Pts',(23.8238896376073,-1.90158501280405,20.2362012721075)) ;
#58532 = CARTESIAN_POINT('Ctrl Pts',(23.8238854382361,-1.90153632942096,20.2361906752451)) ;
#58533 = CARTESIAN_POINT('',(32.7384401598282,-15.0366437072153,9.07440183902105)) ;
#58534 = CARTESIAN_POINT('',(32.7305102571632,-15.0366437072153,9.10296276716598)) ;
#58535 = CARTESIAN_POINT('Origin',(-1.31615393895548,-21.6462763158694,-0.365428342349794)) ;
#58536 = CARTESIAN_POINT('',(30.1189287294544,-1.90153624409553,8.36247938752316)) ;
#58537 = CARTESIAN_POINT('Ctrl Pts',(30.1189287479468,-1.90153633662063,8.36247939239298)) ;
#58538 = CARTESIAN_POINT('Ctrl Pts',(30.1189401385585,-1.90158489480086,8.36247587712654)) ;
#58539 = CARTESIAN_POINT('Ctrl Pts',(30.1191353360247,-1.9024170216435,8.36241563706908)) ;
#58540 = CARTESIAN_POINT('Ctrl Pts',(30.1192214019803,-1.90281621653025,8.36241402382017)) ;
#58541 = CARTESIAN_POINT('Ctrl Pts',(30.1192793604866,-1.90308876899224,8.36241581627159)) ;
#58542 = CARTESIAN_POINT('Ctrl Pts',(30.1193946823344,-1.90363426439912,8.36242184640268)) ;
#58543 = CARTESIAN_POINT('Ctrl Pts',(30.1194520122693,-1.9039071685372,8.36242617442493)) ;
#58544 = CARTESIAN_POINT('Ctrl Pts',(30.1195637149721,-1.90444076412458,8.36243604721865)) ;
#58545 = CARTESIAN_POINT('Ctrl Pts',(30.119618086374,-1.90470145576606,8.36244159705791)) ;
#58546 = CARTESIAN_POINT('Ctrl Pts',(30.1197702395338,-1.9054325846776,8.3624583701444)) ;
#58547 = CARTESIAN_POINT('Ctrl Pts',(30.1198709015847,-1.90591842777427,8.36247112013853)) ;
#58548 = CARTESIAN_POINT('Ctrl Pts',(30.1200728704408,-1.90689580028702,8.36249869047458)) ;
#58549 = CARTESIAN_POINT('Ctrl Pts',(30.1201741709541,-1.90738733034979,8.36251353397729)) ;
#58550 = CARTESIAN_POINT('Ctrl Pts',(30.1204791499426,-1.90886987163284,8.36256032589338)) ;
#58551 = CARTESIAN_POINT('Ctrl Pts',(30.1206839159759,-1.90986883193724,8.36259449775017)) ;
#58552 = CARTESIAN_POINT('Ctrl Pts',(30.1210963164293,-1.91188491186432,8.3626665380976)) ;
#58553 = CARTESIAN_POINT('Ctrl Pts',(30.1213039399985,-1.91290202966046,8.362704444259)) ;
#58554 = CARTESIAN_POINT('Ctrl Pts',(30.1217216830286,-1.91495139626056,8.3627829555271)) ;
#58555 = CARTESIAN_POINT('Ctrl Pts',(30.1219318017981,-1.91598364510872,8.3628235631576)) ;
#58556 = CARTESIAN_POINT('Ctrl Pts',(30.122565199736,-1.91909856243828,8.36294846757877)) ;
#58557 = CARTESIAN_POINT('Ctrl Pts',(30.122991529876,-1.92119938645565,8.36303580047106)) ;
#58558 = CARTESIAN_POINT('Ctrl Pts',(30.123848049114,-1.92542529670216,8.36321530951135)) ;
#58559 = CARTESIAN_POINT('Ctrl Pts',(30.1242782287435,-1.92755038338676,8.36330752011368)) ;
#58560 = CARTESIAN_POINT('Ctrl Pts',(30.1255676923907,-1.93392581469217,8.36358815687788)) ;
#58561 = CARTESIAN_POINT('Ctrl Pts',(30.1264259082826,-1.93817627749712,8.36378052137526)) ;
#58562 = CARTESIAN_POINT('Ctrl Pts',(30.1281018297584,-1.94648421837564,8.36416207931785)) ;
#58563 = CARTESIAN_POINT('Ctrl Pts',(30.1289195159722,-1.95054169712835,8.36435134305257)) ;
#58564 = CARTESIAN_POINT('Ctrl Pts',(30.1304751568044,-1.95826546741375,8.36471485519461)) ;
#58565 = CARTESIAN_POINT('Ctrl Pts',(30.131254439218,-1.96213697736357,8.36489878055514)) ;
#58566 = CARTESIAN_POINT('Ctrl Pts',(30.1328169909108,-1.96990337558838,8.36527033107019)) ;
#58567 = CARTESIAN_POINT('Ctrl Pts',(30.1336002597047,-1.97379826387693,8.36545795798234)) ;
#58568 = CARTESIAN_POINT('Ctrl Pts',(30.1359560375186,-1.98551686150977,8.36602554379915)) ;
#58569 = CARTESIAN_POINT('Ctrl Pts',(30.1375345305293,-1.99337450320726,8.36641016223176)) ;
#58570 = CARTESIAN_POINT('Ctrl Pts',(30.1407069492262,-2.00917423257069,8.36718904807286)) ;
#58571 = CARTESIAN_POINT('Ctrl Pts',(30.1423008672139,-2.01711632006207,8.36758334307332)) ;
#58572 = CARTESIAN_POINT('Ctrl Pts',(30.1455032942253,-2.03307890599031,8.36837995145598)) ;
#58573 = CARTESIAN_POINT('Ctrl Pts',(30.147111803032,-2.04109940443164,8.36878226562087)) ;
#58574 = CARTESIAN_POINT('Ctrl Pts',(30.1519577546552,-2.06526946862637,8.36999950998952)) ;
#58575 = CARTESIAN_POINT('Ctrl Pts',(30.1552156492126,-2.08152759979058,8.37082464380675)) ;
#58576 = CARTESIAN_POINT('Ctrl Pts',(30.161777398163,-2.11428512181414,8.37249574630261)) ;
#58577 = CARTESIAN_POINT('Ctrl Pts',(30.1650812397105,-2.13078451287836,8.37334176140317)) ;
#58578 = CARTESIAN_POINT('Ctrl Pts',(30.1717258126984,-2.16397631245258,8.37505002748482)) ;
#58579 = CARTESIAN_POINT('Ctrl Pts',(30.175066538635,-2.18066871712369,8.37591229532295)) ;
#58580 = CARTESIAN_POINT('Ctrl Pts',(30.181775597047,-2.21419828956957,8.37764922719805)) ;
#58581 = CARTESIAN_POINT('Ctrl Pts',(30.1851439289196,-2.23103545735225,8.37852389341123)) ;
#58582 = CARTESIAN_POINT('Ctrl Pts',(30.1952762466849,-2.28169173768762,8.38116132325939)) ;
#58583 = CARTESIAN_POINT('Ctrl Pts',(30.2020675740848,-2.31565562693768,8.38293744815023)) ;
#58584 = CARTESIAN_POINT('Ctrl Pts',(30.2156472914047,-2.38358352388148,8.38650036927385)) ;
#58585 = CARTESIAN_POINT('Ctrl Pts',(30.2224356667714,-2.41754751791137,8.38828720736706)) ;
#58586 = CARTESIAN_POINT('Ctrl Pts',(30.2359331378935,-2.48508962397494,8.39184833848321)) ;
#58587 = CARTESIAN_POINT('Ctrl Pts',(30.2426422288818,-2.51866773605419,8.393622648711)) ;
#58588 = CARTESIAN_POINT('Ctrl Pts',(30.2625357546531,-2.61824429305133,8.39889310449012)) ;
#58589 = CARTESIAN_POINT('Ctrl Pts',(30.2754864731247,-2.68308495837333,8.40233666363732)) ;
#58590 = CARTESIAN_POINT('Ctrl Pts',(30.3013241640144,-2.81246585314203,8.40922129508462)) ;
#58591 = CARTESIAN_POINT('Ctrl Pts',(30.314869539521,-2.8803050131185,8.41283935709915)) ;
#58592 = CARTESIAN_POINT('Ctrl Pts',(30.3420387230831,-3.01639281064624,8.4201093040508)) ;
#58593 = CARTESIAN_POINT('Ctrl Pts',(30.3556625207004,-3.08464144827008,8.42376122663904)) ;
#58594 = CARTESIAN_POINT('Ctrl Pts',(30.3829866355126,-3.22153498923157,8.43109557879761)) ;
#58595 = CARTESIAN_POINT('Ctrl Pts',(30.3966869484653,-3.2901798925557,8.43477802363559)) ;
#58596 = CARTESIAN_POINT('Ctrl Pts',(30.4241619433415,-3.42785275438354,8.44217096126773)) ;
#58597 = CARTESIAN_POINT('Ctrl Pts',(30.437936624721,-3.49688071289066,8.44588145602008)) ;
#58598 = CARTESIAN_POINT('Ctrl Pts',(30.4793687882844,-3.70451935672761,8.45705207429126)) ;
#58599 = CARTESIAN_POINT('Ctrl Pts',(30.5071344189108,-3.84368480971854,8.46455122679989)) ;
#58600 = CARTESIAN_POINT('Ctrl Pts',(30.5629347866261,-4.12338942313901,8.47964145340705)) ;
#58601 = CARTESIAN_POINT('Ctrl Pts',(30.5909695077761,-4.26392858364792,8.48723258497366)) ;
#58602 = CARTESIAN_POINT('Ctrl Pts',(30.6472880555991,-4.54627494231513,8.50249717923564)) ;
#58603 = CARTESIAN_POINT('Ctrl Pts',(30.6755718749747,-4.68808213956468,8.51017066751273)) ;
#58604 = CARTESIAN_POINT('Ctrl Pts',(30.7323682666508,-4.97285889995491,8.52559164977468)) ;
#58605 = CARTESIAN_POINT('Ctrl Pts',(30.7608808353976,-5.11582846311061,8.53333915657121)) ;
#58606 = CARTESIAN_POINT('Ctrl Pts',(30.8181141662874,-5.40282428630946,8.54890059787569)) ;
#58607 = CARTESIAN_POINT('Ctrl Pts',(30.8468349266871,-5.54685054635029,8.55671453866051)) ;
#58608 = CARTESIAN_POINT('Ctrl Pts',(30.9044639496286,-5.8358540948004,8.57240174475533)) ;
#58609 = CARTESIAN_POINT('Ctrl Pts',(30.9333722118556,-5.98083138321102,8.58027501119716)) ;
#58610 = CARTESIAN_POINT('Ctrl Pts',(31.0203470861221,-6.41703128872674,8.60397360662014)) ;
#58611 = CARTESIAN_POINT('Ctrl Pts',(31.0786638052327,-6.70952194142243,8.61987765788934)) ;
#58612 = CARTESIAN_POINT('Ctrl Pts',(31.1957973094387,-7.29703932648007,8.65184374517469)) ;
#58613 = CARTESIAN_POINT('Ctrl Pts',(31.2546140842477,-7.59206605887567,8.6679058182651)) ;
#58614 = CARTESIAN_POINT('Ctrl Pts',(31.3725802794297,-8.18381025341842,8.70013793087388)) ;
#58615 = CARTESIAN_POINT('Ctrl Pts',(31.431729694701,-8.48052771556226,8.71630798876412)) ;
#58616 = CARTESIAN_POINT('Ctrl Pts',(31.5501934566931,-9.07480802049958,8.74870711107049)) ;
#58617 = CARTESIAN_POINT('Ctrl Pts',(31.6095078010264,-9.37237086329999,8.76493618408882)) ;
#58618 = CARTESIAN_POINT('Ctrl Pts',(31.7874463810178,-10.2650594398744,8.81363947865428)) ;
#58619 = CARTESIAN_POINT('Ctrl Pts',(31.9060662026799,-10.8601852063993,8.84612962326616)) ;
#58620 = CARTESIAN_POINT('Ctrl Pts',(32.1419495440396,-12.04367402468,8.91077083857098)) ;
#58621 = CARTESIAN_POINT('Ctrl Pts',(32.2592130430851,-12.6320370764873,8.94292198368229)) ;
#58622 = CARTESIAN_POINT('Ctrl Pts',(32.4910381898069,-13.7952376555442,9.00650732543321)) ;
#58623 = CARTESIAN_POINT('Ctrl Pts',(32.6124966123284,-14.4046812756116,9.03983394617206)) ;
#58624 = CARTESIAN_POINT('Ctrl Pts',(32.7316800387708,-15.0027225758531,9.07254634846712)) ;
#58625 = CARTESIAN_POINT('Ctrl Pts',(32.7384401599474,-15.0366437072151,9.07440183859066)) ;
#58626 = CARTESIAN_POINT('Ctrl Pts',(32.7305102570438,-15.0366437072151,9.10296276759541)) ;
#58627 = CARTESIAN_POINT('Ctrl Pts',(32.7237611936063,-15.0027225758262,9.10106745107396)) ;
#58628 = CARTESIAN_POINT('Ctrl Pts',(32.7170046769115,-14.9687639419481,9.09917000900167)) ;
#58629 = CARTESIAN_POINT('Ctrl Pts',(32.5978878264882,-14.3700751826827,9.06571767526185)) ;
#58630 = CARTESIAN_POINT('Ctrl Pts',(32.4835188253644,-13.795237655408,9.03358962842959)) ;
#58631 = CARTESIAN_POINT('Ctrl Pts',(32.2520961165689,-12.6320370762946,8.96855483622168)) ;
#58632 = CARTESIAN_POINT('Ctrl Pts',(32.1350423990285,-12.0436740244586,8.9356481263927)) ;
#58633 = CARTESIAN_POINT('Ctrl Pts',(31.8995980373515,-10.8601852061203,8.86942584911774)) ;
#58634 = CARTESIAN_POINT('Ctrl Pts',(31.7812073725445,-10.2650594395664,8.83611035608409)) ;
#58635 = CARTESIAN_POINT('Ctrl Pts',(31.6036302519827,-9.37237086294862,8.78610520227785)) ;
#58636 = CARTESIAN_POINT('Ctrl Pts',(31.5444393691944,-9.07480802013375,8.76943146095126)) ;
#58637 = CARTESIAN_POINT('Ctrl Pts',(31.4262293521357,-8.4805277151675,8.73611843196877)) ;
#58638 = CARTESIAN_POINT('Ctrl Pts',(31.3672102154762,-8.18381025300921,8.71947915291443)) ;
#58639 = CARTESIAN_POINT('Ctrl Pts',(31.2495126446032,-7.59206605843769,8.68627954296213)) ;
#58640 = CARTESIAN_POINT('Ctrl Pts',(31.1908342052898,-7.29703932602775,8.66971923043497)) ;
#58641 = CARTESIAN_POINT('Ctrl Pts',(31.0739872820367,-6.7095219409415,8.63672097181969)) ;
#58642 = CARTESIAN_POINT('Ctrl Pts',(31.0158187877964,-6.41703128823159,8.62028306280528)) ;
#58643 = CARTESIAN_POINT('Ctrl Pts',(30.9290758403507,-5.98083138269464,8.59574914245178)) ;
#58644 = CARTESIAN_POINT('Ctrl Pts',(30.9002464955277,-5.83585409427698,8.58759164120349)) ;
#58645 = CARTESIAN_POINT('Ctrl Pts',(30.8427790540515,-5.5468505458128,8.57132247125625)) ;
#58646 = CARTESIAN_POINT('Ctrl Pts',(30.8141409570852,-5.40282428576498,8.56321080368639)) ;
#58647 = CARTESIAN_POINT('Ctrl Pts',(30.7570774057057,-5.11582846255216,8.54703787183943)) ;
#58648 = CARTESIAN_POINT('Ctrl Pts',(30.7286519495495,-4.9728588993895,8.53897661384235)) ;
#58649 = CARTESIAN_POINT('Ctrl Pts',(30.672035206872,-4.68808213898542,8.52290859435385)) ;
#58650 = CARTESIAN_POINT('Ctrl Pts',(30.6438439167901,-4.54627494172898,8.51490184567515)) ;
#58651 = CARTESIAN_POINT('Ctrl Pts',(30.5877172444839,-4.26392858304801,8.49894617824804)) ;
#58652 = CARTESIAN_POINT('Ctrl Pts',(30.5597818553244,-4.12338942253229,8.49099728517994)) ;
#58653 = CARTESIAN_POINT('Ctrl Pts',(30.504189085279,-3.8436848090982,8.47515935932977)) ;
#58654 = CARTESIAN_POINT('Ctrl Pts',(30.4765316884238,-3.70451935610049,8.46727038400322)) ;
#58655 = CARTESIAN_POINT('Ctrl Pts',(30.4352711864115,-3.49688071225345,8.45548149669456)) ;
#58656 = CARTESIAN_POINT('Ctrl Pts',(30.4215552919392,-3.42785275374295,8.45155927063588)) ;
#58657 = CARTESIAN_POINT('Ctrl Pts',(30.3942016879009,-3.29017989190842,8.44372912271403)) ;
#58658 = CARTESIAN_POINT('Ctrl Pts',(30.3805639777915,-3.22153498858096,8.43982120280978)) ;
#58659 = CARTESIAN_POINT('Ctrl Pts',(30.3533698603856,-3.08464144761279,8.43201864230363)) ;
#58660 = CARTESIAN_POINT('Ctrl Pts',(30.3398134488531,-3.01639280998565,8.4281240169703)) ;
#58661 = CARTESIAN_POINT('Ctrl Pts',(30.3127852897537,-2.88030501245129,8.4203461458039)) ;
#58662 = CARTESIAN_POINT('Ctrl Pts',(30.2993135317183,-2.8124658524715,8.41646293761831)) ;
#58663 = CARTESIAN_POINT('Ctrl Pts',(30.2736249225872,-2.68308495780993,8.40904136228668)) ;
#58664 = CARTESIAN_POINT('Ctrl Pts',(30.2607526663507,-2.61824429260388,8.40531520779866)) ;
#58665 = CARTESIAN_POINT('Ctrl Pts',(30.2409895522636,-2.51866773578479,8.39957505172038)) ;
#58666 = CARTESIAN_POINT('Ctrl Pts',(30.2343260670344,-2.48508962376557,8.39763648444005)) ;
#58667 = CARTESIAN_POINT('Ctrl Pts',(30.2209247071845,-2.41754751782276,8.39372919189985)) ;
#58668 = CARTESIAN_POINT('Ctrl Pts',(30.2141868277782,-2.38358352385361,8.39176048384098)) ;
#58669 = CARTESIAN_POINT('Ctrl Pts',(30.2007140718384,-2.31565562703126,8.3878123227368)) ;
#58670 = CARTESIAN_POINT('Ctrl Pts',(30.1939791861965,-2.28169173784196,8.38583291305283)) ;
#58671 = CARTESIAN_POINT('Ctrl Pts',(30.1839374998947,-2.23103545759718,8.38286905824464)) ;
#58672 = CARTESIAN_POINT('Ctrl Pts',(30.1806003830226,-2.21419828984458,8.38188196578363)) ;
#58673 = CARTESIAN_POINT('Ctrl Pts',(30.1739561962611,-2.18066871745867,8.37991138738601)) ;
#58674 = CARTESIAN_POINT('Ctrl Pts',(30.1706491257674,-2.16397631281742,8.37892790362093)) ;
#58675 = CARTESIAN_POINT('Ctrl Pts',(30.1640749725642,-2.13078451330256,8.37696600844302)) ;
#58676 = CARTESIAN_POINT('Ctrl Pts',(30.1608078858836,-2.11428512226784,8.37598761429832)) ;
#58677 = CARTESIAN_POINT('Ctrl Pts',(30.1543238608813,-2.08152760030284,8.37403657548676)) ;
#58678 = CARTESIAN_POINT('Ctrl Pts',(30.1511069096249,-2.06526946916755,8.37306397724891)) ;
#58679 = CARTESIAN_POINT('Ctrl Pts',(30.1463270661805,-2.04109940501605,8.37160863277271)) ;
#58680 = CARTESIAN_POINT('Ctrl Pts',(30.1447413892533,-2.03307890658913,8.37112408562097)) ;
#58681 = CARTESIAN_POINT('Ctrl Pts',(30.1415866721682,-2.0171163206894,8.37015564163571)) ;
#58682 = CARTESIAN_POINT('Ctrl Pts',(30.1400176317903,-2.0091742332121,8.36967174559335)) ;
#58683 = CARTESIAN_POINT('Ctrl Pts',(30.1368977644696,-1.99337450387689,8.36870358682289)) ;
#58684 = CARTESIAN_POINT('Ctrl Pts',(30.1353469298989,-1.9855168621936,8.36821935170382)) ;
#58685 = CARTESIAN_POINT('Ctrl Pts',(30.1330357437207,-1.97379826458171,8.3674911613461)) ;
#58686 = CARTESIAN_POINT('Ctrl Pts',(30.1322678624578,-1.96990337630014,8.3672481135615)) ;
#58687 = CARTESIAN_POINT('Ctrl Pts',(30.1307374245282,-1.96213697808921,8.3667608997356)) ;
#58688 = CARTESIAN_POINT('Ctrl Pts',(30.1299748673744,-1.95826546814638,8.36651673543883)) ;
#58689 = CARTESIAN_POINT('Ctrl Pts',(30.1284544952475,-1.95054169771239,8.36602619678552)) ;
#58690 = CARTESIAN_POINT('Ctrl Pts',(30.1276562792614,-1.94648421879626,8.36576680750224)) ;
#58691 = CARTESIAN_POINT('Ctrl Pts',(30.1260235401834,-1.93817627758352,8.36522972036066)) ;
#58692 = CARTESIAN_POINT('Ctrl Pts',(30.1251889974474,-1.93392581460767,8.36495209272972)) ;
#58693 = CARTESIAN_POINT('Ctrl Pts',(30.1239394278513,-1.92755038304578,8.3645277703813)) ;
#58694 = CARTESIAN_POINT('Ctrl Pts',(30.1235232858035,-1.92542529627582,8.36438500091296)) ;
#58695 = CARTESIAN_POINT('Ctrl Pts',(30.122696824537,-1.92119938585934,8.36409723271207)) ;
#58696 = CARTESIAN_POINT('Ctrl Pts',(30.1222864956636,-1.91909856175708,8.36395226840083)) ;
#58697 = CARTESIAN_POINT('Ctrl Pts',(30.1216793691147,-1.91598364430227,8.36373274289128)) ;
#58698 = CARTESIAN_POINT('Ctrl Pts',(30.1214783919202,-1.9149513954132,8.36365921025158)) ;
#58699 = CARTESIAN_POINT('Ctrl Pts',(30.1210799690045,-1.9129020287308,8.36351111415669)) ;
#58700 = CARTESIAN_POINT('Ctrl Pts',(30.1208825225924,-1.91188491089433,8.36343655315723)) ;
#58701 = CARTESIAN_POINT('Ctrl Pts',(30.1204920136106,-1.90986883088622,8.36328566679216)) ;
#58702 = CARTESIAN_POINT('Ctrl Pts',(30.1202989409095,-1.90886987054035,8.36320937932708)) ;
#58703 = CARTESIAN_POINT('Ctrl Pts',(30.1200134937087,-1.90738732919764,8.36309224022347)) ;
#58704 = CARTESIAN_POINT('Ctrl Pts',(30.1199190410322,-1.90689579911753,8.363052733028)) ;
#58705 = CARTESIAN_POINT('Ctrl Pts',(30.1197317685678,-1.90591842656552,8.3629722310425)) ;
#58706 = CARTESIAN_POINT('Ctrl Pts',(30.1196389422281,-1.90543258344669,8.36293125935027)) ;
#58707 = CARTESIAN_POINT('Ctrl Pts',(30.1194999212751,-1.90470145455269,8.3628671883431)) ;
#58708 = CARTESIAN_POINT('Ctrl Pts',(30.1194504715158,-1.90444076295015,8.36284391237914)) ;
#58709 = CARTESIAN_POINT('Ctrl Pts',(30.1193496683133,-1.90390716744248,8.36279478319485)) ;
#58710 = CARTESIAN_POINT('Ctrl Pts',(30.1192983134635,-1.90363426334997,8.36276893489634)) ;
#58711 = CARTESIAN_POINT('Ctrl Pts',(30.1191963902662,-1.9030887680236,8.36271464724955)) ;
#58712 = CARTESIAN_POINT('Ctrl Pts',(30.1191458039838,-1.90281621559788,8.36268630247529)) ;
#58713 = CARTESIAN_POINT('Ctrl Pts',(30.1189452598859,-1.90163369988215,8.36249513250655)) ;
#58714 = CARTESIAN_POINT('Ctrl Pts',(30.1189370039164,-1.90158501825139,8.36248726244976)) ;
#58715 = CARTESIAN_POINT('Ctrl Pts',(30.1189287479468,-1.90153633662063,8.36247939239298)) ;
#58716 = CARTESIAN_POINT('',(33.5228460028118,-15.0366437072153,-5.51081016788309)) ;
#58717 = CARTESIAN_POINT('',(33.5276414405314,-15.0366437072153,-5.48155929182947)) ;
#58718 = CARTESIAN_POINT('Origin',(-1.34794834185301,-21.6462763158694,0.22098491377524)) ;
#58719 = CARTESIAN_POINT('',(30.846513338502,-1.90153624401898,-5.05702918454341)) ;
#58720 = CARTESIAN_POINT('Ctrl Pts',(30.8465133573145,-1.90153633646753,-5.05702918788586)) ;
#58721 = CARTESIAN_POINT('Ctrl Pts',(30.8465222174296,-1.90158489349469,-5.05703716995786)) ;
#58722 = CARTESIAN_POINT('Ctrl Pts',(30.8466735947567,-1.90241450269135,-5.05717354569428)) ;
#58723 = CARTESIAN_POINT('Ctrl Pts',(30.8467507979956,-1.90281253748369,-5.05721107343719)) ;
#58724 = CARTESIAN_POINT('Ctrl Pts',(30.8468039942045,-1.90308429852252,-5.05723373643577)) ;
#58725 = CARTESIAN_POINT('Ctrl Pts',(30.8469108725669,-1.90362821098621,-5.05727659697971)) ;
#58726 = CARTESIAN_POINT('Ctrl Pts',(30.8469645623025,-1.90390032361635,-5.05729669871857)) ;
#58727 = CARTESIAN_POINT('Ctrl Pts',(30.8470697757015,-1.90443237212193,-5.05733456015849)) ;
#58728 = CARTESIAN_POINT('Ctrl Pts',(30.8471213002402,-1.90469230818705,-5.0573523147612)) ;
#58729 = CARTESIAN_POINT('Ctrl Pts',(30.8472660029257,-1.9054212966801,-5.05740087187633)) ;
#58730 = CARTESIAN_POINT('Ctrl Pts',(30.8473624268972,-1.90590571009083,-5.05743149773807)) ;
#58731 = CARTESIAN_POINT('Ctrl Pts',(30.8475567254483,-1.90688020657611,-5.05749114352901)) ;
#58732 = CARTESIAN_POINT('Ctrl Pts',(30.8476546040474,-1.90737029029904,-5.05752013976912)) ;
#58733 = CARTESIAN_POINT('Ctrl Pts',(30.8479501620357,-1.90884846925176,-5.05760553053476)) ;
#58734 = CARTESIAN_POINT('Ctrl Pts',(30.8481497568644,-1.90984449025548,-5.05766036572074)) ;
#58735 = CARTESIAN_POINT('Ctrl Pts',(30.8485530904156,-1.91185463829672,-5.05776788797037)) ;
#58736 = CARTESIAN_POINT('Ctrl Pts',(30.8487568350939,-1.91286876350774,-5.05782053637219)) ;
#58737 = CARTESIAN_POINT('Ctrl Pts',(30.8491677134176,-1.91491210053778,-5.0579244329126)) ;
#58738 = CARTESIAN_POINT('Ctrl Pts',(30.8493748474824,-1.91594131239982,-5.05797567854647)) ;
#58739 = CARTESIAN_POINT('Ctrl Pts',(30.8500002927029,-1.91904706548742,-5.05812789724197)) ;
#58740 = CARTESIAN_POINT('Ctrl Pts',(30.8504226362961,-1.92114170896659,-5.05822739720598)) ;
#58741 = CARTESIAN_POINT('Ctrl Pts',(30.8512728440463,-1.92535518708964,-5.0584236247972)) ;
#58742 = CARTESIAN_POINT('Ctrl Pts',(30.8517007140664,-1.92747402218885,-5.05852031724317)) ;
#58743 = CARTESIAN_POINT('Ctrl Pts',(30.8529850289116,-1.93383069872744,-5.05880631432421)) ;
#58744 = CARTESIAN_POINT('Ctrl Pts',(30.8538421570137,-1.9380686583443,-5.05899160211352)) ;
#58745 = CARTESIAN_POINT('Ctrl Pts',(30.8555184296128,-1.94635216115927,-5.05934807613925)) ;
#58746 = CARTESIAN_POINT('Ctrl Pts',(30.8563375860309,-1.95039770503674,-5.05951919052795)) ;
#58747 = CARTESIAN_POINT('Ctrl Pts',(30.8578974438038,-1.95809865321679,-5.05984161264589)) ;
#58748 = CARTESIAN_POINT('Ctrl Pts',(30.8586795936983,-1.96195867181558,-5.06000146823871)) ;
#58749 = CARTESIAN_POINT('Ctrl Pts',(30.8602490506149,-1.96970201797824,-5.06031949703638)) ;
#58750 = CARTESIAN_POINT('Ctrl Pts',(30.8610363579311,-1.9735853455555,-5.06047766846358)) ;
#58751 = CARTESIAN_POINT('Ctrl Pts',(30.8634056537684,-1.98526916037067,-5.06095042086467)) ;
#58752 = CARTESIAN_POINT('Ctrl Pts',(30.864995008453,-1.99310347927764,-5.06126328654964)) ;
#58753 = CARTESIAN_POINT('Ctrl Pts',(30.8681917232794,-2.00885631246943,-5.06188674003531)) ;
#58754 = CARTESIAN_POINT('Ctrl Pts',(30.8697990880122,-2.01677482657967,-5.06219729960863)) ;
#58755 = CARTESIAN_POINT('Ctrl Pts',(30.8730303783887,-2.03269003305421,-5.06281726598735)) ;
#58756 = CARTESIAN_POINT('Ctrl Pts',(30.8746543041626,-2.04068672542293,-5.06312667200092)) ;
#58757 = CARTESIAN_POINT('Ctrl Pts',(30.8795488777629,-2.06478504921205,-5.06405411240299)) ;
#58758 = CARTESIAN_POINT('Ctrl Pts',(30.8828423047139,-2.08099492385557,-5.06467146935712)) ;
#58759 = CARTESIAN_POINT('Ctrl Pts',(30.8894794710646,-2.11365521686435,-5.06590655965855)) ;
#58760 = CARTESIAN_POINT('Ctrl Pts',(30.8928232182896,-2.13010563543453,-5.0665242455345)) ;
#58761 = CARTESIAN_POINT('Ctrl Pts',(30.8995508921739,-2.16319891724182,-5.06776036095689)) ;
#58762 = CARTESIAN_POINT('Ctrl Pts',(30.9029348209093,-2.17984177664019,-5.06837877293634)) ;
#58763 = CARTESIAN_POINT('Ctrl Pts',(30.9097328497242,-2.21327182895652,-5.06961593039811)) ;
#58764 = CARTESIAN_POINT('Ctrl Pts',(30.9131469501731,-2.23005902188247,-5.07023467363518)) ;
#58765 = CARTESIAN_POINT('Ctrl Pts',(30.9234195990794,-2.28056494806296,-5.07209017971721)) ;
#58766 = CARTESIAN_POINT('Ctrl Pts',(30.9303084833242,-2.31442802843042,-5.07332629036645)) ;
#58767 = CARTESIAN_POINT('Ctrl Pts',(30.944088063969,-2.38215430760561,-5.07578760930222)) ;
#58768 = CARTESIAN_POINT('Ctrl Pts',(30.950978764724,-2.41601749274999,-5.07701277357059)) ;
#58769 = CARTESIAN_POINT('Ctrl Pts',(30.9646831779117,-2.48335912659609,-5.07944125064379)) ;
#58770 = CARTESIAN_POINT('Ctrl Pts',(30.9714968932376,-2.51683757534333,-5.0806445458594)) ;
#58771 = CARTESIAN_POINT('Ctrl Pts',(30.9917045603659,-2.61611857900844,-5.08420404090918)) ;
#58772 = CARTESIAN_POINT('Ctrl Pts',(31.004865014558,-2.68076679099434,-5.08650996413046)) ;
#58773 = CARTESIAN_POINT('Ctrl Pts',(31.0311232411281,-2.80974421165781,-5.09109666028362)) ;
#58774 = CARTESIAN_POINT('Ctrl Pts',(31.0448908713434,-2.87736249833903,-5.09349292481004)) ;
#58775 = CARTESIAN_POINT('Ctrl Pts',(31.0725112415595,-3.01300721611788,-5.09828766776301)) ;
#58776 = CARTESIAN_POINT('Ctrl Pts',(31.08636398788,-3.081033647288,-5.10068610773375)) ;
#58777 = CARTESIAN_POINT('Ctrl Pts',(31.114151471521,-3.21748148519082,-5.10548740352965)) ;
#58778 = CARTESIAN_POINT('Ctrl Pts',(31.1280862113957,-3.28590289190996,-5.10789024375613)) ;
#58779 = CARTESIAN_POINT('Ctrl Pts',(31.1560347071644,-3.42312751338264,-5.11270166654699)) ;
#58780 = CARTESIAN_POINT('Ctrl Pts',(31.1700484633858,-3.4919307281396,-5.11511024711247)) ;
#58781 = CARTESIAN_POINT('Ctrl Pts',(31.2122039196158,-3.69889333451627,-5.12234582513575)) ;
#58782 = CARTESIAN_POINT('Ctrl Pts',(31.240459789465,-3.83760568758789,-5.1271827661939)) ;
#58783 = CARTESIAN_POINT('Ctrl Pts',(31.2972534436847,-4.1163996286529,-5.13688609625301)) ;
#58784 = CARTESIAN_POINT('Ctrl Pts',(31.3257912376979,-4.25648121672555,-5.14175242653772)) ;
#58785 = CARTESIAN_POINT('Ctrl Pts',(31.383126632306,-4.53790830204276,-5.15151484518891)) ;
#58786 = CARTESIAN_POINT('Ctrl Pts',(31.4119242370105,-4.67925379837917,-5.15641090732875)) ;
#58787 = CARTESIAN_POINT('Ctrl Pts',(31.4697573566568,-4.96310337250663,-5.16623180664519)) ;
#58788 = CARTESIAN_POINT('Ctrl Pts',(31.498792873749,-5.10560745031275,-5.17115663072387)) ;
#58789 = CARTESIAN_POINT('Ctrl Pts',(31.5570800476211,-5.39166886241539,-5.18103330707449)) ;
#58790 = CARTESIAN_POINT('Ctrl Pts',(31.586331705452,-5.53522619670961,-5.1859851529319)) ;
#58791 = CARTESIAN_POINT('Ctrl Pts',(31.6450294699151,-5.82328879730879,-5.19591364069515)) ;
#58792 = CARTESIAN_POINT('Ctrl Pts',(31.674475576737,-5.96779406361505,-5.20089028144113)) ;
#58793 = CARTESIAN_POINT('Ctrl Pts',(31.7630731119485,-6.40257377433977,-5.21585357516904)) ;
#58794 = CARTESIAN_POINT('Ctrl Pts',(31.8224837418014,-6.69411212587316,-5.22587367466452)) ;
#58795 = CARTESIAN_POINT('Ctrl Pts',(31.9418234967792,-7.27971665165263,-5.24598021423759)) ;
#58796 = CARTESIAN_POINT('Ctrl Pts',(32.0017526281241,-7.57378282593234,-5.25606661641785)) ;
#58797 = CARTESIAN_POINT('Ctrl Pts',(32.1219569994905,-8.16360039960541,-5.27628094520372)) ;
#58798 = CARTESIAN_POINT('Ctrl Pts',(32.1822322425905,-8.45935179899548,-5.28640885302693)) ;
#58799 = CARTESIAN_POINT('Ctrl Pts',(32.3029566284287,-9.05169722610276,-5.30668029492975)) ;
#58800 = CARTESIAN_POINT('Ctrl Pts',(32.36340577261,-9.34829125382689,-5.31682382021219)) ;
#58801 = CARTESIAN_POINT('Ctrl Pts',(32.5447559097541,-10.2380733851616,-5.34723796026816)) ;
#58802 = CARTESIAN_POINT('Ctrl Pts',(32.6656595787642,-10.8312615215168,-5.36749229368494)) ;
#58803 = CARTESIAN_POINT('Ctrl Pts',(32.9060980789528,-12.0108970979659,-5.40773998693454)) ;
#58804 = CARTESIAN_POINT('Ctrl Pts',(33.0256329226131,-12.5973445381112,-5.42773327069192)) ;
#58805 = CARTESIAN_POINT('Ctrl Pts',(33.2619584102353,-13.7567579308779,-5.46723756451734)) ;
#58806 = CARTESIAN_POINT('Ctrl Pts',(33.3787490601544,-14.3297238834965,-5.48674853824458)) ;
#58807 = CARTESIAN_POINT('Ctrl Pts',(33.5032839103796,-14.9406748975524,-5.50754381324112)) ;
#58808 = CARTESIAN_POINT('Ctrl Pts',(33.513072690413,-14.9886972685039,-5.50917831400048)) ;
#58809 = CARTESIAN_POINT('Ctrl Pts',(33.5228460026744,-15.0366437072149,-5.51081016871875)) ;
#58810 = CARTESIAN_POINT('Ctrl Pts',(33.527641440668,-15.0366437072149,-5.48155929099309)) ;
#58811 = CARTESIAN_POINT('Ctrl Pts',(33.5178586766078,-14.9886972685318,-5.4799850897331)) ;
#58812 = CARTESIAN_POINT('Ctrl Pts',(33.5080604095794,-14.9406748976083,-5.47840845711907)) ;
#58813 = CARTESIAN_POINT('Ctrl Pts',(33.3834046007263,-14.329723883609,-5.45835099718485)) ;
#58814 = CARTESIAN_POINT('Ctrl Pts',(33.266497687206,-13.7567579310195,-5.43954920008858)) ;
#58815 = CARTESIAN_POINT('Ctrl Pts',(33.0299293079761,-12.5973445383116,-5.40152647960156)) ;
#58816 = CARTESIAN_POINT('Ctrl Pts',(32.9102678482249,-12.0108970981961,-5.38230551986948)) ;
#58817 = CARTESIAN_POINT('Ctrl Pts',(32.6695643910199,-10.8312615218069,-5.34367399299853)) ;
#58818 = CARTESIAN_POINT('Ctrl Pts',(32.5485224060297,-10.2380733854818,-5.32426334977515)) ;
#58819 = CARTESIAN_POINT('Ctrl Pts',(32.3669540920221,-9.3482912541922,-5.29518002976905)) ;
#58820 = CARTESIAN_POINT('Ctrl Pts',(32.3064304257025,-9.0516972264831,-5.28549106944013)) ;
#58821 = CARTESIAN_POINT('Ctrl Pts',(32.1855528762123,-8.45935179940588,-5.26615388452188)) ;
#58822 = CARTESIAN_POINT('Ctrl Pts',(32.1251989944828,-8.16360040003082,-5.25650565113774)) ;
#58823 = CARTESIAN_POINT('Ctrl Pts',(32.0048324746615,-7.57378282638767,-5.23728038420972)) ;
#58824 = CARTESIAN_POINT('Ctrl Pts',(31.9448198396494,-7.2797166521229,-5.22770333188501)) ;
#58825 = CARTESIAN_POINT('Ctrl Pts',(31.8253070935512,-6.69411212637314,-5.20865199150334)) ;
#58826 = CARTESIAN_POINT('Ctrl Pts',(31.7658069886711,-6.40257377485455,-5.19917766554801)) ;
#58827 = CARTESIAN_POINT('Ctrl Pts',(31.6770694508902,-5.9677940641519,-5.185068349742)) ;
#58828 = CARTESIAN_POINT('Ctrl Pts',(31.6475757053778,-5.82328879785296,-5.18038229216232)) ;
#58829 = CARTESIAN_POINT('Ctrl Pts',(31.5887804014113,-5.53522619726841,-5.17104876906804)) ;
#58830 = CARTESIAN_POINT('Ctrl Pts',(31.5594788431478,-5.39166886298147,-5.16640130239347)) ;
#58831 = CARTESIAN_POINT('Ctrl Pts',(31.5010891801201,-5.10560745089334,-5.15714978225379)) ;
#58832 = CARTESIAN_POINT('Ctrl Pts',(31.4720010764086,-4.96310337309446,-5.15254572237146)) ;
#58833 = CARTESIAN_POINT('Ctrl Pts',(31.4140595090003,-4.67925379898137,-5.14338632515737)) ;
#58834 = CARTESIAN_POINT('Ctrl Pts',(31.3852060474466,-4.53790830265215,-5.13883097473451)) ;
#58835 = CARTESIAN_POINT('Ctrl Pts',(31.3277548237149,-4.25648121734925,-5.12977508249897)) ;
#58836 = CARTESIAN_POINT('Ctrl Pts',(31.2991570660168,-4.11639962928367,-5.12527451452018)) ;
#58837 = CARTESIAN_POINT('Ctrl Pts',(31.2422380913601,-3.83760568823281,-5.11633560532754)) ;
#58838 = CARTESIAN_POINT('Ctrl Pts',(31.213916884013,-3.69889333516823,-5.11189720538476)) ;
#58839 = CARTESIAN_POINT('Ctrl Pts',(31.1716578011018,-3.49193072880207,-5.10529372216643)) ;
#58840 = CARTESIAN_POINT('Ctrl Pts',(31.1576085571185,-3.42312751404861,-5.10310160737705)) ;
#58841 = CARTESIAN_POINT('Ctrl Pts',(31.1295867818156,-3.28590289258288,-5.09873716997887)) ;
#58842 = CARTESIAN_POINT('Ctrl Pts',(31.1156142508242,-3.21748148586721,-5.09656484537069)) ;
#58843 = CARTESIAN_POINT('Ctrl Pts',(31.0877482927399,-3.08103364797132,-5.09224222251172)) ;
#58844 = CARTESIAN_POINT('Ctrl Pts',(31.0738548682071,-3.01300721680465,-5.09009190866395)) ;
#58845 = CARTESIAN_POINT('Ctrl Pts',(31.0461493680224,-2.87736249903269,-5.08581643555565)) ;
#58846 = CARTESIAN_POINT('Ctrl Pts',(31.0323372986602,-2.80974421235489,-5.08369123783789)) ;
#58847 = CARTESIAN_POINT('Ctrl Pts',(31.0059890678275,-2.6807667914274,-5.07965354306197)) ;
#58848 = CARTESIAN_POINT('Ctrl Pts',(30.9927812368087,-2.61611857916068,-5.07763660534097)) ;
#58849 = CARTESIAN_POINT('Ctrl Pts',(30.9724948246683,-2.51683757506432,-5.07455743306453)) ;
#58850 = CARTESIAN_POINT('Ctrl Pts',(30.9656535716986,-2.48335912617165,-5.07352210985946)) ;
#58851 = CARTESIAN_POINT('Ctrl Pts',(30.951891124577,-2.41601749203304,-5.07144762374931)) ;
#58852 = CARTESIAN_POINT('Ctrl Pts',(30.9449699332981,-2.3821543067416,-5.07040844326081)) ;
#58853 = CARTESIAN_POINT('Ctrl Pts',(30.9311257670399,-2.3144280272722,-5.06834107876254)) ;
#58854 = CARTESIAN_POINT('Ctrl Pts',(30.9242028019896,-2.28056494675763,-5.06731285164283)) ;
#58855 = CARTESIAN_POINT('Ctrl Pts',(30.913875427701,-2.23005902035775,-5.06579115534548)) ;
#58856 = CARTESIAN_POINT('Ctrl Pts',(30.9104424789034,-2.21327182735896,-5.065287381856)) ;
#58857 = CARTESIAN_POINT('Ctrl Pts',(30.9036052790388,-2.17984177489741,-5.06428915704125)) ;
#58858 = CARTESIAN_POINT('Ctrl Pts',(30.9002010283375,-2.16319891542671,-5.06379470347773)) ;
#58859 = CARTESIAN_POINT('Ctrl Pts',(30.8934308332709,-2.1301056334757,-5.06281795560951)) ;
#58860 = CARTESIAN_POINT('Ctrl Pts',(30.8900648925502,-2.11365521483403,-5.06233564397707)) ;
#58861 = CARTESIAN_POINT('Ctrl Pts',(30.8833807945581,-2.08099492168341,-5.06138682384278)) ;
#58862 = CARTESIAN_POINT('Ctrl Pts',(30.8800626450252,-2.06478504696959,-5.06092026787666)) ;
#58863 = CARTESIAN_POINT('Ctrl Pts',(30.8751281536704,-2.04068672307579,-5.06023631487228)) ;
#58864 = CARTESIAN_POINT('Ctrl Pts',(30.8734904414429,-2.03269003067224,-5.06001100246102)) ;
#58865 = CARTESIAN_POINT('Ctrl Pts',(30.8702303426428,-2.01677482412858,-5.059566759604)) ;
#58866 = CARTESIAN_POINT('Ctrl Pts',(30.8686079562032,-2.00885630998394,-5.05934782834478)) ;
#58867 = CARTESIAN_POINT('Ctrl Pts',(30.8653795095944,-1.99310347672373,-5.05891793008136)) ;
#58868 = CARTESIAN_POINT('Ctrl Pts',(30.863773454092,-1.98526915778259,-5.05870693483445)) ;
#58869 = CARTESIAN_POINT('Ctrl Pts',(30.8613772328026,-1.9735853429167,-5.05839842036086)) ;
#58870 = CARTESIAN_POINT('Ctrl Pts',(30.8605806341427,-1.9697020153227,-5.0582969236015)) ;
#58871 = CARTESIAN_POINT('Ctrl Pts',(30.8589917862301,-1.96195866912642,-5.05809717460429)) ;
#58872 = CARTESIAN_POINT('Ctrl Pts',(30.858199537266,-1.95809865051073,-5.05799892058861)) ;
#58873 = CARTESIAN_POINT('Ctrl Pts',(30.8566183832002,-1.95039770220822,-5.05780639995442)) ;
#58874 = CARTESIAN_POINT('Ctrl Pts',(30.8557874699109,-1.94635215821993,-5.05770699916629)) ;
#58875 = CARTESIAN_POINT('Ctrl Pts',(30.8540851221175,-1.93806865517772,-5.05750957649875)) ;
#58876 = CARTESIAN_POINT('Ctrl Pts',(30.8532136992519,-1.93383069544475,-5.0574114827615)) ;
#58877 = CARTESIAN_POINT('Ctrl Pts',(30.8519052948742,-1.92747401873175,-5.05727242510519)) ;
#58878 = CARTESIAN_POINT('Ctrl Pts',(30.8514689484325,-1.92535518357459,-5.05722743646948)) ;
#58879 = CARTESIAN_POINT('Ctrl Pts',(30.8506005905671,-1.92114170533599,-5.05714191953601)) ;
#58880 = CARTESIAN_POINT('Ctrl Pts',(30.8501685848271,-1.9190470617987,-5.05710135598556)) ;
#58881 = CARTESIAN_POINT('Ctrl Pts',(30.8495272760002,-1.91594130862596,-5.05704590089974)) ;
#58882 = CARTESIAN_POINT('Ctrl Pts',(30.8493146219259,-1.91491209673629,-5.0570283257986)) ;
#58883 = CARTESIAN_POINT('Ctrl Pts',(30.8488920774437,-1.91286875965011,-5.05699558960563)) ;
#58884 = CARTESIAN_POINT('Ctrl Pts',(30.8486821874486,-1.9118546344095,-5.05698042594019)) ;
#58885 = CARTESIAN_POINT('Ctrl Pts',(30.8482656350974,-1.90984448631342,-5.05695353473325)) ;
#58886 = CARTESIAN_POINT('Ctrl Pts',(30.8480589794452,-1.90884846528467,-5.05694176863321)) ;
#58887 = CARTESIAN_POINT('Ctrl Pts',(30.8477516275676,-1.90737028629171,-5.05692831735834)) ;
#58888 = CARTESIAN_POINT('Ctrl Pts',(30.8476496140468,-1.90688020255704,-5.05692454300991)) ;
#58889 = CARTESIAN_POINT('Ctrl Pts',(30.8474464414083,-1.90590570604561,-5.05691902672418)) ;
#58890 = CARTESIAN_POINT('Ctrl Pts',(30.8473452860647,-1.90542129261717,-5.05691726093279)) ;
#58891 = CARTESIAN_POINT('Ctrl Pts',(30.8471926538241,-1.90469230450297,-5.05691707244812)) ;
#58892 = CARTESIAN_POINT('Ctrl Pts',(30.8471381574318,-1.9044323688528,-5.05691744588009)) ;
#58893 = CARTESIAN_POINT('Ctrl Pts',(30.8470263625795,-1.90390032118951,-5.05691973060544)) ;
#58894 = CARTESIAN_POINT('Ctrl Pts',(30.8469690648644,-1.90362820899944,-5.05692163712989)) ;
#58895 = CARTESIAN_POINT('Ctrl Pts',(30.8468540959934,-1.90308429739362,-5.05692812760186)) ;
#58896 = CARTESIAN_POINT('Ctrl Pts',(30.8467964482283,-1.90281253677263,-5.05693261842809)) ;
#58897 = CARTESIAN_POINT('Ctrl Pts',(30.8465349543911,-1.90163369810809,-5.05702182057777)) ;
#58898 = CARTESIAN_POINT('Ctrl Pts',(30.8465241558528,-1.90158501728781,-5.05702550423181)) ;
#58899 = CARTESIAN_POINT('Ctrl Pts',(30.8465133573145,-1.90153633646753,-5.05702918788586)) ;
#58900 = CARTESIAN_POINT('',(28.1105818993065,-15.0366437072153,-19.0773535407052)) ;
#58901 = CARTESIAN_POINT('',(28.12721624477,-15.0366437072153,-19.0528197166357)) ;
#58902 = CARTESIAN_POINT('Origin',(-1.13057562514854,-21.6462763158694,0.766549294070821)) ;
#58903 = CARTESIAN_POINT('',(25.8721458475363,-1.90153624261815,-17.5417501561681)) ;
#58904 = CARTESIAN_POINT('Ctrl Pts',(25.8721458629685,-1.90153633366587,-17.541750166936)) ;
#58905 = CARTESIAN_POINT('Ctrl Pts',(25.8721505680015,-1.90158489404723,-17.541761110063)) ;
#58906 = CARTESIAN_POINT('Ctrl Pts',(25.872231662671,-1.90242186758655,-17.5419497228258)) ;
#58907 = CARTESIAN_POINT('Ctrl Pts',(25.8722864941205,-1.90282329671317,-17.5420166801772)) ;
#58908 = CARTESIAN_POINT('Ctrl Pts',(25.8723256207478,-1.90309737338209,-17.5420599024175)) ;
#58909 = CARTESIAN_POINT('Ctrl Pts',(25.87240535646,-1.90364591739461,-17.542144304304)) ;
#58910 = CARTESIAN_POINT('Ctrl Pts',(25.8724460128044,-1.90392034589288,-17.5421853999427)) ;
#58911 = CARTESIAN_POINT('Ctrl Pts',(25.8725263299213,-1.90445692101583,-17.5422645367358)) ;
#58912 = CARTESIAN_POINT('Ctrl Pts',(25.8725659935202,-1.90471906782239,-17.5423025737883)) ;
#58913 = CARTESIAN_POINT('Ctrl Pts',(25.8726779452118,-1.90545432006084,-17.5424082166215)) ;
#58914 = CARTESIAN_POINT('Ctrl Pts',(25.8727532776597,-1.90594291769499,-17.5424770373722)) ;
#58915 = CARTESIAN_POINT('Ctrl Pts',(25.8729059462109,-1.90692583135594,-17.542613829521)) ;
#58916 = CARTESIAN_POINT('Ctrl Pts',(25.8729832960174,-1.90742014803357,-17.5426817809481)) ;
#58917 = CARTESIAN_POINT('Ctrl Pts',(25.8732177773336,-1.90891109407639,-17.5428849930091)) ;
#58918 = CARTESIAN_POINT('Ctrl Pts',(25.8733773182412,-1.909915717438,-17.5430196438642)) ;
#58919 = CARTESIAN_POINT('Ctrl Pts',(25.8737010965169,-1.91194322613707,-17.5432887438504)) ;
#58920 = CARTESIAN_POINT('Ctrl Pts',(25.873865355643,-1.91296610964748,-17.543423160218)) ;
#58921 = CARTESIAN_POINT('Ctrl Pts',(25.8741975644926,-1.91502709322433,-17.5436921532795)) ;
#58922 = CARTESIAN_POINT('Ctrl Pts',(25.8743655156668,-1.91606519333414,-17.5438267278498)) ;
#58923 = CARTESIAN_POINT('Ctrl Pts',(25.8748737080304,-1.91919776711167,-17.5442307815105)) ;
#58924 = CARTESIAN_POINT('Ctrl Pts',(25.8752182593229,-1.92131049897224,-17.5445006273183)) ;
#58925 = CARTESIAN_POINT('Ctrl Pts',(25.8759135806846,-1.92556036178824,-17.545040131977)) ;
#58926 = CARTESIAN_POINT('Ctrl Pts',(25.8762643709515,-1.92769749319939,-17.5453097612064)) ;
#58927 = CARTESIAN_POINT('Ctrl Pts',(25.877319104743,-1.93410905870646,-17.5461152268159)) ;
#58928 = CARTESIAN_POINT('Ctrl Pts',(25.8780253649344,-1.93838361099844,-17.5466476898942)) ;
#58929 = CARTESIAN_POINT('Ctrl Pts',(25.8794090677594,-1.9467386359022,-17.5476836482434)) ;
#58930 = CARTESIAN_POINT('Ctrl Pts',(25.8800865515514,-1.95081910919327,-17.5481870830604)) ;
#58931 = CARTESIAN_POINT('Ctrl Pts',(25.8813781226031,-1.95858685031422,-17.5491426562885)) ;
#58932 = CARTESIAN_POINT('Ctrl Pts',(25.8820265367721,-1.96248050050301,-17.5496201673265)) ;
#58933 = CARTESIAN_POINT('Ctrl Pts',(25.8833287929376,-1.97029131284115,-17.5505758423184)) ;
#58934 = CARTESIAN_POINT('Ctrl Pts',(25.8839826359515,-1.97420847500389,-17.5510540047764)) ;
#58935 = CARTESIAN_POINT('Ctrl Pts',(25.8859516548851,-1.98599408824657,-17.5524900126839)) ;
#58936 = CARTESIAN_POINT('Ctrl Pts',(25.887274293954,-1.99389666566597,-17.5534494179564)) ;
#58937 = CARTESIAN_POINT('Ctrl Pts',(25.8899370080667,-2.00978674928339,-17.5553737876842)) ;
#58938 = CARTESIAN_POINT('Ctrl Pts',(25.8912770992061,-2.01777425530681,-17.5563387283357)) ;
#58939 = CARTESIAN_POINT('Ctrl Pts',(25.8939729216926,-2.03382812662241,-17.5582745822623)) ;
#58940 = CARTESIAN_POINT('Ctrl Pts',(25.8953286535016,-2.04189449191906,-17.5592454948569)) ;
#58941 = CARTESIAN_POINT('Ctrl Pts',(25.8994170370107,-2.06620277743539,-17.5621671920232)) ;
#58942 = CARTESIAN_POINT('Ctrl Pts',(25.9021708189187,-2.08255388382099,-17.5641270200586)) ;
#58943 = CARTESIAN_POINT('Ctrl Pts',(25.9077242644949,-2.11549873574347,-17.5680683583183)) ;
#58944 = CARTESIAN_POINT('Ctrl Pts',(25.9105239553166,-2.13209248148531,-17.5700498285693)) ;
#58945 = CARTESIAN_POINT('Ctrl Pts',(25.9161597913601,-2.16547409398065,-17.5740304885995)) ;
#58946 = CARTESIAN_POINT('Ctrl Pts',(25.9189959458912,-2.18226195689482,-17.5760296632346)) ;
#58947 = CARTESIAN_POINT('Ctrl Pts',(25.9246957238415,-2.21598327350102,-17.5800411132428)) ;
#58948 = CARTESIAN_POINT('Ctrl Pts',(25.9275593485239,-2.23291672720091,-17.5820533867552)) ;
#58949 = CARTESIAN_POINT('Ctrl Pts',(25.9361782978858,-2.28386269296286,-17.5881024187311)) ;
#58950 = CARTESIAN_POINT('Ctrl Pts',(25.9419616569795,-2.3180208093972,-17.5921514488495)) ;
#58951 = CARTESIAN_POINT('Ctrl Pts',(25.9535346243998,-2.38633716071619,-17.6002403357774)) ;
#58952 = CARTESIAN_POINT('Ctrl Pts',(25.959324255279,-2.42049538193591,-17.6042801542918)) ;
#58953 = CARTESIAN_POINT('Ctrl Pts',(25.9708422681443,-2.488423735256,-17.6123072114952)) ;
#58954 = CARTESIAN_POINT('Ctrl Pts',(25.9765706601812,-2.52219386740186,-17.616294435377)) ;
#58955 = CARTESIAN_POINT('Ctrl Pts',(25.9935634036828,-2.62233986322234,-17.6281111292612)) ;
#58956 = CARTESIAN_POINT('Ctrl Pts',(26.0046352573757,-2.68755132592453,-17.6357957174787)) ;
#58957 = CARTESIAN_POINT('Ctrl Pts',(26.0267419583726,-2.81770994402766,-17.6511221421599)) ;
#58958 = CARTESIAN_POINT('Ctrl Pts',(26.0383411847504,-2.88597501380354,-17.6591534154139)) ;
#58959 = CARTESIAN_POINT('Ctrl Pts',(26.0616166564067,-3.02291720165828,-17.6752541057803)) ;
#58960 = CARTESIAN_POINT('Ctrl Pts',(26.0732929237367,-3.09159431980986,-17.6833234903958)) ;
#58961 = CARTESIAN_POINT('Ctrl Pts',(26.0967186911401,-3.22934730962459,-17.6995010917953)) ;
#58962 = CARTESIAN_POINT('Ctrl Pts',(26.1084682001473,-3.29842318127411,-17.7076092953976)) ;
#58963 = CARTESIAN_POINT('Ctrl Pts',(26.1320371662318,-3.43696038462189,-17.7238644839388)) ;
#58964 = CARTESIAN_POINT('Ctrl Pts',(26.1438566244585,-3.50642171632358,-17.7320114671818)) ;
#58965 = CARTESIAN_POINT('Ctrl Pts',(26.1794154334704,-3.71536396265693,-17.7565098653357)) ;
#58966 = CARTESIAN_POINT('Ctrl Pts',(26.2032551570819,-3.85540312786147,-17.7729188191408)) ;
#58967 = CARTESIAN_POINT('Ctrl Pts',(26.2511803855432,-4.13686379005994,-17.8058832750933)) ;
#58968 = CARTESIAN_POINT('Ctrl Pts',(26.2752659240111,-4.27828528713331,-17.8224387276865)) ;
#58969 = CARTESIAN_POINT('Ctrl Pts',(26.3236624029499,-4.56240427986944,-17.8556870807628)) ;
#58970 = CARTESIAN_POINT('Ctrl Pts',(26.3479733582527,-4.7051017746222,-17.8723799590352)) ;
#58971 = CARTESIAN_POINT('Ctrl Pts',(26.3968010309501,-4.99166642754464,-17.9058929718701)) ;
#58972 = CARTESIAN_POINT('Ctrl Pts',(26.4213177558355,-5.13553358572935,-17.9227130953899)) ;
#58973 = CARTESIAN_POINT('Ctrl Pts',(26.4705377650822,-5.42433123310099,-17.9564697631733)) ;
#58974 = CARTESIAN_POINT('Ctrl Pts',(26.4952410531139,-5.56926172228562,-17.9734063020221)) ;
#58975 = CARTESIAN_POINT('Ctrl Pts',(26.5448152636506,-5.8600796997275,-18.0073845556476)) ;
#58976 = CARTESIAN_POINT('Ctrl Pts',(26.569686186818,-6.00596718798611,-18.0244262694466)) ;
#58977 = CARTESIAN_POINT('Ctrl Pts',(26.6445222918619,-6.44490565398653,-18.0756919075071)) ;
#58978 = CARTESIAN_POINT('Ctrl Pts',(26.6947107654887,-6.73923262825523,-18.1100563912884)) ;
#58979 = CARTESIAN_POINT('Ctrl Pts',(26.7955346120393,-7.3304385783359,-18.1790660152525)) ;
#58980 = CARTESIAN_POINT('Ctrl Pts',(26.8461700066388,-7.62731755418156,-18.2137111234783)) ;
#58981 = CARTESIAN_POINT('Ctrl Pts',(26.9477402734718,-8.22277685021324,-18.283186169508)) ;
#58982 = CARTESIAN_POINT('Ctrl Pts',(26.9986751564425,-8.52135717039598,-18.3180160914743)) ;
#58983 = CARTESIAN_POINT('Ctrl Pts',(27.1006975970256,-9.11936849871233,-18.3877640259897)) ;
#58984 = CARTESIAN_POINT('Ctrl Pts',(27.1517851596633,-9.41879950685285,-18.4226820311287)) ;
#58985 = CARTESIAN_POINT('Ctrl Pts',(27.3050572428128,-10.3170925794686,-18.5274222073615)) ;
#58986 = CARTESIAN_POINT('Ctrl Pts',(27.4072510673143,-10.9159546767068,-18.5972306681566)) ;
#58987 = CARTESIAN_POINT('Ctrl Pts',(27.6104950296067,-12.1068736981433,-18.7360283725215)) ;
#58988 = CARTESIAN_POINT('Ctrl Pts',(27.7115452108907,-12.6989306223933,-18.8050175519609)) ;
#58989 = CARTESIAN_POINT('Ctrl Pts',(27.9125385133627,-13.8764819135214,-18.9422120174696)) ;
#58990 = CARTESIAN_POINT('Ctrl Pts',(28.0124536696358,-14.4618113899862,-19.0103978272271)) ;
#58991 = CARTESIAN_POINT('Ctrl Pts',(28.1105818992948,-15.0366437072153,-19.0773535407226)) ;
#58992 = CARTESIAN_POINT('Ctrl Pts',(28.1272162447826,-15.0366437072153,-19.0528197166172)) ;
#58993 = CARTESIAN_POINT('Ctrl Pts',(28.1260439213675,-15.0298036697796,-19.0520298964312)) ;
#58994 = CARTESIAN_POINT('Ctrl Pts',(28.124871342501,-15.0229621460442,-19.0512399056728)) ;
#58995 = CARTESIAN_POINT('Ctrl Pts',(28.0263071912092,-14.4478805128969,-18.9848353170201)) ;
#58996 = CARTESIAN_POINT('Ctrl Pts',(27.9271614144017,-13.869434029792,-18.9180494439821)) ;
#58997 = CARTESIAN_POINT('Ctrl Pts',(27.7265237475049,-12.6989306224415,-18.7829258632544)) ;
#58998 = CARTESIAN_POINT('Ctrl Pts',(27.6250318781892,-12.1068736981987,-18.7145881249272)) ;
#58999 = CARTESIAN_POINT('Ctrl Pts',(27.4208636967858,-10.9159546767766,-18.5771535417749)) ;
#59000 = CARTESIAN_POINT('Ctrl Pts',(27.3181874281729,-10.3170925795457,-18.5080566328121)) ;
#59001 = CARTESIAN_POINT('Ctrl Pts',(27.1641543967029,-9.41879950694078,-18.4044387713905)) ;
#59002 = CARTESIAN_POINT('Ctrl Pts',(27.1128069266329,-9.11936849880387,-18.3699041010365)) ;
#59003 = CARTESIAN_POINT('Ctrl Pts',(27.0102503212534,-8.52135717049476,-18.300944000657)) ;
#59004 = CARTESIAN_POINT('Ctrl Pts',(26.9590411909696,-8.2227768503156,-18.2665185632173)) ;
#59005 = CARTESIAN_POINT('Ctrl Pts',(26.8569054593982,-7.62731755429113,-18.1978775152843)) ;
#59006 = CARTESIAN_POINT('Ctrl Pts',(26.805978868849,-7.33043857844908,-18.1636618889539)) ;
#59007 = CARTESIAN_POINT('Ctrl Pts',(26.7045517821677,-6.73923262837554,-18.0955419776217)) ;
#59008 = CARTESIAN_POINT('Ctrl Pts',(26.6540513076982,-6.4449056541104,-18.0616376606576)) ;
#59009 = CARTESIAN_POINT('Ctrl Pts',(26.5787270255406,-6.00596718811531,-18.0110920299747)) ;
#59010 = CARTESIAN_POINT('Ctrl Pts',(26.5536899925335,-5.86007969985845,-17.9942953098607)) ;
#59011 = CARTESIAN_POINT('Ctrl Pts',(26.5037756790954,-5.56926172242007,-17.9608186704879)) ;
#59012 = CARTESIAN_POINT('Ctrl Pts',(26.4788983993272,-5.42433123323721,-17.9441387502522)) ;
#59013 = CARTESIAN_POINT('Ctrl Pts',(26.4293210373901,-5.13553358586907,-17.9109091382572)) ;
#59014 = CARTESIAN_POINT('Ctrl Pts',(26.4046209588946,-4.9916664276861,-17.894359441081)) ;
#59015 = CARTESIAN_POINT('Ctrl Pts',(26.3554151654589,-4.70510177476713,-17.8614041146133)) ;
#59016 = CARTESIAN_POINT('Ctrl Pts',(26.3309094580062,-4.56240428001608,-17.8449984742729)) ;
#59017 = CARTESIAN_POINT('Ctrl Pts',(26.2821091285874,-4.27828528728337,-17.8123457560937)) ;
#59018 = CARTESIAN_POINT('Ctrl Pts',(26.2578145217622,-4.13686379021172,-17.7960986562588)) ;
#59019 = CARTESIAN_POINT('Ctrl Pts',(26.2094523539447,-3.85540312801667,-17.7637786376448)) ;
#59020 = CARTESIAN_POINT('Ctrl Pts',(26.1853848265438,-3.71536396281382,-17.7477056692929)) ;
#59021 = CARTESIAN_POINT('Ctrl Pts',(26.1494647130129,-3.50642171648299,-17.723740155438)) ;
#59022 = CARTESIAN_POINT('Ctrl Pts',(26.1375215227776,-3.43696038478214,-17.7157756632548)) ;
#59023 = CARTESIAN_POINT('Ctrl Pts',(26.1136970574172,-3.29842318143604,-17.6998973079537)) ;
#59024 = CARTESIAN_POINT('Ctrl Pts',(26.1018157834405,-3.22934730978736,-17.6919834431423)) ;
#59025 = CARTESIAN_POINT('Ctrl Pts',(26.0781163980241,-3.0915943199743,-17.6762093981207)) ;
#59026 = CARTESIAN_POINT('Ctrl Pts',(26.0662982955211,-3.02291720182354,-17.668349204735)) ;
#59027 = CARTESIAN_POINT('Ctrl Pts',(26.0427259888543,-2.88597501397047,-17.652686313256)) ;
#59028 = CARTESIAN_POINT('Ctrl Pts',(26.0309718067178,-2.81770994419542,-17.6448835826481)) ;
#59029 = CARTESIAN_POINT('Ctrl Pts',(26.0085513814615,-2.68755132608213,-17.6300198666284)) ;
#59030 = CARTESIAN_POINT('Ctrl Pts',(25.9973144624006,-2.62233986336839,-17.6225787316105)) ;
#59031 = CARTESIAN_POINT('Ctrl Pts',(25.9800473661399,-2.52219386753023,-17.6111666777666)) ;
#59032 = CARTESIAN_POINT('Ctrl Pts',(25.974223031518,-2.48842373537836,-17.6073209586087)) ;
#59033 = CARTESIAN_POINT('Ctrl Pts',(25.96250282621,-2.42049538204628,-17.5995921129432)) ;
#59034 = CARTESIAN_POINT('Ctrl Pts',(25.9566069655597,-2.38633716082053,-17.5957089716173)) ;
#59035 = CARTESIAN_POINT('Ctrl Pts',(25.9448089810994,-2.31802080948946,-17.5879519599898)) ;
#59036 = CARTESIAN_POINT('Ctrl Pts',(25.9389068845097,-2.28386269304911,-17.5840780545739)) ;
#59037 = CARTESIAN_POINT('Ctrl Pts',(25.9300972726076,-2.23291672727815,-17.5783102288032)) ;
#59038 = CARTESIAN_POINT('Ctrl Pts',(25.9271679806095,-2.21598327357521,-17.5763948073344)) ;
#59039 = CARTESIAN_POINT('Ctrl Pts',(25.9213317316417,-2.18226195696306,-17.572584637016)) ;
#59040 = CARTESIAN_POINT('Ctrl Pts',(25.9184247759445,-2.16547409404589,-17.5706898862874)) ;
#59041 = CARTESIAN_POINT('Ctrl Pts',(25.912640797489,-2.13209248154464,-17.5669277199662)) ;
#59042 = CARTESIAN_POINT('Ctrl Pts',(25.909763785347,-2.11549873579995,-17.5650602901298)) ;
#59043 = CARTESIAN_POINT('Ctrl Pts',(25.9040468317566,-2.08255388387165,-17.5613601081469)) ;
#59044 = CARTESIAN_POINT('Ctrl Pts',(25.9012069173771,-2.06620277748319,-17.5595273160017)) ;
#59045 = CARTESIAN_POINT('Ctrl Pts',(25.896979461996,-2.04189449196258,-17.5568107344993)) ;
#59046 = CARTESIAN_POINT('Ctrl Pts',(25.8955756987359,-2.03382812666439,-17.5559106629946)) ;
#59047 = CARTESIAN_POINT('Ctrl Pts',(25.8927795087419,-2.01777425534598,-17.5541228400657)) ;
#59048 = CARTESIAN_POINT('Ctrl Pts',(25.8913870824749,-2.00978674932117,-17.5532350879521)) ;
#59049 = CARTESIAN_POINT('Ctrl Pts',(25.8886138157077,-1.99389666570093,-17.55147377119)) ;
#59050 = CARTESIAN_POINT('Ctrl Pts',(25.8872329913601,-1.98599408828015,-17.5506001827826)) ;
#59051 = CARTESIAN_POINT('Ctrl Pts',(25.8851701644093,-1.97420847503537,-17.5493025313486)) ;
#59052 = CARTESIAN_POINT('Ctrl Pts',(25.8844839503814,-1.9702913128718,-17.548872112564)) ;
#59053 = CARTESIAN_POINT('Ctrl Pts',(25.8831141358671,-1.96248050053228,-17.5480160786815)) ;
#59054 = CARTESIAN_POINT('Ctrl Pts',(25.8824305363957,-1.95858685034292,-17.5475904620819)) ;
#59055 = CARTESIAN_POINT('Ctrl Pts',(25.8810647713827,-1.95081910920302,-17.5467443167528)) ;
#59056 = CARTESIAN_POINT('Ctrl Pts',(25.8803463295568,-1.94673863589274,-17.5463012905094)) ;
#59057 = CARTESIAN_POINT('Ctrl Pts',(25.8788717871484,-1.93838361094976,-17.5453993105077)) ;
#59058 = CARTESIAN_POINT('Ctrl Pts',(25.8781157274861,-1.93410905863785,-17.5449402961466)) ;
#59059 = CARTESIAN_POINT('Ctrl Pts',(25.8769770714627,-1.92769749310063,-17.5442586065577)) ;
#59060 = CARTESIAN_POINT('Ctrl Pts',(25.8765967513452,-1.92556036167893,-17.5440325305957)) ;
#59061 = CARTESIAN_POINT('Ctrl Pts',(25.8758381991075,-1.92131049884297,-17.5435862844946)) ;
#59062 = CARTESIAN_POINT('Ctrl Pts',(25.8754599870247,-1.91919776697313,-17.5433660846349)) ;
#59063 = CARTESIAN_POINT('Ctrl Pts',(25.8748965291957,-1.91606519318084,-17.543043541432)) ;
#59064 = CARTESIAN_POINT('Ctrl Pts',(25.8747093474316,-1.91502709306561,-17.5429373298579)) ;
#59065 = CARTESIAN_POINT('Ctrl Pts',(25.8743364959667,-1.9129661094791,-17.5427282801657)) ;
#59066 = CARTESIAN_POINT('Ctrl Pts',(25.8741508277133,-1.9119432259641,-17.5426254398969)) ;
#59067 = CARTESIAN_POINT('Ctrl Pts',(25.8737809973961,-1.90991571725549,-17.5424242615868)) ;
#59068 = CARTESIAN_POINT('Ctrl Pts',(25.8735968577151,-1.9089110938889,-17.5423258912064)) ;
#59069 = CARTESIAN_POINT('Ctrl Pts',(25.8733212879543,-1.90742014783921,-17.5421832800649)) ;
#59070 = CARTESIAN_POINT('Ctrl Pts',(25.873229532523,-1.90692583116035,-17.5421365753442)) ;
#59071 = CARTESIAN_POINT('Ctrl Pts',(25.8730459473443,-1.90594291749478,-17.5420453818077)) ;
#59072 = CARTESIAN_POINT('Ctrl Pts',(25.8729541310736,-1.90545431985745,-17.5420008728757)) ;
#59073 = CARTESIAN_POINT('Ctrl Pts',(25.8728145537844,-1.90471906780893,-17.5419359748206)) ;
#59074 = CARTESIAN_POINT('Ctrl Pts',(25.8727645372593,-1.90445692120481,-17.5419132072665)) ;
#59075 = CARTESIAN_POINT('Ctrl Pts',(25.872661292673,-1.90392034649367,-17.5418678861124)) ;
#59076 = CARTESIAN_POINT('Ctrl Pts',(25.8726080673986,-1.90364591820329,-17.5418453283351)) ;
#59077 = CARTESIAN_POINT('Ctrl Pts',(25.8725001468687,-1.90309737461164,-17.5418024960997)) ;
#59078 = CARTESIAN_POINT('Ctrl Pts',(25.8724455122429,-1.90282329814739,-17.5417821465215)) ;
#59079 = CARTESIAN_POINT('Ctrl Pts',(25.8721685331813,-1.90163370002429,-17.5417525863779)) ;
#59080 = CARTESIAN_POINT('Ctrl Pts',(25.8721571980749,-1.90158501684508,-17.541751376657)) ;
#59081 = CARTESIAN_POINT('Ctrl Pts',(25.8721458629685,-1.90153633366587,-17.541750166936)) ;
#59082 = CARTESIAN_POINT('',(17.5021003261044,-15.0366437072153,-29.1174641239524)) ;
#59083 = CARTESIAN_POINT('',(17.5274987345145,-15.0366437072153,-29.1021824086489)) ;
#59084 = CARTESIAN_POINT('Origin',(-0.704216953074884,-21.6462763158693,1.17041768075435)) ;
#59085 = CARTESIAN_POINT('',(16.1153339123929,-1.90153624029605,-26.7838933346086)) ;
#59086 = CARTESIAN_POINT('Ctrl Pts',(16.1153339216337,-1.90153632902166,-26.7838933504477)) ;
#59087 = CARTESIAN_POINT('Ctrl Pts',(16.1153335953233,-1.9015848891725,-26.7839052586496)) ;
#59088 = CARTESIAN_POINT('Ctrl Pts',(16.1153279744952,-1.90242135746351,-26.784110382256)) ;
#59089 = CARTESIAN_POINT('Ctrl Pts',(16.1153496048023,-1.90282255227177,-26.7841941289722)) ;
#59090 = CARTESIAN_POINT('Ctrl Pts',(16.1153669531215,-1.90309646909155,-26.7842497548283)) ;
#59091 = CARTESIAN_POINT('Ctrl Pts',(16.1154038521165,-1.903644693376,-26.7843597756432)) ;
#59092 = CARTESIAN_POINT('Ctrl Pts',(16.1154234811304,-1.90391896201011,-26.7844141141024)) ;
#59093 = CARTESIAN_POINT('Ctrl Pts',(16.1154631181323,-1.90445522464972,-26.7845196025717)) ;
#59094 = CARTESIAN_POINT('Ctrl Pts',(16.1154831305781,-1.90471721884436,-26.7845707499452)) ;
#59095 = CARTESIAN_POINT('Ctrl Pts',(16.115540337139,-1.90545203888158,-26.7847135557674)) ;
#59096 = CARTESIAN_POINT('Ctrl Pts',(16.1155797829326,-1.90594034787055,-26.7848075936928)) ;
#59097 = CARTESIAN_POINT('Ctrl Pts',(16.1156608488187,-1.90692268088041,-26.7849957396781)) ;
#59098 = CARTESIAN_POINT('Ctrl Pts',(16.1157024897167,-1.90741670555177,-26.7850898353766)) ;
#59099 = CARTESIAN_POINT('Ctrl Pts',(16.1158298881831,-1.9089067708687,-26.7853725602131)) ;
#59100 = CARTESIAN_POINT('Ctrl Pts',(16.1159180875171,-1.90991080080438,-26.785561647068)) ;
#59101 = CARTESIAN_POINT('Ctrl Pts',(16.1160988314327,-1.91193711189471,-26.7859416082069)) ;
#59102 = CARTESIAN_POINT('Ctrl Pts',(16.1161914094641,-1.91295939122146,-26.7861324619241)) ;
#59103 = CARTESIAN_POINT('Ctrl Pts',(16.1163798463095,-1.91501915746764,-26.786515863185)) ;
#59104 = CARTESIAN_POINT('Ctrl Pts',(16.1164757072989,-1.91605664442983,-26.7867084094301)) ;
#59105 = CARTESIAN_POINT('Ctrl Pts',(16.1167670878519,-1.91918736800688,-26.7872881678793)) ;
#59106 = CARTESIAN_POINT('Ctrl Pts',(16.1169663635439,-1.92129885205805,-26.7876775210615)) ;
#59107 = CARTESIAN_POINT('Ctrl Pts',(16.1173706348745,-1.92554620490979,-26.7884586670275)) ;
#59108 = CARTESIAN_POINT('Ctrl Pts',(16.1175756613148,-1.92768207416669,-26.7888504413886)) ;
#59109 = CARTESIAN_POINT('Ctrl Pts',(16.1181943210993,-1.93408985320923,-26.7900236514862)) ;
#59110 = CARTESIAN_POINT('Ctrl Pts',(16.1186114723357,-1.93836188118933,-26.7908029990837)) ;
#59111 = CARTESIAN_POINT('Ctrl Pts',(16.1194317942334,-1.94671197220809,-26.7923233251266)) ;
#59112 = CARTESIAN_POINT('Ctrl Pts',(16.1198350276133,-1.95079003592607,-26.7930642659994)) ;
#59113 = CARTESIAN_POINT('Ctrl Pts',(16.1206055169498,-1.95855316926191,-26.794473011271)) ;
#59114 = CARTESIAN_POINT('Ctrl Pts',(16.1209932609039,-1.96244449927012,-26.795178234885)) ;
#59115 = CARTESIAN_POINT('Ctrl Pts',(16.1217733986971,-1.97025065724297,-26.7965915516703)) ;
#59116 = CARTESIAN_POINT('Ctrl Pts',(16.1221657940786,-1.97416548522092,-26.7972996439166)) ;
#59117 = CARTESIAN_POINT('Ctrl Pts',(16.1233491364704,-1.98594407558046,-26.7994284424439)) ;
#59118 = CARTESIAN_POINT('Ctrl Pts',(16.1241461989878,-1.99384194397278,-26.8008536949254)) ;
#59119 = CARTESIAN_POINT('Ctrl Pts',(16.1257538074971,-2.00972255893998,-26.8037165582988)) ;
#59120 = CARTESIAN_POINT('Ctrl Pts',(16.1265643780836,-2.01770530534027,-26.8051541543504)) ;
#59121 = CARTESIAN_POINT('Ctrl Pts',(16.1281972001052,-2.03374961042777,-26.8080413264793)) ;
#59122 = CARTESIAN_POINT('Ctrl Pts',(16.1290194522432,-2.04181116911945,-26.8094909021344)) ;
#59123 = CARTESIAN_POINT('Ctrl Pts',(16.1315016683943,-2.06610496976883,-26.8138566462427)) ;
#59124 = CARTESIAN_POINT('Ctrl Pts',(16.1331770043602,-2.08244633284062,-26.8167898838212)) ;
#59125 = CARTESIAN_POINT('Ctrl Pts',(16.1365601959366,-2.11537155357574,-26.8226952780538)) ;
#59126 = CARTESIAN_POINT('Ctrl Pts',(16.1382680929498,-2.13195541144395,-26.8256674098459)) ;
#59127 = CARTESIAN_POINT('Ctrl Pts',(16.1417095180794,-2.16531713254428,-26.8316430424412)) ;
#59128 = CARTESIAN_POINT('Ctrl Pts',(16.1434430610002,-2.18209499193708,-26.8346465334107)) ;
#59129 = CARTESIAN_POINT('Ctrl Pts',(16.1469295656395,-2.21579621476455,-26.8406769245025)) ;
#59130 = CARTESIAN_POINT('Ctrl Pts',(16.1486825293011,-2.23271957820714,-26.843703823457)) ;
#59131 = CARTESIAN_POINT('Ctrl Pts',(16.1539617626142,-2.2836351864612,-26.852807377152)) ;
#59132 = CARTESIAN_POINT('Ctrl Pts',(16.1575083122125,-2.31777294890895,-26.8589069261871)) ;
#59133 = CARTESIAN_POINT('Ctrl Pts',(16.1646109320275,-2.38604859225412,-26.8711003244594)) ;
#59134 = CARTESIAN_POINT('Ctrl Pts',(16.1681670387747,-2.42018645948669,-26.877194148421)) ;
#59135 = CARTESIAN_POINT('Ctrl Pts',(16.1752457642938,-2.48807433612738,-26.8893084008)) ;
#59136 = CARTESIAN_POINT('Ctrl Pts',(16.1787683984017,-2.52182434558099,-26.8953288200009)) ;
#59137 = CARTESIAN_POINT('Ctrl Pts',(16.1892225990797,-2.62191066721012,-26.9131778237026)) ;
#59138 = CARTESIAN_POINT('Ctrl Pts',(16.1960403645944,-2.68708327229862,-26.9247942140295)) ;
#59139 = CARTESIAN_POINT('Ctrl Pts',(16.2096598584406,-2.81716036725213,-26.9479719791873)) ;
#59140 = CARTESIAN_POINT('Ctrl Pts',(16.2168100717623,-2.88538078201676,-26.9601234212194)) ;
#59141 = CARTESIAN_POINT('Ctrl Pts',(16.2311643500484,-3.02223339031803,-26.9844932177342)) ;
#59142 = CARTESIAN_POINT('Ctrl Pts',(16.238368448649,-3.09086558392735,-26.9967115519961)) ;
#59143 = CARTESIAN_POINT('Ctrl Pts',(16.2528267741834,-3.2285284638215,-27.0212141688352)) ;
#59144 = CARTESIAN_POINT('Ctrl Pts',(16.2600810147522,-3.2975591500927,-27.0334984432048)) ;
#59145 = CARTESIAN_POINT('Ctrl Pts',(16.2746366660444,-3.43600573054254,-27.0581315160813)) ;
#59146 = CARTESIAN_POINT('Ctrl Pts',(16.2819380785228,-3.50542162472458,-27.0704803135319)) ;
#59147 = CARTESIAN_POINT('Ctrl Pts',(16.3039093040814,-3.71422719332898,-27.1076209529245)) ;
#59148 = CARTESIAN_POINT('Ctrl Pts',(16.3186460115184,-3.85417475315424,-27.1325070981648)) ;
#59149 = CARTESIAN_POINT('Ctrl Pts',(16.3482808560405,-4.13545130036397,-27.1825154360538)) ;
#59150 = CARTESIAN_POINT('Ctrl Pts',(16.3631790444222,-4.27678028782789,-27.2076375978574)) ;
#59151 = CARTESIAN_POINT('Ctrl Pts',(16.3931221850076,-4.56071342667109,-27.2581011640566)) ;
#59152 = CARTESIAN_POINT('Ctrl Pts',(16.408167159986,-4.70331757714046,-27.2834425545297)) ;
#59153 = CARTESIAN_POINT('Ctrl Pts',(16.4383903366365,-4.98969477637851,-27.3343270936616)) ;
#59154 = CARTESIAN_POINT('Ctrl Pts',(16.4535685497435,-5.13346782516221,-27.3598702354439)) ;
#59155 = CARTESIAN_POINT('Ctrl Pts',(16.4840453325162,-5.4220765581703,-27.411140392136)) ;
#59156 = CARTESIAN_POINT('Ctrl Pts',(16.4993439077866,-5.56691224239239,-27.4368674036729)) ;
#59157 = CARTESIAN_POINT('Ctrl Pts',(16.5300489684253,-5.85753998390375,-27.4884871600178)) ;
#59158 = CARTESIAN_POINT('Ctrl Pts',(16.5454554548018,-6.00333204119435,-27.5143799042186)) ;
#59159 = CARTESIAN_POINT('Ctrl Pts',(16.591818523408,-6.4419833796166,-27.5922792779561)) ;
#59160 = CARTESIAN_POINT('Ctrl Pts',(16.6229186490035,-6.73611782260147,-27.6445070872715)) ;
#59161 = CARTESIAN_POINT('Ctrl Pts',(16.6854064677895,-7.32693704076666,-27.7494047781817)) ;
#59162 = CARTESIAN_POINT('Ctrl Pts',(16.7167941940568,-7.62362181598063,-27.802074639883)) ;
#59163 = CARTESIAN_POINT('Ctrl Pts',(16.779763714813,-8.21869159784999,-27.9077076626911)) ;
#59164 = CARTESIAN_POINT('Ctrl Pts',(16.8113455256892,-8.51707660450211,-27.9606708139371)) ;
#59165 = CARTESIAN_POINT('Ctrl Pts',(16.8746106604458,-9.11469674930695,-28.0667410750769)) ;
#59166 = CARTESIAN_POINT('Ctrl Pts',(16.9062939919982,-9.41393188746664,-28.1198481803558)) ;
#59167 = CARTESIAN_POINT('Ctrl Pts',(17.001358320318,-10.3116373501377,-28.2791608835402)) ;
#59168 = CARTESIAN_POINT('Ctrl Pts',(17.0647535138763,-10.9101077074106,-28.3853579474179)) ;
#59169 = CARTESIAN_POINT('Ctrl Pts',(17.1908503647206,-12.1002477005039,-28.5965291458614)) ;
#59170 = CARTESIAN_POINT('Ctrl Pts',(17.2535520883831,-12.6919173363758,-28.7015032405009)) ;
#59171 = CARTESIAN_POINT('Ctrl Pts',(17.3785914021686,-13.871632628226,-28.9107964804685)) ;
#59172 = CARTESIAN_POINT('Ctrl Pts',(17.4409045653392,-14.4594442698531,-29.0150738827972)) ;
#59173 = CARTESIAN_POINT('Ctrl Pts',(17.5021003260697,-15.0366437072153,-29.1174641239733)) ;
#59174 = CARTESIAN_POINT('Ctrl Pts',(17.5274987345495,-15.0366437072153,-29.1021824086278)) ;
#59175 = CARTESIAN_POINT('Ctrl Pts',(17.526462169319,-15.0269621479894,-29.1004710648072)) ;
#59176 = CARTESIAN_POINT('Ctrl Pts',(17.5254252822432,-15.0172776030755,-29.0987591945383)) ;
#59177 = CARTESIAN_POINT('Ctrl Pts',(17.4635886137329,-14.4397231681225,-28.9966689555074)) ;
#59178 = CARTESIAN_POINT('Ctrl Pts',(17.4016894411209,-13.8616550702235,-28.8944924373392)) ;
#59179 = CARTESIAN_POINT('Ctrl Pts',(17.2764143764457,-12.6919173364626,-28.687747458202)) ;
#59180 = CARTESIAN_POINT('Ctrl Pts',(17.2130385160889,-12.1002477006036,-28.5831789781565)) ;
#59181 = CARTESIAN_POINT('Ctrl Pts',(17.0855310481079,-10.9101077075362,-28.3728565198898)) ;
#59182 = CARTESIAN_POINT('Ctrl Pts',(17.0213995068512,-10.3116373502763,-28.2671025017254)) ;
#59183 = CARTESIAN_POINT('Ctrl Pts',(16.9251737485511,-9.41393188762483,-28.1084886077789)) ;
#59184 = CARTESIAN_POINT('Ctrl Pts',(16.89309372132,-9.11469674947166,-28.0556201863721)) ;
#59185 = CARTESIAN_POINT('Ctrl Pts',(16.8290132911686,-8.51707660467983,-27.9500404721984)) ;
#59186 = CARTESIAN_POINT('Ctrl Pts',(16.7970128959182,-8.21869159803422,-27.8973291748155)) ;
#59187 = CARTESIAN_POINT('Ctrl Pts',(16.7331803030063,-7.62362181617781,-27.7922154452969)) ;
#59188 = CARTESIAN_POINT('Ctrl Pts',(16.7013481217343,-7.32693704097029,-27.7398130033007)) ;
#59189 = CARTESIAN_POINT('Ctrl Pts',(16.6379395701423,-6.73611782281798,-27.6354692989421)) ;
#59190 = CARTESIAN_POINT('Ctrl Pts',(16.6063632328931,-6.44198337983951,-27.5835280166735)) ;
#59191 = CARTESIAN_POINT('Ctrl Pts',(16.5592550506141,-6.00333204142681,-27.5060769629603)) ;
#59192 = CARTESIAN_POINT('Ctrl Pts',(16.5435950275102,-5.85753998413939,-27.4803367667477)) ;
#59193 = CARTESIAN_POINT('Ctrl Pts',(16.5123708606242,-5.56691224263436,-27.4290293462702)) ;
#59194 = CARTESIAN_POINT('Ctrl Pts',(16.4968067178516,-5.42207655841544,-27.4034621213986)) ;
#59195 = CARTESIAN_POINT('Ctrl Pts',(16.4657844991903,-5.13346782541362,-27.3525201425934)) ;
#59196 = CARTESIAN_POINT('Ctrl Pts',(16.4503264289016,-4.98969477663306,-27.3271453852913)) ;
#59197 = CARTESIAN_POINT('Ctrl Pts',(16.4195261167511,-4.70331757740126,-27.2766080970697)) ;
#59198 = CARTESIAN_POINT('Ctrl Pts',(16.4041838863201,-4.56071342693497,-27.2514455592689)) ;
#59199 = CARTESIAN_POINT('Ctrl Pts',(16.3736243375693,-4.27678028809796,-27.2013528735587)) ;
#59200 = CARTESIAN_POINT('Ctrl Pts',(16.3584070422223,-4.13545130063712,-27.1764227120465)) ;
#59201 = CARTESIAN_POINT('Ctrl Pts',(16.3281052846885,-3.85417475343352,-27.1268156424043)) ;
#59202 = CARTESIAN_POINT('Ctrl Pts',(16.3130208737795,-3.7142271936113,-27.1021387034025)) ;
#59203 = CARTESIAN_POINT('Ctrl Pts',(16.2904981790424,-3.50542162501146,-27.0653298720066)) ;
#59204 = CARTESIAN_POINT('Ctrl Pts',(16.2830079109946,-3.4360057308309,-27.0530947051822)) ;
#59205 = CARTESIAN_POINT('Ctrl Pts',(16.2680622843419,-3.2975591503841,-27.0286962726957)) ;
#59206 = CARTESIAN_POINT('Ctrl Pts',(16.2606069274919,-3.22852846411439,-27.0165330059779)) ;
#59207 = CARTESIAN_POINT('Ctrl Pts',(16.2457309721133,-3.09086558422325,-26.9922816686795)) ;
#59208 = CARTESIAN_POINT('Ctrl Pts',(16.2383103872221,-3.02223339061542,-26.9801935898972)) ;
#59209 = CARTESIAN_POINT('Ctrl Pts',(16.2235030435901,-2.88538078231715,-26.9560963937571)) ;
#59210 = CARTESIAN_POINT('Ctrl Pts',(16.2161163184728,-2.81716036755398,-26.9440872561512)) ;
#59211 = CARTESIAN_POINT('Ctrl Pts',(16.2020179696739,-2.68708327265388,-26.9211976084717)) ;
#59212 = CARTESIAN_POINT('Ctrl Pts',(16.194948247823,-2.6219106676199,-26.9097328152556)) ;
#59213 = CARTESIAN_POINT('Ctrl Pts',(16.1840752739186,-2.52182434607447,-26.8921357790644)) ;
#59214 = CARTESIAN_POINT('Ctrl Pts',(16.180406192602,-2.48807433664905,-26.8862034742322)) ;
#59215 = CARTESIAN_POINT('Ctrl Pts',(16.1730188395042,-2.42018646006518,-26.8742749169197)) ;
#59216 = CARTESIAN_POINT('Ctrl Pts',(16.1693005830549,-2.38604859286116,-26.8682786552036)) ;
#59217 = CARTESIAN_POINT('Ctrl Pts',(16.1618544958971,-2.3177729495731,-26.8562919143886)) ;
#59218 = CARTESIAN_POINT('Ctrl Pts',(16.1581267046257,-2.28363518715392,-26.8503014148569)) ;
#59219 = CARTESIAN_POINT('Ctrl Pts',(16.1525564427381,-2.23271957894245,-26.8413729672555)) ;
#59220 = CARTESIAN_POINT('Ctrl Pts',(16.1507032440341,-2.215796215514,-26.8384063777284)) ;
#59221 = CARTESIAN_POINT('Ctrl Pts',(16.1470084290761,-2.18209499271471,-26.8325013228036)) ;
#59222 = CARTESIAN_POINT('Ctrl Pts',(16.1451668147577,-2.165317133336,-26.82956285624)) ;
#59223 = CARTESIAN_POINT('Ctrl Pts',(16.1414992639685,-2.13195541226357,-26.8237232789466)) ;
#59224 = CARTESIAN_POINT('Ctrl Pts',(16.1396733431141,-2.1153715544092,-26.8208221597469)) ;
#59225 = CARTESIAN_POINT('Ctrl Pts',(16.136040571677,-2.0824463337016,-26.8150669327407)) ;
#59226 = CARTESIAN_POINT('Ctrl Pts',(16.1342337624648,-2.06610497064345,-26.8122127999931)) ;
#59227 = CARTESIAN_POINT('Ctrl Pts',(16.1315392659603,-2.04181117001441,-26.8079747807405)) ;
#59228 = CARTESIAN_POINT('Ctrl Pts',(16.130643698243,-2.03374961132952,-26.8065693176076)) ;
#59229 = CARTESIAN_POINT('Ctrl Pts',(16.1288576745114,-2.01770530625544,-26.8037743238924)) ;
#59230 = CARTESIAN_POINT('Ctrl Pts',(16.1279672191938,-2.00972255986181,-26.8023847928903)) ;
#59231 = CARTESIAN_POINT('Ctrl Pts',(16.1261908623183,-1.99384194490789,-26.7996234620433)) ;
#59232 = CARTESIAN_POINT('Ctrl Pts',(16.1253049854103,-1.98594407652206,-26.7982516474091)) ;
#59233 = CARTESIAN_POINT('Ctrl Pts',(16.1239784538382,-1.97416548617237,-26.7962090029555)) ;
#59234 = CARTESIAN_POINT('Ctrl Pts',(16.1235366471204,-1.97025065819767,-26.7955306405245)) ;
#59235 = CARTESIAN_POINT('Ctrl Pts',(16.1226533878464,-1.96244450023135,-26.7941793698772)) ;
#59236 = CARTESIAN_POINT('Ctrl Pts',(16.122211936814,-1.95855317022654,-26.7935064607409)) ;
#59237 = CARTESIAN_POINT('Ctrl Pts',(16.1213281970955,-1.9507900367832,-26.7921658559373)) ;
#59238 = CARTESIAN_POINT('Ctrl Pts',(16.1208624448328,-1.94671197294882,-26.7914625314001)) ;
#59239 = CARTESIAN_POINT('Ctrl Pts',(16.1199034641384,-1.93836188169201,-26.7900256335297)) ;
#59240 = CARTESIAN_POINT('Ctrl Pts',(16.1194102982851,-1.93408985359028,-26.7892920223804)) ;
#59241 = CARTESIAN_POINT('Ctrl Pts',(16.1186635384765,-1.9276820743651,-26.7881958874659)) ;
#59242 = CARTESIAN_POINT('Ctrl Pts',(16.1184134372312,-1.92554620504717,-26.7878312337004)) ;
#59243 = CARTESIAN_POINT('Ctrl Pts',(16.1179126494524,-1.92129885207443,-26.7871081597253)) ;
#59244 = CARTESIAN_POINT('Ctrl Pts',(16.1176619935634,-1.91918736796419,-26.7867497209677)) ;
#59245 = CARTESIAN_POINT('Ctrl Pts',(16.1172862550928,-1.91605664429787,-26.7862207189719)) ;
#59246 = CARTESIAN_POINT('Ctrl Pts',(16.1171610403001,-1.91501915730528,-26.7860458343169)) ;
#59247 = CARTESIAN_POINT('Ctrl Pts',(16.1169105660688,-1.91295939100032,-26.7856997596984)) ;
#59248 = CARTESIAN_POINT('Ctrl Pts',(16.1167853088843,-1.91193711164353,-26.7855285683681)) ;
#59249 = CARTESIAN_POINT('Ctrl Pts',(16.1165342706096,-1.90991080049551,-26.7851909019278)) ;
#59250 = CARTESIAN_POINT('Ctrl Pts',(16.1164085234018,-1.90890677053132,-26.7850244068722)) ;
#59251 = CARTESIAN_POINT('Ctrl Pts',(16.116218407116,-1.90741670517188,-26.7847794180852)) ;
#59252 = CARTESIAN_POINT('Ctrl Pts',(16.1161547773415,-1.9069226804876,-26.7846985526516)) ;
#59253 = CARTESIAN_POINT('Ctrl Pts',(16.1160265200478,-1.90594034744944,-26.7845388007874)) ;
#59254 = CARTESIAN_POINT('Ctrl Pts',(16.1159619131579,-1.90545203844624,-26.7844599017879)) ;
#59255 = CARTESIAN_POINT('Ctrl Pts',(16.1158625385309,-1.90471721841522,-26.7843424676508)) ;
#59256 = CARTESIAN_POINT('Ctrl Pts',(16.1158267232252,-1.90445522424116,-26.7843008285476)) ;
#59257 = CARTESIAN_POINT('Ctrl Pts',(16.1157520891995,-1.90391896164507,-26.7842163970993)) ;
#59258 = CARTESIAN_POINT('Ctrl Pts',(16.1157132748072,-1.90364469303768,-26.7841736021057)) ;
#59259 = CARTESIAN_POINT('Ctrl Pts',(16.1156333538959,-1.9030964687972,-26.7840894667296)) ;
#59260 = CARTESIAN_POINT('Ctrl Pts',(16.1155923338751,-1.90282255200049,-26.7840480836694)) ;
#59261 = CARTESIAN_POINT('Ctrl Pts',(16.1153534832311,-1.90163369505953,-26.7839050636273)) ;
#59262 = CARTESIAN_POINT('Ctrl Pts',(16.1153437024324,-1.9015850120406,-26.7838992070375)) ;
#59263 = CARTESIAN_POINT('Ctrl Pts',(16.1153339216337,-1.90153632902166,-26.7838933504477)) ;
#59264 = CARTESIAN_POINT('',(3.65837019749608,-15.0366437072151,-33.7752359034359)) ;
#59265 = CARTESIAN_POINT('',(3.68783779512015,-15.0366437072151,-33.7720311090636)) ;
#59266 = CARTESIAN_POINT('Origin',(-0.147684368304155,-21.6462763158694,1.35793534153108)) ;
#59267 = CARTESIAN_POINT('',(3.37961603007408,-1.90153624332578,-31.075056312033)) ;
#59268 = CARTESIAN_POINT('Ctrl Pts',(3.37961603187484,-1.90153633508113,-31.0750563309111)) ;
#59269 = CARTESIAN_POINT('Ctrl Pts',(3.37961070599222,-1.90158489145841,-31.0750670039238)) ;
#59270 = CARTESIAN_POINT('Ctrl Pts',(3.37951986530706,-1.90241309119405,-31.0752490477001)) ;
#59271 = CARTESIAN_POINT('Ctrl Pts',(3.37950436522705,-1.90281047539216,-31.0753333407487)) ;
#59272 = CARTESIAN_POINT('Ctrl Pts',(3.37949676124729,-1.9030817925977,-31.0753905685281)) ;
#59273 = CARTESIAN_POINT('Ctrl Pts',(3.37948405658615,-1.90362481732619,-31.0755048329751)) ;
#59274 = CARTESIAN_POINT('Ctrl Pts',(3.37947905017671,-1.90389648606574,-31.0755618513277)) ;
#59275 = CARTESIAN_POINT('Ctrl Pts',(3.37947071353972,-1.90442766694489,-31.0756731786513)) ;
#59276 = CARTESIAN_POINT('Ctrl Pts',(3.37946738820882,-1.9046871792651,-31.0757274871272)) ;
#59277 = CARTESIAN_POINT('Ctrl Pts',(3.37945930658739,-1.90541496833161,-31.075879657174)) ;
#59278 = CARTESIAN_POINT('Ctrl Pts',(3.37945558758785,-1.90589858091376,-31.0759805939111)) ;
#59279 = CARTESIAN_POINT('Ctrl Pts',(3.37945008307113,-1.90687146640829,-31.0761834337627)) ;
#59280 = CARTESIAN_POINT('Ctrl Pts',(3.37944832151258,-1.90736073997115,-31.0762853344068)) ;
#59281 = CARTESIAN_POINT('Ctrl Pts',(3.37944508902581,-1.90883647538957,-31.0765924584461)) ;
#59282 = CARTESIAN_POINT('Ctrl Pts',(3.37944563120107,-1.90983084996186,-31.0767991077804)) ;
#59283 = CARTESIAN_POINT('Ctrl Pts',(3.37944989084143,-1.91183767529128,-31.0772158187512)) ;
#59284 = CARTESIAN_POINT('Ctrl Pts',(3.37945364719749,-1.91285012422377,-31.0774258757787)) ;
#59285 = CARTESIAN_POINT('Ctrl Pts',(3.37946341359751,-1.91489008382497,-31.0778488757296)) ;
#59286 = CARTESIAN_POINT('Ctrl Pts',(3.3794694261378,-1.91591759453621,-31.0780618183902)) ;
#59287 = CARTESIAN_POINT('Ctrl Pts',(3.37949000589426,-1.9190182143266,-31.0787041299186)) ;
#59288 = CARTESIAN_POINT('Ctrl Pts',(3.37950706889375,-1.92110939581349,-31.0791369842042)) ;
#59289 = CARTESIAN_POINT('Ctrl Pts',(3.37954533910382,-1.92531591015439,-31.0800072625959)) ;
#59290 = CARTESIAN_POINT('Ctrl Pts',(3.37956658180458,-1.92743124346434,-31.080444682937)) ;
#59291 = CARTESIAN_POINT('Ctrl Pts',(3.37963442654588,-1.93377741462869,-31.0817565318447)) ;
#59292 = CARTESIAN_POINT('Ctrl Pts',(3.37968507843149,-1.93800837065686,-31.0826305445298)) ;
#59293 = CARTESIAN_POINT('Ctrl Pts',(3.37978980881172,-1.94627818463165,-31.0843382643264)) ;
#59294 = CARTESIAN_POINT('Ctrl Pts',(3.37984395962429,-1.95031704325728,-31.0851719637139)) ;
#59295 = CARTESIAN_POINT('Ctrl Pts',(3.3799503650075,-1.95800520795894,-31.0867585894296)) ;
#59296 = CARTESIAN_POINT('Ctrl Pts',(3.3800054657301,-1.96185878993651,-31.0875536706246)) ;
#59297 = CARTESIAN_POINT('Ctrl Pts',(3.38011866494425,-1.96958922400625,-31.0891483443258)) ;
#59298 = CARTESIAN_POINT('Ctrl Pts',(3.3801767652232,-1.97346607611177,-31.0899479366401)) ;
#59299 = CARTESIAN_POINT('Ctrl Pts',(3.38035473269316,-1.98513040811581,-31.092353336025)) ;
#59300 = CARTESIAN_POINT('Ctrl Pts',(3.38047821962445,-1.99295166328761,-31.0939657705512)) ;
#59301 = CARTESIAN_POINT('Ctrl Pts',(3.38073219781414,-2.00867822864612,-31.0972073510004)) ;
#59302 = CARTESIAN_POINT('Ctrl Pts',(3.38086271750251,-2.01658353865841,-31.0988364937951)) ;
#59303 = CARTESIAN_POINT('Ctrl Pts',(3.38112929199853,-2.03247220660011,-31.1021104018258)) ;
#59304 = CARTESIAN_POINT('Ctrl Pts',(3.38126534761985,-2.04045556453403,-31.1037551669739)) ;
#59305 = CARTESIAN_POINT('Ctrl Pts',(3.3816803546736,-2.0645137045524,-31.10871118306)) ;
#59306 = CARTESIAN_POINT('Ctrl Pts',(3.38196604522678,-2.08069654939365,-31.1120441649112)) ;
#59307 = CARTESIAN_POINT('Ctrl Pts',(3.38255050826333,-2.11330238176182,-31.1187586261777)) ;
#59308 = CARTESIAN_POINT('Ctrl Pts',(3.38284932852915,-2.12972536949358,-31.1221401004387)) ;
#59309 = CARTESIAN_POINT('Ctrl Pts',(3.38345698968157,-2.16276346879482,-31.128941897414)) ;
#59310 = CARTESIAN_POINT('Ctrl Pts',(3.38376584804614,-2.17937857652572,-31.1323622174295)) ;
#59311 = CARTESIAN_POINT('Ctrl Pts',(3.38439130595124,-2.21275288488517,-31.1392319692574)) ;
#59312 = CARTESIAN_POINT('Ctrl Pts',(3.3847079077424,-2.22951208552169,-31.1426814008264)) ;
#59313 = CARTESIAN_POINT('Ctrl Pts',(3.38566651923717,-2.27993379421205,-31.1530586943963)) ;
#59314 = CARTESIAN_POINT('Ctrl Pts',(3.38631726306848,-2.31374040875672,-31.1600155630294)) ;
#59315 = CARTESIAN_POINT('Ctrl Pts',(3.38762973138084,-2.38135375628433,-31.1739281306989)) ;
#59316 = CARTESIAN_POINT('Ctrl Pts',(3.38829149941384,-2.41516047560426,-31.1808838221583)) ;
#59317 = CARTESIAN_POINT('Ctrl Pts',(3.38961550071907,-2.48238981945739,-31.1947153097383)) ;
#59318 = CARTESIAN_POINT('Ctrl Pts',(3.39027775169458,-2.51581244403611,-31.201591103943)) ;
#59319 = CARTESIAN_POINT('Ctrl Pts',(3.39225062944442,-2.61492790016553,-31.2219804336516)) ;
#59320 = CARTESIAN_POINT('Ctrl Pts',(3.39354726626446,-2.67946831375413,-31.2352559286588)) ;
#59321 = CARTESIAN_POINT('Ctrl Pts',(3.39614778446036,-2.80821979180197,-31.2617376664407)) ;
#59322 = CARTESIAN_POINT('Ctrl Pts',(3.3975194687046,-2.87571441576423,-31.2756191140077)) ;
#59323 = CARTESIAN_POINT('Ctrl Pts',(3.40028344398628,-3.01111106169542,-31.3034644569785)) ;
#59324 = CARTESIAN_POINT('Ctrl Pts',(3.4016757737032,-3.07901308373674,-31.3174283481908)) ;
#59325 = CARTESIAN_POINT('Ctrl Pts',(3.40447808763379,-3.21521138105106,-31.3454361670284)) ;
#59326 = CARTESIAN_POINT('Ctrl Pts',(3.40588808753438,-3.2835076563105,-31.3594800929445)) ;
#59327 = CARTESIAN_POINT('Ctrl Pts',(3.40872367041719,-3.4204813166111,-31.3876454742405)) ;
#59328 = CARTESIAN_POINT('Ctrl Pts',(3.41014925541447,-3.4891587016557,-31.4017669294009)) ;
#59329 = CARTESIAN_POINT('Ctrl Pts',(3.41444704959774,-3.69574280763306,-31.4442437450053)) ;
#59330 = CARTESIAN_POINT('Ctrl Pts',(3.41734019001168,-3.83420147875592,-31.4727115671767)) ;
#59331 = CARTESIAN_POINT('Ctrl Pts',(3.42317344443391,-4.11248555184698,-31.5299262156988)) ;
#59332 = CARTESIAN_POINT('Ctrl Pts',(3.42611361752539,-4.25231095389446,-31.55867303564)) ;
#59333 = CARTESIAN_POINT('Ctrl Pts',(3.43203473233886,-4.53322335570595,-31.6164244996989)) ;
#59334 = CARTESIAN_POINT('Ctrl Pts',(3.4350157003956,-4.67431035456218,-31.6454291407638)) ;
#59335 = CARTESIAN_POINT('Ctrl Pts',(3.44101350143713,-4.95764081489597,-31.7036749251378)) ;
#59336 = CARTESIAN_POINT('Ctrl Pts',(3.44403034759642,-5.09988427638858,-31.7329160670173)) ;
#59337 = CARTESIAN_POINT('Ctrl Pts',(3.45009576986787,-5.38542252965196,-31.7916134480566)) ;
#59338 = CARTESIAN_POINT('Ctrl Pts',(3.45314435244133,-5.52871732142045,-31.8210696865129)) ;
#59339 = CARTESIAN_POINT('Ctrl Pts',(3.45926960099568,-5.81625310337682,-31.8801758027233)) ;
#59340 = CARTESIAN_POINT('Ctrl Pts',(3.46234626814327,-5.96049409356606,-31.90982568035)) ;
#59341 = CARTESIAN_POINT('Ctrl Pts',(3.47161340231309,-6.39447866448406,-31.9990335333828)) ;
#59342 = CARTESIAN_POINT('Ctrl Pts',(3.47784092628434,-6.68548384087354,-32.0588497362073)) ;
#59343 = CARTESIAN_POINT('Ctrl Pts',(3.49037064512373,-7.27001739345534,-32.1789985378797)) ;
#59344 = CARTESIAN_POINT('Ctrl Pts',(3.49667287813247,-7.56354576968126,-32.2393311325864)) ;
#59345 = CARTESIAN_POINT('Ctrl Pts',(3.50932984594644,-8.15228466530568,-32.3603402921398)) ;
#59346 = CARTESIAN_POINT('Ctrl Pts',(3.5156845996516,-8.44749518470088,-32.4210168549303)) ;
#59347 = CARTESIAN_POINT('Ctrl Pts',(3.52842552872783,-9.03875731084587,-32.5425414065042)) ;
#59348 = CARTESIAN_POINT('Ctrl Pts',(3.53481171294786,-9.33480891760259,-32.6033893943262)) ;
#59349 = CARTESIAN_POINT('Ctrl Pts',(3.55398681249754,-10.222963786029,-32.785931568223)) ;
#59350 = CARTESIAN_POINT('Ctrl Pts',(3.56679211841551,-10.8150670804398,-32.9076239785171)) ;
#59351 = CARTESIAN_POINT('Ctrl Pts',(3.59228823476391,-11.9925453007398,-33.1496225734659)) ;
#59352 = CARTESIAN_POINT('Ctrl Pts',(3.60497912176864,-12.5779202266805,-33.2699287498025)) ;
#59353 = CARTESIAN_POINT('Ctrl Pts',(3.63009196367396,-13.7352132465282,-33.5077729753066)) ;
#59354 = CARTESIAN_POINT('Ctrl Pts',(3.64251395514895,-14.3071313404322,-33.6253110204958)) ;
#59355 = CARTESIAN_POINT('Ctrl Pts',(3.65594235487389,-14.9249537984812,-33.7522821058483)) ;
#59356 = CARTESIAN_POINT('Ctrl Pts',(3.65715735966845,-14.9808505488474,-33.7637696540393)) ;
#59357 = CARTESIAN_POINT('Ctrl Pts',(3.65837019675597,-15.0366437072147,-33.775235903516)) ;
#59358 = CARTESIAN_POINT('Ctrl Pts',(3.68783779586043,-15.0366437072147,-33.7720311089827)) ;
#59359 = CARTESIAN_POINT('Ctrl Pts',(3.68655737279354,-14.9808505488608,-33.7605722099269)) ;
#59360 = CARTESIAN_POINT('Ctrl Pts',(3.6852744881599,-14.924953798508,-33.7490920441161)) ;
#59361 = CARTESIAN_POINT('Ctrl Pts',(3.67109390924987,-14.3071313404863,-33.6222027631854)) ;
#59362 = CARTESIAN_POINT('Ctrl Pts',(3.65795827615197,-13.7352132465962,-33.5047423312028)) ;
#59363 = CARTESIAN_POINT('Ctrl Pts',(3.63135451591116,-12.5779202267768,-33.2670602528451)) ;
#59364 = CARTESIAN_POINT('Ctrl Pts',(3.61788642534454,-11.9925453008504,-33.1468386024926)) ;
#59365 = CARTESIAN_POINT('Ctrl Pts',(3.59076391217546,-10.8150670805791,-32.9050168888634)) ;
#59366 = CARTESIAN_POINT('Ctrl Pts',(3.57710956614513,-10.2229637861827,-32.7834168172492)) ;
#59367 = CARTESIAN_POINT('Ctrl Pts',(3.55659519104407,-9.33480891777804,-32.6010202983507)) ;
#59368 = CARTESIAN_POINT('Ctrl Pts',(3.54975155110104,-9.03875731102854,-32.5402220618383)) ;
#59369 = CARTESIAN_POINT('Ctrl Pts',(3.53607041798801,-8.44749518489797,-32.4187997636185)) ;
#59370 = CARTESIAN_POINT('Ctrl Pts',(3.52923293366762,-8.15228466551,-32.3581757009477)) ;
#59371 = CARTESIAN_POINT('Ctrl Pts',(3.51558059630923,-7.56354576989996,-32.2372747943589)) ;
#59372 = CARTESIAN_POINT('Ctrl Pts',(3.50876576216914,-7.2700173936812,-32.1769979483863)) ;
#59373 = CARTESIAN_POINT('Ctrl Pts',(3.49517410235908,-6.68548384111368,-32.0569646397574)) ;
#59374 = CARTESIAN_POINT('Ctrl Pts',(3.48839731482568,-6.39447866473132,-31.9972081729466)) ;
#59375 = CARTESIAN_POINT('Ctrl Pts',(3.47827073711185,-5.96049409382388,-31.9080937900342)) ;
#59376 = CARTESIAN_POINT('Ctrl Pts',(3.47490162625046,-5.81625310363817,-31.8784757175788)) ;
#59377 = CARTESIAN_POINT('Ctrl Pts',(3.46817760207663,-5.52871732168881,-31.8194347221429)) ;
#59378 = CARTESIAN_POINT('Ctrl Pts',(3.46482268993128,-5.38542252992385,-31.7900117990359)) ;
#59379 = CARTESIAN_POINT('Ctrl Pts',(3.45812810415939,-5.09988427666742,-31.7313828436523)) ;
#59380 = CARTESIAN_POINT('Ctrl Pts',(3.45478843699215,-4.95764081517829,-31.7021768106739)) ;
#59381 = CARTESIAN_POINT('Ctrl Pts',(3.44812489087114,-4.6743103548514,-31.644003430442)) ;
#59382 = CARTESIAN_POINT('Ctrl Pts',(3.44480102509296,-4.53322335599863,-31.6150360817525)) ;
#59383 = CARTESIAN_POINT('Ctrl Pts',(3.4381688498808,-4.25231095419401,-31.5573619501736)) ;
#59384 = CARTESIAN_POINT('Ctrl Pts',(3.4348605668216,-4.11248555214992,-31.5286551646046)) ;
#59385 = CARTESIAN_POINT('Ctrl Pts',(3.42825798481763,-3.83420147906566,-31.4715241855007)) ;
#59386 = CARTESIAN_POINT('Ctrl Pts',(3.42496374495564,-3.69574280794619,-31.4430999855238)) ;
#59387 = CARTESIAN_POINT('Ctrl Pts',(3.42002979935007,-3.48915870197386,-31.4006923555569)) ;
#59388 = CARTESIAN_POINT('Ctrl Pts',(3.41838635952705,-3.42048131693095,-31.386594593537)) ;
#59389 = CARTESIAN_POINT('Ctrl Pts',(3.41510092364216,-3.28350765663369,-31.358478136704)) ;
#59390 = CARTESIAN_POINT('Ctrl Pts',(3.41345892959589,-3.21521138137592,-31.3444594416721)) ;
#59391 = CARTESIAN_POINT('Ctrl Pts',(3.41017487383933,-3.07901308406493,-31.3165040154161)) ;
#59392 = CARTESIAN_POINT('Ctrl Pts',(3.40853282782131,-3.01111106202524,-31.3025672824885)) ;
#59393 = CARTESIAN_POINT('Ctrl Pts',(3.40524625726093,-2.87571441609737,-31.27477877518)) ;
#59394 = CARTESIAN_POINT('Ctrl Pts',(3.40360177139038,-2.80821979213676,-31.2609269965782)) ;
#59395 = CARTESIAN_POINT('Ctrl Pts',(3.40044870008814,-2.67946831411711,-31.234505352574)) ;
#59396 = CARTESIAN_POINT('Ctrl Pts',(3.39886118325269,-2.61492790055638,-31.2212614926806)) ;
#59397 = CARTESIAN_POINT('Ctrl Pts',(3.39640483303503,-2.51581244446976,-31.2009247437805)) ;
#59398 = CARTESIAN_POINT('Ctrl Pts',(3.39557350845141,-2.48238981990544,-31.1940673374417)) ;
#59399 = CARTESIAN_POINT('Ctrl Pts',(3.39389319436904,-2.41516047608134,-31.1802746012175)) ;
#59400 = CARTESIAN_POINT('Ctrl Pts',(3.39304422256571,-2.38135375677605,-31.1733392693982)) ;
#59401 = CARTESIAN_POINT('Ctrl Pts',(3.3913352153028,-2.31374040927761,-31.1594698279445)) ;
#59402 = CARTESIAN_POINT('Ctrl Pts',(3.39047522401304,-2.2799337947475,-31.1525357163469)) ;
#59403 = CARTESIAN_POINT('Ctrl Pts',(3.38918061233769,-2.2295120860789,-31.1421949650033)) ;
#59404 = CARTESIAN_POINT('Ctrl Pts',(3.38874828632986,-2.21275288544962,-31.1387581192029)) ;
#59405 = CARTESIAN_POINT('Ctrl Pts',(3.38788232780283,-2.17937857710456,-31.1319145233968)) ;
#59406 = CARTESIAN_POINT('Ctrl Pts',(3.38744869751914,-2.16276346938089,-31.1285077731469)) ;
#59407 = CARTESIAN_POINT('Ctrl Pts',(3.38657996660205,-2.12972537009392,-31.1217343692224)) ;
#59408 = CARTESIAN_POINT('Ctrl Pts',(3.38614488362664,-2.11330238236914,-31.1183677144256)) ;
#59409 = CARTESIAN_POINT('Ctrl Pts',(3.38527227154898,-2.08069655001507,-31.1116845912588)) ;
#59410 = CARTESIAN_POINT('Ctrl Pts',(3.3848347902236,-2.06451370518087,-31.1083681176504)) ;
#59411 = CARTESIAN_POINT('Ctrl Pts',(3.38417469768363,-2.04045556517289,-31.1034387562193)) ;
#59412 = CARTESIAN_POINT('Ctrl Pts',(3.38395399652491,-2.03247220724235,-31.101803196829)) ;
#59413 = CARTESIAN_POINT('Ctrl Pts',(3.38351054520699,-2.01658353930749,-31.0985485253133)) ;
#59414 = CARTESIAN_POINT('Ctrl Pts',(3.38328779585336,-2.00867822929873,-31.0969294130999)) ;
#59415 = CARTESIAN_POINT('Ctrl Pts',(3.38283899220078,-1.992951663947,-31.0937090211981)) ;
#59416 = CARTESIAN_POINT('Ctrl Pts',(3.38261296631749,-1.98513040877856,-31.0921077384556)) ;
#59417 = CARTESIAN_POINT('Ctrl Pts',(3.3822696832439,-1.97346607677957,-31.0897203182271)) ;
#59418 = CARTESIAN_POINT('Ctrl Pts',(3.38215453645563,-1.96958922467574,-31.0889269300949)) ;
#59419 = CARTESIAN_POINT('Ctrl Pts',(3.38192228142768,-1.96185879060935,-31.0873452044946)) ;
#59420 = CARTESIAN_POINT('Ctrl Pts',(3.38180517497239,-1.9580052086334,-31.0865568668297)) ;
#59421 = CARTESIAN_POINT('Ctrl Pts',(3.38156801502377,-1.95031704378451,-31.0849844614994)) ;
#59422 = CARTESIAN_POINT('Ctrl Pts',(3.38144167908556,-1.94627818500258,-31.0841586126848)) ;
#59423 = CARTESIAN_POINT('Ctrl Pts',(3.38117685164134,-1.93800837070766,-31.0824683044267)) ;
#59424 = CARTESIAN_POINT('Ctrl Pts',(3.38103843247478,-1.93377741451519,-31.0816038369745)) ;
#59425 = CARTESIAN_POINT('Ctrl Pts',(3.3808226822932,-1.92743124310526,-31.0803080737017)) ;
#59426 = CARTESIAN_POINT('Ctrl Pts',(3.38074939587864,-1.92531590971377,-31.0798763134386)) ;
#59427 = CARTESIAN_POINT('Ctrl Pts',(3.3805996872188,-1.92110939521005,-31.0790181546749)) ;
#59428 = CARTESIAN_POINT('Ctrl Pts',(3.38052330043609,-1.91901821364194,-31.0785917522226)) ;
#59429 = CARTESIAN_POINT('Ctrl Pts',(3.38040532104915,-1.91591759373161,-31.0779600335174)) ;
#59430 = CARTESIAN_POINT('Ctrl Pts',(3.38036541656933,-1.91489008298177,-31.0777507768194)) ;
#59431 = CARTESIAN_POINT('Ctrl Pts',(3.38028402215018,-1.91285012330151,-31.0773355668686)) ;
#59432 = CARTESIAN_POINT('Ctrl Pts',(3.38024253472088,-1.91183767432828,-31.0771296133342)) ;
#59433 = CARTESIAN_POINT('Ctrl Pts',(3.38015711422549,-1.90983084892124,-31.0767217291221)) ;
#59434 = CARTESIAN_POINT('Ctrl Pts',(3.38011322012409,-1.90883647431282,-31.0765197945864)) ;
#59435 = CARTESIAN_POINT('Ctrl Pts',(3.38004404061596,-1.90736073883729,-31.0762205458143)) ;
#59436 = CARTESIAN_POINT('Ctrl Pts',(3.38002041465609,-1.90687146525441,-31.076121406225)) ;
#59437 = CARTESIAN_POINT('Ctrl Pts',(3.37997143425657,-1.90589857972234,-31.0759244919573)) ;
#59438 = CARTESIAN_POINT('Ctrl Pts',(3.37994610382241,-1.90541496712062,-31.0758267145325)) ;
#59439 = CARTESIAN_POINT('Ctrl Pts',(3.37990549909382,-1.90468717824974,-31.075679839486)) ;
#59440 = CARTESIAN_POINT('Ctrl Pts',(3.37989057675563,-1.90442766615567,-31.0756275156108)) ;
#59441 = CARTESIAN_POINT('Ctrl Pts',(3.37985850297489,-1.90389648573531,-31.0755205832803)) ;
#59442 = CARTESIAN_POINT('Ctrl Pts',(3.37984135648545,-1.90362481722601,-31.0754659742485)) ;
#59443 = CARTESIAN_POINT('Ctrl Pts',(3.37980438540426,-1.90308179296695,-31.0753571124616)) ;
#59444 = CARTESIAN_POINT('Ctrl Pts',(3.37978465703699,-1.90281047598829,-31.0753028573013)) ;
#59445 = CARTESIAN_POINT('Ctrl Pts',(3.37962891700279,-1.90163369580955,-31.0750751686933)) ;
#59446 = CARTESIAN_POINT('Ctrl Pts',(3.37962247443882,-1.90158501544534,-31.0750657498022)) ;
#59447 = CARTESIAN_POINT('Ctrl Pts',(3.37961603187484,-1.90153633508113,-31.0750563309111)) ;
#59448 = CARTESIAN_POINT('',(10.8335168660175,-15.0366437072153,-32.1991482053236)) ;
#59449 = CARTESIAN_POINT('',(10.8616065908236,-15.0366437072153,-32.1896836750667)) ;
#59450 = CARTESIAN_POINT('Origin',(-0.436147547989925,-21.6462763158694,1.29443979419782)) ;
#59451 = CARTESIAN_POINT('',(9.98082102021339,-1.90153624263669,-29.622021218349)) ;
#59452 = CARTESIAN_POINT('Ctrl Pts',(9.98082102598227,-1.90153633370295,-29.6220212362645)) ;
#59453 = CARTESIAN_POINT('Ctrl Pts',(9.98081813631591,-1.90158489238407,-29.6220327993228)) ;
#59454 = CARTESIAN_POINT('Ctrl Pts',(9.98076855213416,-1.90241811745866,-29.6222312114266)) ;
#59455 = CARTESIAN_POINT('Ctrl Pts',(9.98077161916715,-1.90281781836607,-29.6223173426495)) ;
#59456 = CARTESIAN_POINT('Ctrl Pts',(9.98077656137303,-1.9030907160465,-29.6223751894864)) ;
#59457 = CARTESIAN_POINT('Ctrl Pts',(9.98078885651281,-1.90363690191882,-29.6224901560522)) ;
#59458 = CARTESIAN_POINT('Ctrl Pts',(9.98079629783591,-1.90391015129655,-29.6225472375348)) ;
#59459 = CARTESIAN_POINT('Ctrl Pts',(9.98081223588766,-1.90444442170522,-29.6226583782004)) ;
#59460 = CARTESIAN_POINT('Ctrl Pts',(9.98082073741189,-1.90470544292088,-29.6227124358077)) ;
#59461 = CARTESIAN_POINT('Ctrl Pts',(9.98084576989917,-1.90543750589486,-29.6228636457412)) ;
#59462 = CARTESIAN_POINT('Ctrl Pts',(9.98086398323431,-1.9059239730479,-29.6229635950973)) ;
#59463 = CARTESIAN_POINT('Ctrl Pts',(9.98090251341636,-1.9069026009321,-29.6231640266788)) ;
#59464 = CARTESIAN_POINT('Ctrl Pts',(9.98092285312758,-1.90739476231177,-29.6232645013418)) ;
#59465 = CARTESIAN_POINT('Ctrl Pts',(9.98098619086646,-1.90887920773021,-29.6235668802546)) ;
#59466 = CARTESIAN_POINT('Ctrl Pts',(9.98103146973062,-1.90987945102643,-29.6237697517133)) ;
#59467 = CARTESIAN_POINT('Ctrl Pts',(9.98112587712619,-1.91189812019236,-29.6241781626848)) ;
#59468 = CARTESIAN_POINT('Ctrl Pts',(9.98117504274455,-1.91291654423624,-29.6243836893032)) ;
#59469 = CARTESIAN_POINT('Ctrl Pts',(9.98127620660854,-1.91496854271383,-29.6247970920327)) ;
#59470 = CARTESIAN_POINT('Ctrl Pts',(9.98132820728659,-1.91600211719088,-29.6250049673334)) ;
#59471 = CARTESIAN_POINT('Ctrl Pts',(9.98148745395848,-1.91912103466703,-29.6256314676495)) ;
#59472 = CARTESIAN_POINT('Ctrl Pts',(9.98159789961051,-1.92122455645945,-29.6260529789081)) ;
#59473 = CARTESIAN_POINT('Ctrl Pts',(9.98182384020141,-1.9254558932669,-29.6268995978579)) ;
#59474 = CARTESIAN_POINT('Ctrl Pts',(9.98193936909476,-1.92758370873797,-29.627324694208)) ;
#59475 = CARTESIAN_POINT('Ctrl Pts',(9.98228989915498,-1.93396732640727,-29.6285986919253)) ;
#59476 = CARTESIAN_POINT('Ctrl Pts',(9.9825287775567,-1.93822324679246,-29.6294463126736)) ;
#59477 = CARTESIAN_POINT('Ctrl Pts',(9.98300116316303,-1.94654185476612,-29.6311012247671)) ;
#59478 = CARTESIAN_POINT('Ctrl Pts',(9.98323473955941,-1.95060454303379,-29.631908492947)) ;
#59479 = CARTESIAN_POINT('Ctrl Pts',(9.98368255605493,-1.95833827461836,-29.633444136637)) ;
#59480 = CARTESIAN_POINT('Ctrl Pts',(9.98390871275382,-1.96221480004706,-29.6342133074122)) ;
#59481 = CARTESIAN_POINT('Ctrl Pts',(9.98436493992941,-1.96999125950243,-29.6357554350788)) ;
#59482 = CARTESIAN_POINT('Ctrl Pts',(9.98459501211632,-1.97389119354246,-29.6365283913966)) ;
#59483 = CARTESIAN_POINT('Ctrl Pts',(9.98529025494379,-1.98562497237449,-29.6388529762627)) ;
#59484 = CARTESIAN_POINT('Ctrl Pts',(9.98576040690957,-1.99349279346355,-29.6404103357754)) ;
#59485 = CARTESIAN_POINT('Ctrl Pts',(9.98671119165241,-2.00931299098254,-29.6435399627786)) ;
#59486 = CARTESIAN_POINT('Ctrl Pts',(9.98719185157983,-2.01726536723783,-29.645112221083)) ;
#59487 = CARTESIAN_POINT('Ctrl Pts',(9.98816197703178,-2.03324863225337,-29.6482708923264)) ;
#59488 = CARTESIAN_POINT('Ctrl Pts',(9.98865144333217,-2.04127952101813,-29.6498573050044)) ;
#59489 = CARTESIAN_POINT('Ctrl Pts',(9.99013124687624,-2.06548089680454,-29.6546364071499)) ;
#59490 = CARTESIAN_POINT('Ctrl Pts',(9.99113289198428,-2.08176008985808,-29.6578489925809)) ;
#59491 = CARTESIAN_POINT('Ctrl Pts',(9.99315950009389,-2.11456004815152,-29.6643189874948)) ;
#59492 = CARTESIAN_POINT('Ctrl Pts',(9.99418450879868,-2.13108081359634,-29.667576381623)) ;
#59493 = CARTESIAN_POINT('Ctrl Pts',(9.99625275550711,-2.16431561192512,-29.6741271744382)) ;
#59494 = CARTESIAN_POINT('Ctrl Pts',(9.9972960100553,-2.18102964097007,-29.6774205667135)) ;
#59495 = CARTESIAN_POINT('Ctrl Pts',(9.9993964069154,-2.21460264965853,-29.6840342819798)) ;
#59496 = CARTESIAN_POINT('Ctrl Pts',(10.0004535513673,-2.23146162930993,-29.6873546042511)) ;
#59497 = CARTESIAN_POINT('Ctrl Pts',(10.0036398912599,-2.28218353274662,-29.6973421615439)) ;
#59498 = CARTESIAN_POINT('Ctrl Pts',(10.0057839243653,-2.31619142072435,-29.7040360101861)) ;
#59499 = CARTESIAN_POINT('Ctrl Pts',(10.0100824939905,-2.38420731512499,-29.7174201942883)) ;
#59500 = CARTESIAN_POINT('Ctrl Pts',(10.0122370715424,-2.4182153078838,-29.7241105129429)) ;
#59501 = CARTESIAN_POINT('Ctrl Pts',(10.0165293804464,-2.48584491142059,-29.7374125662913)) ;
#59502 = CARTESIAN_POINT('Ctrl Pts',(10.0186671287307,-2.51946652224412,-29.7440242952898)) ;
#59503 = CARTESIAN_POINT('Ctrl Pts',(10.0250152291373,-2.61917207551851,-29.7636286226259)) ;
#59504 = CARTESIAN_POINT('Ctrl Pts',(10.0291603271039,-2.68409673841795,-29.776390398192)) ;
#59505 = CARTESIAN_POINT('Ctrl Pts',(10.0374451175131,-2.81365377182546,-29.8018520291029)) ;
#59506 = CARTESIAN_POINT('Ctrl Pts',(10.0417974675238,-2.88158937318959,-29.8152005826093)) ;
#59507 = CARTESIAN_POINT('Ctrl Pts',(10.0505402348891,-3.01787063559852,-29.8419742868526)) ;
#59508 = CARTESIAN_POINT('Ctrl Pts',(10.0549306893133,-3.0862162967159,-29.8553994251151)) ;
#59509 = CARTESIAN_POINT('Ctrl Pts',(10.063746247243,-3.22330444799194,-29.8823245653509)) ;
#59510 = CARTESIAN_POINT('Ctrl Pts',(10.0681713657794,-3.29204693813702,-29.8958245622563)) ;
#59511 = CARTESIAN_POINT('Ctrl Pts',(10.0770536772797,-3.42991551815616,-29.9228974023034)) ;
#59512 = CARTESIAN_POINT('Ctrl Pts',(10.0815108721742,-3.49904160803363,-29.9364702447942)) ;
#59513 = CARTESIAN_POINT('Ctrl Pts',(10.0949274455347,-3.70697543463906,-29.9772947666975)) ;
#59514 = CARTESIAN_POINT('Ctrl Pts',(10.1039317092748,-3.84633872768537,-30.0046524752369)) ;
#59515 = CARTESIAN_POINT('Ctrl Pts',(10.122046733416,-4.12644097408161,-30.0596320060214)) ;
#59516 = CARTESIAN_POINT('Ctrl Pts',(10.1311575503894,-4.26717992751092,-30.0872538092222)) ;
#59517 = CARTESIAN_POINT('Ctrl Pts',(10.1494750088276,-4.54992767466381,-30.1427420485428)) ;
#59518 = CARTESIAN_POINT('Ctrl Pts',(10.1586816754589,-4.69193646747835,-30.1706084759848)) ;
#59519 = CARTESIAN_POINT('Ctrl Pts',(10.1771814062645,-4.97711807142237,-30.2265660630076)) ;
#59520 = CARTESIAN_POINT('Ctrl Pts',(10.186474483048,-5.12029088256691,-30.2546572183432)) ;
#59521 = CARTESIAN_POINT('Ctrl Pts',(10.2051383429346,-5.40769470394702,-30.3110441130795)) ;
#59522 = CARTESIAN_POINT('Ctrl Pts',(10.214509132221,-5.5519257141803,-30.3393398503962)) ;
#59523 = CARTESIAN_POINT('Ctrl Pts',(10.2333201932668,-5.84134011499873,-30.39611560365)) ;
#59524 = CARTESIAN_POINT('Ctrl Pts',(10.2427604661428,-5.98652350558523,-30.4245956192103)) ;
#59525 = CARTESIAN_POINT('Ctrl Pts',(10.2711736295317,-6.4233435202736,-30.5102814718431)) ;
#59526 = CARTESIAN_POINT('Ctrl Pts',(10.2902387921012,-6.71624998261006,-30.5677331383397)) ;
#59527 = CARTESIAN_POINT('Ctrl Pts',(10.3285541927133,-7.30460259223824,-30.6831279529963)) ;
#59528 = CARTESIAN_POINT('Ctrl Pts',(10.3478044672482,-7.6000487395636,-30.741071088868)) ;
#59529 = CARTESIAN_POINT('Ctrl Pts',(10.3864310012383,-8.19263416749283,-30.8572841407583)) ;
#59530 = CARTESIAN_POINT('Ctrl Pts',(10.4058072787758,-8.48977344809338,-30.9155540506836)) ;
#59531 = CARTESIAN_POINT('Ctrl Pts',(10.4446277699812,-9.08489859170915,-31.0322555983316)) ;
#59532 = CARTESIAN_POINT('Ctrl Pts',(10.4640719921157,-9.38288445473128,-31.0906872332025)) ;
#59533 = CARTESIAN_POINT('Ctrl Pts',(10.5224204792962,-10.2768420919756,-31.2659768176842)) ;
#59534 = CARTESIAN_POINT('Ctrl Pts',(10.5613404148874,-10.8728138989514,-31.3828294944131)) ;
#59535 = CARTESIAN_POINT('Ctrl Pts',(10.6387676678931,-12.0579851840454,-31.6151970020299)) ;
#59536 = CARTESIAN_POINT('Ctrl Pts',(10.6772750585538,-12.6471846622151,-31.7307118082486)) ;
#59537 = CARTESIAN_POINT('Ctrl Pts',(10.7534264185142,-13.8120388658114,-31.959078574304)) ;
#59538 = CARTESIAN_POINT('Ctrl Pts',(10.7929238620596,-14.4160365129575,-32.0774868980543)) ;
#59539 = CARTESIAN_POINT('Ctrl Pts',(10.8316989411202,-15.0088506101495,-32.1936997662465)) ;
#59540 = CARTESIAN_POINT('Ctrl Pts',(10.8335168657289,-15.0366437072151,-32.1991482054207)) ;
#59541 = CARTESIAN_POINT('Ctrl Pts',(10.8616065911119,-15.0366437072151,-32.1896836749694)) ;
#59542 = CARTESIAN_POINT('Ctrl Pts',(10.8597565733843,-15.0088506101318,-32.1842460492222)) ;
#59543 = CARTESIAN_POINT('Ctrl Pts',(10.857904869647,-14.9810324826228,-32.1788035330569)) ;
#59544 = CARTESIAN_POINT('Ctrl Pts',(10.8184090484746,-14.3876935911638,-32.0627190668428)) ;
#59545 = CARTESIAN_POINT('Ctrl Pts',(10.7800820901594,-13.8120388657218,-31.9500972327959)) ;
#59546 = CARTESIAN_POINT('Ctrl Pts',(10.7025039813416,-12.6471846620883,-31.7222111943943)) ;
#59547 = CARTESIAN_POINT('Ctrl Pts',(10.6632528658263,-12.0579851838998,-31.6069469782516)) ;
#59548 = CARTESIAN_POINT('Ctrl Pts',(10.5842693409797,-10.8728138987679,-31.3751038396628)) ;
#59549 = CARTESIAN_POINT('Ctrl Pts',(10.5445370048881,-10.2768420917731,-31.2585248925291)) ;
#59550 = CARTESIAN_POINT('Ctrl Pts',(10.4849070942047,-9.38288445450015,-31.08366706989)) ;
#59551 = CARTESIAN_POINT('Ctrl Pts',(10.4650251858398,-9.08489859146851,-31.0253829086787)) ;
#59552 = CARTESIAN_POINT('Ctrl Pts',(10.4253051421847,-8.48977344783374,-30.9089844555366)) ;
#59553 = CARTESIAN_POINT('Ctrl Pts',(10.40546701536,-8.19263416722367,-30.8508701607525)) ;
#59554 = CARTESIAN_POINT('Ctrl Pts',(10.3658881887475,-7.60004873927551,-30.7349779736013)) ;
#59555 = CARTESIAN_POINT('Ctrl Pts',(10.3461475070413,-7.30460259194072,-30.6772000751425)) ;
#59556 = CARTESIAN_POINT('Ctrl Pts',(10.3068161653798,-6.71624998229373,-30.562147570877)) ;
#59557 = CARTESIAN_POINT('Ctrl Pts',(10.2872255419149,-6.42334351994791,-30.5048729527681)) ;
#59558 = CARTESIAN_POINT('Ctrl Pts',(10.2579901956425,-5.98652350524559,-30.4194641258002)) ;
#59559 = CARTESIAN_POINT('Ctrl Pts',(10.2482701603494,-5.84134011465445,-30.3910783731724)) ;
#59560 = CARTESIAN_POINT('Ctrl Pts',(10.2288862936885,-5.55192571382677,-30.3344956205997)) ;
#59561 = CARTESIAN_POINT('Ctrl Pts',(10.2192224634346,-5.40769470358889,-30.30629862028)) ;
#59562 = CARTESIAN_POINT('Ctrl Pts',(10.1999567380997,-5.12029088219959,-30.2501145176226)) ;
#59563 = CARTESIAN_POINT('Ctrl Pts',(10.1903548491999,-4.97711807105047,-30.2221274132028)) ;
#59564 = CARTESIAN_POINT('Ctrl Pts',(10.1712182678004,-4.69193646709734,-30.1663844061269)) ;
#59565 = CARTESIAN_POINT('Ctrl Pts',(10.1616835879102,-4.54992767427827,-30.138628499219)) ;
#59566 = CARTESIAN_POINT('Ctrl Pts',(10.1426859378703,-4.26717992711634,-30.0833694431312)) ;
#59567 = CARTESIAN_POINT('Ctrl Pts',(10.1332229930092,-4.12644097368253,-30.0558662856289)) ;
#59568 = CARTESIAN_POINT('Ctrl Pts',(10.1143720437184,-3.84633872727734,-30.0011347168959)) ;
#59569 = CARTESIAN_POINT('Ctrl Pts',(10.104984095847,-3.70697543422659,-29.9739062865914)) ;
#59570 = CARTESIAN_POINT('Ctrl Pts',(10.0909589888611,-3.49904160761451,-29.9332868035381)) ;
#59571 = CARTESIAN_POINT('Ctrl Pts',(10.0862933965109,-3.42991551773483,-29.9197841783251)) ;
#59572 = CARTESIAN_POINT('Ctrl Pts',(10.0769807583747,-3.2920469377113,-29.8928563322026)) ;
#59573 = CARTESIAN_POINT('Ctrl Pts',(10.0723337145218,-3.22330444756401,-29.879431110642)) ;
#59574 = CARTESIAN_POINT('Ctrl Pts',(10.0630573184486,-3.08621629628361,-29.8526612448547)) ;
#59575 = CARTESIAN_POINT('Ctrl Pts',(10.0584279812629,-3.01787063516402,-29.8393165955654)) ;
#59576 = CARTESIAN_POINT('Ctrl Pts',(10.0491852822835,-2.88158937275076,-29.8127113378945)) ;
#59577 = CARTESIAN_POINT('Ctrl Pts',(10.0445719575502,-2.81365377138444,-29.7994507170098)) ;
#59578 = CARTESIAN_POINT('Ctrl Pts',(10.0357586992447,-2.68409673802282,-29.7741671476752)) ;
#59579 = CARTESIAN_POINT('Ctrl Pts',(10.0313354854857,-2.61917207517383,-29.7614990802411)) ;
#59580 = CARTESIAN_POINT('Ctrl Pts',(10.0245251307954,-2.51946652197692,-29.7420505045245)) ;
#59581 = CARTESIAN_POINT('Ctrl Pts',(10.0222257294742,-2.48584491117954,-29.7354932427815)) ;
#59582 = CARTESIAN_POINT('Ctrl Pts',(10.0175927471364,-2.41821530769531,-29.7223059756892)) ;
#59583 = CARTESIAN_POINT('Ctrl Pts',(10.01525918304,-2.38420731496295,-29.7156759646289)) ;
#59584 = CARTESIAN_POINT('Ctrl Pts',(10.0105814814048,-2.31619142061517,-29.7024195249859)) ;
#59585 = CARTESIAN_POINT('Ctrl Pts',(10.0082373866956,-2.28218353266388,-29.6957930849522)) ;
#59586 = CARTESIAN_POINT('Ctrl Pts',(10.0047297976448,-2.2314616292666,-29.6859137691122)) ;
#59587 = CARTESIAN_POINT('Ctrl Pts',(10.0035620095976,-2.21460264962826,-29.6826307270115)) ;
#59588 = CARTESIAN_POINT('Ctrl Pts',(10.0012316710292,-2.18102964096591,-29.6760944881331)) ;
#59589 = CARTESIAN_POINT('Ctrl Pts',(10.0000691226531,-2.16431561193394,-29.6728412906312)) ;
#59590 = CARTESIAN_POINT('Ctrl Pts',(9.99775126861663,-2.13108081363099,-29.6663746003226)) ;
#59591 = CARTESIAN_POINT('Ctrl Pts',(9.99659597999818,-2.11456004819905,-29.6631611026111)) ;
#59592 = CARTESIAN_POINT('Ctrl Pts',(9.99429387456847,-2.0817600899311,-29.6567839335578)) ;
#59593 = CARTESIAN_POINT('Ctrl Pts',(9.99314710341809,-2.06548089689024,-29.6536202467865)) ;
#59594 = CARTESIAN_POINT('Ctrl Pts',(9.99143297536932,-2.04127952112266,-29.6489200977634)) ;
#59595 = CARTESIAN_POINT('Ctrl Pts',(9.99086258006168,-2.03324863236408,-29.6473609532442)) ;
#59596 = CARTESIAN_POINT('Ctrl Pts',(9.98972334381673,-2.01726536736095,-29.6442592620639)) ;
#59597 = CARTESIAN_POINT('Ctrl Pts',(9.98915450367532,-2.0093129911118,-29.6427167151343)) ;
#59598 = CARTESIAN_POINT('Ctrl Pts',(9.98801744725042,-1.99349279360512,-29.6396498503709)) ;
#59599 = CARTESIAN_POINT('Ctrl Pts',(9.98744925815376,-1.98562497252213,-29.638125523415)) ;
#59600 = CARTESIAN_POINT('Ctrl Pts',(9.98659595732529,-1.97389119369923,-29.6358541944921)) ;
#59601 = CARTESIAN_POINT('Ctrl Pts',(9.98631134296961,-1.96999125966218,-29.6350996155713)) ;
#59602 = CARTESIAN_POINT('Ctrl Pts',(9.98574128636084,-1.96221480021287,-29.6335958415077)) ;
#59603 = CARTESIAN_POINT('Ctrl Pts',(9.98545584580647,-1.95833827478728,-29.6328466457898)) ;
#59604 = CARTESIAN_POINT('Ctrl Pts',(9.98488301744925,-1.95060454321582,-29.6313531235031)) ;
#59605 = CARTESIAN_POINT('Ctrl Pts',(9.98458042814821,-1.94654185495839,-29.6305691084804)) ;
#59606 = CARTESIAN_POINT('Ctrl Pts',(9.98395498092834,-1.93822324700642,-29.6289657688539)) ;
#59607 = CARTESIAN_POINT('Ctrl Pts',(9.98363219212854,-1.9339673266325,-29.628146420813)) ;
#59608 = CARTESIAN_POINT('Ctrl Pts',(9.98314025611079,-1.9275837089799,-29.6269200683138)) ;
#59609 = CARTESIAN_POINT('Ctrl Pts',(9.98297497049299,-1.92545589351462,-29.6265117369574)) ;
#59610 = CARTESIAN_POINT('Ctrl Pts',(9.98264248827336,-1.9212245567182,-29.6257010160644)) ;
#59611 = CARTESIAN_POINT('Ctrl Pts',(9.9824753255637,-1.91912103493106,-29.6252986150088)) ;
#59612 = CARTESIAN_POINT('Ctrl Pts',(9.98222295889623,-1.91600211746307,-29.6247034904741)) ;
#59613 = CARTESIAN_POINT('Ctrl Pts',(9.98213855545869,-1.91496854298954,-29.624506532935)) ;
#59614 = CARTESIAN_POINT('Ctrl Pts',(9.98196891063809,-1.91291654451728,-29.6241162041275)) ;
#59615 = CARTESIAN_POINT('Ctrl Pts',(9.98188367167153,-1.91189812047543,-29.6239228320356)) ;
#59616 = CARTESIAN_POINT('Ctrl Pts',(9.98171166896053,-1.90987945131465,-29.6235405659712)) ;
#59617 = CARTESIAN_POINT('Ctrl Pts',(9.98162494256724,-1.90887920802121,-29.6233516598116)) ;
#59618 = CARTESIAN_POINT('Ctrl Pts',(9.98149237338653,-1.90739476260648,-29.6230726076883)) ;
#59619 = CARTESIAN_POINT('Ctrl Pts',(9.9814477610636,-1.90690260122667,-29.6229803114205)) ;
#59620 = CARTESIAN_POINT('Ctrl Pts',(9.98135713865687,-1.90592397334478,-29.6227974317535)) ;
#59621 = CARTESIAN_POINT('Ctrl Pts',(9.98131115132827,-1.90543750619486,-29.6227068405461)) ;
#59622 = CARTESIAN_POINT('Ctrl Pts',(9.98123957118407,-1.90470544341716,-29.6225713143871)) ;
#59623 = CARTESIAN_POINT('Ctrl Pts',(9.98121362489977,-1.90444442240732,-29.6225231346487)) ;
#59624 = CARTESIAN_POINT('Ctrl Pts',(9.98115905365425,-1.90391015241643,-29.6224250111128)) ;
#59625 = CARTESIAN_POINT('Ctrl Pts',(9.981130433504,-1.90363690324913,-29.6223750656538)) ;
#59626 = CARTESIAN_POINT('Ctrl Pts',(9.98107064682837,-1.90309071780404,-29.6222761009427)) ;
#59627 = CARTESIAN_POINT('Ctrl Pts',(9.9810395738566,-1.90281782033889,-29.6222270586329)) ;
#59628 = CARTESIAN_POINT('Ctrl Pts',(9.98083763067218,-1.90163369767085,-29.6220368741041)) ;
#59629 = CARTESIAN_POINT('Ctrl Pts',(9.98082932832723,-1.9015850156869,-29.6220290551843)) ;
#59630 = CARTESIAN_POINT('Ctrl Pts',(9.98082102598227,-1.90153633370295,-29.6220212362645)) ;
#59631 = CARTESIAN_POINT('',(23.3523050271291,-15.0366437072153,-24.6742797818822)) ;
#59632 = CARTESIAN_POINT('',(23.3738245177983,-15.0366437072153,-24.6538954375541)) ;
#59633 = CARTESIAN_POINT('Origin',(-0.939357956114975,-21.6462763158693,0.991668137384664)) ;
#59634 = CARTESIAN_POINT('',(21.496311701647,-1.90153623936716,-22.6933803669979)) ;
#59635 = CARTESIAN_POINT('Ctrl Pts',(21.4963117139471,-1.90153632716387,-22.6933803803385)) ;
#59636 = CARTESIAN_POINT('Ctrl Pts',(21.4963139585538,-1.90158488788986,-22.6933920772455)) ;
#59637 = CARTESIAN_POINT('Ctrl Pts',(21.4963526813015,-1.90242263142415,-22.6935938659951)) ;
#59638 = CARTESIAN_POINT('Ctrl Pts',(21.4963918791992,-1.90282441372072,-22.6936711055929)) ;
#59639 = CARTESIAN_POINT('Ctrl Pts',(21.4964208293853,-1.90309873132532,-22.6937217687247)) ;
#59640 = CARTESIAN_POINT('Ctrl Pts',(21.4964806174594,-1.9036477572329,-22.693821418077)) ;
#59641 = CARTESIAN_POINT('Ctrl Pts',(21.4965115196631,-1.90392242669208,-22.6938703323172)) ;
#59642 = CARTESIAN_POINT('Ctrl Pts',(21.4965730073544,-1.90445947279204,-22.6939649615802)) ;
#59643 = CARTESIAN_POINT('Ctrl Pts',(21.4966035966074,-1.90472184962075,-22.6940106730897)) ;
#59644 = CARTESIAN_POINT('Ctrl Pts',(21.4966903054876,-1.90545775387604,-22.6941380177788)) ;
#59645 = CARTESIAN_POINT('Ctrl Pts',(21.4967491393391,-1.90594678716221,-22.6942214937476)) ;
#59646 = CARTESIAN_POINT('Ctrl Pts',(21.4968689478468,-1.90693057720395,-22.6943880470282)) ;
#59647 = CARTESIAN_POINT('Ctrl Pts',(21.4969299401569,-1.90742533460924,-22.6944711078024)) ;
#59648 = CARTESIAN_POINT('Ctrl Pts',(21.4971154317997,-1.90891760993743,-22.6947201861981)) ;
#59649 = CARTESIAN_POINT('Ctrl Pts',(21.4972424168975,-1.90992312895963,-22.6948861267403)) ;
#59650 = CARTESIAN_POINT('Ctrl Pts',(21.4975010204046,-1.91195244521774,-22.6952188219258)) ;
#59651 = CARTESIAN_POINT('Ctrl Pts',(21.4976326671314,-1.91297624062658,-22.6953855492251)) ;
#59652 = CARTESIAN_POINT('Ctrl Pts',(21.4978995329129,-1.91503906152865,-22.695719955273)) ;
#59653 = CARTESIAN_POINT('Ctrl Pts',(21.4980347538706,-1.91607808706589,-22.6958876322313)) ;
#59654 = CARTESIAN_POINT('Ctrl Pts',(21.4984445862641,-1.91921345336299,-22.696391919799)) ;
#59655 = CARTESIAN_POINT('Ctrl Pts',(21.4987233311854,-1.92132806855155,-22.6967298168923)) ;
#59656 = CARTESIAN_POINT('Ctrl Pts',(21.4992869388782,-1.92558171967302,-22.6974067674593)) ;
#59657 = CARTESIAN_POINT('Ctrl Pts',(21.4995718277727,-1.927720756062,-22.6977457963179)) ;
#59658 = CARTESIAN_POINT('Ctrl Pts',(21.500429539133,-1.93413803650467,-22.6987600475774)) ;
#59659 = CARTESIAN_POINT('Ctrl Pts',(21.5010053506063,-1.93841639875659,-22.6994324722858)) ;
#59660 = CARTESIAN_POINT('Ctrl Pts',(21.5021350348965,-1.94677887040481,-22.7007428078236)) ;
#59661 = CARTESIAN_POINT('Ctrl Pts',(21.502688960902,-1.95086298048004,-22.7013806684633)) ;
#59662 = CARTESIAN_POINT('Ctrl Pts',(21.5037458825198,-1.95863767629825,-22.7025926144358)) ;
#59663 = CARTESIAN_POINT('Ctrl Pts',(21.5042769737302,-1.96253482848826,-22.7031988866226)) ;
#59664 = CARTESIAN_POINT('Ctrl Pts',(21.505344320571,-1.97035266596653,-22.70441323784)) ;
#59665 = CARTESIAN_POINT('Ctrl Pts',(21.5058805775187,-1.9742733512682,-22.7050213156265)) ;
#59666 = CARTESIAN_POINT('Ctrl Pts',(21.5074963416005,-1.98606956461108,-22.7068486477647)) ;
#59667 = CARTESIAN_POINT('Ctrl Pts',(21.5085828074178,-1.99397924967536,-22.7080710335096)) ;
#59668 = CARTESIAN_POINT('Ctrl Pts',(21.5107715848834,-2.00988362495031,-22.7105249922724)) ;
#59669 = CARTESIAN_POINT('Ctrl Pts',(21.5118739173825,-2.01787831498638,-22.7117565454895)) ;
#59670 = CARTESIAN_POINT('Ctrl Pts',(21.5140925843333,-2.03394662524021,-22.7142288565352)) ;
#59671 = CARTESIAN_POINT('Ctrl Pts',(21.5152089193814,-2.04202024546243,-22.7154696137994)) ;
#59672 = CARTESIAN_POINT('Ctrl Pts',(21.5185767066728,-2.06635039394262,-22.7192052036515)) ;
#59673 = CARTESIAN_POINT('Ctrl Pts',(21.5208468664255,-2.08271620655358,-22.7217134240119)) ;
#59674 = CARTESIAN_POINT('Ctrl Pts',(21.5254273675335,-2.11569068912034,-22.7267609335447)) ;
#59675 = CARTESIAN_POINT('Ctrl Pts',(21.5277377440152,-2.13229935928107,-22.7293001895015)) ;
#59676 = CARTESIAN_POINT('Ctrl Pts',(21.5323903166247,-2.16571099516926,-22.7344038676818)) ;
#59677 = CARTESIAN_POINT('Ctrl Pts',(21.5347325251025,-2.18251395705726,-22.7369682771135)) ;
#59678 = CARTESIAN_POINT('Ctrl Pts',(21.5394409725641,-2.21626560252734,-22.7421158136557)) ;
#59679 = CARTESIAN_POINT('Ctrl Pts',(21.5418072131894,-2.23321428611731,-22.7446989392129)) ;
#59680 = CARTESIAN_POINT('Ctrl Pts',(21.5489307493174,-2.28420607246569,-22.7524662951117)) ;
#59681 = CARTESIAN_POINT('Ctrl Pts',(21.553712806182,-2.31839491051271,-22.7576685546976)) ;
#59682 = CARTESIAN_POINT('Ctrl Pts',(21.5632849986474,-2.38677270505818,-22.7680654550021)) ;
#59683 = CARTESIAN_POINT('Ctrl Pts',(21.5680751645116,-2.4209616478915,-22.7732600631636)) ;
#59684 = CARTESIAN_POINT('Ctrl Pts',(21.5776069357775,-2.48895109533015,-22.7835847070533)) ;
#59685 = CARTESIAN_POINT('Ctrl Pts',(21.5823485541794,-2.52275159998098,-22.7887147304799)) ;
#59686 = CARTESIAN_POINT('Ctrl Pts',(21.5964164967376,-2.6229876659894,-22.8039216843402)) ;
#59687 = CARTESIAN_POINT('Ctrl Pts',(21.6055858239275,-2.68825777904764,-22.8138155781247)) ;
#59688 = CARTESIAN_POINT('Ctrl Pts',(21.6238983410685,-2.81853945525282,-22.8335545263681)) ;
#59689 = CARTESIAN_POINT('Ctrl Pts',(21.6335094237685,-2.88687193565162,-22.843901688933)) ;
#59690 = CARTESIAN_POINT('Ctrl Pts',(21.6527986704329,-3.02394935163266,-22.8646498792361)) ;
#59691 = CARTESIAN_POINT('Ctrl Pts',(21.6624768629465,-3.09269428728769,-22.8750508799517)) ;
#59692 = CARTESIAN_POINT('Ctrl Pts',(21.681896480493,-3.23058330586397,-22.8959066041)) ;
#59693 = CARTESIAN_POINT('Ctrl Pts',(21.6916379170892,-3.29972738877161,-22.9063613165752)) ;
#59694 = CARTESIAN_POINT('Ctrl Pts',(21.7111808231678,-3.43840139526491,-22.9273237072948)) ;
#59695 = CARTESIAN_POINT('Ctrl Pts',(21.7209822941359,-3.50793131885397,-22.9378313841313)) ;
#59696 = CARTESIAN_POINT('Ctrl Pts',(21.7504725253938,-3.71707989210545,-22.9694321897675)) ;
#59697 = CARTESIAN_POINT('Ctrl Pts',(21.7702470244795,-3.85725734359656,-22.9906031688657)) ;
#59698 = CARTESIAN_POINT('Ctrl Pts',(21.8100047544406,-4.13899594338214,-23.0331412836721)) ;
#59699 = CARTESIAN_POINT('Ctrl Pts',(21.8299880288275,-4.2805570917561,-23.0545083781865)) ;
#59700 = CARTESIAN_POINT('Ctrl Pts',(21.870145346404,-4.56495664710652,-23.0974254409772)) ;
#59701 = CARTESIAN_POINT('Ctrl Pts',(21.890319408865,-4.70779505317279,-23.1189753907396)) ;
#59702 = CARTESIAN_POINT('Ctrl Pts',(21.9308412967585,-4.99464268373381,-23.1622439739505)) ;
#59703 = CARTESIAN_POINT('Ctrl Pts',(21.9511891318898,-5.13865190824363,-23.1839625982162)) ;
#59704 = CARTESIAN_POINT('Ctrl Pts',(21.992042125138,-5.42773473827606,-23.2275538051461)) ;
#59705 = CARTESIAN_POINT('Ctrl Pts',(22.0125472880069,-5.57280834379641,-23.2494263833081)) ;
#59706 = CARTESIAN_POINT('Ctrl Pts',(22.0536988560531,-5.8639134989194,-23.2933104325269)) ;
#59707 = CARTESIAN_POINT('Ctrl Pts',(22.0743452620874,-6.00994504852342,-23.3153219027712)) ;
#59708 = CARTESIAN_POINT('Ctrl Pts',(22.1364725738118,-6.44931695857324,-23.3815417220833)) ;
#59709 = CARTESIAN_POINT('Ctrl Pts',(22.1781415168096,-6.74393457555848,-23.4259355317348)) ;
#59710 = CARTESIAN_POINT('Ctrl Pts',(22.2618558852985,-7.33572433109793,-23.5150936882605)) ;
#59711 = CARTESIAN_POINT('Ctrl Pts',(22.303901338843,-7.63289646968583,-23.5598580085705)) ;
#59712 = CARTESIAN_POINT('Ctrl Pts',(22.388245232698,-8.22894377121979,-23.6496317838259)) ;
#59713 = CARTESIAN_POINT('Ctrl Pts',(22.4305436869088,-8.52781893416259,-23.6946412256033)) ;
#59714 = CARTESIAN_POINT('Ctrl Pts',(22.5152708871044,-9.12642078800902,-23.784779082941)) ;
#59715 = CARTESIAN_POINT('Ctrl Pts',(22.5576996395945,-9.42614747891959,-23.8299074923405)) ;
#59716 = CARTESIAN_POINT('Ctrl Pts',(22.6849980529511,-10.3253275998488,-23.9652812195954)) ;
#59717 = CARTESIAN_POINT('Ctrl Pts',(22.7698797528227,-10.9247810626322,-24.0555151428219)) ;
#59718 = CARTESIAN_POINT('Ctrl Pts',(22.9387013685547,-12.1168760951015,-24.2349360469274)) ;
#59719 = CARTESIAN_POINT('Ctrl Pts',(23.0226413407052,-12.7095176648389,-24.3241229744988)) ;
#59720 = CARTESIAN_POINT('Ctrl Pts',(23.1889804045827,-13.8838032555933,-24.5008259087648)) ;
#59721 = CARTESIAN_POINT('Ctrl Pts',(23.2713709284772,-14.465386062484,-24.5883326063611)) ;
#59722 = CARTESIAN_POINT('Ctrl Pts',(23.3523050271262,-15.0366437072153,-24.6742797818849)) ;
#59723 = CARTESIAN_POINT('Ctrl Pts',(23.3738245178012,-15.0366437072153,-24.6538954375513)) ;
#59724 = CARTESIAN_POINT('Ctrl Pts',(23.3734610461599,-15.0340941323794,-24.6535139839134)) ;
#59725 = CARTESIAN_POINT('Ctrl Pts',(23.37309754507,-15.0315443518747,-24.6531324996256)) ;
#59726 = CARTESIAN_POINT('Ctrl Pts',(23.2916449156809,-14.4601946117196,-24.5676502869763)) ;
#59727 = CARTESIAN_POINT('Ctrl Pts',(23.2090927645543,-13.8811769232892,-24.4810268676804)) ;
#59728 = CARTESIAN_POINT('Ctrl Pts',(23.0420288777678,-12.7095176651673,-24.3057581239909)) ;
#59729 = CARTESIAN_POINT('Ctrl Pts',(22.957517168995,-12.1168760954787,-24.2171127741293)) ;
#59730 = CARTESIAN_POINT('Ctrl Pts',(22.7874992191376,-10.9247810631074,-24.0388250979295)) ;
#59731 = CARTESIAN_POINT('Ctrl Pts',(22.7019930343313,-10.3253276003733,-23.9491827182685)) ;
#59732 = CARTESIAN_POINT('Ctrl Pts',(22.5737096414841,-9.4261474795181,-23.814742013168)) ;
#59733 = CARTESIAN_POINT('Ctrl Pts',(22.5309444631412,-9.12642078863219,-23.7699322832708)) ;
#59734 = CARTESIAN_POINT('Ctrl Pts',(22.4455258388896,-8.52781893483503,-23.6804493776025)) ;
#59735 = CARTESIAN_POINT('Ctrl Pts',(22.4028723994856,-8.2289437719168,-23.6357761956683)) ;
#59736 = CARTESIAN_POINT('Ctrl Pts',(22.3177965715717,-7.63289647043186,-23.5466957451952)) ;
#59737 = CARTESIAN_POINT('Ctrl Pts',(22.2753741969594,-7.33572433186842,-23.5022884634925)) ;
#59738 = CARTESIAN_POINT('Ctrl Pts',(22.1908790031011,-6.74393457637766,-23.4138699440584)) ;
#59739 = CARTESIAN_POINT('Ctrl Pts',(22.1488062118971,-6.44931695941667,-23.3698586797545)) ;
#59740 = CARTESIAN_POINT('Ctrl Pts',(22.0860470145102,-6.00994504940297,-23.3042374143459)) ;
#59741 = CARTESIAN_POINT('Ctrl Pts',(22.0651855998762,-5.86391349981098,-23.282429611069)) ;
#59742 = CARTESIAN_POINT('Ctrl Pts',(22.0235938113801,-5.57280834471192,-23.2389625608171)) ;
#59743 = CARTESIAN_POINT('Ctrl Pts',(22.0028634383754,-5.42773473920353,-23.2173033130307)) ;
#59744 = CARTESIAN_POINT('Ctrl Pts',(21.9615478981759,-5.13865190919487,-23.1741502538532)) ;
#59745 = CARTESIAN_POINT('Ctrl Pts',(21.9409627357323,-4.9946426846969,-23.1526564379623)) ;
#59746 = CARTESIAN_POINT('Ctrl Pts',(21.899951420414,-4.70779505415949,-23.1098514650408)) ;
#59747 = CARTESIAN_POINT('Ctrl Pts',(21.8795252772345,-4.56495664810496,-23.0885402988219)) ;
#59748 = CARTESIAN_POINT('Ctrl Pts',(21.8388452293624,-4.28055709277793,-23.0461183924753)) ;
#59749 = CARTESIAN_POINT('Ctrl Pts',(21.8185913441993,-4.13899594441561,-23.0250076341073)) ;
#59750 = CARTESIAN_POINT('Ctrl Pts',(21.7782680553142,-3.85725734465321,-22.9830052451768)) ;
#59751 = CARTESIAN_POINT('Ctrl Pts',(21.7581986950839,-3.71707989317363,-22.9621135733942)) ;
#59752 = CARTESIAN_POINT('Ctrl Pts',(21.7282408036885,-3.50793131993937,-22.9309557589758)) ;
#59753 = CARTESIAN_POINT('Ctrl Pts',(21.7182791782025,-3.43840139635602,-22.9205997885584)) ;
#59754 = CARTESIAN_POINT('Ctrl Pts',(21.6984055622423,-3.29972738987415,-22.8999506628818)) ;
#59755 = CARTESIAN_POINT('Ctrl Pts',(21.6884935732522,-3.23058330697217,-22.8896575062172)) ;
#59756 = CARTESIAN_POINT('Ctrl Pts',(21.6687197927208,-3.09269428840723,-22.8691372630713)) ;
#59757 = CARTESIAN_POINT('Ctrl Pts',(21.6588580127507,-3.02394935275785,-22.8589101656336)) ;
#59758 = CARTESIAN_POINT('Ctrl Pts',(21.6391845502197,-2.88687193678811,-22.8385259239346)) ;
#59759 = CARTESIAN_POINT('Ctrl Pts',(21.6293728961843,-2.81853945639494,-22.828368752632)) ;
#59760 = CARTESIAN_POINT('Ctrl Pts',(21.6106543164916,-2.68825778012938,-22.8090144472516)) ;
#59761 = CARTESIAN_POINT('Ctrl Pts',(21.6012713503163,-2.62298766700186,-22.7993229230439)) ;
#59762 = CARTESIAN_POINT('Ctrl Pts',(21.5868483218045,-2.52275160088707,-22.7844523244347)) ;
#59763 = CARTESIAN_POINT('Ctrl Pts',(21.5819825280398,-2.48895109620037,-22.7794399261495)) ;
#59764 = CARTESIAN_POINT('Ctrl Pts',(21.5721890658123,-2.42096164868958,-22.7693631690854)) ;
#59765 = CARTESIAN_POINT('Ctrl Pts',(21.5672614103372,-2.38677270581997,-22.7642987979908)) ;
#59766 = CARTESIAN_POINT('Ctrl Pts',(21.5573979860251,-2.31839491120195,-22.7541777671244)) ;
#59767 = CARTESIAN_POINT('Ctrl Pts',(21.5524622513411,-2.28420607311861,-22.749121078891)) ;
#59768 = CARTESIAN_POINT('Ctrl Pts',(21.5450919474027,-2.23321428671612,-22.7415874738631)) ;
#59769 = CARTESIAN_POINT('Ctrl Pts',(21.5426407158965,-2.2162656031082,-22.7390848559396)) ;
#59770 = CARTESIAN_POINT('Ctrl Pts',(21.5377556388623,-2.18251395760228,-22.7341046318056)) ;
#59771 = CARTESIAN_POINT('Ctrl Pts',(21.5353217949764,-2.16571099569641,-22.731627024038)) ;
#59772 = CARTESIAN_POINT('Ctrl Pts',(21.5304774869785,-2.13229935977276,-22.7267049672548)) ;
#59773 = CARTESIAN_POINT('Ctrl Pts',(21.5280670363083,-2.11569068959445,-22.7242605065996)) ;
#59774 = CARTESIAN_POINT('Ctrl Pts',(21.5232749127087,-2.0827162069927,-22.7194134565288)) ;
#59775 = CARTESIAN_POINT('Ctrl Pts',(21.520893274851,-2.06635039436428,-22.7170108338336)) ;
#59776 = CARTESIAN_POINT('Ctrl Pts',(21.5173454918877,-2.04202024585826,-22.7134457449312)) ;
#59777 = CARTESIAN_POINT('Ctrl Pts',(21.516166991437,-2.03394662562764,-22.7122638738618)) ;
#59778 = CARTESIAN_POINT('Ctrl Pts',(21.5138184224543,-2.01787831535676,-22.7099146125519)) ;
#59779 = CARTESIAN_POINT('Ctrl Pts',(21.5126483545181,-2.00988362531201,-22.7087472217466)) ;
#59780 = CARTESIAN_POINT('Ctrl Pts',(21.5103164927178,-1.99397925002019,-22.7064287996602)) ;
#59781 = CARTESIAN_POINT('Ctrl Pts',(21.5091547197619,-1.98606956494765,-22.7052777486237)) ;
#59782 = CARTESIAN_POINT('Ctrl Pts',(21.5074175432658,-1.97427335159223,-22.7035654244297)) ;
#59783 = CARTESIAN_POINT('Ctrl Pts',(21.5068393896569,-1.97035266628625,-22.7029970332676)) ;
#59784 = CARTESIAN_POINT('Ctrl Pts',(21.505684604382,-1.96253482879969,-22.701865508132)) ;
#59785 = CARTESIAN_POINT('Ctrl Pts',(21.5051079740316,-1.95863767660568,-22.7013023729089)) ;
#59786 = CARTESIAN_POINT('Ctrl Pts',(21.5039550260575,-1.95086298073556,-22.7001813879179)) ;
#59787 = CARTESIAN_POINT('Ctrl Pts',(21.5033480898594,-1.94677887060986,-22.6995937411855)) ;
#59788 = CARTESIAN_POINT('Ctrl Pts',(21.5021008358999,-1.93841639885889,-22.6983947735248)) ;
#59789 = CARTESIAN_POINT('Ctrl Pts',(21.5014605711589,-1.93413803655436,-22.6977834021797)) ;
#59790 = CARTESIAN_POINT('Ctrl Pts',(21.500494242935,-1.92772075603282,-22.696872038256)) ;
#59791 = CARTESIAN_POINT('Ctrl Pts',(21.500171134863,-1.92558171961753,-22.6965692125178)) ;
#59792 = CARTESIAN_POINT('Ctrl Pts',(21.4995256901997,-1.92132806844377,-22.695969782032)) ;
#59793 = CARTESIAN_POINT('Ctrl Pts',(21.4992033795886,-1.91921345322948,-22.695673152545)) ;
#59794 = CARTESIAN_POINT('Ctrl Pts',(21.4987220194729,-1.91607808689387,-22.6952366196236)) ;
#59795 = CARTESIAN_POINT('Ctrl Pts',(21.4985619091592,-1.91503906134344,-22.6950925191119)) ;
#59796 = CARTESIAN_POINT('Ctrl Pts',(21.4982424413642,-1.91297624041611,-22.6948079403308)) ;
#59797 = CARTESIAN_POINT('Ctrl Pts',(21.4980830857427,-1.91195244499585,-22.6946674602874)) ;
#59798 = CARTESIAN_POINT('Ctrl Pts',(21.4977648789956,-1.90992312871267,-22.6943912242827)) ;
#59799 = CARTESIAN_POINT('Ctrl Pts',(21.4976060566755,-1.90891760967738,-22.6942554415556)) ;
#59800 = CARTESIAN_POINT('Ctrl Pts',(21.4973673858906,-1.90742533433075,-22.6940567371139)) ;
#59801 = CARTESIAN_POINT('Ctrl Pts',(21.497287749008,-1.90693057691868,-22.6939913374149)) ;
#59802 = CARTESIAN_POINT('Ctrl Pts',(21.4971279262894,-1.90594678686493,-22.6938626876047)) ;
#59803 = CARTESIAN_POINT('Ctrl Pts',(21.4970477579221,-1.90545775357358,-22.6937994207613)) ;
#59804 = CARTESIAN_POINT('Ctrl Pts',(21.4969252943185,-1.90472184931356,-22.6937059447438)) ;
#59805 = CARTESIAN_POINT('Ctrl Pts',(21.4968813058637,-1.9044594724889,-22.6936729256337)) ;
#59806 = CARTESIAN_POINT('Ctrl Pts',(21.4967901442597,-1.90392242639159,-22.6936064049946)) ;
#59807 = CARTESIAN_POINT('Ctrl Pts',(21.4967429748205,-1.90364775693111,-22.693572899898)) ;
#59808 = CARTESIAN_POINT('Ctrl Pts',(21.4966467084668,-1.90309873102656,-22.6935078046084)) ;
#59809 = CARTESIAN_POINT('Ctrl Pts',(21.4965976870603,-1.90282441341568,-22.6934761539446)) ;
#59810 = CARTESIAN_POINT('Ctrl Pts',(21.4963333307451,-1.90163369401068,-22.6933876198957)) ;
#59811 = CARTESIAN_POINT('Ctrl Pts',(21.4963225223461,-1.90158501058727,-22.6933840001171)) ;
#59812 = CARTESIAN_POINT('Ctrl Pts',(21.4963117139471,-1.90153632716387,-22.6933803803385)) ;
#59813 = CARTESIAN_POINT('',(31.5544392045414,-15.0366437072153,-12.5883914509194)) ;
#59814 = CARTESIAN_POINT('',(31.565410601292,-15.0366437072153,-12.5608553214549)) ;
#59815 = CARTESIAN_POINT('Origin',(-1.2689288344947,-21.6462763158693,0.505587457724587)) ;
#59816 = CARTESIAN_POINT('',(29.0382272079201,-1.90153624090668,-11.5698872032838)) ;
#59817 = CARTESIAN_POINT('Ctrl Pts',(29.0382272249795,-1.90153633024293,-11.569887210347)) ;
#59818 = CARTESIAN_POINT('Ctrl Pts',(29.0382341685625,-1.90158488937111,-11.5698968952696)) ;
#59819 = CARTESIAN_POINT('Ctrl Pts',(29.0383534545912,-1.90241910213499,-11.5700632756462)) ;
#59820 = CARTESIAN_POINT('Ctrl Pts',(29.0384211680538,-1.9028192570987,-11.5701167460572)) ;
#59821 = CARTESIAN_POINT('Ctrl Pts',(29.0384685127817,-1.90309246453481,-11.5701504595666)) ;
#59822 = CARTESIAN_POINT('Ctrl Pts',(29.0385642093004,-1.90363926995708,-11.5702155771039)) ;
#59823 = CARTESIAN_POINT('Ctrl Pts',(29.0386125891881,-1.90391282912392,-11.5702468889399)) ;
#59824 = CARTESIAN_POINT('Ctrl Pts',(29.0387077264248,-1.90444770504447,-11.5703067495747)) ;
#59825 = CARTESIAN_POINT('Ctrl Pts',(29.0387544856515,-1.90470902198025,-11.5703352937625)) ;
#59826 = CARTESIAN_POINT('Ctrl Pts',(29.038886093546,-1.90544192358575,-11.5704141835626)) ;
#59827 = CARTESIAN_POINT('Ctrl Pts',(29.0389741666542,-1.90592895120476,-11.5704650586967)) ;
#59828 = CARTESIAN_POINT('Ctrl Pts',(29.0391520824275,-1.9069087065474,-11.5705655502498)) ;
#59829 = CARTESIAN_POINT('Ctrl Pts',(29.039241934173,-1.90740143492223,-11.5706151442418)) ;
#59830 = CARTESIAN_POINT('Ctrl Pts',(29.0395137203389,-1.90888759045901,-11.5707627771257)) ;
#59831 = CARTESIAN_POINT('Ctrl Pts',(29.0396978706761,-1.90988898601723,-11.5708597034774)) ;
#59832 = CARTESIAN_POINT('Ctrl Pts',(29.0400707017281,-1.91190998059807,-11.5710523493246)) ;
#59833 = CARTESIAN_POINT('Ctrl Pts',(29.0402593966093,-1.91292957779318,-11.5711480322448)) ;
#59834 = CARTESIAN_POINT('Ctrl Pts',(29.0406404146295,-1.91498393997969,-11.5713387604754)) ;
#59835 = CARTESIAN_POINT('Ctrl Pts',(29.0408327387316,-1.91601870501465,-11.571433803393)) ;
#59836 = CARTESIAN_POINT('Ctrl Pts',(29.0414140068024,-1.9191412150523,-11.571718320527)) ;
#59837 = CARTESIAN_POINT('Ctrl Pts',(29.0418072264422,-1.92124715973623,-11.57190722504)) ;
#59838 = CARTESIAN_POINT('Ctrl Pts',(29.0425996817526,-1.92548337017848,-11.5722835141449)) ;
#59839 = CARTESIAN_POINT('Ctrl Pts',(29.0429989307614,-1.92761363639261,-11.5724708655146)) ;
#59840 = CARTESIAN_POINT('Ctrl Pts',(29.044198247386,-1.93400460629616,-11.5730290758498)) ;
#59841 = CARTESIAN_POINT('Ctrl Pts',(29.0449998498987,-1.93826542817482,-11.5733961485032)) ;
#59842 = CARTESIAN_POINT('Ctrl Pts',(29.0465687990394,-1.94659361634588,-11.5741082576043)) ;
#59843 = CARTESIAN_POINT('Ctrl Pts',(29.0473361728228,-1.95066098331758,-11.5744532262768)) ;
#59844 = CARTESIAN_POINT('Ctrl Pts',(29.0487981958263,-1.95840366162645,-11.5751067922209)) ;
#59845 = CARTESIAN_POINT('Ctrl Pts',(29.0495316973985,-1.96228469190273,-11.575432736428)) ;
#59846 = CARTESIAN_POINT('Ctrl Pts',(29.0510041256863,-1.97007018824413,-11.5760840936556)) ;
#59847 = CARTESIAN_POINT('Ctrl Pts',(29.0517430530695,-1.9739746543226,-11.5764095050075)) ;
#59848 = CARTESIAN_POINT('Ctrl Pts',(29.0539674538176,-1.98572206873987,-11.577385610067)) ;
#59849 = CARTESIAN_POINT('Ctrl Pts',(29.0554605281726,-1.99359903284624,-11.5780362187396)) ;
#59850 = CARTESIAN_POINT('Ctrl Pts',(29.0584648442791,-2.00943761463625,-11.5793391039616)) ;
#59851 = CARTESIAN_POINT('Ctrl Pts',(29.0599760966161,-2.01739923214533,-11.5799913538457)) ;
#59852 = CARTESIAN_POINT('Ctrl Pts',(29.0630151083938,-2.03340107088851,-11.5812983106997)) ;
#59853 = CARTESIAN_POINT('Ctrl Pts',(29.0645428681356,-2.04144129212701,-11.5819530169154)) ;
#59854 = CARTESIAN_POINT('Ctrl Pts',(29.0691486954484,-2.06567079163896,-11.5839213103865)) ;
#59855 = CARTESIAN_POINT('Ctrl Pts',(29.0722492727184,-2.08196890224857,-11.5852391668774)) ;
#59856 = CARTESIAN_POINT('Ctrl Pts',(29.0784997417023,-2.11480697633052,-11.587886143567)) ;
#59857 = CARTESIAN_POINT('Ctrl Pts',(29.0816496513105,-2.13134694000775,-11.5892152189681)) ;
#59858 = CARTESIAN_POINT('Ctrl Pts',(29.0879887575836,-2.16462035934258,-11.5918827990063)) ;
#59859 = CARTESIAN_POINT('Ctrl Pts',(29.0911779600734,-2.18135381116105,-11.5932212868798)) ;
#59860 = CARTESIAN_POINT('Ctrl Pts',(29.097585914687,-2.21496583380245,-11.5959051228844)) ;
#59861 = CARTESIAN_POINT('Ctrl Pts',(29.1008046676486,-2.2318444046333,-11.597250468916)) ;
#59862 = CARTESIAN_POINT('Ctrl Pts',(29.1104908766021,-2.2826252500142,-11.6012923700042)) ;
#59863 = CARTESIAN_POINT('Ctrl Pts',(29.1169882557135,-2.31667265716275,-11.6039948555289)) ;
#59864 = CARTESIAN_POINT('Ctrl Pts',(29.1299871384566,-2.38476758990642,-11.6093895409454)) ;
#59865 = CARTESIAN_POINT('Ctrl Pts',(29.1364886558516,-2.4188151018372,-11.6120816986642)) ;
#59866 = CARTESIAN_POINT('Ctrl Pts',(29.1494208066684,-2.48652329463723,-11.617427940203)) ;
#59867 = CARTESIAN_POINT('Ctrl Pts',(29.1558514467138,-2.52018397555204,-11.620082007424)) ;
#59868 = CARTESIAN_POINT('Ctrl Pts',(29.1749249846731,-2.62000539185675,-11.6279442948498)) ;
#59869 = CARTESIAN_POINT('Ctrl Pts',(29.1873494574745,-2.68500550045174,-11.633052708379)) ;
#59870 = CARTESIAN_POINT('Ctrl Pts',(29.2121491155211,-2.81472076007776,-11.6432341376143)) ;
#59871 = CARTESIAN_POINT('Ctrl Pts',(29.2251571264759,-2.88274300453423,-11.6485653289196)) ;
#59872 = CARTESIAN_POINT('Ctrl Pts',(29.2512562758467,-3.01919807609263,-11.6592483178059)) ;
#59873 = CARTESIAN_POINT('Ctrl Pts',(29.2643474287702,-3.08763090326719,-11.6646000790163)) ;
#59874 = CARTESIAN_POINT('Ctrl Pts',(29.2906093238418,-3.22489389275181,-11.6753256915392)) ;
#59875 = CARTESIAN_POINT('Ctrl Pts',(29.3037800718641,-3.29372405504827,-11.6806995281003)) ;
#59876 = CARTESIAN_POINT('Ctrl Pts',(29.3301979489162,-3.43176846859418,-11.6914699476084)) ;
#59877 = CARTESIAN_POINT('Ctrl Pts',(29.3434450787023,-3.50098271984707,-11.6968665286563)) ;
#59878 = CARTESIAN_POINT('Ctrl Pts',(29.3832965163599,-3.70918173910975,-11.7130906509313)) ;
#59879 = CARTESIAN_POINT('Ctrl Pts',(29.4100108320053,-3.84872277196881,-11.7239526726309)) ;
#59880 = CARTESIAN_POINT('Ctrl Pts',(29.463710046215,-4.12918225244752,-11.7457666556354)) ;
#59881 = CARTESIAN_POINT('Ctrl Pts',(29.4906949669058,-4.27010070014659,-11.7567185614512)) ;
#59882 = CARTESIAN_POINT('Ctrl Pts',(29.5449136076951,-4.5532090553379,-11.7787078273763)) ;
#59883 = CARTESIAN_POINT('Ctrl Pts',(29.5721473374809,-4.69539896192083,-11.7897451626647)) ;
#59884 = CARTESIAN_POINT('Ctrl Pts',(29.6268422993657,-4.98094427794184,-11.8118995803103)) ;
#59885 = CARTESIAN_POINT('Ctrl Pts',(29.6543035363965,-5.12429968739496,-11.823016650298)) ;
#59886 = CARTESIAN_POINT('Ctrl Pts',(29.7094325037144,-5.41207005497427,-11.8453241087356)) ;
#59887 = CARTESIAN_POINT('Ctrl Pts',(29.7371002364177,-5.55648501309814,-11.8565144911195)) ;
#59888 = CARTESIAN_POINT('Ctrl Pts',(29.7926213687897,-5.84626852432184,-11.8789616873085)) ;
#59889 = CARTESIAN_POINT('Ctrl Pts',(29.8204747688937,-5.991637077423,-11.8902185000195)) ;
#59890 = CARTESIAN_POINT('Ctrl Pts',(29.9042824088571,-6.42901419915437,-11.92407780665)) ;
#59891 = CARTESIAN_POINT('Ctrl Pts',(29.9604840591669,-6.72229422551734,-11.9467692397323)) ;
#59892 = CARTESIAN_POINT('Ctrl Pts',(30.073382389645,-7.31139720219581,-11.9923294645172)) ;
#59893 = CARTESIAN_POINT('Ctrl Pts',(30.1300790840833,-7.60722015254495,-12.0151982204241)) ;
#59894 = CARTESIAN_POINT('Ctrl Pts',(30.2438035110593,-8.200561345854,-12.0610514214145)) ;
#59895 = CARTESIAN_POINT('Ctrl Pts',(30.3008312506642,-8.49807958881067,-12.0840358487589)) ;
#59896 = CARTESIAN_POINT('Ctrl Pts',(30.4150541835392,-9.09396373680619,-12.1300577013257)) ;
#59897 = CARTESIAN_POINT('Ctrl Pts',(30.4722493801187,-9.39232964185194,-12.1530951182446)) ;
#59898 = CARTESIAN_POINT('Ctrl Pts',(30.6438411606855,-10.2874274051715,-12.2221918581039)) ;
#59899 = CARTESIAN_POINT('Ctrl Pts',(30.7582438742163,-10.8841592962013,-12.2682358153304)) ;
#59900 = CARTESIAN_POINT('Ctrl Pts',(30.9857608719517,-12.0708421120912,-12.3597714289845)) ;
#59901 = CARTESIAN_POINT('Ctrl Pts',(31.0988751847915,-12.6607930370028,-12.4052630135689)) ;
#59902 = CARTESIAN_POINT('Ctrl Pts',(31.3225120133624,-13.8271328594513,-12.4951790207671)) ;
#59903 = CARTESIAN_POINT('Ctrl Pts',(31.4373907777609,-14.4262400706049,-12.5413543921016)) ;
#59904 = CARTESIAN_POINT('Ctrl Pts',(31.5501658085507,-15.0143581153283,-12.5866741590384)) ;
#59905 = CARTESIAN_POINT('Ctrl Pts',(31.554439204467,-15.0366437072152,-12.5883914511059)) ;
#59906 = CARTESIAN_POINT('Ctrl Pts',(31.565410601367,-15.0366437072152,-12.5608553212663)) ;
#59907 = CARTESIAN_POINT('Ctrl Pts',(31.561127154397,-15.0143581154633,-12.5591632555168)) ;
#59908 = CARTESIAN_POINT('Ctrl Pts',(31.5568406253047,-14.9920565142548,-12.5574699867564)) ;
#59909 = CARTESIAN_POINT('Ctrl Pts',(31.4437198542653,-14.403521757529,-12.5127852997407)) ;
#59910 = CARTESIAN_POINT('Ctrl Pts',(31.3329303683987,-13.8271328601355,-12.4690309217221)) ;
#59911 = CARTESIAN_POINT('Ctrl Pts',(31.1087358495905,-12.6607930379712,-12.3805146116334)) ;
#59912 = CARTESIAN_POINT('Ctrl Pts',(30.9953308303239,-12.0708421132033,-12.335752645243)) ;
#59913 = CARTESIAN_POINT('Ctrl Pts',(30.767205523712,-10.8841592976026,-12.2457437719057)) ;
#59914 = CARTESIAN_POINT('Ctrl Pts',(30.6524852649845,-10.2874274067182,-12.2004967931075)) ;
#59915 = CARTESIAN_POINT('Ctrl Pts',(30.4803926152741,-9.39232964361678,-12.1326571401289)) ;
#59916 = CARTESIAN_POINT('Ctrl Pts',(30.4230263412627,-9.09396373864371,-12.1100490952274)) ;
#59917 = CARTESIAN_POINT('Ctrl Pts',(30.3084518038435,-8.49807959079342,-12.064909703605)) ;
#59918 = CARTESIAN_POINT('Ctrl Pts',(30.2512435437427,-8.20056134790925,-12.0423783485818)) ;
#59919 = CARTESIAN_POINT('Ctrl Pts',(30.1371469009566,-7.60722015474479,-11.9974593389122)) ;
#59920 = CARTESIAN_POINT('Ctrl Pts',(30.0802585253396,-7.31139720446773,-11.9750716665277)) ;
#59921 = CARTESIAN_POINT('Ctrl Pts',(29.9669631044646,-6.72229422793283,-11.9305080635682)) ;
#59922 = CARTESIAN_POINT('Ctrl Pts',(29.9105560734644,-6.42901420164131,-11.9083320971897)) ;
#59923 = CARTESIAN_POINT('Ctrl Pts',(29.8264270778358,-5.99163708001652,-11.8752793325204)) ;
#59924 = CARTESIAN_POINT('Ctrl Pts',(29.7984643309233,-5.84626852695081,-11.8642969596244)) ;
#59925 = CARTESIAN_POINT('Ctrl Pts',(29.7427193144565,-5.55648501579772,-11.842411670182)) ;
#59926 = CARTESIAN_POINT('Ctrl Pts',(29.714937045338,-5.41207005770904,-11.8315087525432)) ;
#59927 = CARTESIAN_POINT('Ctrl Pts',(29.6595728365084,-5.12429969019985,-11.8097917058187)) ;
#59928 = CARTESIAN_POINT('Ctrl Pts',(29.6319908992134,-4.98094428078168,-11.7989775706709)) ;
#59929 = CARTESIAN_POINT('Ctrl Pts',(29.5770470224415,-4.69539896483025,-11.7774478823226)) ;
#59930 = CARTESIAN_POINT('Ctrl Pts',(29.549685087891,-4.55320905828197,-11.7667323167496)) ;
#59931 = CARTESIAN_POINT('Ctrl Pts',(29.4952005928358,-4.27010070315964,-11.7454102947565)) ;
#59932 = CARTESIAN_POINT('Ctrl Pts',(29.468078042368,-4.12918225549492,-11.7348038136532)) ;
#59933 = CARTESIAN_POINT('Ctrl Pts',(29.4140911906375,-3.84872277508455,-11.7137117464274)) ;
#59934 = CARTESIAN_POINT('Ctrl Pts',(29.3872269114725,-3.70918174225949,-11.7032261047998)) ;
#59935 = CARTESIAN_POINT('Ctrl Pts',(29.3471376272874,-3.50098272304754,-11.6875989323238)) ;
#59936 = CARTESIAN_POINT('Ctrl Pts',(29.3338090449177,-3.43176847181153,-11.6824067818549)) ;
#59937 = CARTESIAN_POINT('Ctrl Pts',(29.307222973611,-3.29372405829925,-11.6720584981133)) ;
#59938 = CARTESIAN_POINT('Ctrl Pts',(29.2939654854284,-3.22489389601956,-11.6669023629481)) ;
#59939 = CARTESIAN_POINT('Ctrl Pts',(29.2675234700757,-3.08763090656839,-11.6566288182608)) ;
#59940 = CARTESIAN_POINT('Ctrl Pts',(29.2543389487858,-3.01919807941051,-11.6515113939891)) ;
#59941 = CARTESIAN_POINT('Ctrl Pts',(29.2280443983299,-2.88274300788535,-11.6413188248645)) ;
#59942 = CARTESIAN_POINT('Ctrl Pts',(29.2149343836421,-2.81472076344547,-11.6362436436338)) ;
#59943 = CARTESIAN_POINT('Ctrl Pts',(29.1899281802654,-2.68500550351773,-11.626580603919)) ;
#59944 = CARTESIAN_POINT('Ctrl Pts',(29.1773950157388,-2.62000539458853,-11.621744985863)) ;
#59945 = CARTESIAN_POINT('Ctrl Pts',(29.1581408222584,-2.52018397777059,-11.614336109319)) ;
#59946 = CARTESIAN_POINT('Ctrl Pts',(29.1516470059532,-2.48652329668272,-11.611840602457)) ;
#59947 = CARTESIAN_POINT('Ctrl Pts',(29.1385817152791,-2.41881510353456,-11.6068285165685)) ;
#59948 = CARTESIAN_POINT('Ctrl Pts',(29.132010247518,-2.38476759142876,-11.6043119209325)) ;
#59949 = CARTESIAN_POINT('Ctrl Pts',(29.1188631949375,-2.31667265833498,-11.5992891135706)) ;
#59950 = CARTESIAN_POINT('Ctrl Pts',(29.1122876291262,-2.2826252510114,-11.5967828617679)) ;
#59951 = CARTESIAN_POINT('Ctrl Pts',(29.1024758718508,-2.2318444053694,-11.5930560630614)) ;
#59952 = CARTESIAN_POINT('Ctrl Pts',(29.0992138779589,-2.21496583445174,-11.591819243533)) ;
#59953 = CARTESIAN_POINT('Ctrl Pts',(29.0927160591955,-2.18135381163753,-11.5893609494406)) ;
#59954 = CARTESIAN_POINT('Ctrl Pts',(29.0894802351616,-2.16462035973303,-11.5881394727713)) ;
#59955 = CARTESIAN_POINT('Ctrl Pts',(29.0830435792027,-2.13134694022715,-11.5857167238876)) ;
#59956 = CARTESIAN_POINT('Ctrl Pts',(29.0798427545775,-2.11480697646486,-11.5845154354957)) ;
#59957 = CARTESIAN_POINT('Ctrl Pts',(29.0734846178031,-2.08196890221408,-11.5821386844894)) ;
#59958 = CARTESIAN_POINT('Ctrl Pts',(29.0703273234694,-2.0656707915207,-11.5809631770477)) ;
#59959 = CARTESIAN_POINT('Ctrl Pts',(29.0656299192246,-2.0414412918842,-11.579224724275)) ;
#59960 = CARTESIAN_POINT('Ctrl Pts',(29.0640705314266,-2.03340107060426,-11.5786493984716)) ;
#59961 = CARTESIAN_POINT('Ctrl Pts',(29.060965429039,-2.01739923177882,-11.5775083164946)) ;
#59962 = CARTESIAN_POINT('Ctrl Pts',(29.059419714753,-2.00943761422882,-11.5769425595576)) ;
#59963 = CARTESIAN_POINT('Ctrl Pts',(29.0563426013253,-1.99359903235739,-11.5758223817893)) ;
#59964 = CARTESIAN_POINT('Ctrl Pts',(29.0548112128256,-1.98572206821069,-11.575267934346)) ;
#59965 = CARTESIAN_POINT('Ctrl Pts',(29.0525250409775,-1.97397465373301,-11.5744468630235)) ;
#59966 = CARTESIAN_POINT('Ctrl Pts',(29.0517647978228,-1.9700701876343,-11.5741749502126)) ;
#59967 = CARTESIAN_POINT('Ctrl Pts',(29.0502478835027,-1.96228469125286,-11.5736352444845)) ;
#59968 = CARTESIAN_POINT('Ctrl Pts',(29.049491213007,-1.95840366095669,-11.5733674498795)) ;
#59969 = CARTESIAN_POINT('Ctrl Pts',(29.0479803339922,-1.9506609828574,-11.5728365033947)) ;
#59970 = CARTESIAN_POINT('Ctrl Pts',(29.0471859893661,-1.94659361612655,-11.5725592265675)) ;
#59971 = CARTESIAN_POINT('Ctrl Pts',(29.0455572224161,-1.93826542844876,-11.5719972491222)) ;
#59972 = CARTESIAN_POINT('Ctrl Pts',(29.0447228269808,-1.93400460682272,-11.5717124806397)) ;
#59973 = CARTESIAN_POINT('Ctrl Pts',(29.0434682476483,-1.92761363729763,-11.5712929694538)) ;
#59974 = CARTESIAN_POINT('Ctrl Pts',(29.0430495532631,-1.92548337120945,-11.5711544223689)) ;
#59975 = CARTESIAN_POINT('Ctrl Pts',(29.0422154605149,-1.9212471610181,-11.5708826354932)) ;
#59976 = CARTESIAN_POINT('Ctrl Pts',(29.041800075323,-1.91914121645887,-11.5707493623905)) ;
#59977 = CARTESIAN_POINT('Ctrl Pts',(29.0411824150817,-1.91601870660613,-11.5705561828204)) ;
#59978 = CARTESIAN_POINT('Ctrl Pts',(29.04097742769,-1.91498394163286,-11.5704929223976)) ;
#59979 = CARTESIAN_POINT('Ctrl Pts',(29.0405696466495,-1.91292957956788,-11.5703693643508)) ;
#59980 = CARTESIAN_POINT('Ctrl Pts',(29.0403668539521,-1.91190998243237,-11.5703090643144)) ;
#59981 = CARTESIAN_POINT('Ctrl Pts',(29.0399636978678,-1.90988898797118,-11.5701925286259)) ;
#59982 = CARTESIAN_POINT('Ctrl Pts',(29.0397633493576,-1.90888759247266,-11.5701362566561)) ;
#59983 = CARTESIAN_POINT('Ctrl Pts',(29.0394645067919,-1.90740143702365,-11.5700565302644)) ;
#59984 = CARTESIAN_POINT('Ctrl Pts',(29.039365169076,-1.9069087086778,-11.5700307442789)) ;
#59985 = CARTESIAN_POINT('Ctrl Pts',(29.0391668950545,-1.90592895339284,-11.5699813481084)) ;
#59986 = CARTESIAN_POINT('Ctrl Pts',(29.0390679675556,-1.90544192580431,-11.5699577154576)) ;
#59987 = CARTESIAN_POINT('Ctrl Pts',(29.03891816831,-1.9047090240292,-11.5699244824112)) ;
#59988 = CARTESIAN_POINT('Ctrl Pts',(29.0388645915097,-1.90444770688011,-11.569913048924)) ;
#59989 = CARTESIAN_POINT('Ctrl Pts',(29.0387543560926,-1.90391283053387,-11.5698910816268)) ;
#59990 = CARTESIAN_POINT('Ctrl Pts',(29.0386976993307,-1.90363927114993,-11.5698805430576)) ;
#59991 = CARTESIAN_POINT('Ctrl Pts',(29.0385834427038,-1.90309246529325,-11.5698620076366)) ;
#59992 = CARTESIAN_POINT('Ctrl Pts',(29.0385258858671,-1.90281925763486,-11.5698539244633)) ;
#59993 = CARTESIAN_POINT('Ctrl Pts',(29.0382498911084,-1.90163369484209,-11.5698846841972)) ;
#59994 = CARTESIAN_POINT('Ctrl Pts',(29.038238558044,-1.90158501254251,-11.5698859472721)) ;
#59995 = CARTESIAN_POINT('Ctrl Pts',(29.0382272249795,-1.90153633024293,-11.569887210347)) ;
#59996 = CARTESIAN_POINT('',(33.9237617799844,-15.0366437072151,1.82445047330668)) ;
#59997 = CARTESIAN_POINT('',(33.9221570292818,-15.0366437072151,1.85404835843738)) ;
#59998 = CARTESIAN_POINT('Origin',(-1.36393928288321,-21.6462763158694,-0.073950639135127)) ;
#59999 = CARTESIAN_POINT('',(31.2124507878034,-1.90153624155895,1.69228989918397)) ;
#60000 = CARTESIAN_POINT('Ctrl Pts',(31.2124508063865,-1.90153633154746,1.69228989994415)) ;
#60001 = CARTESIAN_POINT('Ctrl Pts',(31.212461175561,-1.90158488722844,1.69228399858286)) ;
#60002 = CARTESIAN_POINT('Ctrl Pts',(31.2126377175942,-1.90241157971636,1.6921835240153)) ;
#60003 = CARTESIAN_POINT('Ctrl Pts',(31.2127209037029,-1.90280827097885,1.69216349692496)) ;
#60004 = CARTESIAN_POINT('Ctrl Pts',(31.2127775376793,-1.90307911546552,1.69215281262026)) ;
#60005 = CARTESIAN_POINT('Ctrl Pts',(31.2128907504375,-1.90362119469672,1.69213395170716)) ;
#60006 = CARTESIAN_POINT('Ctrl Pts',(31.2129473160421,-1.90389239066645,1.69212587012815)) ;
#60007 = CARTESIAN_POINT('Ctrl Pts',(31.2130578371091,-1.90442264746974,1.69211152595285)) ;
#60008 = CARTESIAN_POINT('Ctrl Pts',(31.2131117923418,-1.90468170848452,1.69210526828505)) ;
#60009 = CARTESIAN_POINT('Ctrl Pts',(31.213263036536,-1.90540821834563,1.69208896765253)) ;
#60010 = CARTESIAN_POINT('Ctrl Pts',(31.2133634468165,-1.90589097623944,1.69207979306088)) ;
#60011 = CARTESIAN_POINT('Ctrl Pts',(31.2135653350542,-1.90686214240077,1.69206332035544)) ;
#60012 = CARTESIAN_POINT('Ctrl Pts',(31.2136668118428,-1.90735055131874,1.69205604627652)) ;
#60013 = CARTESIAN_POINT('Ctrl Pts',(31.2139727705461,-1.90882367886906,1.6920361944457)) ;
#60014 = CARTESIAN_POINT('Ctrl Pts',(31.2141787825174,-1.90981629627927,1.69202554768393)) ;
#60015 = CARTESIAN_POINT('Ctrl Pts',(31.2145943792177,-1.91181957543587,1.69200723738784)) ;
#60016 = CARTESIAN_POINT('Ctrl Pts',(31.2148039614514,-1.91283023535738,1.69199961290675)) ;
#60017 = CARTESIAN_POINT('Ctrl Pts',(31.215226124221,-1.91486659038896,1.69198645586192)) ;
#60018 = CARTESIAN_POINT('Ctrl Pts',(31.2154387046288,-1.91589228554187,1.69198092582033)) ;
#60019 = CARTESIAN_POINT('Ctrl Pts',(31.2160800554371,-1.91898742680707,1.69196668346609)) ;
#60020 = CARTESIAN_POINT('Ctrl Pts',(31.2165124347933,-1.92107491347353,1.69196027231138)) ;
#60021 = CARTESIAN_POINT('Ctrl Pts',(31.2173819724023,-1.92527399569929,1.6919513369368)) ;
#60022 = CARTESIAN_POINT('Ctrl Pts',(31.2178191288148,-1.92738559171555,1.69194884840311)) ;
#60023 = CARTESIAN_POINT('Ctrl Pts',(31.2191304096143,-1.93372055099077,1.6919455119432)) ;
#60024 = CARTESIAN_POINT('Ctrl Pts',(31.2200043381773,-1.93794403242011,1.69194872685841)) ;
#60025 = CARTESIAN_POINT('Ctrl Pts',(31.2217122048351,-1.94619923694316,1.69196075730605)) ;
#60026 = CARTESIAN_POINT('Ctrl Pts',(31.222546139137,-1.95023096071567,1.6919696453857)) ;
#60027 = CARTESIAN_POINT('Ctrl Pts',(31.2241333801421,-1.95790548260028,1.69198990256225)) ;
#60028 = CARTESIAN_POINT('Ctrl Pts',(31.2249288593706,-1.96175219546279,1.69200182885001)) ;
#60029 = CARTESIAN_POINT('Ctrl Pts',(31.226524476387,-1.96946884984108,1.69202842779924)) ;
#60030 = CARTESIAN_POINT('Ctrl Pts',(31.2273246140806,-1.97333879137023,1.69204310224879)) ;
#60031 = CARTESIAN_POINT('Ctrl Pts',(31.2297318261205,-1.98498233146023,1.69209042504112)) ;
#60032 = CARTESIAN_POINT('Ctrl Pts',(31.2313457018942,-1.99278964510905,1.6921263257119)) ;
#60033 = CARTESIAN_POINT('Ctrl Pts',(31.2345904888783,-2.0084881776274,1.69220421002999)) ;
#60034 = CARTESIAN_POINT('Ctrl Pts',(31.2362213985065,-2.01637939632246,1.69224622219019)) ;
#60035 = CARTESIAN_POINT('Ctrl Pts',(31.2394990884388,-2.03223974253541,1.69233492278662)) ;
#60036 = CARTESIAN_POINT('Ctrl Pts',(31.2411458686997,-2.04020887005775,1.69238161202648)) ;
#60037 = CARTESIAN_POINT('Ctrl Pts',(31.2461082290652,-2.06422412624885,1.69252732779402)) ;
#60038 = CARTESIAN_POINT('Ctrl Pts',(31.2494458335295,-2.08037812508227,1.69263190102892)) ;
#60039 = CARTESIAN_POINT('Ctrl Pts',(31.2561700891972,-2.11292583745181,1.69285147290656)) ;
#60040 = CARTESIAN_POINT('Ctrl Pts',(31.2595567378426,-2.12931955119283,1.69296651950916)) ;
#60041 = CARTESIAN_POINT('Ctrl Pts',(31.2663692987432,-2.16229876012589,1.69320450644542)) ;
#60042 = CARTESIAN_POINT('Ctrl Pts',(31.2697952092503,-2.17888425147949,1.6933274643675)) ;
#60043 = CARTESIAN_POINT('Ctrl Pts',(31.2766764656943,-2.21219907029455,1.69357952704175)) ;
#60044 = CARTESIAN_POINT('Ctrl Pts',(31.2801318115104,-2.22892839776393,1.69370863404421)) ;
#60045 = CARTESIAN_POINT('Ctrl Pts',(31.2905272293254,-2.27926023016279,1.69410317044972)) ;
#60046 = CARTESIAN_POINT('Ctrl Pts',(31.2974966855476,-2.31300658479306,1.69437574300689)) ;
#60047 = CARTESIAN_POINT('Ctrl Pts',(31.3114350251233,-2.38049941248962,1.69493190615983)) ;
#60048 = CARTESIAN_POINT('Ctrl Pts',(31.3184039032708,-2.41424587189324,1.69521554061887)) ;
#60049 = CARTESIAN_POINT('Ctrl Pts',(31.332262048329,-2.48135538068444,1.69578759918834)) ;
#60050 = CARTESIAN_POINT('Ctrl Pts',(31.3391513142871,-2.51471843011748,1.69607604104233)) ;
#60051 = CARTESIAN_POINT('Ctrl Pts',(31.3595810816876,-2.61365721512364,1.69694041210369)) ;
#60052 = CARTESIAN_POINT('Ctrl Pts',(31.3728835588276,-2.67808258704843,1.69751527163408)) ;
#60053 = CARTESIAN_POINT('Ctrl Pts',(31.3994174846424,-2.80659298449379,1.69867586291107)) ;
#60054 = CARTESIAN_POINT('Ctrl Pts',(31.4133256032471,-2.87395568035031,1.69929267964525)) ;
#60055 = CARTESIAN_POINT('Ctrl Pts',(31.4412251194173,-3.00908767377159,1.70054240363067)) ;
#60056 = CARTESIAN_POINT('Ctrl Pts',(31.455216514895,-3.07685697140873,1.70117534966788)) ;
#60057 = CARTESIAN_POINT('Ctrl Pts',(31.4832800222044,-3.21278904930444,1.70245451856394)) ;
#60058 = CARTESIAN_POINT('Ctrl Pts',(31.4973521331798,-3.28095182954947,1.70310075716268)) ;
#60059 = CARTESIAN_POINT('Ctrl Pts',(31.5255744612477,-3.41765775489871,1.70440458104699)) ;
#60060 = CARTESIAN_POINT('Ctrl Pts',(31.5397246782305,-3.4862009000063,1.70506216835304)) ;
#60061 = CARTESIAN_POINT('Ctrl Pts',(31.5822885313072,-3.69238120731966,1.70704982916459)) ;
#60062 = CARTESIAN_POINT('Ctrl Pts',(31.6108153752653,-3.83056924086275,1.70839469325321)) ;
#60063 = CARTESIAN_POINT('Ctrl Pts',(31.668149650939,-4.10830936735011,1.71111617408425)) ;
#60064 = CARTESIAN_POINT('Ctrl Pts',(31.6969570794573,-4.24786146037364,1.71249285009703)) ;
#60065 = CARTESIAN_POINT('Ctrl Pts',(31.7548310815494,-4.52822477818846,1.7152729122382)) ;
#60066 = CARTESIAN_POINT('Ctrl Pts',(31.7838976535024,-4.66903600207234,1.7166763247973)) ;
#60067 = CARTESIAN_POINT('Ctrl Pts',(31.8422684285719,-4.95181265200927,1.71950612302232)) ;
#60068 = CARTESIAN_POINT('Ctrl Pts',(31.8715726309751,-5.09377807807733,1.72093252190176)) ;
#60069 = CARTESIAN_POINT('Ctrl Pts',(31.9303971118103,-5.37875820553491,1.72380532693214)) ;
#60070 = CARTESIAN_POINT('Ctrl Pts',(31.9599173898905,-5.52177290692212,1.72525173956014)) ;
#60071 = CARTESIAN_POINT('Ctrl Pts',(32.0191524404763,-5.80874665865466,1.72816209630444)) ;
#60072 = CARTESIAN_POINT('Ctrl Pts',(32.048867212918,-5.95270570900133,1.72962604159107)) ;
#60073 = CARTESIAN_POINT('Ctrl Pts',(32.138270873612,-6.38584199444269,1.73404093995574)) ;
#60074 = CARTESIAN_POINT('Ctrl Pts',(32.1982191083803,-6.67627835925047,1.73701487958215)) ;
#60075 = CARTESIAN_POINT('Ctrl Pts',(32.3186342423773,-7.25966935677229,1.74300929128555)) ;
#60076 = CARTESIAN_POINT('Ctrl Pts',(32.3791011395381,-7.55262398951995,1.74602980162912)) ;
#60077 = CARTESIAN_POINT('Ctrl Pts',(32.5003805641629,-8.14021211025548,1.75210457488547)) ;
#60078 = CARTESIAN_POINT('Ctrl Pts',(32.5611930905981,-8.43484559824006,1.75515885676166)) ;
#60079 = CARTESIAN_POINT('Ctrl Pts',(32.6829906805412,-9.02495201759556,1.76128948583913)) ;
#60080 = CARTESIAN_POINT('Ctrl Pts',(32.7439757435688,-9.3204249489734,1.76436584192077)) ;
#60081 = CARTESIAN_POINT('Ctrl Pts',(32.9269300423157,-10.2068437912566,1.77361151529095)) ;
#60082 = CARTESIAN_POINT('Ctrl Pts',(33.0488983929961,-10.7977897348994,1.77979728107415)) ;
#60083 = CARTESIAN_POINT('Ctrl Pts',(33.2914474187023,-11.9729664053665,1.79212964973308)) ;
#60084 = CARTESIAN_POINT('Ctrl Pts',(33.4120280895723,-12.5571971322423,1.79827632943994)) ;
#60085 = CARTESIAN_POINT('Ctrl Pts',(33.650416233567,-13.7122280573775,1.81045128027227)) ;
#60086 = CARTESIAN_POINT('Ctrl Pts',(33.7682237047013,-14.2830282556339,1.81647958809695)) ;
#60087 = CARTESIAN_POINT('Ctrl Pts',(33.8972495735035,-14.9081862858531,1.82309151287019)) ;
#60088 = CARTESIAN_POINT('Ctrl Pts',(33.9105199299277,-14.9724840415154,1.82377166717193)) ;
#60089 = CARTESIAN_POINT('Ctrl Pts',(33.9237617800355,-15.0366437072146,1.82445047235355)) ;
#60090 = CARTESIAN_POINT('Ctrl Pts',(33.9221570292296,-15.0366437072146,1.85404835939107)) ;
#60091 = CARTESIAN_POINT('Ctrl Pts',(33.908919411658,-14.972484041484,1.8532914895515)) ;
#60092 = CARTESIAN_POINT('Ctrl Pts',(33.8956533090097,-14.9081862857901,1.85253287884846)) ;
#60093 = CARTESIAN_POINT('Ctrl Pts',(33.7666689205491,-14.2830282555071,1.84515589394836)) ;
#60094 = CARTESIAN_POINT('Ctrl Pts',(33.6489002671268,-13.7122280572179,1.83841163542848)) ;
#60095 = CARTESIAN_POINT('Ctrl Pts',(33.4105932208991,-12.5571971320165,1.82474092404397)) ;
#60096 = CARTESIAN_POINT('Ctrl Pts',(33.2900548261047,-11.9729664051072,1.81781450787719)) ;
#60097 = CARTESIAN_POINT('Ctrl Pts',(33.0475942695711,-10.7977897345726,1.8038504210827)) ;
#60098 = CARTESIAN_POINT('Ctrl Pts',(32.9256721036565,-10.2068437908959,1.7968128272885)) ;
#60099 = CARTESIAN_POINT('Ctrl Pts',(32.7427906577076,-9.32042494856183,1.78622346292756)) ;
#60100 = CARTESIAN_POINT('Ctrl Pts',(32.6818304791294,-9.02495201716702,1.78268814012078)) ;
#60101 = CARTESIAN_POINT('Ctrl Pts',(32.5600840342718,-8.43484559777765,1.77561419531639)) ;
#60102 = CARTESIAN_POINT('Ctrl Pts',(32.49929776751,-8.14021210977616,1.77207558219994)) ;
#60103 = CARTESIAN_POINT('Ctrl Pts',(32.37807248954,-7.55262398900691,1.76500213252937)) ;
#60104 = CARTESIAN_POINT('Ctrl Pts',(32.3176334773044,-7.25966935624243,1.76146731493739)) ;
#60105 = CARTESIAN_POINT('Ctrl Pts',(32.1972761120659,-6.67627835868714,1.75440742105084)) ;
#60106 = CARTESIAN_POINT('Ctrl Pts',(32.1373577569814,-6.38584199386269,1.75088238301948)) ;
#60107 = CARTESIAN_POINT('Ctrl Pts',(32.0480008498943,-5.95270570839647,1.7456051650227)) ;
#60108 = CARTESIAN_POINT('Ctrl Pts',(32.0183019863929,-5.80874665804157,1.74384779656639)) ;
#60109 = CARTESIAN_POINT('Ctrl Pts',(31.9590995092937,-5.52177290629252,1.74033665714888)) ;
#60110 = CARTESIAN_POINT('Ctrl Pts',(31.9295958956328,-5.37875820489711,1.73858288736032)) ;
#60111 = CARTESIAN_POINT('Ctrl Pts',(31.8708056415613,-5.09377807742317,1.73507880675721)) ;
#60112 = CARTESIAN_POINT('Ctrl Pts',(31.8415190008,-4.95181265134699,1.73332850242113)) ;
#60113 = CARTESIAN_POINT('Ctrl Pts',(31.7831844427051,-4.66903600139383,1.72983072134243)) ;
#60114 = CARTESIAN_POINT('Ctrl Pts',(31.7541365246517,-4.52822477750184,1.72808325781884)) ;
#60115 = CARTESIAN_POINT('Ctrl Pts',(31.6963012048463,-4.24786145967095,1.72458974281748)) ;
#60116 = CARTESIAN_POINT('Ctrl Pts',(31.6675138018479,-4.10830936663942,1.72284371779161)) ;
#60117 = CARTESIAN_POINT('Ctrl Pts',(31.6102213783154,-3.83056924013612,1.71935031957733)) ;
#60118 = CARTESIAN_POINT('Ctrl Pts',(31.5817163545517,-3.69238120658509,1.71760300565428)) ;
#60119 = CARTESIAN_POINT('Ctrl Pts',(31.5391871086669,-3.48620089925991,1.71497705269782)) ;
#60120 = CARTESIAN_POINT('Ctrl Pts',(31.5250487431677,-3.41765775414836,1.71410087762607)) ;
#60121 = CARTESIAN_POINT('Ctrl Pts',(31.4968508874359,-3.28095182879129,1.71234568803049)) ;
#60122 = CARTESIAN_POINT('Ctrl Pts',(31.4827913970942,-3.21278904854235,1.71146667552467)) ;
#60123 = CARTESIAN_POINT('Ctrl Pts',(31.45475409678,-3.07685697063884,1.70970414701375)) ;
#60124 = CARTESIAN_POINT('Ctrl Pts',(31.4407762859572,-3.00908767299782,1.70882064674741)) ;
#60125 = CARTESIAN_POINT('Ctrl Pts',(31.4129051990138,-2.87395567956879,1.70704657649424)) ;
#60126 = CARTESIAN_POINT('Ctrl Pts',(31.3990119207755,-2.8065929837084,1.70615604529268)) ;
#60127 = CARTESIAN_POINT('Ctrl Pts',(31.3725080560023,-2.67808258636586,1.70444101112125)) ;
#60128 = CARTESIAN_POINT('Ctrl Pts',(31.3592214053287,-2.61365721455308,1.70357425002237)) ;
#60129 = CARTESIAN_POINT('Ctrl Pts',(31.3388179431848,-2.51471842971896,1.70222470770763)) ;
#60130 = CARTESIAN_POINT('Ctrl Pts',(31.3319378763602,-2.48135538034391,1.70176659804155)) ;
#60131 = CARTESIAN_POINT('Ctrl Pts',(31.3180991179551,-2.41424587166938,1.7008369741399)) ;
#60132 = CARTESIAN_POINT('Ctrl Pts',(31.3111404254024,-2.3804994123244,1.70036547766291)) ;
#60133 = CARTESIAN_POINT('Ctrl Pts',(31.2972236611806,-2.31300658474519,1.69941138097162)) ;
#60134 = CARTESIAN_POINT('Ctrl Pts',(31.290265589944,-2.27926023017359,1.69892882493465)) ;
#60135 = CARTESIAN_POINT('Ctrl Pts',(31.2798884536427,-2.22892839786223,1.69819710618152)) ;
#60136 = CARTESIAN_POINT('Ctrl Pts',(31.276439404296,-2.21219907042198,1.69795186774684)) ;
#60137 = CARTESIAN_POINT('Ctrl Pts',(31.2695712333151,-2.17888425166482,1.69745845812796)) ;
#60138 = CARTESIAN_POINT('Ctrl Pts',(31.2661521115581,-2.16229876034004,1.697210289186)) ;
#60139 = CARTESIAN_POINT('Ctrl Pts',(31.2593537552793,-2.12931955146433,1.69671031363605)) ;
#60140 = CARTESIAN_POINT('Ctrl Pts',(31.255974520594,-2.11292583775185,1.69645852469451)) ;
#60141 = CARTESIAN_POINT('Ctrl Pts',(31.2492659429168,-2.08037812543891,1.69594978951167)) ;
#60142 = CARTESIAN_POINT('Ctrl Pts',(31.2459365972835,-2.06422412663359,1.69569289121035)) ;
#60143 = CARTESIAN_POINT('Ctrl Pts',(31.2409875718499,-2.04020887048424,1.69530122725515)) ;
#60144 = CARTESIAN_POINT('Ctrl Pts',(31.2393453970935,-2.03223974297573,1.69516959453648)) ;
#60145 = CARTESIAN_POINT('Ctrl Pts',(31.2360773309043,-2.01637939679035,1.69490339454841)) ;
#60146 = CARTESIAN_POINT('Ctrl Pts',(31.2344514394269,-2.00848817810898,1.69476882809305)) ;
#60147 = CARTESIAN_POINT('Ctrl Pts',(31.2312172527528,-1.99278964561794,1.69449543266551)) ;
#60148 = CARTESIAN_POINT('Ctrl Pts',(31.2296089560453,-1.98498233198264,1.69435663222621)) ;
#60149 = CARTESIAN_POINT('Ctrl Pts',(31.2272107386957,-1.97333879191288,1.69414341220993)) ;
#60150 = CARTESIAN_POINT('Ctrl Pts',(31.2264137048588,-1.96946885039057,1.69407149051786)) ;
#60151 = CARTESIAN_POINT('Ctrl Pts',(31.2248245655682,-1.96175219602569,1.69392541699786)) ;
#60152 = CARTESIAN_POINT('Ctrl Pts',(31.2240324600155,-1.95790548316983,1.69385126694658)) ;
#60153 = CARTESIAN_POINT('Ctrl Pts',(31.2224523333459,-1.95023096151237,1.69369979443971)) ;
#60154 = CARTESIAN_POINT('Ctrl Pts',(31.2216223266799,-1.94619923797133,1.69361846626251)) ;
#60155 = CARTESIAN_POINT('Ctrl Pts',(31.219923170987,-1.93794403392222,1.69344577332982)) ;
#60156 = CARTESIAN_POINT('Ctrl Pts',(31.2190540178856,-1.93372055273508,1.69335448113254)) ;
#60157 = CARTESIAN_POINT('Ctrl Pts',(31.2177507846797,-1.9273855938235,1.69320938984938)) ;
#60158 = CARTESIAN_POINT('Ctrl Pts',(31.2173164599791,-1.92527399792839,1.69315965099183)) ;
#60159 = CARTESIAN_POINT('Ctrl Pts',(31.2164529857702,-1.92107491594367,1.69305675445358)) ;
#60160 = CARTESIAN_POINT('Ctrl Pts',(31.2160238342365,-1.91898742939789,1.69300363238707)) ;
#60161 = CARTESIAN_POINT('Ctrl Pts',(31.2153877829594,-1.9158922883102,1.69292013131494)) ;
#60162 = CARTESIAN_POINT('Ctrl Pts',(31.2151770466207,-1.9148665932158,1.69289164972855)) ;
#60163 = CARTESIAN_POINT('Ctrl Pts',(31.214758781138,-1.912830238301,1.69283292599244)) ;
#60164 = CARTESIAN_POINT('Ctrl Pts',(31.2145512518463,-1.91181957843706,1.6928026864043)) ;
#60165 = CARTESIAN_POINT('Ctrl Pts',(31.2141400711059,-1.90981629939523,1.69273954955086)) ;
#60166 = CARTESIAN_POINT('Ctrl Pts',(31.2139364179195,-1.90882368204382,1.69270669130966)) ;
#60167 = CARTESIAN_POINT('Ctrl Pts',(31.2136343991363,-1.90735055457764,1.69265387591175)) ;
#60168 = CARTESIAN_POINT('Ctrl Pts',(31.2135343036764,-1.90686214568561,1.69263567297964)) ;
#60169 = CARTESIAN_POINT('Ctrl Pts',(31.2133353799399,-1.90589097957973,1.69259746889062)) ;
#60170 = CARTESIAN_POINT('Ctrl Pts',(31.2132365502277,-1.90540822171605,1.69257749172998)) ;
#60171 = CARTESIAN_POINT('Ctrl Pts',(31.2130879550431,-1.90468171186102,1.69254493427891)) ;
#60172 = CARTESIAN_POINT('Ctrl Pts',(31.2130349926572,-1.90442265081812,1.69253287985787)) ;
#60173 = CARTESIAN_POINT('Ctrl Pts',(31.212926670338,-1.90389239396861,1.69250667033966)) ;
#60174 = CARTESIAN_POINT('Ctrl Pts',(31.2128713100969,-1.90362119797884,1.6924925202205)) ;
#60175 = CARTESIAN_POINT('Ctrl Pts',(31.2127608002093,-1.90307911869992,1.69246152943509)) ;
#60176 = CARTESIAN_POINT('Ctrl Pts',(31.2127056533896,-1.90280827418462,1.69244478463953)) ;
#60177 = CARTESIAN_POINT('Ctrl Pts',(31.2124703134312,-1.90163369130276,1.69230175545996)) ;
#60178 = CARTESIAN_POINT('Ctrl Pts',(31.2124605599088,-1.90158501142511,1.69229582770205)) ;
#60179 = CARTESIAN_POINT('Ctrl Pts',(31.2124508063865,-1.90153633154746,1.69228989994415)) ;
#60180 = CARTESIAN_POINT('',(30.0223054639863,-15.0366437072153,15.9000442597426)) ;
#60181 = CARTESIAN_POINT('',(30.008421202744,-15.0366437072153,15.9262327545903)) ;
#60182 = CARTESIAN_POINT('Origin',(-1.20682669964218,-21.6462763158694,-0.639819022420589)) ;
#60183 = CARTESIAN_POINT('',(27.6170790376327,-1.90153624262371,14.6416486341816)) ;
#60184 = CARTESIAN_POINT('Ctrl Pts',(27.6170790543757,-1.90153633367698,14.6416486427733)) ;
#60185 = CARTESIAN_POINT('Ctrl Pts',(27.6170909284475,-1.90158489354294,14.6416476702318)) ;
#60186 = CARTESIAN_POINT('Ctrl Pts',(27.6172953105488,-1.90242072876526,14.6416309303902)) ;
#60187 = CARTESIAN_POINT('Ctrl Pts',(27.6173800480628,-1.90282163236688,14.6416479748488)) ;
#60188 = CARTESIAN_POINT('Ctrl Pts',(27.6174364929341,-1.90309535052159,14.6416622714043)) ;
#60189 = CARTESIAN_POINT('Ctrl Pts',(27.6175482732284,-1.90364317745633,14.6416931294984)) ;
#60190 = CARTESIAN_POINT('Ctrl Pts',(27.617603556575,-1.90391724740132,14.6417097721296)) ;
#60191 = CARTESIAN_POINT('Ctrl Pts',(27.6177109618581,-1.9044531216928,14.6417436089329)) ;
#60192 = CARTESIAN_POINT('Ctrl Pts',(27.6177630814776,-1.90471492622262,14.6417608075557)) ;
#60193 = CARTESIAN_POINT('Ctrl Pts',(27.6179086726074,-1.90544920904616,14.6418101549156)) ;
#60194 = CARTESIAN_POINT('Ctrl Pts',(27.6180046400594,-1.90593715923105,14.6418444219163)) ;
#60195 = CARTESIAN_POINT('Ctrl Pts',(27.6181967623408,-1.9069187704498,14.6419151220803)) ;
#60196 = CARTESIAN_POINT('Ctrl Pts',(27.6182929059663,-1.90741243213361,14.6419515766631)) ;
#60197 = CARTESIAN_POINT('Ctrl Pts',(27.6185819071216,-1.90890140264463,14.6420633878904)) ;
#60198 = CARTESIAN_POINT('Ctrl Pts',(27.6187753531983,-1.90990469490898,14.6421411566644)) ;
#60199 = CARTESIAN_POINT('Ctrl Pts',(27.6191642634503,-1.91192951728473,14.6423009341078)) ;
#60200 = CARTESIAN_POINT('Ctrl Pts',(27.6193597088623,-1.91295104556991,14.6423829773627)) ;
#60201 = CARTESIAN_POINT('Ctrl Pts',(27.6197524670421,-1.91500929858626,14.6425502462511)) ;
#60202 = CARTESIAN_POINT('Ctrl Pts',(27.6199497785913,-1.91604602336157,14.642635474202)) ;
#60203 = CARTESIAN_POINT('Ctrl Pts',(27.6205440333576,-1.91917444700591,14.6428948333414)) ;
#60204 = CARTESIAN_POINT('Ctrl Pts',(27.6209433157231,-1.92128437993827,14.6430725971919)) ;
#60205 = CARTESIAN_POINT('Ctrl Pts',(27.6217446234793,-1.92552861272312,14.6434337015435)) ;
#60206 = CARTESIAN_POINT('Ctrl Pts',(27.6221466321499,-1.92766291303188,14.6436170737834)) ;
#60207 = CARTESIAN_POINT('Ctrl Pts',(27.6233507429032,-1.93406598522556,14.6441708786263)) ;
#60208 = CARTESIAN_POINT('Ctrl Pts',(27.6241509510669,-1.93833487530353,14.6445449356854)) ;
#60209 = CARTESIAN_POINT('Ctrl Pts',(27.6257123249711,-1.94667883314713,14.6452811783355)) ;
#60210 = CARTESIAN_POINT('Ctrl Pts',(27.6264734566239,-1.95075390159159,14.6456434285222)) ;
#60211 = CARTESIAN_POINT('Ctrl Pts',(27.6279207920016,-1.95851130719468,14.6463359871736)) ;
#60212 = CARTESIAN_POINT('Ctrl Pts',(27.6286454412933,-1.96239975312801,14.6466847136137)) ;
#60213 = CARTESIAN_POINT('Ctrl Pts',(27.6300978542299,-1.97020012554322,14.6473866516838)) ;
#60214 = CARTESIAN_POINT('Ctrl Pts',(27.6308256170244,-1.9741120520386,14.6477398649235)) ;
#60215 = CARTESIAN_POINT('Ctrl Pts',(27.6330137497998,-1.98588191268041,14.6488054035607)) ;
#60216 = CARTESIAN_POINT('Ctrl Pts',(27.6344789863001,-1.99377392756813,14.6495235859559)) ;
#60217 = CARTESIAN_POINT('Ctrl Pts',(27.6374225189715,-2.00964277263372,14.6509727376127)) ;
#60218 = CARTESIAN_POINT('Ctrl Pts',(27.6389008016604,-2.01761960263699,14.651703732227)) ;
#60219 = CARTESIAN_POINT('Ctrl Pts',(27.6418699519166,-2.03365201652979,14.65317672962)) ;
#60220 = CARTESIAN_POINT('Ctrl Pts',(27.6433608190934,-2.0417076004239,14.6539187331361)) ;
#60221 = CARTESIAN_POINT('Ctrl Pts',(27.6478512357866,-2.06598339581858,14.6561592501836)) ;
#60222 = CARTESIAN_POINT('Ctrl Pts',(27.6508686476163,-2.08231264757128,14.6576721797494)) ;
#60223 = CARTESIAN_POINT('Ctrl Pts',(27.6569440624088,-2.1152134659747,14.6607283838232)) ;
#60224 = CARTESIAN_POINT('Ctrl Pts',(27.6600020427949,-2.13178503283035,14.6622717010056)) ;
#60225 = CARTESIAN_POINT('Ctrl Pts',(27.6661506889654,-2.16512202815071,14.6653822147967)) ;
#60226 = CARTESIAN_POINT('Ctrl Pts',(27.6692413457347,-2.18188745277619,14.6669494267159)) ;
#60227 = CARTESIAN_POINT('Ctrl Pts',(27.6754470665202,-2.21556369825287,14.670101961583)) ;
#60228 = CARTESIAN_POINT('Ctrl Pts',(27.6785621294787,-2.23247451911198,14.6716872865286)) ;
#60229 = CARTESIAN_POINT('Ctrl Pts',(27.687931224249,-2.28335239179949,14.67646232417)) ;
#60230 = CARTESIAN_POINT('Ctrl Pts',(27.6942091959947,-2.31746485344798,14.6796710353371)) ;
#60231 = CARTESIAN_POINT('Ctrl Pts',(27.7067599654047,-2.38568989519371,14.6860982692832)) ;
#60232 = CARTESIAN_POINT('Ctrl Pts',(27.7130327398153,-2.41980246162625,14.6893168298943)) ;
#60233 = CARTESIAN_POINT('Ctrl Pts',(27.7255032417993,-2.48764002417549,14.6957245106718)) ;
#60234 = CARTESIAN_POINT('Ctrl Pts',(27.7317009610019,-2.52136502033768,14.6989136466471)) ;
#60235 = CARTESIAN_POINT('Ctrl Pts',(27.7500761798837,-2.62137716461915,14.7083790904372)) ;
#60236 = CARTESIAN_POINT('Ctrl Pts',(27.7620357950646,-2.68650146817802,14.714553331675)) ;
#60237 = CARTESIAN_POINT('Ctrl Pts',(27.7858983569804,-2.81647723388609,14.7268883261163)) ;
#60238 = CARTESIAN_POINT('Ctrl Pts',(27.7984089201602,-2.88464214796207,14.7333648690751)) ;
#60239 = CARTESIAN_POINT('Ctrl Pts',(27.8234997178078,-3.02138341989203,14.7463680676332)) ;
#60240 = CARTESIAN_POINT('Ctrl Pts',(27.8360799339147,-3.08995977781875,14.752894757897)) ;
#60241 = CARTESIAN_POINT('Ctrl Pts',(27.8613088744068,-3.22751066216052,14.7659945877528)) ;
#60242 = CARTESIAN_POINT('Ctrl Pts',(27.8739575913392,-3.29648518856197,14.7725677413957)) ;
#60243 = CARTESIAN_POINT('Ctrl Pts',(27.899321952774,-3.43481913589162,14.7857576231482)) ;
#60244 = CARTESIAN_POINT('Ctrl Pts',(27.9120375963184,-3.50417855682328,14.7923743530643)) ;
#60245 = CARTESIAN_POINT('Ctrl Pts',(27.9502821814213,-3.71281425181492,14.8122862828268)) ;
#60246 = CARTESIAN_POINT('Ctrl Pts',(27.9759088285234,-3.8526479574165,14.8256431260594)) ;
#60247 = CARTESIAN_POINT('Ctrl Pts',(28.0274063617563,-4.13369567233197,14.8525051109128)) ;
#60248 = CARTESIAN_POINT('Ctrl Pts',(28.0532772198779,-4.27490968172529,14.8660103053992)) ;
#60249 = CARTESIAN_POINT('Ctrl Pts',(28.1052456159083,-4.55861182703004,14.8931552682346)) ;
#60250 = CARTESIAN_POINT('Ctrl Pts',(28.1313431411544,-4.70109996203175,14.9067950600667)) ;
#60251 = CARTESIAN_POINT('Ctrl Pts',(28.1837466950101,-4.98724417938732,14.9341966563273)) ;
#60252 = CARTESIAN_POINT('Ctrl Pts',(28.210052717377,-5.1309002617562,14.9479584725376)) ;
#60253 = CARTESIAN_POINT('Ctrl Pts',(28.2628547252717,-5.41927419743718,14.9755922436653)) ;
#60254 = CARTESIAN_POINT('Ctrl Pts',(28.2893507077362,-5.563992050747,14.9894642043592)) ;
#60255 = CARTESIAN_POINT('Ctrl Pts',(28.3425138642521,-5.85438335238595,15.0173068271929)) ;
#60256 = CARTESIAN_POINT('Ctrl Pts',(28.3691810377508,-6.00005680071646,15.0312774903742)) ;
#60257 = CARTESIAN_POINT('Ctrl Pts',(28.4494109621522,-6.43835127486106,15.0733208029126)) ;
#60258 = CARTESIAN_POINT('Ctrl Pts',(28.503202151952,-6.7322464251316,15.1015247071888)) ;
#60259 = CARTESIAN_POINT('Ctrl Pts',(28.6112411485239,-7.32258498307404,15.1581955212879)) ;
#60260 = CARTESIAN_POINT('Ctrl Pts',(28.6654889372312,-7.61902839077961,15.1866624651996)) ;
#60261 = CARTESIAN_POINT('Ctrl Pts',(28.7742876405899,-8.21361405443553,15.2437741189221)) ;
#60262 = CARTESIAN_POINT('Ctrl Pts',(28.8288385462861,-8.51175631038259,15.2724188456229)) ;
#60263 = CARTESIAN_POINT('Ctrl Pts',(28.9380894768923,-9.10889026217819,15.3298017983529)) ;
#60264 = CARTESIAN_POINT('Ctrl Pts',(28.9927894976113,-9.40788195803363,15.3585400322891)) ;
#60265 = CARTESIAN_POINT('Ctrl Pts',(29.1568817385665,-10.3048570937892,15.4447695077162)) ;
#60266 = CARTESIAN_POINT('Ctrl Pts',(29.2662662086701,-10.9028405664495,15.5022753819552)) ;
#60267 = CARTESIAN_POINT('Ctrl Pts',(29.4837774821227,-12.0920123230926,15.6166613433893)) ;
#60268 = CARTESIAN_POINT('Ctrl Pts',(29.5919042492133,-12.6832006071272,15.6735414989958)) ;
#60269 = CARTESIAN_POINT('Ctrl Pts',(29.8081521853442,-13.8656062554755,15.7873251993035)) ;
#60270 = CARTESIAN_POINT('Ctrl Pts',(29.9162144772883,-14.4565031966882,15.8441984291581)) ;
#60271 = CARTESIAN_POINT('Ctrl Pts',(30.0223054640206,-15.0366437072152,15.9000442596779)) ;
#60272 = CARTESIAN_POINT('Ctrl Pts',(30.0084212027096,-15.0366437072153,15.926232754655)) ;
#60273 = CARTESIAN_POINT('Ctrl Pts',(30.0060125542796,-15.0234311859071,15.9249466590702)) ;
#60274 = CARTESIAN_POINT('Ctrl Pts',(30.0036028909758,-15.0102130853827,15.9236600162224)) ;
#60275 = CARTESIAN_POINT('Ctrl Pts',(29.8977542434076,-14.4295845145506,15.8671417561465)) ;
#60276 = CARTESIAN_POINT('Ctrl Pts',(29.7924622066071,-13.8519867029534,15.8109107703475)) ;
#60277 = CARTESIAN_POINT('Ctrl Pts',(29.5794117650166,-12.6832006073523,15.6971048239497)) ;
#60278 = CARTESIAN_POINT('Ctrl Pts',(29.4716533429022,-12.0920123233512,15.6395298960295)) ;
#60279 = CARTESIAN_POINT('Ctrl Pts',(29.2549128278598,-10.9028405667752,15.52369013004)) ;
#60280 = CARTESIAN_POINT('Ctrl Pts',(29.145930698655,-10.3048570941488,15.4654253603752)) ;
#60281 = CARTESIAN_POINT('Ctrl Pts',(28.982473067386,-9.40788195844391,15.3779988841212)) ;
#60282 = CARTESIAN_POINT('Ctrl Pts',(28.9279898032311,-9.10889026260538,15.3488518039411)) ;
#60283 = CARTESIAN_POINT('Ctrl Pts',(28.819184355446,-8.51175631084354,15.2906285814875)) ;
#60284 = CARTESIAN_POINT('Ctrl Pts',(28.7648621676244,-8.21361405491334,15.2615524471178)) ;
#60285 = CARTESIAN_POINT('Ctrl Pts',(28.6565350551247,-7.61902839129104,15.2035512786878)) ;
#60286 = CARTESIAN_POINT('Ctrl Pts',(28.6025301214926,-7.32258498360224,15.1746262615182)) ;
#60287 = CARTESIAN_POINT('Ctrl Pts',(28.4949942247213,-6.73224642569316,15.117006500543)) ;
#60288 = CARTESIAN_POINT('Ctrl Pts',(28.4414632435045,-6.43835127543923,15.0883117908206)) ;
#60289 = CARTESIAN_POINT('Ctrl Pts',(28.3616404604458,-6.00005680131941,15.0455005282547)) ;
#60290 = CARTESIAN_POINT('Ctrl Pts',(28.3351118233974,-5.85438335299716,15.0312685576118)) ;
#60291 = CARTESIAN_POINT('Ctrl Pts',(28.2822323150105,-5.5639920513746,15.0028909176579)) ;
#60292 = CARTESIAN_POINT('Ctrl Pts',(28.2558814431192,-5.41927419807298,14.9887452493908)) ;
#60293 = CARTESIAN_POINT('Ctrl Pts',(28.2033774709265,-5.13090026240829,14.9605493233015)) ;
#60294 = CARTESIAN_POINT('Ctrl Pts',(28.1772243675642,-4.98724418004753,14.9464990712542)) ;
#60295 = CARTESIAN_POINT('Ctrl Pts',(28.1251361712074,-4.70109996270815,14.9185026476569)) ;
#60296 = CARTESIAN_POINT('Ctrl Pts',(28.0992010719645,-4.55861182771449,14.9045564878861)) ;
#60297 = CARTESIAN_POINT('Ctrl Pts',(28.0475694932131,-4.27490968242578,14.8767762202746)) ;
#60298 = CARTESIAN_POINT('Ctrl Pts',(28.0218730013745,-4.13369567304044,14.8629421360925)) ;
#60299 = CARTESIAN_POINT('Ctrl Pts',(27.9707398824971,-3.85264795814086,14.8353927928548)) ;
#60300 = CARTESIAN_POINT('Ctrl Pts',(27.9453032274214,-3.71281425254719,14.8216775866479)) ;
#60301 = CARTESIAN_POINT('Ctrl Pts',(27.9073599757471,-3.50417855756733,14.8011972817496)) ;
#60302 = CARTESIAN_POINT('Ctrl Pts',(27.8947475265083,-3.43481913663961,14.7943859067264)) ;
#60303 = CARTESIAN_POINT('Ctrl Pts',(27.8695962549378,-3.29648518931778,14.7807940948554)) ;
#60304 = CARTESIAN_POINT('Ctrl Pts',(27.8570574316513,-3.22751066292022,14.7740136598092)) ;
#60305 = CARTESIAN_POINT('Ctrl Pts',(27.8320566915263,-3.08995977858624,14.7604833984031)) ;
#60306 = CARTESIAN_POINT('Ctrl Pts',(27.8195947672391,-3.0213834206634,14.7537335860997)) ;
#60307 = CARTESIAN_POINT('Ctrl Pts',(27.7947515317538,-2.88464214874115,14.7402634357714)) ;
#60308 = CARTESIAN_POINT('Ctrl Pts',(27.7823702021659,-2.81647723466904,14.7335431324013)) ;
#60309 = CARTESIAN_POINT('Ctrl Pts',(27.7587693018651,-2.68650146887413,14.7207145917589)) ;
#60310 = CARTESIAN_POINT('Ctrl Pts',(27.7469473689554,-2.62137716522004,14.7142806541665)) ;
#60311 = CARTESIAN_POINT('Ctrl Pts',(27.7288009900815,-2.52136502079237,14.7043835722678)) ;
#60312 = CARTESIAN_POINT('Ctrl Pts',(27.7226832974612,-2.48764002458085,14.7010434901236)) ;
#60313 = CARTESIAN_POINT('Ctrl Pts',(27.7103814461481,-2.41980246193246,14.6943177003912)) ;
#60314 = CARTESIAN_POINT('Ctrl Pts',(27.7041972790692,-2.38568989545004,14.6909320086009)) ;
#60315 = CARTESIAN_POINT('Ctrl Pts',(27.6918341987723,-2.31746485360458,14.6841507553881)) ;
#60316 = CARTESIAN_POINT('Ctrl Pts',(27.685655267294,-2.28335239190624,14.6807552344374)) ;
#60317 = CARTESIAN_POINT('Ctrl Pts',(27.6764452063594,-2.23247451914435,14.6756802271275)) ;
#60318 = CARTESIAN_POINT('Ctrl Pts',(27.6733849172902,-2.21556369826045,14.6739915876559)) ;
#60319 = CARTESIAN_POINT('Ctrl Pts',(27.6672930286196,-2.18188745273454,14.6706243426214)) ;
#60320 = CARTESIAN_POINT('Ctrl Pts',(27.6642614279573,-2.16512202808461,14.6689457390569)) ;
#60321 = CARTESIAN_POINT('Ctrl Pts',(27.6582363492046,-2.13178503271551,14.6656021523692)) ;
#60322 = CARTESIAN_POINT('Ctrl Pts',(27.6552428635025,-2.11521346583559,14.6639371852972)) ;
#60323 = CARTESIAN_POINT('Ctrl Pts',(27.6493038328078,-2.08231264738407,14.6606237335042)) ;
#60324 = CARTESIAN_POINT('Ctrl Pts',(27.6463582651616,-2.06598339560755,14.6589752914224)) ;
#60325 = CARTESIAN_POINT('Ctrl Pts',(27.6419838500786,-2.04170760017737,14.6565159721111)) ;
#60326 = CARTESIAN_POINT('Ctrl Pts',(27.6405330465524,-2.03365201627149,14.6556984005285)) ;
#60327 = CARTESIAN_POINT('Ctrl Pts',(27.637647614093,-2.01761960235524,14.6540674946091)) ;
#60328 = CARTESIAN_POINT('Ctrl Pts',(27.6362129847709,-2.00964277234037,14.6532541610049)) ;
#60329 = CARTESIAN_POINT('Ctrl Pts',(27.6333616654222,-1.99377392725156,14.65163107656)) ;
#60330 = CARTESIAN_POINT('Ctrl Pts',(27.6319449619722,-1.98588191235219,14.6508213511158)) ;
#60331 = CARTESIAN_POINT('Ctrl Pts',(27.6298350755515,-1.97411205169318,14.6496082241895)) ;
#60332 = CARTESIAN_POINT('Ctrl Pts',(27.6291343137748,-1.97020012519214,14.649204081625)) ;
#60333 = CARTESIAN_POINT('Ctrl Pts',(27.6277382520011,-1.96239975276553,14.6483958539812)) ;
#60334 = CARTESIAN_POINT('Ctrl Pts',(27.6270429511546,-1.95851130682655,14.6479917704986)) ;
#60335 = CARTESIAN_POINT('Ctrl Pts',(27.6256575021144,-1.95075390138752,14.647182481904)) ;
#60336 = CARTESIAN_POINT('Ctrl Pts',(27.6249305344201,-1.94667883312135,14.6467557917342)) ;
#60337 = CARTESIAN_POINT('Ctrl Pts',(27.6234449317041,-1.93833487564255,14.6458766296228)) ;
#60338 = CARTESIAN_POINT('Ctrl Pts',(27.6226862623354,-1.93406598575086,14.6454242221669)) ;
#60339 = CARTESIAN_POINT('Ctrl Pts',(27.6215521528282,-1.92766291383711,14.6447383810907)) ;
#60340 = CARTESIAN_POINT('Ctrl Pts',(27.6211747756013,-1.92552861362188,14.6445085490605)) ;
#60341 = CARTESIAN_POINT('Ctrl Pts',(27.6204262099871,-1.9212843810226,14.6440479625576)) ;
#60342 = CARTESIAN_POINT('Ctrl Pts',(27.6200550047194,-1.91917444818244,14.6438172397235)) ;
#60343 = CARTESIAN_POINT('Ctrl Pts',(27.6195068479476,-1.91604602467482,14.6434709306027)) ;
#60344 = CARTESIAN_POINT('Ctrl Pts',(27.6193255770221,-1.91500929994461,14.6433554468457)) ;
#60345 = CARTESIAN_POINT('Ctrl Pts',(27.6189667196087,-1.91295104701829,14.6431242343686)) ;
#60346 = CARTESIAN_POINT('Ctrl Pts',(27.6187891319118,-1.91192951877891,14.6430085079098)) ;
#60347 = CARTESIAN_POINT('Ctrl Pts',(27.6184386344892,-1.9099046964915,14.642776276223)) ;
#60348 = CARTESIAN_POINT('Ctrl Pts',(27.6182657066978,-1.90890140427079,14.6426598058766)) ;
#60349 = CARTESIAN_POINT('Ctrl Pts',(27.618010978076,-1.90741243382484,14.6424833498222)) ;
#60350 = CARTESIAN_POINT('Ctrl Pts',(27.6179268504269,-1.90691877216053,14.6424242307122)) ;
#60351 = CARTESIAN_POINT('Ctrl Pts',(27.6177605161466,-1.90593716098465,14.6423048892371)) ;
#60352 = CARTESIAN_POINT('Ctrl Pts',(27.6176782980773,-1.90544921082332,14.6422446881598)) ;
#60353 = CARTESIAN_POINT('Ctrl Pts',(27.6175557499485,-1.90471492798114,14.6421518770811)) ;
#60354 = CARTESIAN_POINT('Ctrl Pts',(27.617512265948,-1.90445312340757,14.6421183899336)) ;
#60355 = CARTESIAN_POINT('Ctrl Pts',(27.6174239851282,-1.90391724903068,14.6420484805282)) ;
#60356 = CARTESIAN_POINT('Ctrl Pts',(27.6173791859132,-1.90364317904312,14.6420120627081)) ;
#60357 = CARTESIAN_POINT('Ctrl Pts',(27.6172909153254,-1.90309535201991,14.6419368605644)) ;
#60358 = CARTESIAN_POINT('Ctrl Pts',(27.6172474060307,-1.9028216338149,14.6418981649009)) ;
#60359 = CARTESIAN_POINT('Ctrl Pts',(27.617091807557,-1.90163369931123,14.6416675448799)) ;
#60360 = CARTESIAN_POINT('Ctrl Pts',(27.6170854309663,-1.90158501649411,14.6416580938266)) ;
#60361 = CARTESIAN_POINT('Ctrl Pts',(27.6170790543757,-1.90153633367698,14.6416486427733)) ;
#60362 = CARTESIAN_POINT('',(20.5712511819766,-15.0366437072153,27.0365282098628)) ;
#60363 = CARTESIAN_POINT('',(20.5476539041778,-15.0366437072153,27.0544663940874)) ;
#60364 = CARTESIAN_POINT('Origin',(-0.82663321391253,-21.6462763158694,-1.08741739643852)) ;
#60365 = CARTESIAN_POINT('',(18.916713407666,-1.90153624425509,24.8845109088162)) ;
#60366 = CARTESIAN_POINT('Ctrl Pts',(18.9167134194622,-1.90153633693974,24.8845109239092)) ;
#60367 = CARTESIAN_POINT('Ctrl Pts',(18.9167246001933,-1.90158489749522,24.8845150304531)) ;
#60368 = CARTESIAN_POINT('Ctrl Pts',(18.9169173960229,-1.90242225530982,24.8845858419702)) ;
#60369 = CARTESIAN_POINT('Ctrl Pts',(18.9169872501015,-1.90282386080039,24.8846369937121)) ;
#60370 = CARTESIAN_POINT('Ctrl Pts',(18.9170325447247,-1.90309805778379,24.8846737408821)) ;
#60371 = CARTESIAN_POINT('Ctrl Pts',(18.9171211741336,-1.90364684244124,24.8847488264717)) ;
#60372 = CARTESIAN_POINT('Ctrl Pts',(18.917164427513,-1.90392139127148,24.8847872166913)) ;
#60373 = CARTESIAN_POINT('Ctrl Pts',(18.9172478295099,-1.90445820158809,24.8848631676174)) ;
#60374 = CARTESIAN_POINT('Ctrl Pts',(18.9172879740443,-1.90472046326274,24.8849007314765)) ;
#60375 = CARTESIAN_POINT('Ctrl Pts',(18.9173995679819,-1.90545604096936,24.8850068498011)) ;
#60376 = CARTESIAN_POINT('Ctrl Pts',(18.9174723960696,-1.90594485602389,24.8850783796347)) ;
#60377 = CARTESIAN_POINT('Ctrl Pts',(18.917617312545,-1.9069282070596,24.8852234867119)) ;
#60378 = CARTESIAN_POINT('Ctrl Pts',(18.9176893817405,-1.90742274369117,24.8852970787139)) ;
#60379 = CARTESIAN_POINT('Ctrl Pts',(18.9179050798507,-1.90891435313948,24.8855203186311)) ;
#60380 = CARTESIAN_POINT('Ctrl Pts',(18.9180482304223,-1.90991942349788,24.8856724062683)) ;
#60381 = CARTESIAN_POINT('Ctrl Pts',(18.9183345848843,-1.91194783429415,24.8859812837709)) ;
#60382 = CARTESIAN_POINT('Ctrl Pts',(18.9184777572423,-1.91297117290453,24.8861380971322)) ;
#60383 = CARTESIAN_POINT('Ctrl Pts',(18.9187644623475,-1.91503307343387,24.8864554017379)) ;
#60384 = CARTESIAN_POINT('Ctrl Pts',(18.9189079930907,-1.91607163539539,24.8866158945166)) ;
#60385 = CARTESIAN_POINT('Ctrl Pts',(18.9193391502031,-1.91920560283358,24.8871016891789)) ;
#60386 = CARTESIAN_POINT('Ctrl Pts',(18.9196273767154,-1.92131927460614,24.8874312766233)) ;
#60387 = CARTESIAN_POINT('Ctrl Pts',(18.9202039805437,-1.92557102804893,24.8880966734798)) ;
#60388 = CARTESIAN_POINT('Ctrl Pts',(18.9204923293024,-1.92770911017595,24.8884325047192)) ;
#60389 = CARTESIAN_POINT('Ctrl Pts',(18.9213540857366,-1.93412352783167,24.8894425437714)) ;
#60390 = CARTESIAN_POINT('Ctrl Pts',(18.9219242497512,-1.9383999815575,24.8901192480343)) ;
#60391 = CARTESIAN_POINT('Ctrl Pts',(18.9230340800967,-1.94675872290243,24.8914454363964)) ;
#60392 = CARTESIAN_POINT('Ctrl Pts',(18.9235736882947,-1.95084101120065,24.8920949648635)) ;
#60393 = CARTESIAN_POINT('Ctrl Pts',(18.9245982302545,-1.95861222317853,24.893333470053)) ;
#60394 = CARTESIAN_POINT('Ctrl Pts',(18.9251103696797,-1.96250762108956,24.8939553645543)) ;
#60395 = CARTESIAN_POINT('Ctrl Pts',(18.926135595151,-1.97032193942165,24.8952045402017)) ;
#60396 = CARTESIAN_POINT('Ctrl Pts',(18.9266486797592,-1.97424085985611,24.8958318224441)) ;
#60397 = CARTESIAN_POINT('Ctrl Pts',(18.928189858839,-1.98603176322635,24.8977210686261)) ;
#60398 = CARTESIAN_POINT('Ctrl Pts',(18.9292199162513,-1.99393788781487,24.8989904032649)) ;
#60399 = CARTESIAN_POINT('Ctrl Pts',(18.9312865299045,-2.00983510388289,24.9015461889568)) ;
#60400 = CARTESIAN_POINT('Ctrl Pts',(18.9323230632391,-2.01782619518781,24.9028326573775)) ;
#60401 = CARTESIAN_POINT('Ctrl Pts',(18.9344029442502,-2.03388727245648,24.9054208944857)) ;
#60402 = CARTESIAN_POINT('Ctrl Pts',(18.9354462912739,-2.04195725842473,24.9067226636703)) ;
#60403 = CARTESIAN_POINT('Ctrl Pts',(18.9385864310043,-2.06627645495748,24.9106486518594)) ;
#60404 = CARTESIAN_POINT('Ctrl Pts',(18.9406934032119,-2.08263490068957,24.9132934891451)) ;
#60405 = CARTESIAN_POINT('Ctrl Pts',(18.9449314942448,-2.11559454019749,24.9186278233006)) ;
#60406 = CARTESIAN_POINT('Ctrl Pts',(18.9470625746199,-2.13219573417824,24.9213173494524)) ;
#60407 = CARTESIAN_POINT('Ctrl Pts',(18.9513444123465,-2.16559233026566,24.9267318585154)) ;
#60408 = CARTESIAN_POINT('Ctrl Pts',(18.9534951550791,-2.18238772853293,24.9294568515428)) ;
#60409 = CARTESIAN_POINT('Ctrl Pts',(18.9578112165814,-2.21612418118078,24.9349335682933)) ;
#60410 = CARTESIAN_POINT('Ctrl Pts',(18.9599765335518,-2.23306523556928,24.9376852933859)) ;
#60411 = CARTESIAN_POINT('Ctrl Pts',(18.9664862051206,-2.28403406873264,24.9459678532064)) ;
#60412 = CARTESIAN_POINT('Ctrl Pts',(18.970844338311,-2.31820751721538,24.9515260283606)) ;
#60413 = CARTESIAN_POINT('Ctrl Pts',(18.9795517811882,-2.38655453263177,24.9626491168712)) ;
#60414 = CARTESIAN_POINT('Ctrl Pts',(18.9839010538543,-2.42072808590034,24.9682140548224)) ;
#60415 = CARTESIAN_POINT('Ctrl Pts',(18.9925437571043,-2.48868692909063,24.9792855908494)) ;
#60416 = CARTESIAN_POINT('Ctrl Pts',(18.9968371734376,-2.52247221905787,24.98479219977)) ;
#60417 = CARTESIAN_POINT('Ctrl Pts',(19.0095621717323,-2.62266316565928,25.0011276406879)) ;
#60418 = CARTESIAN_POINT('Ctrl Pts',(19.0178385952872,-2.68790389863798,25.0117720165858)) ;
#60419 = CARTESIAN_POINT('Ctrl Pts',(19.03434711155,-2.81812392918961,25.0330266013669)) ;
#60420 = CARTESIAN_POINT('Ctrl Pts',(19.0429988126584,-2.88642263976059,25.0441795241338)) ;
#60421 = CARTESIAN_POINT('Ctrl Pts',(19.0603444951684,-3.02343231225636,25.0665602460336)) ;
#60422 = CARTESIAN_POINT('Ctrl Pts',(19.0690384453017,-3.09214327425391,25.0777880689548)) ;
#60423 = CARTESIAN_POINT('Ctrl Pts',(19.0864691080612,-3.22996414826103,25.100314771687)) ;
#60424 = CARTESIAN_POINT('Ctrl Pts',(19.0952058080039,-3.29907406025701,25.111613661136)) ;
#60425 = CARTESIAN_POINT('Ctrl Pts',(19.1127217414322,-3.43767953424804,25.134279218396)) ;
#60426 = CARTESIAN_POINT('Ctrl Pts',(19.1215009732858,-3.50717509624653,25.1456458874472)) ;
#60427 = CARTESIAN_POINT('Ctrl Pts',(19.1479015029145,-3.71622030857066,25.179843118157)) ;
#60428 = CARTESIAN_POINT('Ctrl Pts',(19.1655857217907,-3.85632848456949,25.2027708370381)) ;
#60429 = CARTESIAN_POINT('Ctrl Pts',(19.2011138810135,-4.13792784955716,25.2488638763194)) ;
#60430 = CARTESIAN_POINT('Ctrl Pts',(19.2189577736851,-4.27941903862544,25.2720292329816)) ;
#60431 = CARTESIAN_POINT('Ctrl Pts',(19.2547950843996,-4.56367804415205,25.3185776818844)) ;
#60432 = CARTESIAN_POINT('Ctrl Pts',(19.27278848106,-4.70644585970026,25.3419607901433)) ;
#60433 = CARTESIAN_POINT('Ctrl Pts',(19.3089135538598,-4.99315173061398,25.3889256738188)) ;
#60434 = CARTESIAN_POINT('Ctrl Pts',(19.3270452193696,-5.13708978599453,25.4125074573199)) ;
#60435 = CARTESIAN_POINT('Ctrl Pts',(19.3634349644308,-5.42602975175821,25.4598510947412)) ;
#60436 = CARTESIAN_POINT('Ctrl Pts',(19.3816930387743,-5.57103166213904,25.4836129526197)) ;
#60437 = CARTESIAN_POINT('Ctrl Pts',(19.4183233423265,-5.86199295357377,25.5312984414969)) ;
#60438 = CARTESIAN_POINT('Ctrl Pts',(19.4366955705936,-6.007952334629,25.5552220732107)) ;
#60439 = CARTESIAN_POINT('Ctrl Pts',(19.491964714102,-6.44710710781996,25.6272084747515)) ;
#60440 = CARTESIAN_POINT('Ctrl Pts',(19.5290141484514,-6.74157912528294,25.6754867038415)) ;
#60441 = CARTESIAN_POINT('Ctrl Pts',(19.6034176105111,-7.3330764193532,25.7724744209222)) ;
#60442 = CARTESIAN_POINT('Ctrl Pts',(19.6407716074773,-7.63010169599417,25.8211839322927)) ;
#60443 = CARTESIAN_POINT('Ctrl Pts',(19.7156804754865,-8.22585443201747,25.9188921269566)) ;
#60444 = CARTESIAN_POINT('Ctrl Pts',(19.7532353312954,-8.52458189139653,25.9678908218298)) ;
#60445 = CARTESIAN_POINT('Ctrl Pts',(19.8284413201389,-9.12288791730656,26.0660359638418)) ;
#60446 = CARTESIAN_POINT('Ctrl Pts',(19.8660924460453,-9.42246648384445,26.1151824164005)) ;
#60447 = CARTESIAN_POINT('Ctrl Pts',(19.9790325106291,-10.321202231654,26.2626319069737)) ;
#60448 = CARTESIAN_POINT('Ctrl Pts',(20.0543082599602,-10.9203594456895,26.3609449797701)) ;
#60449 = CARTESIAN_POINT('Ctrl Pts',(20.2039793991902,-12.1118653471233,26.5564729205436)) ;
#60450 = CARTESIAN_POINT('Ctrl Pts',(20.2783747273927,-12.7042140345733,26.6536878354332)) ;
#60451 = CARTESIAN_POINT('Ctrl Pts',(20.4260447461218,-13.880135442222,26.8466913840078)) ;
#60452 = CARTESIAN_POINT('Ctrl Pts',(20.4993050558587,-14.4635951119166,26.9424616027179)) ;
#60453 = CARTESIAN_POINT('Ctrl Pts',(20.5712511819835,-15.0366437072153,27.0365282098576)) ;
#60454 = CARTESIAN_POINT('Ctrl Pts',(20.5476539041697,-15.0366437072153,27.0544663940936)) ;
#60455 = CARTESIAN_POINT('Ctrl Pts',(20.5470684975163,-15.0319446558128,27.0536915741554)) ;
#60456 = CARTESIAN_POINT('Ctrl Pts',(20.5464830041271,-15.0272449043538,27.0529166384232)) ;
#60457 = CARTESIAN_POINT('Ctrl Pts',(20.4750716273534,-14.454025800044,26.9583992626796)) ;
#60458 = CARTESIAN_POINT('Ctrl Pts',(20.4029804926787,-13.8752942608754,26.8629676433982)) ;
#60459 = CARTESIAN_POINT('Ctrl Pts',(20.2571208155035,-12.7042140341984,26.6698446391085)) ;
#60460 = CARTESIAN_POINT('Ctrl Pts',(20.1833522435298,-12.1118653466928,26.572153276506)) ;
#60461 = CARTESIAN_POINT('Ctrl Pts',(20.0349925688502,-10.920359445147,26.375628386271)) ;
#60462 = CARTESIAN_POINT('Ctrl Pts',(19.9604014044365,-10.3212022310552,26.2767949055354)) ;
#60463 = CARTESIAN_POINT('Ctrl Pts',(19.8485411167186,-9.42246648316126,26.1285245899066)) ;
#60464 = CARTESIAN_POINT('Ctrl Pts',(19.8112587958758,-9.12288791659522,26.07909777902)) ;
#60465 = CARTESIAN_POINT('Ctrl Pts',(19.7368107782602,-8.52458189062898,25.980376442246)) ;
#60466 = CARTESIAN_POINT('Ctrl Pts',(19.6996450743571,-8.22585443122183,25.9310819217775)) ;
#60467 = CARTESIAN_POINT('Ctrl Pts',(19.6255385891123,-7.63010169514257,25.8327637715793)) ;
#60468 = CARTESIAN_POINT('Ctrl Pts',(19.5885977925355,-7.3330764184737,25.7837401534318)) ;
#60469 = CARTESIAN_POINT('Ctrl Pts',(19.5150503130468,-6.74157912434787,25.6861017353031)) ;
#60470 = CARTESIAN_POINT('Ctrl Pts',(19.4784435993818,-6.44710710685725,25.6374869586913)) ;
#60471 = CARTESIAN_POINT('Ctrl Pts',(19.4238671648451,-6.00795233362499,25.5649739734696)) ;
#60472 = CARTESIAN_POINT('Ctrl Pts',(19.4057306413877,-5.86199295255608,25.5408711636141)) ;
#60473 = CARTESIAN_POINT('Ctrl Pts',(19.3695829331826,-5.57103166109401,25.4928188152847)) ;
#60474 = CARTESIAN_POINT('Ctrl Pts',(19.3515717474928,-5.42602975069957,25.4688692775275)) ;
#60475 = CARTESIAN_POINT('Ctrl Pts',(19.3156890740419,-5.13708978490872,25.4211401742822)) ;
#60476 = CARTESIAN_POINT('Ctrl Pts',(19.2978175810733,-4.99315172951466,25.3973606127537)) ;
#60477 = CARTESIAN_POINT('Ctrl Pts',(19.2622290484611,-4.70644585857401,25.3499878618243)) ;
#60478 = CARTESIAN_POINT('Ctrl Pts',(19.2445119981902,-4.56367804301236,25.3263946804981)) ;
#60479 = CARTESIAN_POINT('Ctrl Pts',(19.2092477367877,-4.27941903745906,25.2794106108267)) ;
#60480 = CARTESIAN_POINT('Ctrl Pts',(19.1917005045017,-4.13792784837747,25.2560197387988)) ;
#60481 = CARTESIAN_POINT('Ctrl Pts',(19.1567923462519,-3.85632848336334,25.2094553870243)) ;
#60482 = CARTESIAN_POINT('Ctrl Pts',(19.139431372585,-3.71622030735133,25.1862819435199)) ;
#60483 = CARTESIAN_POINT('Ctrl Pts',(19.1135435210161,-3.50717509500758,25.1516949850762)) ;
#60484 = CARTESIAN_POINT('Ctrl Pts',(19.1049398604539,-3.43767953300257,25.1401948501975)) ;
#60485 = CARTESIAN_POINT('Ctrl Pts',(19.0877864714919,-3.29907405899852,25.1172536937959)) ;
#60486 = CARTESIAN_POINT('Ctrl Pts',(19.0792367414662,-3.22996414699606,25.1058126735094)) ;
#60487 = CARTESIAN_POINT('Ctrl Pts',(19.062194333463,-3.09214327297596,25.0829908271812)) ;
#60488 = CARTESIAN_POINT('Ctrl Pts',(19.0537016428067,-3.02343231097198,25.0716100107814)) ;
#60489 = CARTESIAN_POINT('Ctrl Pts',(19.0367771600085,-2.88642263846334,25.0489091011817)) ;
#60490 = CARTESIAN_POINT('Ctrl Pts',(19.0283453365751,-2.81812392788592,25.03758903175)) ;
#60491 = CARTESIAN_POINT('Ctrl Pts',(19.0122819774909,-2.68790389729668,25.0159960472697)) ;
#60492 = CARTESIAN_POINT('Ctrl Pts',(19.0042397670059,-2.62266316428518,25.0051736272164)) ;
#60493 = CARTESIAN_POINT('Ctrl Pts',(18.9919040506772,-2.52247221763345,24.9885422618283)) ;
#60494 = CARTESIAN_POINT('Ctrl Pts',(18.9877467682398,-2.48868692764926,24.9829321666061)) ;
#60495 = CARTESIAN_POINT('Ctrl Pts',(18.9793909578204,-2.42072808442481,24.9716425403104)) ;
#60496 = CARTESIAN_POINT('Ctrl Pts',(18.975192415586,-2.38655453113906,24.9659630200594)) ;
#60497 = CARTESIAN_POINT('Ctrl Pts',(18.966804251457,-2.31820751568836,24.9545972221456)) ;
#60498 = CARTESIAN_POINT('Ctrl Pts',(18.9626145959631,-2.28403406718845,24.9489109735716)) ;
#60499 = CARTESIAN_POINT('Ctrl Pts',(18.9563754571263,-2.23306523399947,24.9404227601082)) ;
#60500 = CARTESIAN_POINT('Ctrl Pts',(18.9543033160809,-2.21612417960246,24.9376002045167)) ;
#60501 = CARTESIAN_POINT('Ctrl Pts',(18.9501808944577,-2.18238772693766,24.9319762865525)) ;
#60502 = CARTESIAN_POINT('Ctrl Pts',(18.9481306120741,-2.16559232866193,24.9291749255512)) ;
#60503 = CARTESIAN_POINT('Ctrl Pts',(18.944058974838,-2.13219573255776,24.9236006262252)) ;
#60504 = CARTESIAN_POINT('Ctrl Pts',(18.9420376063183,-2.11559453856861,24.9208276992869)) ;
#60505 = CARTESIAN_POINT('Ctrl Pts',(18.9380315181337,-2.08263489904415,24.915317001147)) ;
#60506 = CARTESIAN_POINT('Ctrl Pts',(18.9360467599696,-2.06627645330387,24.9125792591586)) ;
#60507 = CARTESIAN_POINT('Ctrl Pts',(18.9331039504433,-2.04195725675893,24.908503264445)) ;
#60508 = CARTESIAN_POINT('Ctrl Pts',(18.9321287556484,-2.03388727078661,24.9071496872821)) ;
#60509 = CARTESIAN_POINT('Ctrl Pts',(18.9301912869132,-2.01782619350988,24.904453191174)) ;
#60510 = CARTESIAN_POINT('Ctrl Pts',(18.9292290123289,-2.00983510220101,24.9031102727181)) ;
#60511 = CARTESIAN_POINT('Ctrl Pts',(18.9273192627605,-1.99393788612502,24.9004352420469)) ;
#60512 = CARTESIAN_POINT('Ctrl Pts',(18.9263717649069,-1.98603176153238,24.8991031472622)) ;
#60513 = CARTESIAN_POINT('Ctrl Pts',(18.9249636908405,-1.97424085815624,24.897112717278)) ;
#60514 = CARTESIAN_POINT('Ctrl Pts',(18.9244965377394,-1.97032193772004,24.8964505188111)) ;
#60515 = CARTESIAN_POINT('Ctrl Pts',(18.9235671714202,-1.96250761938401,24.8951284729298)) ;
#60516 = CARTESIAN_POINT('Ctrl Pts',(18.9231049567604,-1.9586122214708,24.894468626608)) ;
#60517 = CARTESIAN_POINT('Ctrl Pts',(18.9221856891252,-1.95084100968508,24.8931500940073)) ;
#60518 = CARTESIAN_POINT('Ctrl Pts',(18.9217041964974,-1.94675872159085,24.8924563872854)) ;
#60519 = CARTESIAN_POINT('Ctrl Pts',(18.9207232588284,-1.93839998066323,24.8910322173662)) ;
#60520 = CARTESIAN_POINT('Ctrl Pts',(18.9202237554944,-1.93412352715089,24.8903017983059)) ;
#60521 = CARTESIAN_POINT('Ctrl Pts',(18.9194810766782,-1.9277091098154,24.8892012388849)) ;
#60522 = CARTESIAN_POINT('Ctrl Pts',(18.91923462799,-1.92557102779551,24.8888335560678)) ;
#60523 = CARTESIAN_POINT('Ctrl Pts',(18.9187477427387,-1.92131927456496,24.8880999569773)) ;
#60524 = CARTESIAN_POINT('Ctrl Pts',(18.9185072775343,-1.91920560289798,24.8877340623579)) ;
#60525 = CARTESIAN_POINT('Ctrl Pts',(18.9181545368557,-1.91607163561626,24.8871886571131)) ;
#60526 = CARTESIAN_POINT('Ctrl Pts',(18.9180382925426,-1.91503307370567,24.8870074217427)) ;
#60527 = CARTESIAN_POINT('Ctrl Pts',(18.9178092554453,-1.91297117327927,24.8866462790838)) ;
#60528 = CARTESIAN_POINT('Ctrl Pts',(18.9176964606399,-1.9119478347208,24.8864663733209)) ;
#60529 = CARTESIAN_POINT('Ctrl Pts',(18.9174754496683,-1.90991942402579,24.8861078230146)) ;
#60530 = CARTESIAN_POINT('Ctrl Pts',(18.917367202443,-1.90891435371686,24.8859292025562)) ;
#60531 = CARTESIAN_POINT('Ctrl Pts',(18.9172098049877,-1.90742274434305,24.8856616436526)) ;
#60532 = CARTESIAN_POINT('Ctrl Pts',(18.9171581759787,-1.90692820773646,24.8855725134313)) ;
#60533 = CARTESIAN_POINT('Ctrl Pts',(18.9170571273222,-1.90594485674973,24.8853940589178)) ;
#60534 = CARTESIAN_POINT('Ctrl Pts',(18.9170076883461,-1.90545604172008,24.8853047491503)) ;
#60535 = CARTESIAN_POINT('Ctrl Pts',(18.9169352925858,-1.90472046411337,24.885168833172)) ;
#60536 = CARTESIAN_POINT('Ctrl Pts',(18.9169098377483,-1.90445820251875,24.8851201025163)) ;
#60537 = CARTESIAN_POINT('Ctrl Pts',(18.9168589676523,-1.90392139236518,24.8850194215245)) ;
#60538 = CARTESIAN_POINT('Ctrl Pts',(18.9168335483687,-1.90364684362271,24.8849674742005)) ;
#60539 = CARTESIAN_POINT('Ctrl Pts',(18.9167849105521,-1.90309805913159,24.8848619878359)) ;
#60540 = CARTESIAN_POINT('Ctrl Pts',(18.9167616202308,-1.90282386221791,24.8848085134487)) ;
#60541 = CARTESIAN_POINT('Ctrl Pts',(18.9167170645518,-1.90163370354021,24.8845334285406)) ;
#60542 = CARTESIAN_POINT('Ctrl Pts',(18.916715242007,-1.90158502023998,24.8845221762249)) ;
#60543 = CARTESIAN_POINT('Ctrl Pts',(18.9167134194622,-1.90153633693974,24.8845109239092)) ;
#60544 = CARTESIAN_POINT('',(7.31761838529024,-15.0366437072153,33.1753326132827)) ;
#60545 = CARTESIAN_POINT('',(7.28867002793266,-15.0366437072153,33.181704628584)) ;
#60546 = CARTESIAN_POINT('Origin',(-0.293637272419033,-21.6462763158694,-1.3340075774398)) ;
#60547 = CARTESIAN_POINT('',(6.71960918123862,-1.90153624278853,30.5274922283378)) ;
#60548 = CARTESIAN_POINT('Ctrl Pts',(6.7196091855373,-1.90153633400663,30.527492246694)) ;
#60549 = CARTESIAN_POINT('Ctrl Pts',(6.71961763099485,-1.90158489163453,30.5275006628107)) ;
#60550 = CARTESIAN_POINT('Ctrl Pts',(6.71976214984686,-1.90241581081184,30.5276446795811)) ;
#60551 = CARTESIAN_POINT('Ctrl Pts',(6.7198038475356,-1.90281444934172,30.5277198556706)) ;
#60552 = CARTESIAN_POINT('Ctrl Pts',(6.71982938587613,-1.90308662225266,30.5277718277734)) ;
#60553 = CARTESIAN_POINT('Ctrl Pts',(6.71987802505912,-1.90363135851574,30.5278763911327)) ;
#60554 = CARTESIAN_POINT('Ctrl Pts',(6.71990103052572,-1.90390388306625,30.5279289951723)) ;
#60555 = CARTESIAN_POINT('Ctrl Pts',(6.71994458342815,-1.90443673670834,30.5280321636685)) ;
#60556 = CARTESIAN_POINT('Ctrl Pts',(6.71996512589195,-1.90469706598677,30.5280827292591)) ;
#60557 = CARTESIAN_POINT('Ctrl Pts',(6.72002151385849,-1.90542716873087,30.5282248117068)) ;
#60558 = CARTESIAN_POINT('Ctrl Pts',(6.72005735925489,-1.90591232651548,30.528319584007)) ;
#60559 = CARTESIAN_POINT('Ctrl Pts',(6.72012752404694,-1.90688832041617,30.5285106660766)) ;
#60560 = CARTESIAN_POINT('Ctrl Pts',(6.72016181990902,-1.90737915718282,30.5286069811638)) ;
#60561 = CARTESIAN_POINT('Ctrl Pts',(6.72026321513444,-1.90885960740112,30.528897935056)) ;
#60562 = CARTESIAN_POINT('Ctrl Pts',(6.72032886026737,-1.90985715876355,30.5290945736736)) ;
#60563 = CARTESIAN_POINT('Ctrl Pts',(6.72045822892328,-1.91187039526605,30.5294921111097)) ;
#60564 = CARTESIAN_POINT('Ctrl Pts',(6.72052191412236,-1.91288607857933,30.5296930179773)) ;
#60565 = CARTESIAN_POINT('Ctrl Pts',(6.72064806943539,-1.91493255493047,30.5300982964868)) ;
#60566 = CARTESIAN_POINT('Ctrl Pts',(6.72071053707861,-1.91596334801114,30.5303026686815)) ;
#60567 = CARTESIAN_POINT('Ctrl Pts',(6.72089664234593,-1.91907387250008,30.5309199105522)) ;
#60568 = CARTESIAN_POINT('Ctrl Pts',(6.72101902700158,-1.92117173390307,30.5313368924495)) ;
#60569 = CARTESIAN_POINT('Ctrl Pts',(6.72126132588643,-1.92539168486392,30.5321765268574)) ;
#60570 = CARTESIAN_POINT('Ctrl Pts',(6.72138120521115,-1.92751377487788,30.5325991871476)) ;
#60571 = CARTESIAN_POINT('Ctrl Pts',(6.72173680403374,-1.93388021616538,30.5338680933395)) ;
#60572 = CARTESIAN_POINT('Ctrl Pts',(6.72196854648776,-1.93812468561987,30.5347152396626)) ;
#60573 = CARTESIAN_POINT('Ctrl Pts',(6.7224158750982,-1.94642091221635,30.5363723094294)) ;
#60574 = CARTESIAN_POINT('Ctrl Pts',(6.72263139013284,-1.95047267003741,30.5371822486719)) ;
#60575 = CARTESIAN_POINT('Ctrl Pts',(6.72303836615672,-1.95818550039066,30.5387247503642)) ;
#60576 = CARTESIAN_POINT('Ctrl Pts',(6.72324062169856,-1.96205150175638,30.5394983009961)) ;
#60577 = CARTESIAN_POINT('Ctrl Pts',(6.72364373171298,-1.96980684956421,30.541050650625)) ;
#60578 = CARTESIAN_POINT('Ctrl Pts',(6.72384458442883,-1.97369619601971,30.5418294500114)) ;
#60579 = CARTESIAN_POINT('Ctrl Pts',(6.72444578258132,-1.98539811988876,30.5441733177044)) ;
#60580 = CARTESIAN_POINT('Ctrl Pts',(6.72484481411897,-1.99324458139089,30.5457458453102)) ;
#60581 = CARTESIAN_POINT('Ctrl Pts',(6.72564157932198,-2.00902183023835,30.5489090300892)) ;
#60582 = CARTESIAN_POINT('Ctrl Pts',(6.72603928501628,-2.01695261740918,30.5504996933823)) ;
#60583 = CARTESIAN_POINT('Ctrl Pts',(6.72683444436499,-2.03289249115159,30.5536976440974)) ;
#60584 = CARTESIAN_POINT('Ctrl Pts',(6.72723189722214,-2.04090157772765,30.5553049316954)) ;
#60585 = CARTESIAN_POINT('Ctrl Pts',(6.72842471757584,-2.06503725187992,30.5601496340252)) ;
#60586 = CARTESIAN_POINT('Ctrl Pts',(6.72922064600262,-2.08127225042057,30.5634098657348)) ;
#60587 = CARTESIAN_POINT('Ctrl Pts',(6.73081561318064,-2.11398316398243,30.5699806239775)) ;
#60588 = CARTESIAN_POINT('Ctrl Pts',(6.73161460493413,-2.13045907920851,30.5732911608989)) ;
#60589 = CARTESIAN_POINT('Ctrl Pts',(6.73321551517985,-2.16360365253471,30.579952376134)) ;
#60590 = CARTESIAN_POINT('Ctrl Pts',(6.73401741622393,-2.180272306796,30.5833030574759)) ;
#60591 = CARTESIAN_POINT('Ctrl Pts',(6.73562319127244,-2.21375417249349,30.5900345750952)) ;
#60592 = CARTESIAN_POINT('Ctrl Pts',(6.73642706307232,-2.23056738393757,30.593415411859)) ;
#60593 = CARTESIAN_POINT('Ctrl Pts',(6.73883960451742,-2.28115158932819,30.6035883104669)) ;
#60594 = CARTESIAN_POINT('Ctrl Pts',(6.74044927101791,-2.31506715404313,30.6104107449792)) ;
#60595 = CARTESIAN_POINT('Ctrl Pts',(6.7436578074868,-2.38289840191499,30.6240580155635)) ;
#60596 = CARTESIAN_POINT('Ctrl Pts',(6.7452566337006,-2.41681407140828,30.6308828583751)) ;
#60597 = CARTESIAN_POINT('Ctrl Pts',(6.74842826526026,-2.48426007754026,30.6444567327451)) ;
#60598 = CARTESIAN_POINT('Ctrl Pts',(6.75000105319838,-2.51779041422449,30.6512057681449)) ;
#60599 = CARTESIAN_POINT('Ctrl Pts',(6.75465637156452,-2.61722529246259,30.6712221068618)) ;
#60600 = CARTESIAN_POINT('Ctrl Pts',(6.75767596939282,-2.68197370184678,30.6842586177816)) ;
#60601 = CARTESIAN_POINT('Ctrl Pts',(6.76368709728244,-2.81116116814065,30.7102723568555)) ;
#60602 = CARTESIAN_POINT('Ctrl Pts',(6.76683044475462,-2.87889443254617,30.7239132426992)) ;
#60603 = CARTESIAN_POINT('Ctrl Pts',(6.77312397740687,-3.01476979976207,30.7512800220962)) ;
#60604 = CARTESIAN_POINT('Ctrl Pts',(6.77627412448397,-3.08291190264499,30.7650059240521)) ;
#60605 = CARTESIAN_POINT('Ctrl Pts',(6.7825832881807,-3.21959175557408,30.7925394970826)) ;
#60606 = CARTESIAN_POINT('Ctrl Pts',(6.7857422893433,-3.28812950560671,30.8063471715564)) ;
#60607 = CARTESIAN_POINT('Ctrl Pts',(6.79207032559441,-3.42558746291981,30.8340412422536)) ;
#60608 = CARTESIAN_POINT('Ctrl Pts',(6.79523935870023,-3.49450767020372,30.8479276389131)) ;
#60609 = CARTESIAN_POINT('Ctrl Pts',(6.80476249563476,-3.70182219440112,30.8897005080007)) ;
#60610 = CARTESIAN_POINT('Ctrl Pts',(6.81113274335611,-3.84077041300617,30.9177006360046)) ;
#60611 = CARTESIAN_POINT('Ctrl Pts',(6.82391799489518,-4.1200384133498,30.973981271921)) ;
#60612 = CARTESIAN_POINT('Ctrl Pts',(6.83033294053835,-4.26035819516773,31.0022617926555)) ;
#60613 = CARTESIAN_POINT('Ctrl Pts',(6.84320669650211,-4.54226381709422,31.0590810847542)) ;
#60614 = CARTESIAN_POINT('Ctrl Pts',(6.84966548083055,-4.68384965629434,31.0876198616476)) ;
#60615 = CARTESIAN_POINT('Ctrl Pts',(6.86262474154796,-4.96818188617416,31.1449338183818)) ;
#60616 = CARTESIAN_POINT('Ctrl Pts',(6.86912520496441,-5.1109282768689,31.1737090010814)) ;
#60617 = CARTESIAN_POINT('Ctrl Pts',(6.88216489466588,-5.39747610568063,31.2314740888635)) ;
#60618 = CARTESIAN_POINT('Ctrl Pts',(6.88870411459209,-5.54127754379532,31.2604639953449)) ;
#60619 = CARTESIAN_POINT('Ctrl Pts',(6.90181790733773,-5.82982996387431,31.3186369560578)) ;
#60620 = CARTESIAN_POINT('Ctrl Pts',(6.90839247900822,-5.97458094583994,31.3478200105417)) ;
#60621 = CARTESIAN_POINT('Ctrl Pts',(6.92816363850333,-6.41009995266176,31.435626637206)) ;
#60622 = CARTESIAN_POINT('Ctrl Pts',(6.94140774507523,-6.70213403375071,31.494507655259)) ;
#60623 = CARTESIAN_POINT('Ctrl Pts',(6.96799044907206,-7.28873431687813,31.6127847052307)) ;
#60624 = CARTESIAN_POINT('Ctrl Pts',(6.98132900895718,-7.58330051895022,31.6721807454196)) ;
#60625 = CARTESIAN_POINT('Ctrl Pts',(7.00806644621525,-8.17412101370043,31.7913167596082)) ;
#60626 = CARTESIAN_POINT('Ctrl Pts',(7.02146530498564,-8.47037530637525,31.8510567377018)) ;
#60627 = CARTESIAN_POINT('Ctrl Pts',(7.0482880948497,-9.06372795280004,31.9707097837378)) ;
#60628 = CARTESIAN_POINT('Ctrl Pts',(7.06171201723382,-9.36082630655692,32.0306228535982)) ;
#60629 = CARTESIAN_POINT('Ctrl Pts',(7.10196750689891,-10.2521214159956,32.2103656563209)) ;
#60630 = CARTESIAN_POINT('Ctrl Pts',(7.12878294951035,-10.8463182044253,32.3301989454179)) ;
#60631 = CARTESIAN_POINT('Ctrl Pts',(7.18207860074687,-12.0279596230766,32.5685105146323)) ;
#60632 = CARTESIAN_POINT('Ctrl Pts',(7.20855873401127,-12.6154042533499,32.6869888113477)) ;
#60633 = CARTESIAN_POINT('Ctrl Pts',(7.26088782347813,-13.7767891024697,32.9212267181271)) ;
#60634 = CARTESIAN_POINT('Ctrl Pts',(7.28673674368023,-14.3507293213134,33.0369863361147)) ;
#60635 = CARTESIAN_POINT('Ctrl Pts',(7.31395599106871,-14.9552953856141,33.1589249456923)) ;
#60636 = CARTESIAN_POINT('Ctrl Pts',(7.31578843034751,-14.9959966435745,33.1671342399967)) ;
#60637 = CARTESIAN_POINT('Ctrl Pts',(7.31761838590214,-15.036643707215,33.1753326131477)) ;
#60638 = CARTESIAN_POINT('Ctrl Pts',(7.28867002732122,-15.036643707215,33.1817046287183)) ;
#60639 = CARTESIAN_POINT('Ctrl Pts',(7.28688844246616,-14.9959966435996,33.1734956083764)) ;
#60640 = CARTESIAN_POINT('Ctrl Pts',(7.28510452610483,-14.9552953856643,33.1652756333756)) ;
#60641 = CARTESIAN_POINT('Ctrl Pts',(7.25860735275774,-14.3507293214144,33.0431780832932)) ;
#60642 = CARTESIAN_POINT('Ctrl Pts',(7.23346099536329,-13.7767891025969,32.927263819543)) ;
#60643 = CARTESIAN_POINT('Ctrl Pts',(7.18259964647052,-12.6154042535299,32.6927028386439)) ;
#60644 = CARTESIAN_POINT('Ctrl Pts',(7.15688461897252,-12.0279596232834,32.5740561294197)) ;
#60645 = CARTESIAN_POINT('Ctrl Pts',(7.10519001132364,-10.8463182046858,32.3353921438736)) ;
#60646 = CARTESIAN_POINT('Ctrl Pts',(7.07921035581152,-10.2521214162831,32.21537488413)) ;
#60647 = CARTESIAN_POINT('Ctrl Pts',(7.040273204793,-9.36082630688502,32.035341893136)) ;
#60648 = CARTESIAN_POINT('Ctrl Pts',(7.02729958170864,-9.06372795314166,31.9753297049073)) ;
#60649 = CARTESIAN_POINT('Ctrl Pts',(7.00140227647856,-8.47037530674386,31.8554729443044)) ;
#60650 = CARTESIAN_POINT('Ctrl Pts',(6.98847858562182,-8.17412101408252,31.7956283738466)) ;
#60651 = CARTESIAN_POINT('Ctrl Pts',(6.96272091250221,-7.5833005193592,31.6762766972686)) ;
#60652 = CARTESIAN_POINT('Ctrl Pts',(6.94988691163539,-7.2887343173005,31.6167695952442)) ;
#60653 = CARTESIAN_POINT('Ctrl Pts',(6.92434947612469,-6.70213403419977,31.4982624642858)) ;
#60654 = CARTESIAN_POINT('Ctrl Pts',(6.91164600393193,-6.4100999531241,31.4392624436099)) ;
#60655 = CARTESIAN_POINT('Ctrl Pts',(6.89272077672772,-5.97458094632212,31.3512696131719)) ;
#60656 = CARTESIAN_POINT('Ctrl Pts',(6.88643404984998,-5.82982996436308,31.3220231992594)) ;
#60657 = CARTESIAN_POINT('Ctrl Pts',(6.87390961359624,-5.54127754429721,31.2637205113756)) ;
#60658 = CARTESIAN_POINT('Ctrl Pts',(6.86767190307711,-5.39747610618906,31.2346642376563)) ;
#60659 = CARTESIAN_POINT('Ctrl Pts',(6.85525147412051,-5.11092827739036,31.1767628402795)) ;
#60660 = CARTESIAN_POINT('Ctrl Pts',(6.84906874932502,-4.96818188670214,31.147917718022)) ;
#60661 = CARTESIAN_POINT('Ctrl Pts',(6.83676475000976,-4.68384965683525,31.090459527349)) ;
#60662 = CARTESIAN_POINT('Ctrl Pts',(6.83064346251804,-4.54226381764156,31.0618464617856)) ;
#60663 = CARTESIAN_POINT('Ctrl Pts',(6.81846956547935,-4.26035819572789,31.004873119091)) ;
#60664 = CARTESIAN_POINT('Ctrl Pts',(6.81241693002235,-4.12003841391635,30.9765128478552)) ;
#60665 = CARTESIAN_POINT('Ctrl Pts',(6.80038888440364,-3.84077041358543,30.9200655383146)) ;
#60666 = CARTESIAN_POINT('Ctrl Pts',(6.79441341605943,-3.7018221949867,30.8919785128001)) ;
#60667 = CARTESIAN_POINT('Ctrl Pts',(6.78551640858875,-3.49450767079874,30.8500678221975)) ;
#60668 = CARTESIAN_POINT('Ctrl Pts',(6.78256179852198,-3.42558746351796,30.8361342274587)) ;
#60669 = CARTESIAN_POINT('Ctrl Pts',(6.77667653021486,-3.28812950621108,30.8083426961684)) ;
#60670 = CARTESIAN_POINT('Ctrl Pts',(6.77374586998814,-3.21959175618158,30.7944847600546)) ;
#60671 = CARTESIAN_POINT('Ctrl Pts',(6.76791086463551,-3.08291190325872,30.7668468168815)) ;
#60672 = CARTESIAN_POINT('Ctrl Pts',(6.7650065040537,-3.01476980037891,30.7530668132276)) ;
#60673 = CARTESIAN_POINT('Ctrl Pts',(6.75922734717836,-2.87889443316919,30.7255868111615)) ;
#60674 = CARTESIAN_POINT('Ctrl Pts',(6.75635251278026,-2.81116116876676,30.7118868211215)) ;
#60675 = CARTESIAN_POINT('Ctrl Pts',(6.75088517917376,-2.68197370257456,30.6857533838959)) ;
#60676 = CARTESIAN_POINT('Ctrl Pts',(6.74815180308469,-2.61722529329389,30.672653870829)) ;
#60677 = CARTESIAN_POINT('Ctrl Pts',(6.74397221313066,-2.51779041521477,30.6525328164037)) ;
#60678 = CARTESIAN_POINT('Ctrl Pts',(6.74256579040069,-2.48426007858418,30.6457471612638)) ;
#60679 = CARTESIAN_POINT('Ctrl Pts',(6.73974476333519,-2.41681407256003,30.6320961130316)) ;
#60680 = CARTESIAN_POINT('Ctrl Pts',(6.73833014158143,-2.38289840312096,30.6252307237637)) ;
#60681 = CARTESIAN_POINT('Ctrl Pts',(6.73551179023391,-2.31506715535754,30.6114975669625)) ;
#60682 = CARTESIAN_POINT('Ctrl Pts',(6.73410801808841,-2.28115159069683,30.604629811687)) ;
#60683 = CARTESIAN_POINT('Ctrl Pts',(6.73202609214958,-2.23056738538709,30.5943841391202)) ;
#60684 = CARTESIAN_POINT('Ctrl Pts',(6.73133608993551,-2.21375417396992,30.5909782377709)) ;
#60685 = CARTESIAN_POINT('Ctrl Pts',(6.72996696101551,-2.18027230832599,30.5841946304111)) ;
#60686 = CARTESIAN_POINT('Ctrl Pts',(6.72928783210833,-2.16360365409132,30.5808169248839)) ;
#60687 = CARTESIAN_POINT('Ctrl Pts',(6.72794380721774,-2.13045908081809,30.5740991649175)) ;
#60688 = CARTESIAN_POINT('Ctrl Pts',(6.72727889411935,-2.11398316561836,30.570759115058)) ;
#60689 = CARTESIAN_POINT('Ctrl Pts',(6.725967457352,-2.0812722521088,30.5641259470635)) ;
#60690 = CARTESIAN_POINT('Ctrl Pts',(6.72532088666064,-2.06503725359408,30.5608328392358)) ;
#60691 = CARTESIAN_POINT('Ctrl Pts',(6.72436922338636,-2.0409015794804,30.5559350542269)) ;
#60692 = CARTESIAN_POINT('Ctrl Pts',(6.72405505930643,-2.03289249291726,30.5543094333854)) ;
#60693 = CARTESIAN_POINT('Ctrl Pts',(6.72343394173311,-2.01695261920032,30.551073173184)) ;
#60694 = CARTESIAN_POINT('Ctrl Pts',(6.72312698743446,-2.00902183204201,30.5494625340009)) ;
#60695 = CARTESIAN_POINT('Ctrl Pts',(6.72252192513256,-1.99324458321975,30.5462571522277)) ;
#60696 = CARTESIAN_POINT('Ctrl Pts',(6.72222378916939,-1.98539812173034,30.5446624158292)) ;
#60697 = CARTESIAN_POINT('Ctrl Pts',(6.72178525733552,-1.97369619787999,30.5422827425759)) ;
#60698 = CARTESIAN_POINT('Ctrl Pts',(6.7216405369464,-1.96980685143068,30.5414915875313)) ;
#60699 = CARTESIAN_POINT('Ctrl Pts',(6.72135457499626,-1.96205150363523,30.5399134516662)) ;
#60700 = CARTESIAN_POINT('Ctrl Pts',(6.72121333168194,-1.95818550227575,30.5391264712288)) ;
#60701 = CARTESIAN_POINT('Ctrl Pts',(6.72093501346366,-1.95047267180703,30.5375556497875)) ;
#60702 = CARTESIAN_POINT('Ctrl Pts',(6.72079052496425,-1.94642091385843,30.5367300763953)) ;
#60703 = CARTESIAN_POINT('Ctrl Pts',(6.7205007238683,-1.93812468700046,30.5350383321452)) ;
#60704 = CARTESIAN_POINT('Ctrl Pts',(6.72035534007046,-1.93388021741182,30.5341721768161)) ;
#60705 = CARTESIAN_POINT('Ctrl Pts',(6.72014527293166,-1.92751377592369,30.5328712366358)) ;
#60706 = CARTESIAN_POINT('Ctrl Pts',(6.72007660203497,-1.9253916858432,30.5324373045041)) ;
#60707 = CARTESIAN_POINT('Ctrl Pts',(6.71994395320502,-1.92117173474938,30.5315735342658)) ;
#60708 = CARTESIAN_POINT('Ctrl Pts',(6.71987994033495,-1.91907387328002,30.5311437037529)) ;
#60709 = CARTESIAN_POINT('Ctrl Pts',(6.7197896717627,-1.91596334869304,30.5305053666097)) ;
#60710 = CARTESIAN_POINT('Ctrl Pts',(6.71976055221698,-1.91493255558014,30.5302936539369)) ;
#60711 = CARTESIAN_POINT('Ctrl Pts',(6.71970487564627,-1.91288607916449,30.5298728618694)) ;
#60712 = CARTESIAN_POINT('Ctrl Pts',(6.71967831613871,-1.91187039581876,30.5296637830122)) ;
#60713 = CARTESIAN_POINT('Ctrl Pts',(6.71962880631066,-1.90985715925278,30.5292486673054)) ;
#60714 = CARTESIAN_POINT('Ctrl Pts',(6.71960581774062,-1.90885960785732,30.5290426392613)) ;
#60715 = CARTESIAN_POINT('Ctrl Pts',(6.71957567318844,-1.9073791575924,30.5287360019001)) ;
#60716 = CARTESIAN_POINT('Ctrl Pts',(6.71956635769722,-1.90688832081251,30.5286341882147)) ;
#60717 = CARTESIAN_POINT('Ctrl Pts',(6.71954980425477,-1.9059123268808,30.5284313053881)) ;
#60718 = CARTESIAN_POINT('Ctrl Pts',(6.7195425427954,-1.90542716908072,30.5283302412843)) ;
#60719 = CARTESIAN_POINT('Ctrl Pts',(6.71953406025587,-1.90469706627519,30.5281776140417)) ;
#60720 = CARTESIAN_POINT('Ctrl Pts',(6.719531472145,-1.9044367369481,30.528123096389)) ;
#60721 = CARTESIAN_POINT('Ctrl Pts',(6.71952768036084,-1.9039038832069,30.5280111757878)) ;
#60722 = CARTESIAN_POINT('Ctrl Pts',(6.71952647168563,-1.90363135860541,30.5279537739008)) ;
#60723 = CARTESIAN_POINT('Ctrl Pts',(6.71952671038721,-1.90308662224053,30.527838451684)) ;
#60724 = CARTESIAN_POINT('Ctrl Pts',(6.71952806578134,-1.90281444927565,30.5277805598112)) ;
#60725 = CARTESIAN_POINT('Ctrl Pts',(6.7196030061094,-1.90163369649324,30.5275142094095)) ;
#60726 = CARTESIAN_POINT('Ctrl Pts',(6.71960609582335,-1.90158501524993,30.5275032280517)) ;
#60727 = CARTESIAN_POINT('Ctrl Pts',(6.7196091855373,-1.90153633400663,30.527492246694)) ;
#60728 = CARTESIAN_POINT('',(-14.2513506240265,-15.0366437072153,30.8390862093178)) ;
#60729 = CARTESIAN_POINT('',(-14.2782523899391,-15.0366437072153,30.8266401270699)) ;
#60730 = CARTESIAN_POINT('Origin',(0.573544392334142,-21.6462763158694,-1.23969588788644)) ;
#60731 = CARTESIAN_POINT('',(-13.1250168776941,-1.90153624278253,28.3692590890207)) ;
#60732 = CARTESIAN_POINT('Ctrl Pts',(-13.1250168853804,-1.90153633399464,
28.3692591062341)) ;
#60733 = CARTESIAN_POINT('Ctrl Pts',(-13.1250152689507,-1.90158489352019,
28.3692709113022)) ;
#60734 = CARTESIAN_POINT('Ctrl Pts',(-13.1249874709885,-1.90241997831702,
28.3694739246719)) ;
#60735 = CARTESIAN_POINT('Ctrl Pts',(-13.1249998825665,-1.90282053513345,
28.3695593911006)) ;
#60736 = CARTESIAN_POINT('Ctrl Pts',(-13.125011087353,-1.90309401671833,28.3696164802336)) ;
#60737 = CARTESIAN_POINT('Ctrl Pts',(-13.1250358173985,-1.90364137046846,
28.3697296738716)) ;
#60738 = CARTESIAN_POINT('Ctrl Pts',(-13.1250494264321,-1.90391520380722,
28.3697857307775)) ;
#60739 = CARTESIAN_POINT('Ctrl Pts',(-13.1250773667014,-1.90445061563352,
28.3698947199767)) ;
#60740 = CARTESIAN_POINT('Ctrl Pts',(-13.1250917025522,-1.90471219430631,
28.3699476501771)) ;
#60741 = CARTESIAN_POINT('Ctrl Pts',(-13.1251330497042,-1.9054458369876,28.3700955747726)) ;
#60742 = CARTESIAN_POINT('Ctrl Pts',(-13.1251620395678,-1.90593335948141,
28.3701931737557)) ;
#60743 = CARTESIAN_POINT('Ctrl Pts',(-13.1252221711934,-1.90691411034398,
28.3703886754018)) ;
#60744 = CARTESIAN_POINT('Ctrl Pts',(-13.1252533348784,-1.90740733936085,
28.3704865680697)) ;
#60745 = CARTESIAN_POINT('Ctrl Pts',(-13.1253492373837,-1.9088950048919,28.3707809471545)) ;
#60746 = CARTESIAN_POINT('Ctrl Pts',(-13.1254163516026,-1.90989741787098,
28.3709781508729)) ;
#60747 = CARTESIAN_POINT('Ctrl Pts',(-13.1255547019883,-1.91192046573787,
28.3713748005062)) ;
#60748 = CARTESIAN_POINT('Ctrl Pts',(-13.1256259736338,-1.91294109879846,
28.3715742295908)) ;
#60749 = CARTESIAN_POINT('Ctrl Pts',(-13.1257715916628,-1.91499754808388,
28.3719751225115)) ;
#60750 = CARTESIAN_POINT('Ctrl Pts',(-13.1258459404148,-1.91603336435267,
28.3721765852616)) ;
#60751 = CARTESIAN_POINT('Ctrl Pts',(-13.1260725286467,-1.9191590465366,28.3727834866439)) ;
#60752 = CARTESIAN_POINT('Ctrl Pts',(-13.1262282666174,-1.9212671305763,28.3731914550528)) ;
#60753 = CARTESIAN_POINT('Ctrl Pts',(-13.1265451591989,-1.92550764432193,
28.3740104294866)) ;
#60754 = CARTESIAN_POINT('Ctrl Pts',(-13.1267063463805,-1.92764007448401,
28.3744214205466)) ;
#60755 = CARTESIAN_POINT('Ctrl Pts',(-13.1271936927362,-1.93403753623515,
28.3756526816843)) ;
#60756 = CARTESIAN_POINT('Ctrl Pts',(-13.1275235719574,-1.93830268601545,
28.3764712575976)) ;
#60757 = CARTESIAN_POINT('Ctrl Pts',(-13.1281736016328,-1.94663933327223,
28.3780688149077)) ;
#60758 = CARTESIAN_POINT('Ctrl Pts',(-13.1284938184142,-1.95071083142766,
28.3788477657729)) ;
#60759 = CARTESIAN_POINT('Ctrl Pts',(-13.129106438373,-1.95846141009329,28.3803291801374)) ;
#60760 = CARTESIAN_POINT('Ctrl Pts',(-13.1294151360898,-1.96234641865746,
28.3810709957486)) ;
#60761 = CARTESIAN_POINT('Ctrl Pts',(-13.1300368386708,-1.97013989558661,
28.3825579761773)) ;
#60762 = CARTESIAN_POINT('Ctrl Pts',(-13.1303498452033,-1.97404836396523,
28.3833031402261)) ;
#60763 = CARTESIAN_POINT('Ctrl Pts',(-13.1312944889748,-1.98580782013941,
28.3855437839311)) ;
#60764 = CARTESIAN_POINT('Ctrl Pts',(-13.1319317073656,-1.99369285855913,
28.3870444349558)) ;
#60765 = CARTESIAN_POINT('Ctrl Pts',(-13.1332181965959,-2.0095476757302,28.3900594567134)) ;
#60766 = CARTESIAN_POINT('Ctrl Pts',(-13.1338674934606,-2.0175174543069,28.3915738153658)) ;
#60767 = CARTESIAN_POINT('Ctrl Pts',(-13.135176390318,-2.03353569574261,28.3946156827108)) ;
#60768 = CARTESIAN_POINT('Ctrl Pts',(-13.1358359910487,-2.04158415860608,
28.3961431910624)) ;
#60769 = CARTESIAN_POINT('Ctrl Pts',(-13.1378283038094,-2.06583849453389,
28.4007442732752)) ;
#60770 = CARTESIAN_POINT('Ctrl Pts',(-13.1391744335532,-2.08215331147535,
28.4038364464638)) ;
#60771 = CARTESIAN_POINT('Ctrl Pts',(-13.1418947741956,-2.11502504608969,
28.41006292857)) ;
#60772 = CARTESIAN_POINT('Ctrl Pts',(-13.1432690289151,-2.13158196396751,
28.4131972172602)) ;
#60773 = CARTESIAN_POINT('Ctrl Pts',(-13.1460395960048,-2.1648894899987,28.4194996938546)) ;
#60774 = CARTESIAN_POINT('Ctrl Pts',(-13.1474359241405,-2.18164009431291,
28.4226678735906)) ;
#60775 = CARTESIAN_POINT('Ctrl Pts',(-13.1502453305346,-2.21528657066704,
28.4290295617627)) ;
#60776 = CARTESIAN_POINT('Ctrl Pts',(-13.1516584108559,-2.23218244271495,
28.4322230692458)) ;
#60777 = CARTESIAN_POINT('Ctrl Pts',(-13.1559153789589,-2.28301534046843,
28.4418284715407)) ;
#60778 = CARTESIAN_POINT('Ctrl Pts',(-13.158776927892,-2.31709764749398,28.4482652766609)) ;
#60779 = CARTESIAN_POINT('Ctrl Pts',(-13.164510098709,-2.38526237999286,28.4611342536291)) ;
#60780 = CARTESIAN_POINT('Ctrl Pts',(-13.1673817596031,-2.41934479180169,
28.4675664043175)) ;
#60781 = CARTESIAN_POINT('Ctrl Pts',(-13.1730997731453,-2.48712238776894,
28.4803542410124)) ;
#60782 = CARTESIAN_POINT('Ctrl Pts',(-13.1759461420269,-2.52081757197294,
28.4867099195188)) ;
#60783 = CARTESIAN_POINT('Ctrl Pts',(-13.1843953174782,-2.6207413083776,28.5055540107254)) ;
#60784 = CARTESIAN_POINT('Ctrl Pts',(-13.1899080876518,-2.68580804401566,
28.5178195277039)) ;
#60785 = CARTESIAN_POINT('Ctrl Pts',(-13.2009227453959,-2.81566305062235,
28.5422921887985)) ;
#60786 = CARTESIAN_POINT('Ctrl Pts',(-13.2067068091717,-2.8837618261483,28.5551226014694)) ;
#60787 = CARTESIAN_POINT('Ctrl Pts',(-13.2183211631654,-3.02037042177582,
28.580855636929)) ;
#60788 = CARTESIAN_POINT('Ctrl Pts',(-13.2241514889584,-3.08888024195006,
28.5937582432754)) ;
#60789 = CARTESIAN_POINT('Ctrl Pts',(-13.2358547746908,-3.22629766446251,
28.6196343081466)) ;
#60790 = CARTESIAN_POINT('Ctrl Pts',(-13.2417277490524,-3.2952052667871,28.6326077599955)) ;
#60791 = CARTESIAN_POINT('Ctrl Pts',(-13.2535135489871,-3.43340499251651,
28.6586237837857)) ;
#60792 = CARTESIAN_POINT('Ctrl Pts',(-13.2594263764131,-3.50269711592473,
28.6716663548693)) ;
#60793 = CARTESIAN_POINT('Ctrl Pts',(-13.2772211700303,-3.71113037749264,
28.7108948224511)) ;
#60794 = CARTESIAN_POINT('Ctrl Pts',(-13.2891593483695,-3.85082840634055,
28.7371815190198)) ;
#60795 = CARTESIAN_POINT('Ctrl Pts',(-13.3131704391015,-4.13160342849318,
28.7900065741187)) ;
#60796 = CARTESIAN_POINT('Ctrl Pts',(-13.3252434057619,-4.27268042187732,
28.81654490756)) ;
#60797 = CARTESIAN_POINT('Ctrl Pts',(-13.3495113303093,-4.55610729892767,
28.8698549782839)) ;
#60798 = CARTESIAN_POINT('Ctrl Pts',(-13.3617063123166,-4.69845718168438,
28.8966267042002)) ;
#60799 = CARTESIAN_POINT('Ctrl Pts',(-13.3862067189839,-4.98432376133397,
28.9503847487854)) ;
#60800 = CARTESIAN_POINT('Ctrl Pts',(-13.3985121557369,-5.1278404582419,28.977371061863)) ;
#60801 = CARTESIAN_POINT('Ctrl Pts',(-13.4232226290045,-5.41593459280462,
29.0315391438259)) ;
#60802 = CARTESIAN_POINT('Ctrl Pts',(-13.4356276714463,-5.5605120304571,29.0587209099683)) ;
#60803 = CARTESIAN_POINT('Ctrl Pts',(-13.4605269614328,-5.85062157360454,
29.1132605538531)) ;
#60804 = CARTESIAN_POINT('Ctrl Pts',(-13.4730212100494,-5.99615367910082,
29.1406184310989)) ;
#60805 = CARTESIAN_POINT('Ctrl Pts',(-13.5106226096791,-6.43402288850668,
29.2229270113459)) ;
#60806 = CARTESIAN_POINT('Ctrl Pts',(-13.5358483446402,-6.72763288063727,
29.2781126940939)) ;
#60807 = CARTESIAN_POINT('Ctrl Pts',(-13.5865374915687,-7.31739864982827,
29.3889537854771)) ;
#60808 = CARTESIAN_POINT('Ctrl Pts',(-13.6120009385329,-7.61355442692234,
29.4446091779287)) ;
#60809 = CARTESIAN_POINT('Ctrl Pts',(-13.6630887777036,-8.20756318104024,
29.5562319618921)) ;
#60810 = CARTESIAN_POINT('Ctrl Pts',(-13.6887131872509,-8.5054161580608,29.6121993453803)) ;
#60811 = CARTESIAN_POINT('Ctrl Pts',(-13.7400472188843,-9.10197072784479,
29.72428792256)) ;
#60812 = CARTESIAN_POINT('Ctrl Pts',(-13.7657568490879,-9.40067232061517,
29.7804091124971)) ;
#60813 = CARTESIAN_POINT('Ctrl Pts',(-13.8429009085766,-10.2967771471123,
29.9487656754132)) ;
#60814 = CARTESIAN_POINT('Ctrl Pts',(-13.8943503623133,-10.8941804135972,
30.0609941047966)) ;
#60815 = CARTESIAN_POINT('Ctrl Pts',(-13.9966930472064,-12.0821983511367,
30.2841625050184)) ;
#60816 = CARTESIAN_POINT('Ctrl Pts',(-14.0475863486027,-12.6728130222429,
30.395102443371)) ;
#60817 = CARTESIAN_POINT('Ctrl Pts',(-14.1497718947981,-13.858425809999,30.6177958799877)) ;
#60818 = CARTESIAN_POINT('Ctrl Pts',(-14.201028282145,-14.452999812307,30.7294693948825)) ;
#60819 = CARTESIAN_POINT('Ctrl Pts',(-14.2513506239133,-15.0366437072152,
30.8390862093702)) ;
#60820 = CARTESIAN_POINT('Ctrl Pts',(-14.2782523900534,-15.0366437072152,
30.826640127017)) ;
#60821 = CARTESIAN_POINT('Ctrl Pts',(-14.2767312222616,-15.019224461707,30.8233774515699)) ;
#60822 = CARTESIAN_POINT('Ctrl Pts',(-14.2752091967655,-15.0017954800496,
30.820112955973)) ;
#60823 = CARTESIAN_POINT('Ctrl Pts',(-14.2241842264702,-14.4175024634034,
30.7106734040413)) ;
#60824 = CARTESIAN_POINT('Ctrl Pts',(-14.1737849268775,-13.8404650781122,
30.6025965267698)) ;
#60825 = CARTESIAN_POINT('Ctrl Pts',(-14.0717790076265,-12.6728130216194,
30.3839097272942)) ;
#60826 = CARTESIAN_POINT('Ctrl Pts',(-14.0201724215192,-12.0821983504207,
30.2732997895684)) ;
#60827 = CARTESIAN_POINT('Ctrl Pts',(-13.9163371854979,-10.894180412695,30.0508219169878)) ;
#60828 = CARTESIAN_POINT('Ctrl Pts',(-13.8641086058156,-10.2967771461165,
29.9389539496297)) ;
#60829 = CARTESIAN_POINT('Ctrl Pts',(-13.7857356278822,-9.40067231947891,
29.7711659448977)) ;
#60830 = CARTESIAN_POINT('Ctrl Pts',(-13.7596062483987,-9.10197072666172,
29.7152389516462)) ;
#60831 = CARTESIAN_POINT('Ctrl Pts',(-13.7074095360729,-8.50541615678423,
29.6035494930342)) ;
#60832 = CARTESIAN_POINT('Ctrl Pts',(-13.6813422113468,-8.20756317971701,
29.5477870239176)) ;
#60833 = CARTESIAN_POINT('Ctrl Pts',(-13.6293411273122,-7.61355442550602,
29.4365867519988)) ;
#60834 = CARTESIAN_POINT('Ctrl Pts',(-13.6034073853457,-7.31739864836555,
29.3811489411741)) ;
#60835 = CARTESIAN_POINT('Ctrl Pts',(-13.5517439698451,-6.72763287908212,
29.2707585944094)) ;
#60836 = CARTESIAN_POINT('Ctrl Pts',(-13.5260143313033,-6.43402288690552,
29.2158060422727)) ;
#60837 = CARTESIAN_POINT('Ctrl Pts',(-13.4876244850302,-5.99615367743104,
29.1338622362707)) ;
#60838 = CARTESIAN_POINT('Ctrl Pts',(-13.4748619542748,-5.85062157191195,
29.1066284795542)) ;
#60839 = CARTESIAN_POINT('Ctrl Pts',(-13.4494133660394,-5.56051202871903,
29.0523429680906)) ;
#60840 = CARTESIAN_POINT('Ctrl Pts',(-13.4367273096283,-5.41593459104392,
29.0252912128496)) ;
#60841 = CARTESIAN_POINT('Ctrl Pts',(-13.4114396744369,-5.12784045643605,
28.9713901544167)) ;
#60842 = CARTESIAN_POINT('Ctrl Pts',(-13.3988381015846,-4.9843237595056,28.944540848483)) ;
#60843 = CARTESIAN_POINT('Ctrl Pts',(-13.3737269870879,-4.69845717981123,
28.8910653474164)) ;
#60844 = CARTESIAN_POINT('Ctrl Pts',(-13.361217457538,-4.5561072970322,28.8644391466846)) ;
#60845 = CARTESIAN_POINT('Ctrl Pts',(-13.3362972659841,-4.27268041993744,
28.8114308468023)) ;
#60846 = CARTESIAN_POINT('Ctrl Pts',(-13.3238866282584,-4.13160342653121,
28.7850487366265)) ;
#60847 = CARTESIAN_POINT('Ctrl Pts',(-13.2991698265207,-3.85082840433457,
28.7325501781962)) ;
#60848 = CARTESIAN_POINT('Ctrl Pts',(-13.2868637167631,-3.71113037546474,
28.7064337048231)) ;
#60849 = CARTESIAN_POINT('Ctrl Pts',(-13.2684853726168,-3.50269711386417,
28.6674752164577)) ;
#60850 = CARTESIAN_POINT('Ctrl Pts',(-13.2623727032127,-3.43340499044509,
28.6545251021161)) ;
#60851 = CARTESIAN_POINT('Ctrl Pts',(-13.2501742422854,-3.29520526469404,
28.6286999956262)) ;
#60852 = CARTESIAN_POINT('Ctrl Pts',(-13.2440884526162,-3.22629766235862,
28.6158250026206)) ;
#60853 = CARTESIAN_POINT('Ctrl Pts',(-13.2319432445035,-3.08888023982465,
28.5901533928093)) ;
#60854 = CARTESIAN_POINT('Ctrl Pts',(-13.2258838404854,-3.02037041963968,
28.5773567693331)) ;
#60855 = CARTESIAN_POINT('Ctrl Pts',(-13.2137900707746,-2.88376182399075,
28.5518455351981)) ;
#60856 = CARTESIAN_POINT('Ctrl Pts',(-13.2077557406446,-2.81566304845413,
28.5391309080698)) ;
#60857 = CARTESIAN_POINT('Ctrl Pts',(-13.1962343453602,-2.68580804224111,
28.5148926888158)) ;
#60858 = CARTESIAN_POINT('Ctrl Pts',(-13.1904549255703,-2.62074130702757,
28.5027505371832)) ;
#60859 = CARTESIAN_POINT('Ctrl Pts',(-13.1815625546521,-2.52081757127485,
28.4841114901825)) ;
#60860 = CARTESIAN_POINT('Ctrl Pts',(-13.1785611978528,-2.4871223872907,28.4778275167724)) ;
#60861 = CARTESIAN_POINT('Ctrl Pts',(-13.1725165575394,-2.41934479176566,
28.4651907938141)) ;
#60862 = CARTESIAN_POINT('Ctrl Pts',(-13.169473290243,-2.38526238017923,28.4588380367523)) ;
#60863 = CARTESIAN_POINT('Ctrl Pts',(-13.163376620504,-2.31709764812506,28.4461372323948)) ;
#60864 = CARTESIAN_POINT('Ctrl Pts',(-13.1603232594475,-2.28301534132186,
28.4397891690633)) ;
#60865 = CARTESIAN_POINT('Ctrl Pts',(-13.1557582890889,-2.23218244390001,
28.4303262638613)) ;
#60866 = CARTESIAN_POINT('Ctrl Pts',(-13.1542391276856,-2.21528657196237,
28.427181834738)) ;
#60867 = CARTESIAN_POINT('Ctrl Pts',(-13.1512092615423,-2.18164009582775,
28.420922142157)) ;
#60868 = CARTESIAN_POINT('Ctrl Pts',(-13.1496985588601,-2.16488949162284,
28.4178068777459)) ;
#60869 = CARTESIAN_POINT('Ctrl Pts',(-13.146688677501,-2.13158196580896,28.411615119772)) ;
#60870 = CARTESIAN_POINT('Ctrl Pts',(-13.1451895152596,-2.11502504803915,
28.4085386194796)) ;
#60871 = CARTESIAN_POINT('Ctrl Pts',(-13.142205038103,-2.08215331363928,28.4024343399867)) ;
#60872 = CARTESIAN_POINT('Ctrl Pts',(-13.1407197669701,-2.06583849680426,
28.3994065404838)) ;
#60873 = CARTESIAN_POINT('Ctrl Pts',(-13.1385027926659,-2.0415841610347,28.3949093978052)) ;
#60874 = CARTESIAN_POINT('Ctrl Pts',(-13.13776560024,-2.03353569822372,28.3934177872064)) ;
#60875 = CARTESIAN_POINT('Ctrl Pts',(-13.1362945662569,-2.01751745689249,
28.3904509325074)) ;
#60876 = CARTESIAN_POINT('Ctrl Pts',(-13.1355607254437,-2.00954767836777,
28.3889756880625)) ;
#60877 = CARTESIAN_POINT('Ctrl Pts',(-13.1340956457591,-1.99369286130014,
28.386043291071)) ;
#60878 = CARTESIAN_POINT('Ctrl Pts',(-13.1333644329482,-1.98580782293182,
28.3845861265074)) ;
#60879 = CARTESIAN_POINT('Ctrl Pts',(-13.1322682487679,-1.97404836683433,
28.3824155928787)) ;
#60880 = CARTESIAN_POINT('Ctrl Pts',(-13.1319029491467,-1.97013989848118,
28.3816946221949)) ;
#60881 = CARTESIAN_POINT('Ctrl Pts',(-13.1311721108169,-1.96234642160287,
28.3802581333518)) ;
#60882 = CARTESIAN_POINT('Ctrl Pts',(-13.1308065737453,-1.95846141306429,
28.3795426144322)) ;
#60883 = CARTESIAN_POINT('Ctrl Pts',(-13.130074097652,-1.95071083402189,28.3781166513345)) ;
#60884 = CARTESIAN_POINT('Ctrl Pts',(-13.1296877147739,-1.94663933544429,
28.3773683120693)) ;
#60885 = CARTESIAN_POINT('Ctrl Pts',(-13.128890937428,-1.93830268732315,28.3758386472643)) ;
#60886 = CARTESIAN_POINT('Ctrl Pts',(-13.1284806092105,-1.93403753710027,
28.3750572909193)) ;
#60887 = CARTESIAN_POINT('Ctrl Pts',(-13.1278576899737,-1.92764007468588,
28.3738887523245)) ;
#60888 = CARTESIAN_POINT('Ctrl Pts',(-13.1276487985248,-1.92550764430288,
28.3734998315585)) ;
#60889 = CARTESIAN_POINT('Ctrl Pts',(-13.1272297591529,-1.92126713011769,
28.3727281151621)) ;
#60890 = CARTESIAN_POINT('Ctrl Pts',(-13.127019643716,-1.91915904585948,28.3723453043983)) ;
#60891 = CARTESIAN_POINT('Ctrl Pts',(-13.1267037765904,-1.91603336335157,
28.3717797077569)) ;
#60892 = CARTESIAN_POINT('Ctrl Pts',(-13.1265983616708,-1.9149975469756,28.3715926177219)) ;
#60893 = CARTESIAN_POINT('Ctrl Pts',(-13.1263870873875,-1.91294109747722,
28.3712221005706)) ;
#60894 = CARTESIAN_POINT('Ctrl Pts',(-13.1262812303145,-1.91192046431214,
28.3710386723848)) ;
#60895 = CARTESIAN_POINT('Ctrl Pts',(-13.1260684851354,-1.90989741623553,
28.3706764414003)) ;
#60896 = CARTESIAN_POINT('Ctrl Pts',(-13.1259616328263,-1.90889500315093,
28.3704976224562)) ;
#60897 = CARTESIAN_POINT('Ctrl Pts',(-13.1257993541946,-1.90740733746617,
28.3702339522025)) ;
#60898 = CARTESIAN_POINT('Ctrl Pts',(-13.1257449190146,-1.90691410839945,
28.3701468260634)) ;
#60899 = CARTESIAN_POINT('Ctrl Pts',(-13.1256348434522,-1.90593335743554,
28.3699744309199)) ;
#60900 = CARTESIAN_POINT('Ctrl Pts',(-13.1255792249402,-1.90544583488841,
28.3698891516492)) ;
#60901 = CARTESIAN_POINT('Ctrl Pts',(-13.1254932500023,-1.90471219217896,
28.3697618740597)) ;
#60902 = CARTESIAN_POINT('Ctrl Pts',(-13.1254621892913,-1.90445061353546,
28.3697166816103)) ;
#60903 = CARTESIAN_POINT('Ctrl Pts',(-13.1253972100148,-1.90391520175604,
28.3696248284912)) ;
#60904 = CARTESIAN_POINT('Ctrl Pts',(-13.1253632960718,-1.9036413684333,28.3695781656405)) ;
#60905 = CARTESIAN_POINT('Ctrl Pts',(-13.1252930340526,-1.90309401473251,
28.3694860373478)) ;
#60906 = CARTESIAN_POINT('Ctrl Pts',(-13.1252567766583,-1.90282053317478,
28.3694405387916)) ;
#60907 = CARTESIAN_POINT('Ctrl Pts',(-13.1250350734088,-1.90163369914819,
28.369272862051)) ;
#60908 = CARTESIAN_POINT('Ctrl Pts',(-13.1250259793946,-1.90158501657141,
28.3692659841426)) ;
#60909 = CARTESIAN_POINT('Ctrl Pts',(-13.1250168853804,-1.90153633399464,
28.3692591062341)) ;
#60910 = CARTESIAN_POINT('',(-25.8831717248504,-15.0366437072153,22.0048097991458)) ;
#60911 = CARTESIAN_POINT('',(-25.9023611320428,-15.0366437072153,21.98221828251)) ;
#60912 = CARTESIAN_POINT('Origin',(1.04106958514517,-21.6462763158693,-0.884292476110772)) ;
#60913 = CARTESIAN_POINT('',(-23.8238854115647,-1.90153624079472,20.2361906783538)) ;
#60914 = CARTESIAN_POINT('Ctrl Pts',(-23.8238854254577,-1.90153633001901,
20.23619069048)) ;
#60915 = CARTESIAN_POINT('Ctrl Pts',(-23.8238889212641,-1.90158489068798,
20.23620207647)) ;
#60916 = CARTESIAN_POINT('Ctrl Pts',(-23.8239492198937,-1.9024225062293,20.2363984716666)) ;
#60917 = CARTESIAN_POINT('Ctrl Pts',(-23.8239965310121,-1.90282422971975,
20.2364710111718)) ;
#60918 = CARTESIAN_POINT('Ctrl Pts',(-23.8240307835122,-1.90309850720873,
20.2365182410673)) ;
#60919 = CARTESIAN_POINT('Ctrl Pts',(-23.8241009836495,-1.90364745287506,
20.2366108299045)) ;
#60920 = CARTESIAN_POINT('Ctrl Pts',(-23.8241369875051,-1.90392208221389,
20.2366561102625)) ;
#60921 = CARTESIAN_POINT('Ctrl Pts',(-23.8242083345894,-1.90445904989118,
20.2367435251871)) ;
#60922 = CARTESIAN_POINT('Ctrl Pts',(-23.8242436812157,-1.90472138841956,
20.236785655814)) ;
#60923 = CARTESIAN_POINT('Ctrl Pts',(-23.8243436342305,-1.90545718379177,
20.2369028631524)) ;
#60924 = CARTESIAN_POINT('Ctrl Pts',(-23.8244111378045,-1.90594614422066,
20.2369794780989)) ;
#60925 = CARTESIAN_POINT('Ctrl Pts',(-23.8245482298291,-1.90692978769714,
20.2371320802637)) ;
#60926 = CARTESIAN_POINT('Ctrl Pts',(-23.8246178340023,-1.90742447139286,
20.2372080491789)) ;
#60927 = CARTESIAN_POINT('Ctrl Pts',(-23.8248291351697,-1.90891652441222,
20.2374355804445)) ;
#60928 = CARTESIAN_POINT('Ctrl Pts',(-23.8249732947336,-1.90992189364657,
20.2375867973708)) ;
#60929 = CARTESIAN_POINT('Ctrl Pts',(-23.825266307357,-1.91195090760971,20.2378895395296)) ;
#60930 = CARTESIAN_POINT('Ctrl Pts',(-23.8254151855814,-1.9129745505112,20.2380410345524)) ;
#60931 = CARTESIAN_POINT('Ctrl Pts',(-23.8257165959959,-1.91503706413992,
20.2383445838546)) ;
#60932 = CARTESIAN_POINT('Ctrl Pts',(-23.8258691298177,-1.91607593490945,
20.2384966362262)) ;
#60933 = CARTESIAN_POINT('Ctrl Pts',(-23.8263310116615,-1.91921083418716,
20.2389535916698)) ;
#60934 = CARTESIAN_POINT('Ctrl Pts',(-23.8266446075399,-1.9213251344095,20.2392593264881)) ;
#60935 = CARTESIAN_POINT('Ctrl Pts',(-23.827278005508,-1.92557815197685,20.2398712840593)) ;
#60936 = CARTESIAN_POINT('Ctrl Pts',(-23.8275978309142,-1.9277168697781,20.2401774795076)) ;
#60937 = CARTESIAN_POINT('Ctrl Pts',(-23.8285600272612,-1.93413319445796,
20.2410929181444)) ;
#60938 = CARTESIAN_POINT('Ctrl Pts',(-23.8292050669925,-1.93841091953424,
20.241699057121)) ;
#60939 = CARTESIAN_POINT('Ctrl Pts',(-23.8304696089694,-1.9467721457928,20.2428793998365)) ;
#60940 = CARTESIAN_POINT('Ctrl Pts',(-23.8310891586715,-1.95085564765416,
20.2434535479221)) ;
#60941 = CARTESIAN_POINT('Ctrl Pts',(-23.8322707390319,-1.9586291805441,20.2445439567061)) ;
#60942 = CARTESIAN_POINT('Ctrl Pts',(-23.8328641758305,-1.96252574723342,
20.245089173699)) ;
#60943 = CARTESIAN_POINT('Ctrl Pts',(-23.8340563782582,-1.97034241017641,
20.246180845225)) ;
#60944 = CARTESIAN_POINT('Ctrl Pts',(-23.8346551450615,-1.9742625064435,20.2467272983799)) ;
#60945 = CARTESIAN_POINT('Ctrl Pts',(-23.8364587317813,-1.98605694755246,
20.2483689818616)) ;
#60946 = CARTESIAN_POINT('Ctrl Pts',(-23.8376708072141,-1.99396544428758,
20.249466572326)) ;
#60947 = CARTESIAN_POINT('Ctrl Pts',(-23.8401117020587,-2.00986743013604,
20.2516691720465)) ;
#60948 = CARTESIAN_POINT('Ctrl Pts',(-23.8413405400649,-2.0178609190749,20.2527741593558)) ;
#60949 = CARTESIAN_POINT('Ctrl Pts',(-23.8438131290869,-2.03392681527835,
20.254991769387)) ;
#60950 = CARTESIAN_POINT('Ctrl Pts',(-23.8450568806311,-2.04199922254737,
20.2561043914876)) ;
#60951 = CARTESIAN_POINT('Ctrl Pts',(-23.8488082444504,-2.06632571575214,
20.2594534651195)) ;
#60952 = CARTESIAN_POINT('Ctrl Pts',(-23.8513358992443,-2.08268906962494,
20.2617012013615)) ;
#60953 = CARTESIAN_POINT('Ctrl Pts',(-23.8564345078822,-2.11565859823547,
20.2662232117135)) ;
#60954 = CARTESIAN_POINT('Ctrl Pts',(-23.8590054930501,-2.13226477317813,
20.2684974490114)) ;
#60955 = CARTESIAN_POINT('Ctrl Pts',(-23.8641818125931,-2.16567138944634,
20.2730674984476)) ;
#60956 = CARTESIAN_POINT('Ctrl Pts',(-23.866787157862,-2.18247182693246,20.2753632965351)) ;
#60957 = CARTESIAN_POINT('Ctrl Pts',(-23.8720237580892,-2.21621840171076,
20.2799708998623)) ;
#60958 = CARTESIAN_POINT('Ctrl Pts',(-23.8746550145169,-2.23316453901088,
20.2822827033741)) ;
#60959 = CARTESIAN_POINT('Ctrl Pts',(-23.8825753927727,-2.28414866460182,
20.289233302234)) ;
#60960 = CARTESIAN_POINT('Ctrl Pts',(-23.8878910763925,-2.31833236629326,
20.2938873413591)) ;
#60961 = CARTESIAN_POINT('Ctrl Pts',(-23.8985296507322,-2.38669988812742,
20.3031869725674)) ;
#60962 = CARTESIAN_POINT('Ctrl Pts',(-23.9038525680176,-2.42088369460506,
20.3078325290128)) ;
#60963 = CARTESIAN_POINT('Ctrl Pts',(-23.9144431540245,-2.48886292769985,
20.3170647066451)) ;
#60964 = CARTESIAN_POINT('Ctrl Pts',(-23.9197108343457,-2.52265835436257,
20.3216513141901)) ;
#60965 = CARTESIAN_POINT('Ctrl Pts',(-23.9353381111146,-2.6228793615095,20.3352460832032)) ;
#60966 = CARTESIAN_POINT('Ctrl Pts',(-23.9455218681759,-2.68813966879725,
20.344089279458)) ;
#60967 = CARTESIAN_POINT('Ctrl Pts',(-23.9658579668207,-2.8184007703173,20.3617298151846)) ;
#60968 = CARTESIAN_POINT('Ctrl Pts',(-23.9765296668213,-2.88672197974776,
20.3709756639712)) ;
#60969 = CARTESIAN_POINT('Ctrl Pts',(-23.9979455672397,-3.02377678576226,
20.3895136499768)) ;
#60970 = CARTESIAN_POINT('Ctrl Pts',(-24.0086897931138,-3.09251038241904,
20.3988057572494)) ;
#60971 = CARTESIAN_POINT('Ctrl Pts',(-24.0302469042348,-3.23037665716361,
20.4174365347916)) ;
#60972 = CARTESIAN_POINT('Ctrl Pts',(-24.0410597997926,-3.29950933523776,
20.4267751929177)) ;
#60973 = CARTESIAN_POINT('Ctrl Pts',(-24.0627509880244,-3.43816046842335,
20.4454986657553)) ;
#60974 = CARTESIAN_POINT('Ctrl Pts',(-24.0736292820235,-3.50767892353821,
20.4548834789066)) ;
#60975 = CARTESIAN_POINT('Ctrl Pts',(-24.1063578732419,-3.71679299919776,
20.4831059472441)) ;
#60976 = CARTESIAN_POINT('Ctrl Pts',(-24.1283018087199,-3.8569473294019,20.5020117146455)) ;
#60977 = CARTESIAN_POINT('Ctrl Pts',(-24.1724183592319,-4.13863945838501,
20.5399956588899)) ;
#60978 = CARTESIAN_POINT('Ctrl Pts',(-24.194591013067,-4.28017725724343,20.5590737900776)) ;
#60979 = CARTESIAN_POINT('Ctrl Pts',(-24.2391457094888,-4.56452990289024,
20.5973912011102)) ;
#60980 = CARTESIAN_POINT('Ctrl Pts',(-24.2615277692301,-4.70734474876847,
20.6166304604686)) ;
#60981 = CARTESIAN_POINT('Ctrl Pts',(-24.306482840028,-4.99414506583698,20.6552578617666)) ;
#60982 = CARTESIAN_POINT('Ctrl Pts',(-24.3290558597318,-5.13813053704231,
20.6746459935306)) ;
#60983 = CARTESIAN_POINT('Ctrl Pts',(-24.3743749176294,-5.42716568490539,
20.7135582803702)) ;
#60984 = CARTESIAN_POINT('Ctrl Pts',(-24.3971209600605,-5.57221536156083,
20.7330824304562)) ;
#60985 = CARTESIAN_POINT('Ctrl Pts',(-24.442768450973,-5.86327250094969,20.7722535176391)) ;
#60986 = CARTESIAN_POINT('Ctrl Pts',(-24.4656699002175,-6.00927996368441,
20.7919004538369)) ;
#60987 = CARTESIAN_POINT('Ctrl Pts',(-24.5345812515141,-6.44857940245386,
20.8510052199905)) ;
#60988 = CARTESIAN_POINT('Ctrl Pts',(-24.580798106769,-6.7431484243555,20.8906270652943)) ;
#60989 = CARTESIAN_POINT('Ctrl Pts',(-24.673646087651,-7.3348405683828,20.9701983608142)) ;
#60990 = CARTESIAN_POINT('Ctrl Pts',(-24.7202772382944,-7.63196369054212,
21.0101477815896)) ;
#60991 = CARTESIAN_POINT('Ctrl Pts',(-24.8138175020744,-8.22791267832212,
21.0902629313793)) ;
#60992 = CARTESIAN_POINT('Ctrl Pts',(-24.8607266276025,-8.52673854393955,
21.1304286458044)) ;
#60993 = CARTESIAN_POINT('Ctrl Pts',(-24.9546872472594,-9.12524166268665,
21.2108642459101)) ;
#60994 = CARTESIAN_POINT('Ctrl Pts',(-25.001738747189,-9.42491891582326,21.2511341247632)) ;
#60995 = CARTESIAN_POINT('Ctrl Pts',(-25.142904087342,-10.3239507234301,21.3719310144489)) ;
#60996 = CARTESIAN_POINT('Ctrl Pts',(-25.2370286632435,-10.9233053106647,
21.4524453967184)) ;
#60997 = CARTESIAN_POINT('Ctrl Pts',(-25.4242285326933,-12.1152037156214,
21.6125353332349)) ;
#60998 = CARTESIAN_POINT('Ctrl Pts',(-25.5173038764335,-12.707747533395,21.6921108284061)) ;
#60999 = CARTESIAN_POINT('Ctrl Pts',(-25.7018585299048,-13.8825790582674,
21.8498668522659)) ;
#61000 = CARTESIAN_POINT('Ctrl Pts',(-25.7933256204984,-14.4647882728862,
21.9280367100096)) ;
#61001 = CARTESIAN_POINT('Ctrl Pts',(-25.8831717248474,-15.0366437072153,
22.0048097991493)) ;
#61002 = CARTESIAN_POINT('Ctrl Pts',(-25.9023611320459,-15.0366437072153,
21.9822182825064)) ;
#61003 = CARTESIAN_POINT('Ctrl Pts',(-25.9018452635895,-15.0333766937121,
21.9817827114191)) ;
#61004 = CARTESIAN_POINT('Ctrl Pts',(-25.9013293415857,-15.0301093422777,
21.9813470954983)) ;
#61005 = CARTESIAN_POINT('Ctrl Pts',(-25.8110134109735,-14.4581357186702,
21.90508940013)) ;
#61006 = CARTESIAN_POINT('Ctrl Pts',(-25.7195946111273,-13.8792135350187,
21.8279119784973)) ;
#61007 = CARTESIAN_POINT('Ctrl Pts',(-25.5345906631916,-12.7077475336248,
21.6717592497823)) ;
#61008 = CARTESIAN_POINT('Ctrl Pts',(-25.4410055390766,-12.1152037158853,
21.592783914476)) ;
#61009 = CARTESIAN_POINT('Ctrl Pts',(-25.2527389751069,-10.9233053109973,
21.4339497878536)) ;
#61010 = CARTESIAN_POINT('Ctrl Pts',(-25.1580575854303,-10.3239507237972,
21.3540909374484)) ;
#61011 = CARTESIAN_POINT('Ctrl Pts',(-25.0160140002822,-9.42491891624215,
21.2343279977195)) ;
#61012 = CARTESIAN_POINT('Ctrl Pts',(-24.9686625301724,-9.12524166312279,
21.1944112710693)) ;
#61013 = CARTESIAN_POINT('Ctrl Pts',(-24.8740854099916,-8.52673854441016,
21.114701471501)) ;
#61014 = CARTESIAN_POINT('Ctrl Pts',(-24.826859765719,-8.22791267880993,21.0749083917548)) ;
#61015 = CARTESIAN_POINT('Ctrl Pts',(-24.7326668804222,-7.63196369106424,
20.9955615674227)) ;
#61016 = CARTESIAN_POINT('Ctrl Pts',(-24.6856996517898,-7.33484056892204,
20.956007808249)) ;
#61017 = CARTESIAN_POINT('Ctrl Pts',(-24.5921554552203,-6.74314842492882,
20.8772561612121)) ;
#61018 = CARTESIAN_POINT('Ctrl Pts',(-24.5455785122871,-6.44857940304413,
20.8380582439013)) ;
#61019 = CARTESIAN_POINT('Ctrl Pts',(-24.4761037454443,-6.00927996429998,
20.779616781815)) ;
#61020 = CARTESIAN_POINT('Ctrl Pts',(-24.4530105855386,-5.86327250157364,
20.7601955448585)) ;
#61021 = CARTESIAN_POINT('Ctrl Pts',(-24.406970575575,-5.57221536220158,20.7214865668323)) ;
#61022 = CARTESIAN_POINT('Ctrl Pts',(-24.3840237262814,-5.42716568555446,
20.7021988248636)) ;
#61023 = CARTESIAN_POINT('Ctrl Pts',(-24.3382922419094,-5.13813053770804,
20.6637720840111)) ;
#61024 = CARTESIAN_POINT('Ctrl Pts',(-24.3155076110681,-4.994145066511,20.6446330801402)) ;
#61025 = CARTESIAN_POINT('Ctrl Pts',(-24.2701161458643,-4.70734474945901,
20.6065194420599)) ;
#61026 = CARTESIAN_POINT('Ctrl Pts',(-24.2475093201436,-4.56452990358902,
20.5875447976717)) ;
#61027 = CARTESIAN_POINT('Ctrl Pts',(-24.2024885349213,-4.28017725795857,
20.5497761088005)) ;
#61028 = CARTESIAN_POINT('Ctrl Pts',(-24.1800745928605,-4.13863945910828,
20.530982044075)) ;
#61029 = CARTESIAN_POINT('Ctrl Pts',(-24.1354537656291,-3.85694733014141,
20.4935917802858)) ;
#61030 = CARTESIAN_POINT('Ctrl Pts',(-24.1132469192356,-3.71679299994535,
20.474995535545)) ;
#61031 = CARTESIAN_POINT('Ctrl Pts',(-24.0801013421189,-3.50767892429782,
20.447263980962)) ;
#61032 = CARTESIAN_POINT('Ctrl Pts',(-24.0690802474695,-3.43816046918698,
20.4380472857343)) ;
#61033 = CARTESIAN_POINT('Ctrl Pts',(-24.0470941841408,-3.29950933600938,
20.4196709667008)) ;
#61034 = CARTESIAN_POINT('Ctrl Pts',(-24.0361292167885,-3.2303766579392,20.4105113413331)) ;
#61035 = CARTESIAN_POINT('Ctrl Pts',(-24.0142563188986,-3.09251038320258,
20.3922523367185)) ;
#61036 = CARTESIAN_POINT('Ctrl Pts',(-24.0033483986767,-3.02377678654973,
20.3831529453317)) ;
#61037 = CARTESIAN_POINT('Ctrl Pts',(-23.9815899152853,-2.88672198054314,
20.365018279184)) ;
#61038 = CARTESIAN_POINT('Ctrl Pts',(-23.9707393775487,-2.81840077111661,
20.355982974458)) ;
#61039 = CARTESIAN_POINT('Ctrl Pts',(-23.9500412143655,-2.6881396694976,20.3387686940272)) ;
#61040 = CARTESIAN_POINT('Ctrl Pts',(-23.9396669651916,-2.62287936210179,
20.33014976239)) ;
#61041 = CARTESIAN_POINT('Ctrl Pts',(-23.9237230744987,-2.52265835478894,
20.3169277400514)) ;
#61042 = CARTESIAN_POINT('Ctrl Pts',(-23.9183446726732,-2.4888629280703,20.3124714839205)) ;
#61043 = CARTESIAN_POINT('Ctrl Pts',(-23.9075207487582,-2.42088369486294,
20.3035140128745)) ;
#61044 = CARTESIAN_POINT('Ctrl Pts',(-23.9020752382555,-2.3866998883287,20.2990127843041)) ;
#61045 = CARTESIAN_POINT('Ctrl Pts',(-23.8911769857135,-2.31833236638135,
20.2900188698735)) ;
#61046 = CARTESIAN_POINT('Ctrl Pts',(-23.8857242745468,-2.28414866463331,
20.2855261520298)) ;
#61047 = CARTESIAN_POINT('Ctrl Pts',(-23.8775838646232,-2.23316453895799,
20.2788345944482)) ;
#61048 = CARTESIAN_POINT('Ctrl Pts',(-23.8748768256776,-2.21621840162983,
20.2766120090047)) ;
#61049 = CARTESIAN_POINT('Ctrl Pts',(-23.8694827328601,-2.18247182679563,
20.2721898202708)) ;
#61050 = CARTESIAN_POINT('Ctrl Pts',(-23.8667956804559,-2.16567138928169,
20.2699902152505)) ;
#61051 = CARTESIAN_POINT('Ctrl Pts',(-23.8614483991428,-2.13226477295818,
20.2656214375521)) ;
#61052 = CARTESIAN_POINT('Ctrl Pts',(-23.8587881823468,-2.11565859798799,
20.2634522518394)) ;
#61053 = CARTESIAN_POINT('Ctrl Pts',(-23.8535008795025,-2.08268906932289,
20.2591523894634)) ;
#61054 = CARTESIAN_POINT('Ctrl Pts',(-23.850873824714,-2.06632571542302,20.2570216759331)) ;
#61055 = CARTESIAN_POINT('Ctrl Pts',(-23.8469619668925,-2.041999222178,20.2538615504348)) ;
#61056 = CARTESIAN_POINT('Ctrl Pts',(-23.8456627852911,-2.03392681489554,
20.2528141856382)) ;
#61057 = CARTESIAN_POINT('Ctrl Pts',(-23.8430743685028,-2.0178609186655,20.2507329385867)) ;
#61058 = CARTESIAN_POINT('Ctrl Pts',(-23.8417851338501,-2.0098674297134,20.2496990557024)) ;
#61059 = CARTESIAN_POINT('Ctrl Pts',(-23.8392166571814,-1.99396544383862,
20.2476466569085)) ;
#61060 = CARTESIAN_POINT('Ctrl Pts',(-23.8379374338061,-1.9860569470905,20.2466281191092)) ;
#61061 = CARTESIAN_POINT('Ctrl Pts',(-23.8360255891411,-1.974262505962,20.2451138867272)) ;
#61062 = CARTESIAN_POINT('Ctrl Pts',(-23.8353894649892,-1.97034240968838,
20.244611414041)) ;
#61063 = CARTESIAN_POINT('Ctrl Pts',(-23.8341192976822,-1.96252574673243,
20.2436115298626)) ;
#61064 = CARTESIAN_POINT('Ctrl Pts',(-23.833485255703,-1.95862918003667,20.2431141169819)) ;
#61065 = CARTESIAN_POINT('Ctrl Pts',(-23.8322180529177,-1.95085564685803,
20.242124510617)) ;
#61066 = CARTESIAN_POINT('Ctrl Pts',(-23.831551236331,-1.94677214470025,20.2416060093154)) ;
#61067 = CARTESIAN_POINT('Ctrl Pts',(-23.8301818626089,-1.93841091783493,
20.2405490838777)) ;
#61068 = CARTESIAN_POINT('Ctrl Pts',(-23.8294793527083,-1.93413319244849,
20.2400106039159)) ;
#61069 = CARTESIAN_POINT('Ctrl Pts',(-23.8284203074574,-1.92771686730304,
20.2392091844746)) ;
#61070 = CARTESIAN_POINT('Ctrl Pts',(-23.8280664036579,-1.92557814934648,
20.238943109163)) ;
#61071 = CARTESIAN_POINT('Ctrl Pts',(-23.8273600352524,-1.9213251314707,20.2384170589335)) ;
#61072 = CARTESIAN_POINT('Ctrl Pts',(-23.8270075938031,-1.91921083109556,
20.238157056608)) ;
#61073 = CARTESIAN_POINT('Ctrl Pts',(-23.8264819338432,-1.91607593159048,
20.2377751864947)) ;
#61074 = CARTESIAN_POINT('Ctrl Pts',(-23.8263072072762,-1.91503706074593,
20.2376492614186)) ;
#61075 = CARTESIAN_POINT('Ctrl Pts',(-23.8259588939672,-1.91297454696765,
20.2374009304249)) ;
#61076 = CARTESIAN_POINT('Ctrl Pts',(-23.8257853088977,-1.91195090399017,
20.2372785225245)) ;
#61077 = CARTESIAN_POINT('Ctrl Pts',(-23.8254391507072,-1.90992188988011,
20.2370383481173)) ;
#61078 = CARTESIAN_POINT('Ctrl Pts',(-23.8252666033692,-1.908916520574,20.2369205518394)) ;
#61079 = CARTESIAN_POINT('Ctrl Pts',(-23.8250078847294,-1.9074244674468,20.2367488447037)) ;
#61080 = CARTESIAN_POINT('Ctrl Pts',(-23.8249216558837,-1.90692978371519,
20.2366924478544)) ;
#61081 = CARTESIAN_POINT('Ctrl Pts',(-23.8247488849763,-1.90594614016797,
20.2365818500951)) ;
#61082 = CARTESIAN_POINT('Ctrl Pts',(-23.8246623585185,-1.90545717970068,
20.2365276306065)) ;
#61083 = CARTESIAN_POINT('Ctrl Pts',(-23.8245305246237,-1.90472138440371,
20.2364479563656)) ;
#61084 = CARTESIAN_POINT('Ctrl Pts',(-23.8244832305277,-1.90445904599412,
20.2364198914254)) ;
#61085 = CARTESIAN_POINT('Ctrl Pts',(-23.8243854245268,-1.90392207855429,
20.2363636264214)) ;
#61086 = CARTESIAN_POINT('Ctrl Pts',(-23.8243349158579,-1.90364744934,20.2363354224894)) ;
#61087 = CARTESIAN_POINT('Ctrl Pts',(-23.8242321896462,-1.9030985039168,20.236281126385)) ;
#61088 = CARTESIAN_POINT('Ctrl Pts',(-23.8241800404489,-1.90282422655538,
20.2362549661509)) ;
#61089 = CARTESIAN_POINT('Ctrl Pts',(-23.8239076987598,-1.90163369678401,
20.2361955498099)) ;
#61090 = CARTESIAN_POINT('Ctrl Pts',(-23.8238965621088,-1.90158501340151,
20.236193120145)) ;
#61091 = CARTESIAN_POINT('Ctrl Pts',(-23.8238854254577,-1.90153633001901,
20.23619069048)) ;
#61092 = CARTESIAN_POINT('',(-32.7305102571637,-15.0366437072153,9.10296276716422)) ;
#61093 = CARTESIAN_POINT('',(-32.738440159828,-15.0366437072153,9.0744018390217)) ;
#61094 = CARTESIAN_POINT('Origin',(1.31615393895547,-21.6462763158694,-0.365428342349787)) ;
#61095 = CARTESIAN_POINT('',(-30.1189287239454,-1.90153624313405,8.36247940662196)) ;
#61096 = CARTESIAN_POINT('Ctrl Pts',(-30.1189287421105,-1.90153633469768,
8.3624794119278)) ;
#61097 = CARTESIAN_POINT('Ctrl Pts',(-30.1189366899314,-1.90158489287906,
8.36248829647417)) ;
#61098 = CARTESIAN_POINT('Ctrl Pts',(-30.1190728896525,-1.90241702169426,
8.36264054861436)) ;
#61099 = CARTESIAN_POINT('Ctrl Pts',(-30.1191458040911,-1.90281621613969,
8.36268630250738)) ;
#61100 = CARTESIAN_POINT('Ctrl Pts',(-30.1191963902888,-1.9030887682969,8.36271464737924)) ;
#61101 = CARTESIAN_POINT('Ctrl Pts',(-30.1192983133845,-1.90363426309853,
8.36276893498663)) ;
#61102 = CARTESIAN_POINT('Ctrl Pts',(-30.1193496681974,-1.90390716693057,
8.362794783217)) ;
#61103 = CARTESIAN_POINT('Ctrl Pts',(-30.1194504713046,-1.90444076192566,
8.36284391234841)) ;
#61104 = CARTESIAN_POINT('Ctrl Pts',(-30.1194999210193,-1.90470145327792,
8.36286718827989)) ;
#61105 = CARTESIAN_POINT('Ctrl Pts',(-30.1196389419315,-1.90543258195801,
8.36293125926836)) ;
#61106 = CARTESIAN_POINT('Ctrl Pts',(-30.1197317682973,-1.90591842510436,
8.3629722308881)) ;
#61107 = CARTESIAN_POINT('Ctrl Pts',(-30.1199190407705,-1.9068957977074,8.36305273288145)) ;
#61108 = CARTESIAN_POINT('Ctrl Pts',(-30.1200134934398,-1.90738732781205,
8.36309224012143)) ;
#61109 = CARTESIAN_POINT('Ctrl Pts',(-30.1202989406533,-1.90886986923223,
8.36320937923951)) ;
#61110 = CARTESIAN_POINT('Ctrl Pts',(-30.1204920133598,-1.90986882963001,
8.36328566672494)) ;
#61111 = CARTESIAN_POINT('Ctrl Pts',(-30.120882522362,-1.91188490974371,8.36343655309822)) ;
#61112 = CARTESIAN_POINT('Ctrl Pts',(-30.1210799687811,-1.91290202763325,
8.36351111411351)) ;
#61113 = CARTESIAN_POINT('Ctrl Pts',(-30.121478391718,-1.914951394423,8.36365921021491)) ;
#61114 = CARTESIAN_POINT('Ctrl Pts',(-30.1216793689211,-1.91598364336599,
8.36373274286551)) ;
#61115 = CARTESIAN_POINT('Ctrl Pts',(-30.1222864955005,-1.91909856098391,
8.36395226839086)) ;
#61116 = CARTESIAN_POINT('Ctrl Pts',(-30.1226968244005,-1.92119938519643,
8.36409723269177)) ;
#61117 = CARTESIAN_POINT('Ctrl Pts',(-30.1235232857103,-1.92542529583428,
8.36438500090773)) ;
#61118 = CARTESIAN_POINT('Ctrl Pts',(-30.1239394277851,-1.92755038271577,
8.36452777036499)) ;
#61119 = CARTESIAN_POINT('Ctrl Pts',(-30.1251889974469,-1.9339258146116,8.36495209273466)) ;
#61120 = CARTESIAN_POINT('Ctrl Pts',(-30.1260235402243,-1.93817627781002,
8.36522972038847)) ;
#61121 = CARTESIAN_POINT('Ctrl Pts',(-30.127656279388,-1.94648421945793,8.36576680755742)) ;
#61122 = CARTESIAN_POINT('Ctrl Pts',(-30.1284544954223,-1.95054169858679,
8.36602619683147)) ;
#61123 = CARTESIAN_POINT('Ctrl Pts',(-30.1299748675873,-1.95826546921425,
8.36651673549711)) ;
#61124 = CARTESIAN_POINT('Ctrl Pts',(-30.1307374247382,-1.96213697914807,
8.36676089979701)) ;
#61125 = CARTESIAN_POINT('Ctrl Pts',(-30.1322678626644,-1.96990337734099,
8.36724811362133)) ;
#61126 = CARTESIAN_POINT('Ctrl Pts',(-30.1330357439221,-1.97379826561344,
8.36749116141787)) ;
#61127 = CARTESIAN_POINT('Ctrl Pts',(-30.1353469300952,-1.98551686319814,
8.36821935177273)) ;
#61128 = CARTESIAN_POINT('Ctrl Pts',(-30.1368977646678,-1.99337450486331,
8.36870358687115)) ;
#61129 = CARTESIAN_POINT('Ctrl Pts',(-30.1400176319817,-2.00917423416183,
8.3696717456377)) ;
#61130 = CARTESIAN_POINT('Ctrl Pts',(-30.1415866723529,-2.01711632162066,
8.37015564168992)) ;
#61131 = CARTESIAN_POINT('Ctrl Pts',(-30.1447413894306,-2.03307890748333,
8.37112408567312)) ;
#61132 = CARTESIAN_POINT('Ctrl Pts',(-30.1463270663545,-2.04109940589163,
8.37160863282255)) ;
#61133 = CARTESIAN_POINT('Ctrl Pts',(-30.1511069097881,-2.06526946998702,
8.37306397729435)) ;
#61134 = CARTESIAN_POINT('Ctrl Pts',(-30.1543238610328,-2.08152760108453,
8.37403657554525)) ;
#61135 = CARTESIAN_POINT('Ctrl Pts',(-30.1608078860201,-2.11428512297351,
8.37598761435187)) ;
#61136 = CARTESIAN_POINT('Ctrl Pts',(-30.1640749726964,-2.13078451396997,
8.37696600848241)) ;
#61137 = CARTESIAN_POINT('Ctrl Pts',(-30.1706491258843,-2.16397631340779,
8.37892790365587)) ;
#61138 = CARTESIAN_POINT('Ctrl Pts',(-30.1739561963703,-2.18066871801029,
8.37991138741871)) ;
#61139 = CARTESIAN_POINT('Ctrl Pts',(-30.1806003831165,-2.21419829031838,
8.38188196581156)) ;
#61140 = CARTESIAN_POINT('Ctrl Pts',(-30.1839374999802,-2.23103545803188,
8.38286905827254)) ;
#61141 = CARTESIAN_POINT('Ctrl Pts',(-30.1939791862586,-2.28169173815909,
8.38583291307417)) ;
#61142 = CARTESIAN_POINT('Ctrl Pts',(-30.2007140718881,-2.31565562726959,
8.38781232274202)) ;
#61143 = CARTESIAN_POINT('Ctrl Pts',(-30.2141868277967,-2.38358352393428,
8.39176048383652)) ;
#61144 = CARTESIAN_POINT('Ctrl Pts',(-30.2209247071832,-2.41754751782455,
8.39372919190598)) ;
#61145 = CARTESIAN_POINT('Ctrl Pts',(-30.234326067002,-2.48508962361059,8.3976364844371)) ;
#61146 = CARTESIAN_POINT('Ctrl Pts',(-30.2409895522187,-2.51866773555189,
8.39957505170218)) ;
#61147 = CARTESIAN_POINT('Ctrl Pts',(-30.2607526662601,-2.61824429213986,
8.40531520776665)) ;
#61148 = CARTESIAN_POINT('Ctrl Pts',(-30.2736249224652,-2.68308495719539,
8.40904136225151)) ;
#61149 = CARTESIAN_POINT('Ctrl Pts',(-30.2993135315686,-2.81246585171732,
8.41646293757522)) ;
#61150 = CARTESIAN_POINT('Ctrl Pts',(-30.312785289604,-2.88030501170083,8.42034614576319)) ;
#61151 = CARTESIAN_POINT('Ctrl Pts',(-30.339813448705,-3.01639280924263,8.42812401692986)) ;
#61152 = CARTESIAN_POINT('Ctrl Pts',(-30.3533698602386,-3.0846414468735,8.43201864226201)) ;
#61153 = CARTESIAN_POINT('Ctrl Pts',(-30.3805639776459,-3.22153498784917,
8.43982120276864)) ;
#61154 = CARTESIAN_POINT('Ctrl Pts',(-30.394201687757,-3.29017989118037,8.44372912266984)) ;
#61155 = CARTESIAN_POINT('Ctrl Pts',(-30.4215552917968,-3.42785275302243,
8.45155927059217)) ;
#61156 = CARTESIAN_POINT('Ctrl Pts',(-30.4352711862702,-3.49688071153673,
8.45548149664984)) ;
#61157 = CARTESIAN_POINT('Ctrl Pts',(-30.4765316882847,-3.70451935539514,
8.46727038395918)) ;
#61158 = CARTESIAN_POINT('Ctrl Pts',(-30.5041890851405,-3.84368480840043,
8.47515935928979)) ;
#61159 = CARTESIAN_POINT('Ctrl Pts',(-30.5597818551889,-4.12338942184984,
8.4909972851407)) ;
#61160 = CARTESIAN_POINT('Ctrl Pts',(-30.58771724435,-4.26392858237327,8.49894617820889)) ;
#61161 = CARTESIAN_POINT('Ctrl Pts',(-30.6438439166593,-4.54627494106967,
8.5149018456369)) ;
#61162 = CARTESIAN_POINT('Ctrl Pts',(-30.6720352067423,-4.68808213833386,
8.52290859431798)) ;
#61163 = CARTESIAN_POINT('Ctrl Pts',(-30.7286519494228,-4.97285889875352,
8.53897661380741)) ;
#61164 = CARTESIAN_POINT('Ctrl Pts',(-30.7570774055805,-5.11582846192401,
8.54703787180537)) ;
#61165 = CARTESIAN_POINT('Ctrl Pts',(-30.8141409569631,-5.40282428515253,
8.56321080365312)) ;
#61166 = CARTESIAN_POINT('Ctrl Pts',(-30.8427790539311,-5.54685054520825,
8.57132247122268)) ;
#61167 = CARTESIAN_POINT('Ctrl Pts',(-30.9002464954105,-5.83585409368823,
8.58759164117081)) ;
#61168 = CARTESIAN_POINT('Ctrl Pts',(-30.9290758402359,-5.98083138211383,
8.59574914241628)) ;
#61169 = CARTESIAN_POINT('Ctrl Pts',(-31.0158187876865,-6.41703128767462,
8.62028306277105)) ;
#61170 = CARTESIAN_POINT('Ctrl Pts',(-31.0739872819299,-6.70952194040057,
8.63672097178661)) ;
#61171 = CARTESIAN_POINT('Ctrl Pts',(-31.1908342051894,-7.29703932551894,
8.66971923040377)) ;
#61172 = CARTESIAN_POINT('Ctrl Pts',(-31.2495126445056,-7.59206605794504,
8.68627954293313)) ;
#61173 = CARTESIAN_POINT('Ctrl Pts',(-31.3672102153851,-8.18381025254895,
8.7194791528873)) ;
#61174 = CARTESIAN_POINT('Ctrl Pts',(-31.4262293520484,-8.48052771472347,
8.73611843194019)) ;
#61175 = CARTESIAN_POINT('Ctrl Pts',(-31.5444393691136,-9.07480801972223,
8.7694314609245)) ;
#61176 = CARTESIAN_POINT('Ctrl Pts',(-31.6036302519042,-9.37237086255337,
8.78610520225537)) ;
#61177 = CARTESIAN_POINT('Ctrl Pts',(-31.7812073724757,-10.26505943922,8.83611035606427)) ;
#61178 = CARTESIAN_POINT('Ctrl Pts',(-31.89959803729,-10.8601852058064,8.86942584909673)) ;
#61179 = CARTESIAN_POINT('Ctrl Pts',(-32.13504239898,-12.0436740242095,8.93564812637502)) ;
#61180 = CARTESIAN_POINT('Ctrl Pts',(-32.2520961165265,-12.6320370760777,
8.96855483620709)) ;
#61181 = CARTESIAN_POINT('Ctrl Pts',(-32.4835188253346,-13.7952376552548,
9.03358962841841)) ;
#61182 = CARTESIAN_POINT('Ctrl Pts',(-32.6047730141693,-14.40468127544,9.06765183250815)) ;
#61183 = CARTESIAN_POINT('Ctrl Pts',(-32.7237611936004,-15.002722575796,9.1010674510721)) ;
#61184 = CARTESIAN_POINT('Ctrl Pts',(-32.7305102570438,-15.0366437072151,
9.1029627675952)) ;
#61185 = CARTESIAN_POINT('Ctrl Pts',(-32.738440159947,-15.0366437072151,9.07440183859236)) ;
#61186 = CARTESIAN_POINT('Ctrl Pts',(-32.7316800387762,-15.0027225758828,
9.07254634847045)) ;
#61187 = CARTESIAN_POINT('Ctrl Pts',(-32.7249124353925,-14.9687639420613,
9.07068883708644)) ;
#61188 = CARTESIAN_POINT('Ctrl Pts',(-32.6055998276366,-14.3700751829105,
9.03794155762668)) ;
#61189 = CARTESIAN_POINT('Ctrl Pts',(-32.4910381898364,-13.7952376556947,
9.0065073254432)) ;
#61190 = CARTESIAN_POINT('Ctrl Pts',(-32.2592130431272,-12.6320370767004,
8.94292198369549)) ;
#61191 = CARTESIAN_POINT('Ctrl Pts',(-32.141949544088,-12.0436740249246,8.91077083858567)) ;
#61192 = CARTESIAN_POINT('Ctrl Pts',(-31.9060662027409,-10.8601852067075,
8.84612962328421)) ;
#61193 = CARTESIAN_POINT('Ctrl Pts',(-31.7874463810849,-10.2650594402146,
8.81363947867534)) ;
#61194 = CARTESIAN_POINT('Ctrl Pts',(-31.6095078011031,-9.3723708636882,8.76493618411246)) ;
#61195 = CARTESIAN_POINT('Ctrl Pts',(-31.5501934567731,-9.0748080209038,8.74870711109432)) ;
#61196 = CARTESIAN_POINT('Ctrl Pts',(-31.4317296947875,-8.48052771599843,
8.71630798878961)) ;
#61197 = CARTESIAN_POINT('Ctrl Pts',(-31.3725802795186,-8.18381025387053,
8.70013793090298)) ;
#61198 = CARTESIAN_POINT('Ctrl Pts',(-31.254614084343,-7.59206605935958,8.66790581829583)) ;
#61199 = CARTESIAN_POINT('Ctrl Pts',(-31.1957973095379,-7.29703932697985,
8.65184374520358)) ;
#61200 = CARTESIAN_POINT('Ctrl Pts',(-31.0786638053382,-6.70952194195379,
8.61987765791991)) ;
#61201 = CARTESIAN_POINT('Ctrl Pts',(-31.0203470862311,-6.4170312892738,8.60397360665013)) ;
#61202 = CARTESIAN_POINT('Ctrl Pts',(-30.9333722119693,-5.98083138378153,
8.58027501122829)) ;
#61203 = CARTESIAN_POINT('Ctrl Pts',(-30.9044639497444,-5.83585409537872,
8.5724017447851)) ;
#61204 = CARTESIAN_POINT('Ctrl Pts',(-30.846834926806,-5.54685054694414,8.55671453869105)) ;
#61205 = CARTESIAN_POINT('Ctrl Pts',(-30.8181141664073,-5.40282428691104,
8.54890059790883)) ;
#61206 = CARTESIAN_POINT('Ctrl Pts',(-30.7608808355205,-5.11582846372763,
8.53333915660507)) ;
#61207 = CARTESIAN_POINT('Ctrl Pts',(-30.7323682667758,-4.97285890057961,
8.52559164980705)) ;
#61208 = CARTESIAN_POINT('Ctrl Pts',(-30.6755718751027,-4.68808214020468,
8.51017066754581)) ;
#61209 = CARTESIAN_POINT('Ctrl Pts',(-30.647288055729,-4.54627494296275,8.50249717926813)) ;
#61210 = CARTESIAN_POINT('Ctrl Pts',(-30.590969507909,-4.26392858431071,8.48723258500705)) ;
#61211 = CARTESIAN_POINT('Ctrl Pts',(-30.5629347867595,-4.12338942380938,
8.47964145344446)) ;
#61212 = CARTESIAN_POINT('Ctrl Pts',(-30.5071344190471,-3.84368481040393,
8.46455122683816)) ;
#61213 = CARTESIAN_POINT('Ctrl Pts',(-30.4793687884229,-3.70451935742048,
8.45705207432742)) ;
#61214 = CARTESIAN_POINT('Ctrl Pts',(-30.4379366248619,-3.49688071359469,
8.44588145605661)) ;
#61215 = CARTESIAN_POINT('Ctrl Pts',(-30.4241619434822,-3.42785275509126,
8.44217096130755)) ;
#61216 = CARTESIAN_POINT('Ctrl Pts',(-30.3966869486075,-3.29017989327082,
8.4347780236757)) ;
#61217 = CARTESIAN_POINT('Ctrl Pts',(-30.3829866356556,-3.2215349899504,8.4310955788379)) ;
#61218 = CARTESIAN_POINT('Ctrl Pts',(-30.3556625208449,-3.08464144899626,
8.42376122667959)) ;
#61219 = CARTESIAN_POINT('Ctrl Pts',(-30.3420387232273,-3.01639281137611,
8.42010930409529)) ;
#61220 = CARTESIAN_POINT('Ctrl Pts',(-30.3148695396667,-2.88030501385569,
8.41283935714398)) ;
#61221 = CARTESIAN_POINT('Ctrl Pts',(-30.301324164162,-2.81246585388284,8.40922129512537)) ;
#61222 = CARTESIAN_POINT('Ctrl Pts',(-30.2754864732429,-2.68308495896682,
8.4023366636702)) ;
#61223 = CARTESIAN_POINT('Ctrl Pts',(-30.2625357547394,-2.61824429348635,
8.39889310451541)) ;
#61224 = CARTESIAN_POINT('Ctrl Pts',(-30.2426422289194,-2.51866773624582,
8.39362264872344)) ;
#61225 = CARTESIAN_POINT('Ctrl Pts',(-30.2359331379167,-2.48508962408448,
8.39184833848451)) ;
#61226 = CARTESIAN_POINT('Ctrl Pts',(-30.2224356667615,-2.4175475178558,8.38828720735983)) ;
#61227 = CARTESIAN_POINT('Ctrl Pts',(-30.2156472913765,-2.38358352374292,
8.38650036926848)) ;
#61228 = CARTESIAN_POINT('Ctrl Pts',(-30.2020675740235,-2.31565562663307,
8.38293744813557)) ;
#61229 = CARTESIAN_POINT('Ctrl Pts',(-30.1952762466078,-2.28169173729999,
8.38116132323752)) ;
#61230 = CARTESIAN_POINT('Ctrl Pts',(-30.1851439288179,-2.23103545684079,
8.37852389338254)) ;
#61231 = CARTESIAN_POINT('Ctrl Pts',(-30.1817755969363,-2.21419828901697,
8.37764922716979)) ;
#61232 = CARTESIAN_POINT('Ctrl Pts',(-30.1750665385079,-2.18066871648915,
8.37591229529037)) ;
#61233 = CARTESIAN_POINT('Ctrl Pts',(-30.171725812564,-2.16397631177722,8.37505002744728)) ;
#61234 = CARTESIAN_POINT('Ctrl Pts',(-30.16508123956,-2.13078451212187,8.37334176136098)) ;
#61235 = CARTESIAN_POINT('Ctrl Pts',(-30.1617773979994,-2.11428512101739,
8.3724957462761)) ;
#61236 = CARTESIAN_POINT('Ctrl Pts',(-30.1552156490333,-2.08152759891375,
8.37082464377552)) ;
#61237 = CARTESIAN_POINT('Ctrl Pts',(-30.1519577544726,-2.06526946770973,
8.36999950993898)) ;
#61238 = CARTESIAN_POINT('Ctrl Pts',(-30.1471118028374,-2.04109940345594,
8.36878226556815)) ;
#61239 = CARTESIAN_POINT('Ctrl Pts',(-30.1455032940284,-2.03307890499497,
8.36837995139651)) ;
#61240 = CARTESIAN_POINT('Ctrl Pts',(-30.1423008670093,-2.01711631902769,
8.36758334301117)) ;
#61241 = CARTESIAN_POINT('Ctrl Pts',(-30.1407069490228,-2.00917423151679,
8.36718904799129)) ;
#61242 = CARTESIAN_POINT('Ctrl Pts',(-30.1375345303182,-1.99337450211475,
8.36641016214816)) ;
#61243 = CARTESIAN_POINT('Ctrl Pts',(-30.1359560372963,-1.98551686039824,
8.3660255437412)) ;
#61244 = CARTESIAN_POINT('Ctrl Pts',(-30.1336002594764,-1.97379826273675,
8.36545795792382)) ;
#61245 = CARTESIAN_POINT('Ctrl Pts',(-30.1328169906812,-1.96990337443867,
8.36527033100878)) ;
#61246 = CARTESIAN_POINT('Ctrl Pts',(-30.1312544389846,-1.96213697619486,
8.36489878049294)) ;
#61247 = CARTESIAN_POINT('Ctrl Pts',(-30.1304751565699,-1.95826546623556,
8.36471485512932)) ;
#61248 = CARTESIAN_POINT('Ctrl Pts',(-30.1289195156902,-1.95054169571453,
8.36435134297619)) ;
#61249 = CARTESIAN_POINT('Ctrl Pts',(-30.1281018294351,-1.94648421672414,
8.36416207920644)) ;
#61250 = CARTESIAN_POINT('Ctrl Pts',(-30.1264259078607,-1.93817627535945,
8.36378052124339)) ;
#61251 = CARTESIAN_POINT('Ctrl Pts',(-30.1255676919097,-1.9339258123061,8.36358815676693)) ;
#61252 = CARTESIAN_POINT('Ctrl Pts',(-30.1242782281864,-1.9275503806276,8.363307519989)) ;
#61253 = CARTESIAN_POINT('Ctrl Pts',(-30.1238480485303,-1.9254252938187,8.36321530938629)) ;
#61254 = CARTESIAN_POINT('Ctrl Pts',(-30.122991529241,-1.92119938332494,8.36303580033953)) ;
#61255 = CARTESIAN_POINT('Ctrl Pts',(-30.1225651990868,-1.91909855918412,
8.36294846740335)) ;
#61256 = CARTESIAN_POINT('Ctrl Pts',(-30.1219318011106,-1.91598364167241,
8.36282356297935)) ;
#61257 = CARTESIAN_POINT('Ctrl Pts',(-30.1217216823121,-1.91495139276497,
8.36278295540766)) ;
#61258 = CARTESIAN_POINT('Ctrl Pts',(-30.121303939256,-1.91290202604524,8.36270444414061)) ;
#61259 = CARTESIAN_POINT('Ctrl Pts',(-30.1210963156627,-1.91188490819044,
8.36266653802089)) ;
#61260 = CARTESIAN_POINT('Ctrl Pts',(-30.1206839151831,-1.90986882814559,
8.36259449767639)) ;
#61261 = CARTESIAN_POINT('Ctrl Pts',(-30.1204791491518,-1.90886986778167,
8.3625603257668)) ;
#61262 = CARTESIAN_POINT('Ctrl Pts',(-30.1201741701421,-1.90738732641242,
8.36251353386047)) ;
#61263 = CARTESIAN_POINT('Ctrl Pts',(-30.1200728696049,-1.90689579632289,
8.36249869042318)) ;
#61264 = CARTESIAN_POINT('Ctrl Pts',(-30.1198709007348,-1.90591842375347,
8.36247112009354)) ;
#61265 = CARTESIAN_POINT('Ctrl Pts',(-30.119770238727,-1.90543258062349,8.36245836991853)) ;
#61266 = CARTESIAN_POINT('Ctrl Pts',(-30.1196180856502,-1.9047014521107,8.3624415968411)) ;
#61267 = CARTESIAN_POINT('Ctrl Pts',(-30.1195637143114,-1.90444076092128,
8.36243604712368)) ;
#61268 = CARTESIAN_POINT('Ctrl Pts',(-30.1194520118001,-1.90390716624985,
8.36242617434808)) ;
#61269 = CARTESIAN_POINT('Ctrl Pts',(-30.1193946819637,-1.90363426257986,
8.3624218463327)) ;
#61270 = CARTESIAN_POINT('Ctrl Pts',(-30.119279360318,-1.90308876810775,8.36241581619551)) ;
#61271 = CARTESIAN_POINT('Ctrl Pts',(-30.1192214019085,-1.90281621611284,
8.36241402375624)) ;
#61272 = CARTESIAN_POINT('Ctrl Pts',(-30.1189510053552,-1.90163369796138,
8.36247443771244)) ;
#61273 = CARTESIAN_POINT('Ctrl Pts',(-30.1189398737328,-1.90158501632953,
8.36247692482012)) ;
#61274 = CARTESIAN_POINT('Ctrl Pts',(-30.1189287421105,-1.90153633469768,
8.3624794119278)) ;
#61275 = CARTESIAN_POINT('',(-33.5276414405313,-15.0366437072153,-5.48155929182975)) ;
#61276 = CARTESIAN_POINT('',(-33.5228460028119,-15.0366437072153,-5.51081016788253)) ;
#61277 = CARTESIAN_POINT('Origin',(1.34794834185301,-21.6462763158694,0.220984913775247)) ;
#61278 = CARTESIAN_POINT('',(-30.8465133415523,-1.9015362431713,-5.057029164855)) ;
#61279 = CARTESIAN_POINT('Ctrl Pts',(-30.8465133602742,-1.90153633477217,
-5.05702916766694)) ;
#61280 = CARTESIAN_POINT('Ctrl Pts',(-30.846524305277,-1.90158489180048,-5.05702443248837)) ;
#61281 = CARTESIAN_POINT('Ctrl Pts',(-30.8467113041087,-1.9024145039777,-5.05694353046583)) ;
#61282 = CARTESIAN_POINT('Ctrl Pts',(-30.8467964485072,-1.90281253800259,
-5.05693261829815)) ;
#61283 = CARTESIAN_POINT('Ctrl Pts',(-30.8468540962568,-1.90308429852864,
-5.05692812744458)) ;
#61284 = CARTESIAN_POINT('Ctrl Pts',(-30.8469690650942,-1.90362820994333,
-5.05692163693397)) ;
#61285 = CARTESIAN_POINT('Ctrl Pts',(-30.8470263627717,-1.90390032204335,
-5.05691973052414)) ;
#61286 = CARTESIAN_POINT('Ctrl Pts',(-30.8471381575833,-1.90443236952265,
-5.05691744581171)) ;
#61287 = CARTESIAN_POINT('Ctrl Pts',(-30.8471926539434,-1.90469230508585,
-5.05691707246499)) ;
#61288 = CARTESIAN_POINT('Ctrl Pts',(-30.8473452861646,-1.90542129310748,
-5.05691726094962)) ;
#61289 = CARTESIAN_POINT('Ctrl Pts',(-30.8474464415333,-1.90590570652529,
-5.05691902657438)) ;
#61290 = CARTESIAN_POINT('Ctrl Pts',(-30.8476496141687,-1.90688020302458,
-5.05692454286342)) ;
#61291 = CARTESIAN_POINT('Ctrl Pts',(-30.847751627679,-1.90737028675471,-5.0569283172706)) ;
#61292 = CARTESIAN_POINT('Ctrl Pts',(-30.8480589795514,-1.90884846572905,
-5.05694176855341)) ;
#61293 = CARTESIAN_POINT('Ctrl Pts',(-30.8482656351864,-1.90984448674729,
-5.05695353474426)) ;
#61294 = CARTESIAN_POINT('Ctrl Pts',(-30.8486821875314,-1.9118546348179,-5.05698042595716)) ;
#61295 = CARTESIAN_POINT('Ctrl Pts',(-30.8488920775291,-1.91286876004502,
-5.0569955895894)) ;
#61296 = CARTESIAN_POINT('Ctrl Pts',(-30.8493146220058,-1.91491209710514,
-5.0570283257827)) ;
#61297 = CARTESIAN_POINT('Ctrl Pts',(-30.8495272760765,-1.91594130898178,
-5.05704590088905)) ;
#61298 = CARTESIAN_POINT('Ctrl Pts',(-30.8501685848949,-1.91904706211498,
-5.05710135597619)) ;
#61299 = CARTESIAN_POINT('Ctrl Pts',(-30.8506005906325,-1.9211417056253,-5.05714191950652)) ;
#61300 = CARTESIAN_POINT('Ctrl Pts',(-30.8514689484867,-1.9253551838102,-5.05722743644029)) ;
#61301 = CARTESIAN_POINT('Ctrl Pts',(-30.85190529492,-1.92747401894057,-5.05727242509241)) ;
#61302 = CARTESIAN_POINT('Ctrl Pts',(-30.8532136992813,-1.93383069557251,
-5.05741148274527)) ;
#61303 = CARTESIAN_POINT('Ctrl Pts',(-30.8540851221337,-1.93806865525155,
-5.05750957649476)) ;
#61304 = CARTESIAN_POINT('Ctrl Pts',(-30.8557874699047,-1.94635215818821,
-5.05770699916352)) ;
#61305 = CARTESIAN_POINT('Ctrl Pts',(-30.8566183831832,-1.95039770212494,
-5.05780639995181)) ;
#61306 = CARTESIAN_POINT('Ctrl Pts',(-30.8581995372407,-1.95809865038701,
-5.05799892058496)) ;
#61307 = CARTESIAN_POINT('Ctrl Pts',(-30.8589917862104,-1.96195866901122,
-5.0580971745769)) ;
#61308 = CARTESIAN_POINT('Ctrl Pts',(-30.8605806341267,-1.96970201522502,
-5.05829692357479)) ;
#61309 = CARTESIAN_POINT('Ctrl Pts',(-30.8613772327858,-1.97358534282792,
-5.05839842034979)) ;
#61310 = CARTESIAN_POINT('Ctrl Pts',(-30.8637734540801,-1.98526915772027,
-5.0587069348275)) ;
#61311 = CARTESIAN_POINT('Ctrl Pts',(-30.8653795095856,-1.99310347667916,
-5.05891793007803)) ;
#61312 = CARTESIAN_POINT('Ctrl Pts',(-30.8686079562012,-2.00885630997501,
-5.05934782834555)) ;
#61313 = CARTESIAN_POINT('Ctrl Pts',(-30.8702303426481,-2.01677482413742,
-5.05956675958315)) ;
#61314 = CARTESIAN_POINT('Ctrl Pts',(-30.8734904414554,-2.03269003071707,
-5.06001100244198)) ;
#61315 = CARTESIAN_POINT('Ctrl Pts',(-30.8751281536876,-2.04068672313867,
-5.06023631484786)) ;
#61316 = CARTESIAN_POINT('Ctrl Pts',(-30.8800626450534,-2.06478504708697,
-5.06092026785506)) ;
#61317 = CARTESIAN_POINT('Ctrl Pts',(-30.8833807945906,-2.08099492183752,
-5.06138682384106)) ;
#61318 = CARTESIAN_POINT('Ctrl Pts',(-30.8900648925976,-2.11365521506201,
-5.06233564397943)) ;
#61319 = CARTESIAN_POINT('Ctrl Pts',(-30.8934308333245,-2.1301056337409,-5.0628179556211)) ;
#61320 = CARTESIAN_POINT('Ctrl Pts',(-30.9002010284063,-2.16319891576677,
-5.06379470349268)) ;
#61321 = CARTESIAN_POINT('Ctrl Pts',(-30.9036052791168,-2.17984177527506,
-5.0642891570483)) ;
#61322 = CARTESIAN_POINT('Ctrl Pts',(-30.9104424789968,-2.21327182781219,
-5.0652873818654)) ;
#61323 = CARTESIAN_POINT('Ctrl Pts',(-30.9138754278022,-2.23005902084895,
-5.06579115535564)) ;
#61324 = CARTESIAN_POINT('Ctrl Pts',(-30.924202802114,-2.28056494736301,-5.06731285165701)) ;
#61325 = CARTESIAN_POINT('Ctrl Pts',(-30.9311257671805,-2.31442802795414,
-5.06834107877602)) ;
#61326 = CARTESIAN_POINT('Ctrl Pts',(-30.94496993347,-2.38215430757668,-5.07040844327922)) ;
#61327 = CARTESIAN_POINT('Ctrl Pts',(-30.951891124766,-2.41601749294468,-5.07144762376045)) ;
#61328 = CARTESIAN_POINT('Ctrl Pts',(-30.9656535719189,-2.48335912723555,
-5.07352210987511)) ;
#61329 = CARTESIAN_POINT('Ctrl Pts',(-30.972494824902,-2.51683757620396,-5.07455743309499)) ;
#61330 = CARTESIAN_POINT('Ctrl Pts',(-30.9927812370883,-2.61611858052478,
-5.07763660537817)) ;
#61331 = CARTESIAN_POINT('Ctrl Pts',(-31.0059890681356,-2.68076679293773,
-5.07965354311224)) ;
#61332 = CARTESIAN_POINT('Ctrl Pts',(-31.0323372989951,-2.80974421399637,
-5.08369123789235)) ;
#61333 = CARTESIAN_POINT('Ctrl Pts',(-31.0461493683562,-2.87736250066609,
-5.08581643560629)) ;
#61334 = CARTESIAN_POINT('Ctrl Pts',(-31.0738548685374,-3.01300721842185,
-5.09009190871467)) ;
#61335 = CARTESIAN_POINT('Ctrl Pts',(-31.087748293069,-3.08103364958037,-5.09224222256004)) ;
#61336 = CARTESIAN_POINT('Ctrl Pts',(-31.1156142511499,-3.21748148745996,
-5.0965648454186)) ;
#61337 = CARTESIAN_POINT('Ctrl Pts',(-31.129586782141,-3.28590289416745,-5.09873717001806)) ;
#61338 = CARTESIAN_POINT('Ctrl Pts',(-31.1576085574405,-3.42312751561677,
-5.10310160741578)) ;
#61339 = CARTESIAN_POINT('Ctrl Pts',(-31.1716578014195,-3.49193073036205,
-5.10529372222149)) ;
#61340 = CARTESIAN_POINT('Ctrl Pts',(-31.2139168843255,-3.69889333670347,
-5.11189720543959)) ;
#61341 = CARTESIAN_POINT('Ctrl Pts',(-31.2422380916696,-3.83760568975149,
-5.11633560537967)) ;
#61342 = CARTESIAN_POINT('Ctrl Pts',(-31.2991570663195,-4.11639963076904,
-5.12527451457136)) ;
#61343 = CARTESIAN_POINT('Ctrl Pts',(-31.3277548240148,-4.25648121881785,
-5.12977508254569)) ;
#61344 = CARTESIAN_POINT('Ctrl Pts',(-31.3852060477396,-4.53790830408714,
-5.13883097478029)) ;
#61345 = CARTESIAN_POINT('Ctrl Pts',(-31.41405950929,-4.67925380039948,-5.14338632520198)) ;
#61346 = CARTESIAN_POINT('Ctrl Pts',(-31.4720010766913,-4.96310337447864,
-5.1525457224151)) ;
#61347 = CARTESIAN_POINT('Ctrl Pts',(-31.5010891803993,-5.10560745226049,
-5.15714978229708)) ;
#61348 = CARTESIAN_POINT('Ctrl Pts',(-31.55947884342,-5.39166886431443,-5.16640130243607)) ;
#61349 = CARTESIAN_POINT('Ctrl Pts',(-31.5887804016795,-5.53522619858423,
-5.17104876911307)) ;
#61350 = CARTESIAN_POINT('Ctrl Pts',(-31.6475757056389,-5.82328879913435,
-5.18038229220635)) ;
#61351 = CARTESIAN_POINT('Ctrl Pts',(-31.6770694511483,-5.96779406541603,
-5.1850683497823)) ;
#61352 = CARTESIAN_POINT('Ctrl Pts',(-31.7658069889186,-6.40257377606671,
-5.19917766558687)) ;
#61353 = CARTESIAN_POINT('Ctrl Pts',(-31.825307093791,-6.69411212755049,-5.20865199154413)) ;
#61354 = CARTESIAN_POINT('Ctrl Pts',(-31.944819839875,-7.27971665323027,-5.2277033319237)) ;
#61355 = CARTESIAN_POINT('Ctrl Pts',(-32.0048324748802,-7.57378282745991,
-5.23728038424542)) ;
#61356 = CARTESIAN_POINT('Ctrl Pts',(-32.1251989946871,-8.16360040103258,
-5.25650565117136)) ;
#61357 = CARTESIAN_POINT('Ctrl Pts',(-32.1855528764093,-8.45935180037231,
-5.26615388455479)) ;
#61358 = CARTESIAN_POINT('Ctrl Pts',(-32.306430425885,-9.05169722737876,-5.28549106947084)) ;
#61359 = CARTESIAN_POINT('Ctrl Pts',(-32.3669540921975,-9.34829125505241,
-5.29518002979795)) ;
#61360 = CARTESIAN_POINT('Ctrl Pts',(-32.5485224061834,-10.2380733862356,
-5.32426334980075)) ;
#61361 = CARTESIAN_POINT('Ctrl Pts',(-32.6695643911593,-10.8312615224899,
-5.34367399302085)) ;
#61362 = CARTESIAN_POINT('Ctrl Pts',(-32.9102678483355,-12.0108970987381,
-5.38230551988749)) ;
#61363 = CARTESIAN_POINT('Ctrl Pts',(-33.0299293080724,-12.5973445387836,
-5.40152647961662)) ;
#61364 = CARTESIAN_POINT('Ctrl Pts',(-33.2664976872741,-13.756757931353,-5.43954920009931)) ;
#61365 = CARTESIAN_POINT('Ctrl Pts',(-33.3834046007805,-14.329723883874,-5.45835099719278)) ;
#61366 = CARTESIAN_POINT('Ctrl Pts',(-33.5080604096064,-14.9406748977399,
-5.4784084571226)) ;
#61367 = CARTESIAN_POINT('Ctrl Pts',(-33.5178586766213,-14.9886972685975,
-5.47998508973445)) ;
#61368 = CARTESIAN_POINT('Ctrl Pts',(-33.5276414406682,-15.0366437072149,
-5.48155929099228)) ;
#61369 = CARTESIAN_POINT('Ctrl Pts',(-33.5228460026744,-15.0366437072149,
-5.51081016871838)) ;
#61370 = CARTESIAN_POINT('Ctrl Pts',(-33.513072690402,-14.9886972684499,-5.5091783139983)) ;
#61371 = CARTESIAN_POINT('Ctrl Pts',(-33.5032839103576,-14.9406748974443,
-5.50754381323711)) ;
#61372 = CARTESIAN_POINT('Ctrl Pts',(-33.3787490601101,-14.3297238832788,
-5.48674853823682)) ;
#61373 = CARTESIAN_POINT('Ctrl Pts',(-33.2619584101797,-13.756757930604,-5.4672375645064)) ;
#61374 = CARTESIAN_POINT('Ctrl Pts',(-33.0256329225343,-12.5973445377235,
-5.42773327067727)) ;
#61375 = CARTESIAN_POINT('Ctrl Pts',(-32.9060980788614,-12.0108970975206,
-5.40773998692343)) ;
#61376 = CARTESIAN_POINT('Ctrl Pts',(-32.6656595786491,-10.8312615209558,
-5.36749229367)) ;
#61377 = CARTESIAN_POINT('Ctrl Pts',(-32.5447559096276,-10.2380733845424,
-5.34723796024904)) ;
#61378 = CARTESIAN_POINT('Ctrl Pts',(-32.3634057724657,-9.34829125312033,
-5.31682382019003)) ;
#61379 = CARTESIAN_POINT('Ctrl Pts',(-32.3029566282788,-9.05169722536708,
-5.30668029490438)) ;
#61380 = CARTESIAN_POINT('Ctrl Pts',(-32.1822322424287,-8.45935179820167,
-5.28640885299969)) ;
#61381 = CARTESIAN_POINT('Ctrl Pts',(-32.1219569993225,-8.16360039878257,
-5.27628094517738)) ;
#61382 = CARTESIAN_POINT('Ctrl Pts',(-32.0017526279443,-7.57378282505162,
-5.25606661638952)) ;
#61383 = CARTESIAN_POINT('Ctrl Pts',(-31.9418234965939,-7.27971665074306,
-5.24598021420588)) ;
#61384 = CARTESIAN_POINT('Ctrl Pts',(-31.8224837416044,-6.6941121249061,-5.22587367463099)) ;
#61385 = CARTESIAN_POINT('Ctrl Pts',(-31.7630731117453,-6.40257377334411,
-5.21585357513672)) ;
#61386 = CARTESIAN_POINT('Ctrl Pts',(-31.6744755765251,-5.96779406257672,
-5.20089028140719)) ;
#61387 = CARTESIAN_POINT('Ctrl Pts',(-31.645029469701,-5.82328879625627,-5.19591364065643)) ;
#61388 = CARTESIAN_POINT('Ctrl Pts',(-31.5863317052322,-5.53522619562883,
-5.18598515289222)) ;
#61389 = CARTESIAN_POINT('Ctrl Pts',(-31.5570800473982,-5.39166886132052,
-5.18103330703587)) ;
#61390 = CARTESIAN_POINT('Ctrl Pts',(-31.4987928735203,-5.10560744918979,
-5.17115663068443)) ;
#61391 = CARTESIAN_POINT('Ctrl Pts',(-31.469757356425,-4.9631033713697,-5.16623180660667)) ;
#61392 = CARTESIAN_POINT('Ctrl Pts',(-31.411924236773,-4.67925379721435,-5.15641090728921)) ;
#61393 = CARTESIAN_POINT('Ctrl Pts',(-31.3831266320664,-4.53790830086409,
-5.15151484514484)) ;
#61394 = CARTESIAN_POINT('Ctrl Pts',(-31.3257912374526,-4.25648121551928,
-5.14175242649281)) ;
#61395 = CARTESIAN_POINT('Ctrl Pts',(-31.2972534434363,-4.11639962743284,
-5.13688609621007)) ;
#61396 = CARTESIAN_POINT('Ctrl Pts',(-31.2404597892109,-3.8376056863405,-5.12718276615013)) ;
#61397 = CARTESIAN_POINT('Ctrl Pts',(-31.2122039193593,-3.69889333325525,
-5.12234582508958)) ;
#61398 = CARTESIAN_POINT('Ctrl Pts',(-31.1700484631251,-3.49193072685828,
-5.11511024706567)) ;
#61399 = CARTESIAN_POINT('Ctrl Pts',(-31.1560347069013,-3.42312751209455,
-5.11270166650645)) ;
#61400 = CARTESIAN_POINT('Ctrl Pts',(-31.1280862111298,-3.28590289060839,
-5.10789024371521)) ;
#61401 = CARTESIAN_POINT('Ctrl Pts',(-31.1141514712529,-3.21748148388252,
-5.10548740349358)) ;
#61402 = CARTESIAN_POINT('Ctrl Pts',(-31.0863639876091,-3.08103364596632,
-5.10068610769772)) ;
#61403 = CARTESIAN_POINT('Ctrl Pts',(-31.0725112412887,-3.01300721478954,
-5.09828766771808)) ;
#61404 = CARTESIAN_POINT('Ctrl Pts',(-31.0448908710698,-2.87736249699739,
-5.09349292476487)) ;
#61405 = CARTESIAN_POINT('Ctrl Pts',(-31.0311232408531,-2.80974421030951,
-5.09109666023862)) ;
#61406 = CARTESIAN_POINT('Ctrl Pts',(-31.0048650142947,-2.68076678970341,
-5.08650996408753)) ;
#61407 = CARTESIAN_POINT('Ctrl Pts',(-30.9917045601157,-2.61611857778466,
-5.08420404087192)) ;
#61408 = CARTESIAN_POINT('Ctrl Pts',(-30.9714968930084,-2.51683757422274,
-5.08064454582576)) ;
#61409 = CARTESIAN_POINT('Ctrl Pts',(-30.9646831776891,-2.48335912551026,
-5.07944125061466)) ;
#61410 = CARTESIAN_POINT('Ctrl Pts',(-30.9509787645156,-2.41601749173412,
-5.07701277354403)) ;
#61411 = CARTESIAN_POINT('Ctrl Pts',(-30.9440880637705,-2.38215430662499,
-5.07578760926055)) ;
#61412 = CARTESIAN_POINT('Ctrl Pts',(-30.9303084831399,-2.31442802752013,
-5.07332629032738)) ;
#61413 = CARTESIAN_POINT('Ctrl Pts',(-30.9234195988981,-2.2805649471878,-5.07209017970508)) ;
#61414 = CARTESIAN_POINT('Ctrl Pts',(-30.9131469500024,-2.23005902105978,
-5.07023467362553)) ;
#61415 = CARTESIAN_POINT('Ctrl Pts',(-30.9097328495601,-2.21327182815133,
-5.06961593037097)) ;
#61416 = CARTESIAN_POINT('Ctrl Pts',(-30.9029348207521,-2.17984177586973,
-5.06837877291122)) ;
#61417 = CARTESIAN_POINT('Ctrl Pts',(-30.8995508920192,-2.16319891648864,
-5.06776036093859)) ;
#61418 = CARTESIAN_POINT('Ctrl Pts',(-30.8928232181419,-2.13010563471574,
-5.06652424551718)) ;
#61419 = CARTESIAN_POINT('Ctrl Pts',(-30.8894794709209,-2.11365521616266,
-5.06590655963874)) ;
#61420 = CARTESIAN_POINT('Ctrl Pts',(-30.882842304577,-2.08099492318782,-5.06467146933891)) ;
#61421 = CARTESIAN_POINT('Ctrl Pts',(-30.8795488776322,-2.06478504856123,
-5.06405411236837)) ;
#61422 = CARTESIAN_POINT('Ctrl Pts',(-30.8746543040369,-2.04068672479713,
-5.06312667196831)) ;
#61423 = CARTESIAN_POINT('Ctrl Pts',(-30.8730303782615,-2.03269003243661,
-5.06281726597446)) ;
#61424 = CARTESIAN_POINT('Ctrl Pts',(-30.8697990878884,-2.01677482597858,
-5.06219729959632)) ;
#61425 = CARTESIAN_POINT('Ctrl Pts',(-30.8681917231571,-2.00885631187657,
-5.06188674002439)) ;
#61426 = CARTESIAN_POINT('Ctrl Pts',(-30.8649950083338,-1.99310347870114,
-5.06126328654053)) ;
#61427 = CARTESIAN_POINT('Ctrl Pts',(-30.8634056536514,-1.98526915980233,
-5.06095042085202)) ;
#61428 = CARTESIAN_POINT('Ctrl Pts',(-30.8610363578164,-1.9735853449993,-5.06047766845265)) ;
#61429 = CARTESIAN_POINT('Ctrl Pts',(-30.8602490504964,-1.96970201742585,
-5.06031949705393)) ;
#61430 = CARTESIAN_POINT('Ctrl Pts',(-30.8586795935814,-1.96195867127126,
-5.06000146825683)) ;
#61431 = CARTESIAN_POINT('Ctrl Pts',(-30.8578974436936,-1.95809865267673,
-5.05984161262806)) ;
#61432 = CARTESIAN_POINT('Ctrl Pts',(-30.8563375858908,-1.95039770434896,
-5.05951919050395)) ;
#61433 = CARTESIAN_POINT('Ctrl Pts',(-30.8555184294407,-1.94635216031222,
-5.05934807610711)) ;
#61434 = CARTESIAN_POINT('Ctrl Pts',(-30.853842156775,-1.93806865717107,-5.05899160207087)) ;
#61435 = CARTESIAN_POINT('Ctrl Pts',(-30.8529850286401,-1.93383069738739,
-5.0588063142689)) ;
#61436 = CARTESIAN_POINT('Ctrl Pts',(-30.8517007137438,-1.92747402059848,
-5.05852031717912)) ;
#61437 = CARTESIAN_POINT('Ctrl Pts',(-30.8512728437056,-1.92535518541571,
-5.05842362473753)) ;
#61438 = CARTESIAN_POINT('Ctrl Pts',(-30.8504226359227,-1.92114170712674,
-5.05822739713357)) ;
#61439 = CARTESIAN_POINT('Ctrl Pts',(-30.8500002923028,-1.9190470635643,-5.05812789722599)) ;
#61440 = CARTESIAN_POINT('Ctrl Pts',(-30.8493748470567,-1.91594131035434,
-5.05797567853019)) ;
#61441 = CARTESIAN_POINT('Ctrl Pts',(-30.8491677129878,-1.9149120984522,-5.05792443286985)) ;
#61442 = CARTESIAN_POINT('Ctrl Pts',(-30.8487568346472,-1.91286876134158,
-5.05782053632988)) ;
#61443 = CARTESIAN_POINT('Ctrl Pts',(-30.8485530899563,-1.91185463609014,
-5.05776788795337)) ;
#61444 = CARTESIAN_POINT('Ctrl Pts',(-30.848149756389,-1.90984448796971,-5.05766036570063)) ;
#61445 = CARTESIAN_POINT('Ctrl Pts',(-30.8479501615709,-1.90884846692931,
-5.05760553040331)) ;
#61446 = CARTESIAN_POINT('Ctrl Pts',(-30.8476546035702,-1.90737028791818,
-5.05752013963832)) ;
#61447 = CARTESIAN_POINT('Ctrl Pts',(-30.8475567249699,-1.90688020417638,
-5.05749114338188)) ;
#61448 = CARTESIAN_POINT('Ctrl Pts',(-30.8473624264111,-1.90590570765277,
-5.05743149758875)) ;
#61449 = CARTESIAN_POINT('Ctrl Pts',(-30.847266002424,-1.90542129422109,-5.05740087179522)) ;
#61450 = CARTESIAN_POINT('Ctrl Pts',(-30.8471212998049,-1.90469230606236,
-5.05735231470238)) ;
#61451 = CARTESIAN_POINT('Ctrl Pts',(-30.8470697753425,-1.90443237036805,
-5.0573345601076)) ;
#61452 = CARTESIAN_POINT('Ctrl Pts',(-30.8469645620923,-1.90390032261935,
-5.05729669872756)) ;
#61453 = CARTESIAN_POINT('Ctrl Pts',(-30.8469108724233,-1.90362821037409,
-5.05727659707329)) ;
#61454 = CARTESIAN_POINT('Ctrl Pts',(-30.84680399421,-1.9030842986835,-5.05723373660809)) ;
#61455 = CARTESIAN_POINT('Ctrl Pts',(-30.8467507980804,-1.90281253803109,
-5.05721107361941)) ;
#61456 = CARTESIAN_POINT('Ctrl Pts',(-30.8465314744222,-1.90163369641421,
-5.05704304528566)) ;
#61457 = CARTESIAN_POINT('Ctrl Pts',(-30.8465224173482,-1.90158501559319,
-5.0570361064763)) ;
#61458 = CARTESIAN_POINT('Ctrl Pts',(-30.8465133602742,-1.90153633477217,
-5.05702916766694)) ;
#61459 = CARTESIAN_POINT('',(-28.127216244771,-15.0366437072153,-19.0528197166343)) ;
#61460 = CARTESIAN_POINT('',(-28.1105818993065,-15.0366437072153,-19.0773535407052)) ;
#61461 = CARTESIAN_POINT('Origin',(1.13057562514854,-21.6462763158694,0.766549294070828)) ;
#61462 = CARTESIAN_POINT('',(-25.8721458584193,-1.90153624169001,-17.541750139775)) ;
#61463 = CARTESIAN_POINT('Ctrl Pts',(-25.8721458739748,-1.90153633180959,
-17.5417501500193)) ;
#61464 = CARTESIAN_POINT('Ctrl Pts',(-25.8721577813986,-1.90158489219061,
-17.5417504704143)) ;
#61465 = CARTESIAN_POINT('Ctrl Pts',(-25.8723630148979,-1.90242186726325,
-17.5417559926659)) ;
#61466 = CARTESIAN_POINT('Ctrl Pts',(-25.8724455119795,-1.90282329663281,
-17.5417821463521)) ;
#61467 = CARTESIAN_POINT('Ctrl Pts',(-25.8725001466519,-1.90309737347548,
-17.541802496001)) ;
#61468 = CARTESIAN_POINT('Ctrl Pts',(-25.8726080673333,-1.90364591781988,
-17.5418453282902)) ;
#61469 = CARTESIAN_POINT('Ctrl Pts',(-25.8726612926932,-1.90392034648623,
-17.5418678860799)) ;
#61470 = CARTESIAN_POINT('Ctrl Pts',(-25.8727645374215,-1.90445692193452,
-17.5419132072959)) ;
#61471 = CARTESIAN_POINT('Ctrl Pts',(-25.8728145539649,-1.90471906890233,
-17.5419359749571)) ;
#61472 = CARTESIAN_POINT('Ctrl Pts',(-25.8729541313185,-1.90545432128996,
-17.542000873042)) ;
#61473 = CARTESIAN_POINT('Ctrl Pts',(-25.8730459476192,-1.90594291892127,
-17.5420453819276)) ;
#61474 = CARTESIAN_POINT('Ctrl Pts',(-25.8732295327942,-1.90692583257785,
-17.5421365754662)) ;
#61475 = CARTESIAN_POINT('Ctrl Pts',(-25.8733212882221,-1.90742014925225,
-17.5421832801901)) ;
#61476 = CARTESIAN_POINT('Ctrl Pts',(-25.8735968579746,-1.90891109528826,
-17.5423258913389)) ;
#61477 = CARTESIAN_POINT('Ctrl Pts',(-25.8737809976514,-1.90991571864561,
-17.5424242617222)) ;
#61478 = CARTESIAN_POINT('Ctrl Pts',(-25.8741508279643,-1.91194322733529,
-17.5426254400316)) ;
#61479 = CARTESIAN_POINT('Ctrl Pts',(-25.8743364962106,-1.91296611084088,
-17.5427282803074)) ;
#61480 = CARTESIAN_POINT('Ctrl Pts',(-25.8747093476694,-1.91502709440813,
-17.5429373300016)) ;
#61481 = CARTESIAN_POINT('Ctrl Pts',(-25.8748965294705,-1.91606519451243,
-17.5430435415171)) ;
#61482 = CARTESIAN_POINT('Ctrl Pts',(-25.8754599872941,-1.91919776827529,
-17.5433660847172)) ;
#61483 = CARTESIAN_POINT('Ctrl Pts',(-25.8758381993206,-1.92131050012656,
-17.543586284653)) ;
#61484 = CARTESIAN_POINT('Ctrl Pts',(-25.8765967515513,-1.92556036292269,
-17.5440325307497)) ;
#61485 = CARTESIAN_POINT('Ctrl Pts',(-25.8769770716705,-1.92769749432427,
-17.5442586067019)) ;
#61486 = CARTESIAN_POINT('Ctrl Pts',(-25.8781157276811,-1.93410905980131,
-17.5449402962874)) ;
#61487 = CARTESIAN_POINT('Ctrl Pts',(-25.8788717873392,-1.93838361207301,
-17.54539931064)) ;
#61488 = CARTESIAN_POINT('Ctrl Pts',(-25.8803463297327,-1.94673863693752,
-17.5463012906347)) ;
#61489 = CARTESIAN_POINT('Ctrl Pts',(-25.8810647715554,-1.9508191102094,-17.5467443168686)) ;
#61490 = CARTESIAN_POINT('Ctrl Pts',(-25.8824305365614,-1.95858685131004,
-17.5475904621936)) ;
#61491 = CARTESIAN_POINT('Ctrl Pts',(-25.8831141360427,-1.96248050149649,
-17.5480160787776)) ;
#61492 = CARTESIAN_POINT('Ctrl Pts',(-25.8844839505559,-1.97029131383045,
-17.5488721126596)) ;
#61493 = CARTESIAN_POINT('Ctrl Pts',(-25.8851701645755,-1.97420847599133,
-17.5493025314554)) ;
#61494 = CARTESIAN_POINT('Ctrl Pts',(-25.8872329915253,-1.98599408922772,
-17.5506001828878)) ;
#61495 = CARTESIAN_POINT('Ctrl Pts',(-25.8886138158768,-1.99389666664285,
-17.5514737712874)) ;
#61496 = CARTESIAN_POINT('Ctrl Pts',(-25.8913870826419,-2.00978675025176,
-17.5532350880485)) ;
#61497 = CARTESIAN_POINT('Ctrl Pts',(-25.8927795088963,-2.01777425627098,
-17.5541228401787)) ;
#61498 = CARTESIAN_POINT('Ctrl Pts',(-25.8955756988877,-2.033828127578,-17.5559106631073)) ;
#61499 = CARTESIAN_POINT('Ctrl Pts',(-25.8969794621623,-2.04189449287027,
-17.5568107345884)) ;
#61500 = CARTESIAN_POINT('Ctrl Pts',(-25.9012069175401,-2.06620277837357,
-17.5595273160892)) ;
#61501 = CARTESIAN_POINT('Ctrl Pts',(-25.9040468319125,-2.08255388475044,
-17.5613601082406)) ;
#61502 = CARTESIAN_POINT('Ctrl Pts',(-25.9097637854993,-2.1154987366553,-17.5650602902202)) ;
#61503 = CARTESIAN_POINT('Ctrl Pts',(-25.9126407976318,-2.13209248238822,
-17.5669277200662)) ;
#61504 = CARTESIAN_POINT('Ctrl Pts',(-25.9184247760832,-2.16547409486571,
-17.5706898863848)) ;
#61505 = CARTESIAN_POINT('Ctrl Pts',(-25.9213317317786,-2.18226195777091,
-17.5725846371116)) ;
#61506 = CARTESIAN_POINT('Ctrl Pts',(-25.9271679807421,-2.21598327435907,
-17.5763948074275)) ;
#61507 = CARTESIAN_POINT('Ctrl Pts',(-25.9300972727453,-2.2329167280499,-17.5783102288843)) ;
#61508 = CARTESIAN_POINT('Ctrl Pts',(-25.9389068846414,-2.28386269378459,
-17.5840780546505)) ;
#61509 = CARTESIAN_POINT('Ctrl Pts',(-25.9448089812287,-2.3180208102006,-17.587951960061)) ;
#61510 = CARTESIAN_POINT('Ctrl Pts',(-25.9566069656804,-2.38633716148301,
-17.5957089716833)) ;
#61511 = CARTESIAN_POINT('Ctrl Pts',(-25.9625028263135,-2.4204953826845,-17.5995921130256)) ;
#61512 = CARTESIAN_POINT('Ctrl Pts',(-25.9742230316132,-2.48842373596822,
-17.6073209586855)) ;
#61513 = CARTESIAN_POINT('Ctrl Pts',(-25.980047366237,-2.52219386809602,-17.6111666778318)) ;
#61514 = CARTESIAN_POINT('Ctrl Pts',(-25.9973144624853,-2.62233986386287,
-17.6225787316677)) ;
#61515 = CARTESIAN_POINT('Ctrl Pts',(-26.0085513815388,-2.68755132653018,
-17.6300198666794)) ;
#61516 = CARTESIAN_POINT('Ctrl Pts',(-26.030971806787,-2.81770994459726,-17.6448835826939)) ;
#61517 = CARTESIAN_POINT('Ctrl Pts',(-26.042725988924,-2.88597501437035,-17.6526863133006)) ;
#61518 = CARTESIAN_POINT('Ctrl Pts',(-26.06629829559,-3.02291720221945,-17.6683492047793)) ;
#61519 = CARTESIAN_POINT('Ctrl Pts',(-26.0781163980912,-3.09159432036822,
-17.6762093981667)) ;
#61520 = CARTESIAN_POINT('Ctrl Pts',(-26.101815783507,-3.22934731017729,-17.6919834431879)) ;
#61521 = CARTESIAN_POINT('Ctrl Pts',(-26.1136970574824,-3.29842318182397,
-17.6998973080004)) ;
#61522 = CARTESIAN_POINT('Ctrl Pts',(-26.1375215228422,-3.43696038516605,
-17.7157756633011)) ;
#61523 = CARTESIAN_POINT('Ctrl Pts',(-26.1494647130785,-3.50642171686489,
-17.7237401554819)) ;
#61524 = CARTESIAN_POINT('Ctrl Pts',(-26.1853848266085,-3.71536396318966,
-17.7477056693359)) ;
#61525 = CARTESIAN_POINT('Ctrl Pts',(-26.2094523540066,-3.85540312838846,
-17.7637786376903)) ;
#61526 = CARTESIAN_POINT('Ctrl Pts',(-26.2578145218226,-4.13686379057535,
-17.7960986563036)) ;
#61527 = CARTESIAN_POINT('Ctrl Pts',(-26.2821091286492,-4.2782852876429,-17.812345756135)) ;
#61528 = CARTESIAN_POINT('Ctrl Pts',(-26.3309094580666,-4.56240428036738,
-17.8449984743132)) ;
#61529 = CARTESIAN_POINT('Ctrl Pts',(-26.3554151655153,-4.70510177511429,
-17.8614041146579)) ;
#61530 = CARTESIAN_POINT('Ctrl Pts',(-26.4046209589496,-4.99166642802495,
-17.8943594411247)) ;
#61531 = CARTESIAN_POINT('Ctrl Pts',(-26.4293210374488,-5.13553358620376,
-17.9109091382938)) ;
#61532 = CARTESIAN_POINT('Ctrl Pts',(-26.4788983993845,-5.42433123356354,
-17.9441387502879)) ;
#61533 = CARTESIAN_POINT('Ctrl Pts',(-26.5037756791504,-5.56926172274222,
-17.9608186705255)) ;
#61534 = CARTESIAN_POINT('Ctrl Pts',(-26.553689992587,-5.86007970017216,-17.9942953098974)) ;
#61535 = CARTESIAN_POINT('Ctrl Pts',(-26.5787270255941,-6.00596718842478,
-18.0110920300097)) ;
#61536 = CARTESIAN_POINT('Ctrl Pts',(-26.6540513077496,-6.44490565440716,
-18.0616376606911)) ;
#61537 = CARTESIAN_POINT('Ctrl Pts',(-26.7045517822166,-6.73923262866378,
-18.0955419776558)) ;
#61538 = CARTESIAN_POINT('Ctrl Pts',(-26.8059788688949,-7.33043857872017,
-18.163661888986)) ;
#61539 = CARTESIAN_POINT('Ctrl Pts',(-26.8569054594421,-7.62731755455363,
-18.1978775153162)) ;
#61540 = CARTESIAN_POINT('Ctrl Pts',(-26.9590411910106,-8.22277685056084,
-18.2665185632472)) ;
#61541 = CARTESIAN_POINT('Ctrl Pts',(-27.0102503212944,-8.52135717073135,
-18.3009440006836)) ;
#61542 = CARTESIAN_POINT('Ctrl Pts',(-27.1128069266711,-9.11936849902312,
-18.369904101061)) ;
#61543 = CARTESIAN_POINT('Ctrl Pts',(-27.1641543967405,-9.41879950715136,
-18.4044387714126)) ;
#61544 = CARTESIAN_POINT('Ctrl Pts',(-27.318187428206,-10.3170925797302,-18.5080566328313)) ;
#61545 = CARTESIAN_POINT('Ctrl Pts',(-27.4208636968131,-10.9159546769438,
-18.5771535417962)) ;
#61546 = CARTESIAN_POINT('Ctrl Pts',(-27.6250318782106,-12.1068736983314,
-18.7145881249444)) ;
#61547 = CARTESIAN_POINT('Ctrl Pts',(-27.7265237475234,-12.6989306225571,
-18.7829258632698)) ;
#61548 = CARTESIAN_POINT('Ctrl Pts',(-27.9283695022688,-13.8764819136135,
-18.9188630557109)) ;
#61549 = CARTESIAN_POINT('Ctrl Pts',(-28.0286949437812,-14.4618113900316,
-18.9864437399958)) ;
#61550 = CARTESIAN_POINT('Ctrl Pts',(-28.1272162447821,-15.0366437072153,
-19.0528197166179)) ;
#61551 = CARTESIAN_POINT('Ctrl Pts',(-28.1105818992957,-15.0366437072153,
-19.0773535407212)) ;
#61552 = CARTESIAN_POINT('Ctrl Pts',(-28.1094142530856,-15.0298036696733,
-19.0765568221348)) ;
#61553 = CARTESIAN_POINT('Ctrl Pts',(-28.1082463538653,-15.0229621458316,
-19.0757599293754)) ;
#61554 = CARTESIAN_POINT('Ctrl Pts',(-28.0100756837395,-14.4478805124694,
-19.0087749993418)) ;
#61555 = CARTESIAN_POINT('Ctrl Pts',(-27.9113355275183,-13.8694340292541,
-18.9413908806558)) ;
#61556 = CARTESIAN_POINT('Ctrl Pts',(-27.711545210769,-12.6989306216801,-18.8050175518778)) ;
#61557 = CARTESIAN_POINT('Ctrl Pts',(-27.6104950294686,-12.1068736973243,
-18.7360283724237)) ;
#61558 = CARTESIAN_POINT('Ctrl Pts',(-27.4072510671399,-10.9159546756748,
-18.5972306680339)) ;
#61559 = CARTESIAN_POINT('Ctrl Pts',(-27.305057242619,-10.3170925783295,-18.5274222072277)) ;
#61560 = CARTESIAN_POINT('Ctrl Pts',(-27.1517851594422,-9.41879950555309,
-18.4226820309762)) ;
#61561 = CARTESIAN_POINT('Ctrl Pts',(-27.1006975967947,-9.11936849735901,
-18.3877640258319)) ;
#61562 = CARTESIAN_POINT('Ctrl Pts',(-26.9986751561934,-8.52135716893573,
-18.318016091304)) ;
#61563 = CARTESIAN_POINT('Ctrl Pts',(-26.9477402732135,-8.22277684869958,
-18.2831861693315)) ;
#61564 = CARTESIAN_POINT('Ctrl Pts',(-26.8461700063625,-7.62731755256142,
-18.2137111232893)) ;
#61565 = CARTESIAN_POINT('Ctrl Pts',(-26.7955346117563,-7.33043857666269,
-18.1790660150537)) ;
#61566 = CARTESIAN_POINT('Ctrl Pts',(-26.6947107651878,-6.73923262647628,
-18.1100563910771)) ;
#61567 = CARTESIAN_POINT('Ctrl Pts',(-26.6445222915509,-6.44490565215494,
-18.0756919072913)) ;
#61568 = CARTESIAN_POINT('Ctrl Pts',(-26.5696861864936,-6.00596718607602,
-18.0244262692216)) ;
#61569 = CARTESIAN_POINT('Ctrl Pts',(-26.5448152633208,-5.86007969779135,
-18.007384555421)) ;
#61570 = CARTESIAN_POINT('Ctrl Pts',(-26.4952410527753,-5.56926172029744,
-17.9734063017893)) ;
#61571 = CARTESIAN_POINT('Ctrl Pts',(-26.4705377647392,-5.42433123108689,
-17.9564697629374)) ;
#61572 = CARTESIAN_POINT('Ctrl Pts',(-26.4213177554839,-5.13553358366361,
-17.9227130951479)) ;
#61573 = CARTESIAN_POINT('Ctrl Pts',(-26.3968010305949,-4.99166642545318,
-17.9058929716238)) ;
#61574 = CARTESIAN_POINT('Ctrl Pts',(-26.3479733578889,-4.70510177247949,
-17.8723799587828)) ;
#61575 = CARTESIAN_POINT('Ctrl Pts',(-26.3236624025812,-4.5624042777012,-17.8556870805081)) ;
#61576 = CARTESIAN_POINT('Ctrl Pts',(-26.2752659236338,-4.27828528491426,
-17.8224387274259)) ;
#61577 = CARTESIAN_POINT('Ctrl Pts',(-26.2511803851627,-4.13686378781561,
-17.805883274828)) ;
#61578 = CARTESIAN_POINT('Ctrl Pts',(-26.2032551566929,-3.85540312556682,
-17.7729188188696)) ;
#61579 = CARTESIAN_POINT('Ctrl Pts',(-26.1794154330761,-3.71536396033722,
-17.756509865063)) ;
#61580 = CARTESIAN_POINT('Ctrl Pts',(-26.1438566240579,-3.5064217139665,-17.7320114669046)) ;
#61581 = CARTESIAN_POINT('Ctrl Pts',(-26.1320371658283,-3.43696038225238,
-17.7238644836613)) ;
#61582 = CARTESIAN_POINT('Ctrl Pts',(-26.1084681997397,-3.29842317887984,
-17.7076092951171)) ;
#61583 = CARTESIAN_POINT('Ctrl Pts',(-26.096718690731,-3.22934730721796,-17.6995010915124)) ;
#61584 = CARTESIAN_POINT('Ctrl Pts',(-26.0732929233236,-3.09159431737861,
-17.6833234901097)) ;
#61585 = CARTESIAN_POINT('Ctrl Pts',(-26.0616166559903,-3.02291719921474,
-17.6752541054946)) ;
#61586 = CARTESIAN_POINT('Ctrl Pts',(-26.0383411843299,-2.88597501133551,
-17.6591534151252)) ;
#61587 = CARTESIAN_POINT('Ctrl Pts',(-26.0267419579497,-2.81770994154741,
-17.6511221418702)) ;
#61588 = CARTESIAN_POINT('Ctrl Pts',(-26.0046352570039,-2.68755132374404,
-17.6357957172242)) ;
#61589 = CARTESIAN_POINT('Ctrl Pts',(-25.9935634033709,-2.62233986136937,
-17.6281111290389)) ;
#61590 = CARTESIAN_POINT('Ctrl Pts',(-25.9765706599549,-2.52219386605188,
-17.6162944352138)) ;
#61591 = CARTESIAN_POINT('Ctrl Pts',(-25.9708422679448,-2.48842373407561,
-17.6123072113547)) ;
#61592 = CARTESIAN_POINT('Ctrl Pts',(-25.9593242551378,-2.4204953810967,-17.6042801541909)) ;
#61593 = CARTESIAN_POINT('Ctrl Pts',(-25.9535346242879,-2.38633716004853,
-17.6002403356964)) ;
#61594 = CARTESIAN_POINT('Ctrl Pts',(-25.941961656926,-2.31802080907265,-17.5921514488089)) ;
#61595 = CARTESIAN_POINT('Ctrl Pts',(-25.9361782978659,-2.2838626928099,-17.5881024187041)) ;
#61596 = CARTESIAN_POINT('Ctrl Pts',(-25.9275593485474,-2.23291672730382,
-17.5820533867584)) ;
#61597 = CARTESIAN_POINT('Ctrl Pts',(-25.9246957238749,-2.21598327368894,
-17.5800411132628)) ;
#61598 = CARTESIAN_POINT('Ctrl Pts',(-25.9189959459532,-2.1822619572521,-17.5760296632747)) ;
#61599 = CARTESIAN_POINT('Ctrl Pts',(-25.9161597914317,-2.16547409442222,
-17.5740304886564)) ;
#61600 = CARTESIAN_POINT('Ctrl Pts',(-25.9105239554163,-2.13209248209452,
-17.5700498286465)) ;
#61601 = CARTESIAN_POINT('Ctrl Pts',(-25.9077242646122,-2.11549873643605,
-17.5680683584003)) ;
#61602 = CARTESIAN_POINT('Ctrl Pts',(-25.9021708190636,-2.08255388467903,
-17.5641270201609)) ;
#61603 = CARTESIAN_POINT('Ctrl Pts',(-25.8994170371719,-2.06620277837558,
-17.5621671921317)) ;
#61604 = CARTESIAN_POINT('Ctrl Pts',(-25.8953286536826,-2.04189449298133,
-17.5592454949812)) ;
#61605 = CARTESIAN_POINT('Ctrl Pts',(-25.8939729218816,-2.03382812772519,
-17.5582745823897)) ;
#61606 = CARTESIAN_POINT('Ctrl Pts',(-25.8912770994085,-2.01777425649022,
-17.556338728473)) ;
#61607 = CARTESIAN_POINT('Ctrl Pts',(-25.8899370082718,-2.00978675050687,
-17.5553737878323)) ;
#61608 = CARTESIAN_POINT('Ctrl Pts',(-25.8872742941722,-1.99389666696925,
-17.5534494181145)) ;
#61609 = CARTESIAN_POINT('Ctrl Pts',(-25.8859516551153,-1.98599408958961,
-17.5524900128389)) ;
#61610 = CARTESIAN_POINT('Ctrl Pts',(-25.8839826361903,-1.97420847640609,
-17.5510540049405)) ;
#61611 = CARTESIAN_POINT('Ctrl Pts',(-25.8833287931713,-1.97029131426291,
-17.5505758424973)) ;
#61612 = CARTESIAN_POINT('Ctrl Pts',(-25.8820265370122,-1.96248050196401,
-17.5496201675104)) ;
#61613 = CARTESIAN_POINT('Ctrl Pts',(-25.8813781228567,-1.9585868517949,-17.5491426564597)) ;
#61614 = CARTESIAN_POINT('Ctrl Pts',(-25.8800865517807,-1.95081911052775,
-17.5481870832136)) ;
#61615 = CARTESIAN_POINT('Ctrl Pts',(-25.8794090679542,-1.94673863706264,
-17.5476836483835)) ;
#61616 = CARTESIAN_POINT('Ctrl Pts',(-25.8780253650712,-1.93838361180268,
-17.5466476899886)) ;
#61617 = CARTESIAN_POINT('Ctrl Pts',(-25.8773191048395,-1.93410905932831,
-17.5461152269026)) ;
#61618 = CARTESIAN_POINT('Ctrl Pts',(-25.8762643710015,-1.92769749354789,
-17.5453097612609)) ;
#61619 = CARTESIAN_POINT('Ctrl Pts',(-25.8759135807207,-1.92556036204565,
-17.5450401320186)) ;
#61620 = CARTESIAN_POINT('Ctrl Pts',(-25.8752182593306,-1.9213104990485,-17.544500627335)) ;
#61621 = CARTESIAN_POINT('Ctrl Pts',(-25.8748737080166,-1.91919776709772,
-17.5442307815258)) ;
#61622 = CARTESIAN_POINT('Ctrl Pts',(-25.8743655156321,-1.91606519318668,
-17.5438267278466)) ;
#61623 = CARTESIAN_POINT('Ctrl Pts',(-25.8741975644428,-1.91502709303237,
-17.5436921532823)) ;
#61624 = CARTESIAN_POINT('Ctrl Pts',(-25.8738653555782,-1.91296610936764,
-17.5434231602105)) ;
#61625 = CARTESIAN_POINT('Ctrl Pts',(-25.8737010964528,-1.91194322581388,
-17.543288743826)) ;
#61626 = CARTESIAN_POINT('Ctrl Pts',(-25.8733773181643,-1.9099157170284,-17.5430196438268)) ;
#61627 = CARTESIAN_POINT('Ctrl Pts',(-25.8732177772496,-1.90891109362396,
-17.5428849929664)) ;
#61628 = CARTESIAN_POINT('Ctrl Pts',(-25.8729832959266,-1.90742014751768,
-17.542681780892)) ;
#61629 = CARTESIAN_POINT('Ctrl Pts',(-25.8729059461416,-1.90692583082018,
-17.5426138294259)) ;
#61630 = CARTESIAN_POINT('Ctrl Pts',(-25.8727532775796,-1.90594291711709,
-17.5424770372775)) ;
#61631 = CARTESIAN_POINT('Ctrl Pts',(-25.8726779451098,-1.90545431946123,
-17.5424082165512)) ;
#61632 = CARTESIAN_POINT('Ctrl Pts',(-25.8725659934106,-1.90471906717225,
-17.5423025737106)) ;
#61633 = CARTESIAN_POINT('Ctrl Pts',(-25.8725263298085,-1.90445692033434,
-17.5422645366511)) ;
#61634 = CARTESIAN_POINT('Ctrl Pts',(-25.8724460126798,-1.90392034514695,
-17.5421853998518)) ;
#61635 = CARTESIAN_POINT('Ctrl Pts',(-25.8724053562799,-1.90364591661258,
-17.5421443042816)) ;
#61636 = CARTESIAN_POINT('Ctrl Pts',(-25.8723256205637,-1.90309737253521,
-17.5420599023772)) ;
#61637 = CARTESIAN_POINT('Ctrl Pts',(-25.8722864938872,-1.90282329582858,
-17.5420166801957)) ;
#61638 = CARTESIAN_POINT('Ctrl Pts',(-25.872156512694,-1.90163369816862,-17.5417703145868)) ;
#61639 = CARTESIAN_POINT('Ctrl Pts',(-25.8721511933344,-1.9015850149891,-17.5417602323031)) ;
#61640 = CARTESIAN_POINT('Ctrl Pts',(-25.8721458739748,-1.90153633180959,
-17.5417501500193)) ;
#61641 = CARTESIAN_POINT('',(-17.5274987345151,-15.0366437072153,-29.1021824086485)) ;
#61642 = CARTESIAN_POINT('',(-17.5021003261057,-15.0366437072153,-29.1174641239516)) ;
#61643 = CARTESIAN_POINT('Origin',(0.704216953074891,-21.6462763158693,1.17041768075435)) ;
#61644 = CARTESIAN_POINT('',(-16.1153339290263,-1.90153624083151,-26.7838933247298)) ;
#61645 = CARTESIAN_POINT('Ctrl Pts',(-16.1153339387476,-1.90153633009259,
-26.783893340409)) ;
#61646 = CARTESIAN_POINT('Ctrl Pts',(-16.1153446126417,-1.90158489024226,
-26.7838986300072)) ;
#61647 = CARTESIAN_POINT('Ctrl Pts',(-16.1155284746913,-1.90242135803618,
-26.7839897454288)) ;
#61648 = CARTESIAN_POINT('Ctrl Pts',(-16.1155923341218,-1.90282255286718,
-26.7840480837299)) ;
#61649 = CARTESIAN_POINT('Ctrl Pts',(-16.1156333539989,-1.90309646971259,
-26.7840894668884)) ;
#61650 = CARTESIAN_POINT('Ctrl Pts',(-16.1157132749115,-1.90364469403042,
-26.7841736022824)) ;
#61651 = CARTESIAN_POINT('Ctrl Pts',(-16.1157520893281,-1.90391896267546,
-26.7842163972704)) ;
#61652 = CARTESIAN_POINT('Ctrl Pts',(-16.1158267233644,-1.90445522534681,
-26.7843008287304)) ;
#61653 = CARTESIAN_POINT('Ctrl Pts',(-16.1158625386521,-1.90471721955859,
-26.7843424678536)) ;
#61654 = CARTESIAN_POINT('Ctrl Pts',(-16.1159619132824,-1.90545203961471,
-26.7844599019948)) ;
#61655 = CARTESIAN_POINT('Ctrl Pts',(-16.116026520158,-1.90594034860819,-26.7845388010006)) ;
#61656 = CARTESIAN_POINT('Ctrl Pts',(-16.1161547774474,-1.90692268162604,
-26.7846985528625)) ;
#61657 = CARTESIAN_POINT('Ctrl Pts',(-16.1162184071348,-1.90741670630277,
-26.7847794183467)) ;
#61658 = CARTESIAN_POINT('Ctrl Pts',(-16.1164085234146,-1.90890677163164,
-26.7850244071299)) ;
#61659 = CARTESIAN_POINT('Ctrl Pts',(-16.1165342707288,-1.90991080157223,
-26.7851909021158)) ;
#61660 = CARTESIAN_POINT('Ctrl Pts',(-16.1167853089992,-1.91193711267859,
-26.7855285685486)) ;
#61661 = CARTESIAN_POINT('Ctrl Pts',(-16.1169105661903,-1.9129593920142,-26.7856997598699)) ;
#61662 = CARTESIAN_POINT('Ctrl Pts',(-16.1171610404156,-1.91501915827682,
-26.7860458344817)) ;
#61663 = CARTESIAN_POINT('Ctrl Pts',(-16.1172862552069,-1.91605664524807,
-26.7862207191324)) ;
#61664 = CARTESIAN_POINT('Ctrl Pts',(-16.1176619936659,-1.9191873688501,-26.7867497211197)) ;
#61665 = CARTESIAN_POINT('Ctrl Pts',(-16.1179126495691,-1.92129885291666,
-26.7871081598582)) ;
#61666 = CARTESIAN_POINT('Ctrl Pts',(-16.1184134373359,-1.92554620580213,
-26.7878312338195)) ;
#61667 = CARTESIAN_POINT('Ctrl Pts',(-16.1186635385443,-1.92768207507662,
-26.7881958875967)) ;
#61668 = CARTESIAN_POINT('Ctrl Pts',(-16.119410298339,-1.93408985417006,-26.7892920224878)) ;
#61669 = CARTESIAN_POINT('Ctrl Pts',(-16.1199034641827,-1.938361882184,-26.7900256336217)) ;
#61670 = CARTESIAN_POINT('Ctrl Pts',(-16.1208624448587,-1.94671197326914,
-26.7914625314618)) ;
#61671 = CARTESIAN_POINT('Ctrl Pts',(-16.1213281971216,-1.95079003701957,
-26.7921658559786)) ;
#61672 = CARTESIAN_POINT('Ctrl Pts',(-16.1222119368299,-1.95855317037308,
-26.7935064607666)) ;
#61673 = CARTESIAN_POINT('Ctrl Pts',(-16.1226533878534,-1.96244450036797,
-26.7941793699059)) ;
#61674 = CARTESIAN_POINT('Ctrl Pts',(-16.1235366471255,-1.97025065831423,
-26.7955306405496)) ;
#61675 = CARTESIAN_POINT('Ctrl Pts',(-16.1239784538358,-1.97416548627894,
-26.7962090029826)) ;
#61676 = CARTESIAN_POINT('Ctrl Pts',(-16.1253049854054,-1.98594407659837,
-26.7982516474305)) ;
#61677 = CARTESIAN_POINT('Ctrl Pts',(-16.1261908623444,-1.99384194496366,
-26.799623462041)) ;
#61678 = CARTESIAN_POINT('Ctrl Pts',(-16.1279672192149,-2.0097225598768,-26.8023847928812)) ;
#61679 = CARTESIAN_POINT('Ctrl Pts',(-16.1288576745073,-2.01770530625007,
-26.8037743238935)) ;
#61680 = CARTESIAN_POINT('Ctrl Pts',(-16.1306436982338,-2.03374961128295,
-26.8065693176019)) ;
#61681 = CARTESIAN_POINT('Ctrl Pts',(-16.1315392659522,-2.04181116994711,
-26.8079747807291)) ;
#61682 = CARTESIAN_POINT('Ctrl Pts',(-16.1342337624508,-2.06610497051377,
-26.8122127999703)) ;
#61683 = CARTESIAN_POINT('Ctrl Pts',(-16.1360405716602,-2.08244633352993,
-26.8150669327094)) ;
#61684 = CARTESIAN_POINT('Ctrl Pts',(-16.1396733430882,-2.11537155415295,
-26.8208221597007)) ;
#61685 = CARTESIAN_POINT('Ctrl Pts',(-16.141499263935,-2.13195541196474,-26.8237232788947)) ;
#61686 = CARTESIAN_POINT('Ctrl Pts',(-16.1451668147149,-2.16531713295146,
-26.829562856173)) ;
#61687 = CARTESIAN_POINT('Ctrl Pts',(-16.1470084290269,-2.18209499228712,
-26.8325013227301)) ;
#61688 = CARTESIAN_POINT('Ctrl Pts',(-16.1507032439754,-2.21579621499984,
-26.8384063776397)) ;
#61689 = CARTESIAN_POINT('Ctrl Pts',(-16.1525564426753,-2.23271957838481,
-26.8413729671588)) ;
#61690 = CARTESIAN_POINT('Ctrl Pts',(-16.1581267045493,-2.28363518646551,
-26.8503014147369)) ;
#61691 = CARTESIAN_POINT('Ctrl Pts',(-16.1618544958079,-2.31777294879703,
-26.8562919142551)) ;
#61692 = CARTESIAN_POINT('Ctrl Pts',(-16.1693005829469,-2.38604859190971,
-26.8682786550392)) ;
#61693 = CARTESIAN_POINT('Ctrl Pts',(-16.17301883939,-2.42018645902605,-26.8742749167378)) ;
#61694 = CARTESIAN_POINT('Ctrl Pts',(-16.180406192469,-2.48807433543556,-26.8862034740195)) ;
#61695 = CARTESIAN_POINT('Ctrl Pts',(-16.1840752737782,-2.52182434477429,
-26.8921357788352)) ;
#61696 = CARTESIAN_POINT('Ctrl Pts',(-16.1949482476549,-2.62191066606263,
-26.9097328149812)) ;
#61697 = CARTESIAN_POINT('Ctrl Pts',(-16.2020179694901,-2.68708327092924,
-26.9211976081664)) ;
#61698 = CARTESIAN_POINT('Ctrl Pts',(-16.2161163182727,-2.81716036567911,
-26.9440872558194)) ;
#61699 = CARTESIAN_POINT('Ctrl Pts',(-16.2235030433896,-2.88538078045149,
-26.9560963934278)) ;
#61700 = CARTESIAN_POINT('Ctrl Pts',(-16.2383103870237,-3.02223338876827,
-26.9801935895711)) ;
#61701 = CARTESIAN_POINT('Ctrl Pts',(-16.2457309719123,-3.09086558238541,
-26.9922816683572)) ;
#61702 = CARTESIAN_POINT('Ctrl Pts',(-16.2606069272933,-3.22852846229517,
-27.0165330056586)) ;
#61703 = CARTESIAN_POINT('Ctrl Pts',(-16.2680622841446,-3.29755914857421,
-27.0286962723779)) ;
#61704 = CARTESIAN_POINT('Ctrl Pts',(-16.2830079107993,-3.43600572903974,
-27.0530947048677)) ;
#61705 = CARTESIAN_POINT('Ctrl Pts',(-16.2904981788528,-3.50542162322967,
-27.0653298716909)) ;
#61706 = CARTESIAN_POINT('Ctrl Pts',(-16.3130208735933,-3.71422719185778,
-27.1021387030916)) ;
#61707 = CARTESIAN_POINT('Ctrl Pts',(-16.3281052845003,-3.85417475169892,
-27.1268156420992)) ;
#61708 = CARTESIAN_POINT('Ctrl Pts',(-16.3584070420383,-4.13545129894057,
-27.176422711748)) ;
#61709 = CARTESIAN_POINT('Ctrl Pts',(-16.3736243373896,-4.27678028642054,
-27.2013528732623)) ;
#61710 = CARTESIAN_POINT('Ctrl Pts',(-16.4041838861447,-4.56071342529593,
-27.2514455589791)) ;
#61711 = CARTESIAN_POINT('Ctrl Pts',(-16.4195261165778,-4.70331757578152,
-27.2766080967833)) ;
#61712 = CARTESIAN_POINT('Ctrl Pts',(-16.4503264287325,-4.98969477505206,
-27.3271453850117)) ;
#61713 = CARTESIAN_POINT('Ctrl Pts',(-16.4657844990219,-5.13346782385208,
-27.3525201423181)) ;
#61714 = CARTESIAN_POINT('Ctrl Pts',(-16.4968067176875,-5.42207655689294,
-27.4034621211301)) ;
#61715 = CARTESIAN_POINT('Ctrl Pts',(-16.5123708604603,-5.56691224113146,
-27.4290293460064)) ;
#61716 = CARTESIAN_POINT('Ctrl Pts',(-16.5435950273506,-5.85753998267579,
-27.4803367664907)) ;
#61717 = CARTESIAN_POINT('Ctrl Pts',(-16.5592550504579,-6.00333203998292,
-27.506076962706)) ;
#61718 = CARTESIAN_POINT('Ctrl Pts',(-16.6063632327434,-6.44198337845498,
-27.5835280164297)) ;
#61719 = CARTESIAN_POINT('Ctrl Pts',(-16.6379395699958,-6.73611782147322,
-27.6354692987059)) ;
#61720 = CARTESIAN_POINT('Ctrl Pts',(-16.7013481215964,-7.32693703970546,
-27.7398130030787)) ;
#61721 = CARTESIAN_POINT('Ctrl Pts',(-16.733180302874,-7.62362181495312,-27.7922154450812)) ;
#61722 = CARTESIAN_POINT('Ctrl Pts',(-16.7970128957945,-8.21869159689002,
-27.897329174614)) ;
#61723 = CARTESIAN_POINT('Ctrl Pts',(-16.8290132910475,-8.51707660357599,
-27.950040472005)) ;
#61724 = CARTESIAN_POINT('Ctrl Pts',(-16.8930937212076,-9.11469674844867,
-28.055620186193)) ;
#61725 = CARTESIAN_POINT('Ctrl Pts',(-16.9251737484442,-9.41393188664231,
-28.1084886076062)) ;
#61726 = CARTESIAN_POINT('Ctrl Pts',(-17.0213995067575,-10.3116373494152,
-28.2671025015741)) ;
#61727 = CARTESIAN_POINT('Ctrl Pts',(-17.0855310480243,-10.9101077067561,
-28.372856519752)) ;
#61728 = CARTESIAN_POINT('Ctrl Pts',(-17.2130385160227,-12.1002476999845,
-28.5831789780471)) ;
#61729 = CARTESIAN_POINT('Ctrl Pts',(-17.2764143763867,-12.6919173359235,
-28.6877474581075)) ;
#61730 = CARTESIAN_POINT('Ctrl Pts',(-17.4027580047438,-13.8716326279716,
-28.8962559180836)) ;
#61731 = CARTESIAN_POINT('Ctrl Pts',(-17.4657003340837,-14.4594442697278,
-29.0001547637196)) ;
#61732 = CARTESIAN_POINT('Ctrl Pts',(-17.5274987345487,-15.0366437072153,
-29.1021824086283)) ;
#61733 = CARTESIAN_POINT('Ctrl Pts',(-17.502100326071,-15.0366437072153,-29.1174641239725)) ;
#61734 = CARTESIAN_POINT('Ctrl Pts',(-17.5010738690874,-15.026962147902,-29.1157466982005)) ;
#61735 = CARTESIAN_POINT('Ctrl Pts',(-17.5000470977353,-15.0172776029008,
-29.1140287414815)) ;
#61736 = CARTESIAN_POINT('Ctrl Pts',(-17.4388139593873,-14.4397231677713,
-29.0115753703577)) ;
#61737 = CARTESIAN_POINT('Ctrl Pts',(-17.3775338698389,-13.8616550697814,
-28.9090263622473)) ;
#61738 = CARTESIAN_POINT('Ctrl Pts',(-17.2535520883261,-12.6919173358369,
-28.7015032404052)) ;
#61739 = CARTESIAN_POINT('Ctrl Pts',(-17.1908503646563,-12.100247699885,-28.5965291457508)) ;
#61740 = CARTESIAN_POINT('Ctrl Pts',(-17.064753513795,-10.9101077066308,-28.3853579472788)) ;
#61741 = CARTESIAN_POINT('Ctrl Pts',(-17.0013583202276,-10.3116373492769,
-28.2791608833869)) ;
#61742 = CARTESIAN_POINT('Ctrl Pts',(-16.9062939918949,-9.41393188648451,
-28.1198481801811)) ;
#61743 = CARTESIAN_POINT('Ctrl Pts',(-16.8746106603403,-9.11469674828439,
-28.0667410748938)) ;
#61744 = CARTESIAN_POINT('Ctrl Pts',(-16.8113455255754,-8.51707660339873,
-27.9606708137394)) ;
#61745 = CARTESIAN_POINT('Ctrl Pts',(-16.7797637146953,-8.21869159670628,
-27.907707662486)) ;
#61746 = CARTESIAN_POINT('Ctrl Pts',(-16.7167941939307,-7.62362181475645,
-27.8020746396636)) ;
#61747 = CARTESIAN_POINT('Ctrl Pts',(-16.6854064676566,-7.32693703950234,
-27.7494047779567)) ;
#61748 = CARTESIAN_POINT('Ctrl Pts',(-16.622918648862,-6.73611782125726,-27.6445070870324)) ;
#61749 = CARTESIAN_POINT('Ctrl Pts',(-16.5918185232645,-6.44198337823263,
-27.5922792777087)) ;
#61750 = CARTESIAN_POINT('Ctrl Pts',(-16.545455454652,-6.00333203975106,-27.5143799039606)) ;
#61751 = CARTESIAN_POINT('Ctrl Pts',(-16.5300489682726,-5.85753998244076,
-27.4884871597568)) ;
#61752 = CARTESIAN_POINT('Ctrl Pts',(-16.4993439076299,-5.56691224089011,
-27.4368674034048)) ;
#61753 = CARTESIAN_POINT('Ctrl Pts',(-16.4840453323553,-5.42207655664842,
-27.4111403918658)) ;
#61754 = CARTESIAN_POINT('Ctrl Pts',(-16.4535685495787,-5.13346782360132,
-27.3598702351666)) ;
#61755 = CARTESIAN_POINT('Ctrl Pts',(-16.4383903364743,-4.98969477479818,
-27.3343270933781)) ;
#61756 = CARTESIAN_POINT('Ctrl Pts',(-16.4081671598198,-4.70331757552142,
-27.2834425542393)) ;
#61757 = CARTESIAN_POINT('Ctrl Pts',(-16.3931221848344,-4.56071342503274,
-27.2581011637657)) ;
#61758 = CARTESIAN_POINT('Ctrl Pts',(-16.3631790442451,-4.27678028615114,
-27.2076375975596)) ;
#61759 = CARTESIAN_POINT('Ctrl Pts',(-16.3482808558656,-4.13545129866813,
-27.18251543575)) ;
#61760 = CARTESIAN_POINT('Ctrl Pts',(-16.3186460113394,-3.85417475142036,
-27.1325070978543)) ;
#61761 = CARTESIAN_POINT('Ctrl Pts',(-16.3039093038976,-3.71422719157617,
-27.1076209526123)) ;
#61762 = CARTESIAN_POINT('Ctrl Pts',(-16.2819380783363,-3.50542162294355,
-27.0704803132146)) ;
#61763 = CARTESIAN_POINT('Ctrl Pts',(-16.2746366658577,-3.4360057287521,-27.0581315157619)) ;
#61764 = CARTESIAN_POINT('Ctrl Pts',(-16.2600810145637,-3.29755914828356,
-27.0334984428819)) ;
#61765 = CARTESIAN_POINT('Ctrl Pts',(-16.2528267739962,-3.22852846200301,
-27.0212141685092)) ;
#61766 = CARTESIAN_POINT('Ctrl Pts',(-16.23836844846,-3.09086558209025,-26.9967115516668)) ;
#61767 = CARTESIAN_POINT('Ctrl Pts',(-16.2311643498569,-3.02223338847166,
-26.9844932174041)) ;
#61768 = CARTESIAN_POINT('Ctrl Pts',(-16.2168100715694,-2.8853807801519,-26.9601234208857)) ;
#61769 = CARTESIAN_POINT('Ctrl Pts',(-16.2096598582408,-2.81716036537802,
-26.9479719788555)) ;
#61770 = CARTESIAN_POINT('Ctrl Pts',(-16.1960403644138,-2.68708327060819,
-26.9247942137304)) ;
#61771 = CARTESIAN_POINT('Ctrl Pts',(-16.1892225989311,-2.62191066572221,
-26.9131778234331)) ;
#61772 = CARTESIAN_POINT('Ctrl Pts',(-16.1787683982861,-2.52182434440409,
-26.8953288197866)) ;
#61773 = CARTESIAN_POINT('Ctrl Pts',(-16.1752457641844,-2.48807433505531,
-26.8893084006073)) ;
#61774 = CARTESIAN_POINT('Ctrl Pts',(-16.1681670386877,-2.42018645862559,
-26.8771941482657)) ;
#61775 = CARTESIAN_POINT('Ctrl Pts',(-16.1646109319503,-2.3860485914991,-26.8711003243238)) ;
#61776 = CARTESIAN_POINT('Ctrl Pts',(-16.1575083121581,-2.31777294836608,
-26.8589069260889)) ;
#61777 = CARTESIAN_POINT('Ctrl Pts',(-16.1539617625691,-2.2836351860244,-26.8528073770738)) ;
#61778 = CARTESIAN_POINT('Ctrl Pts',(-16.148682529273,-2.23271957792855,-26.8437038234067)) ;
#61779 = CARTESIAN_POINT('Ctrl Pts',(-16.1469295656237,-2.21579621453857,
-26.8406769244575)) ;
#61780 = CARTESIAN_POINT('Ctrl Pts',(-16.1434430609953,-2.18209499181582,
-26.8346465333844)) ;
#61781 = CARTESIAN_POINT('Ctrl Pts',(-16.1417095180719,-2.16531713247511,
-26.831643042429)) ;
#61782 = CARTESIAN_POINT('Ctrl Pts',(-16.1382680929536,-2.13195541147845,
-26.8256674098519)) ;
#61783 = CARTESIAN_POINT('Ctrl Pts',(-16.1365601959534,-2.11537155366181,
-26.8226952780645)) ;
#61784 = CARTESIAN_POINT('Ctrl Pts',(-16.1331770043878,-2.082446333029,-26.81678988385)) ;
#61785 = CARTESIAN_POINT('Ctrl Pts',(-16.1315016684144,-2.06610497000793,
-26.8138566462883)) ;
#61786 = CARTESIAN_POINT('Ctrl Pts',(-16.1290194522718,-2.04181116943406,
-26.809490902193)) ;
#61787 = CARTESIAN_POINT('Ctrl Pts',(-16.1281972001465,-2.03374961076746,
-26.8080413265364)) ;
#61788 = CARTESIAN_POINT('Ctrl Pts',(-16.1265643781298,-2.01770530572983,
-26.8051541544166)) ;
#61789 = CARTESIAN_POINT('Ctrl Pts',(-16.1257538075399,-2.00972255935432,
-26.803716558373)) ;
#61790 = CARTESIAN_POINT('Ctrl Pts',(-16.1241461990354,-1.99384194443646,
-26.8008536950086)) ;
#61791 = CARTESIAN_POINT('Ctrl Pts',(-16.1233491365322,-1.98594407606877,
-26.7994284425245)) ;
#61792 = CARTESIAN_POINT('Ctrl Pts',(-16.1221657941448,-1.97416548574584,
-26.7972996440034)) ;
#61793 = CARTESIAN_POINT('Ctrl Pts',(-16.1217733987392,-1.97025065777981,
-26.7965915517745)) ;
#61794 = CARTESIAN_POINT('Ctrl Pts',(-16.1209932609488,-1.96244449983124,
-26.7951782349933)) ;
#61795 = CARTESIAN_POINT('Ctrl Pts',(-16.1206055170121,-1.95855316983527,
-26.7944730113718)) ;
#61796 = CARTESIAN_POINT('Ctrl Pts',(-16.1198350276745,-1.95079003648729,
-26.7930642660979)) ;
#61797 = CARTESIAN_POINT('Ctrl Pts',(-16.1194317942876,-1.94671197274391,
-26.7923233252232)) ;
#61798 = CARTESIAN_POINT('Ctrl Pts',(-16.1186114723841,-1.93836188167317,
-26.7908029991712)) ;
#61799 = CARTESIAN_POINT('Ctrl Pts',(-16.1181943211566,-1.93408985366662,
-26.790023651562)) ;
#61800 = CARTESIAN_POINT('Ctrl Pts',(-16.1175756613713,-1.92768207458426,
-26.7888504414553)) ;
#61801 = CARTESIAN_POINT('Ctrl Pts',(-16.1173706349253,-1.92554620531401,
-26.7884586670944)) ;
#61802 = CARTESIAN_POINT('Ctrl Pts',(-16.1169663635938,-1.9212988524359,-26.7876775211226)) ;
#61803 = CARTESIAN_POINT('Ctrl Pts',(-16.116767087912,-1.91918736837177,-26.7872881679312)) ;
#61804 = CARTESIAN_POINT('Ctrl Pts',(-16.1164757073549,-1.91605664477523,
-26.7867084094797)) ;
#61805 = CARTESIAN_POINT('Ctrl Pts',(-16.1163798463686,-1.91501915780667,
-26.7865158632312)) ;
#61806 = CARTESIAN_POINT('Ctrl Pts',(-16.1161914095241,-1.91295939154775,
-26.7861324619666)) ;
#61807 = CARTESIAN_POINT('Ctrl Pts',(-16.1160988314997,-1.91193711221481,
-26.7859416082438)) ;
#61808 = CARTESIAN_POINT('Ctrl Pts',(-16.1159180875877,-1.909910801112,-26.7855616470997)) ;
#61809 = CARTESIAN_POINT('Ctrl Pts',(-16.1158298882342,-1.90890677116962,
-26.785372560255)) ;
#61810 = CARTESIAN_POINT('Ctrl Pts',(-16.1157024897718,-1.90741670584362,
-26.7850898354139)) ;
#61811 = CARTESIAN_POINT('Ctrl Pts',(-16.1156608488991,-1.90692268117004,
-26.7849957396996)) ;
#61812 = CARTESIAN_POINT('Ctrl Pts',(-16.1155797830039,-1.90594034815389,
-26.7848075937183)) ;
#61813 = CARTESIAN_POINT('Ctrl Pts',(-16.1155403371682,-1.90545203916062,
-26.7847135558172)) ;
#61814 = CARTESIAN_POINT('Ctrl Pts',(-16.1154831306131,-1.90471721919977,
-26.7845707500099)) ;
#61815 = CARTESIAN_POINT('Ctrl Pts',(-16.1154631181873,-1.90445522508891,
-26.7845196026446)) ;
#61816 = CARTESIAN_POINT('Ctrl Pts',(-16.1154234811987,-1.90391896261954,
-26.7844141142082)) ;
#61817 = CARTESIAN_POINT('Ctrl Pts',(-16.1154038522064,-1.90364469407305,
-26.7843597757572)) ;
#61818 = CARTESIAN_POINT('Ctrl Pts',(-16.1153669532182,-1.9030964699622,-26.7842497549801)) ;
#61819 = CARTESIAN_POINT('Ctrl Pts',(-16.1153496049406,-1.9028225532317,-26.7841941291205)) ;
#61820 = CARTESIAN_POINT('Ctrl Pts',(-16.1153351246656,-1.90163369613048,
-26.783916109868)) ;
#61821 = CARTESIAN_POINT('Ctrl Pts',(-16.1153345317066,-1.90158501311153,
-26.7839047251385)) ;
#61822 = CARTESIAN_POINT('Ctrl Pts',(-16.1153339387476,-1.90153633009259,
-26.783893340409)) ;
#61823 = CARTESIAN_POINT('',(-3.68783779512238,-15.0366437072151,-33.7720311090634)) ;
#61824 = CARTESIAN_POINT('',(-3.65837019749682,-15.0366437072151,-33.7752359034359)) ;
#61825 = CARTESIAN_POINT('Origin',(0.147684368304155,-21.6462763158694,1.35793534153108)) ;
#61826 = CARTESIAN_POINT('',(-3.37961604955383,-1.90153624239224,-31.0750563097204)) ;
#61827 = CARTESIAN_POINT('Ctrl Pts',(-3.37961605183184,-1.90153633321405,
-31.0750563283525)) ;
#61828 = CARTESIAN_POINT('Ctrl Pts',(-3.37962354756522,-1.9015848895933,-31.0750656069308)) ;
#61829 = CARTESIAN_POINT('Ctrl Pts',(-3.37975139855505,-1.90241309156327,
-31.0752238670187)) ;
#61830 = CARTESIAN_POINT('Ctrl Pts',(-3.37978465679827,-1.90281047596646,
-31.0753028573227)) ;
#61831 = CARTESIAN_POINT('Ctrl Pts',(-3.37980438554198,-1.90308179329851,
-31.0753571125156)) ;
#61832 = CARTESIAN_POINT('Ctrl Pts',(-3.3798413566566,-1.90362481830771,-31.0754659744547)) ;
#61833 = CARTESIAN_POINT('Ctrl Pts',(-3.37985850315228,-1.90389648719278,
-31.075520583564)) ;
#61834 = CARTESIAN_POINT('Ctrl Pts',(-3.37989057697063,-1.90442766834731,
-31.075627516043)) ;
#61835 = CARTESIAN_POINT('Ctrl Pts',(-3.37990549913902,-1.90468718080719,
-31.0756798400127)) ;
#61836 = CARTESIAN_POINT('Ctrl Pts',(-3.37994610388543,-1.90541496999656,
-31.0758267151235)) ;
#61837 = CARTESIAN_POINT('Ctrl Pts',(-3.37997143437742,-1.90589858257301,
-31.0759244925368)) ;
#61838 = CARTESIAN_POINT('Ctrl Pts',(-3.38002041476513,-1.9068714680578,-31.0761214067959)) ;
#61839 = CARTESIAN_POINT('Ctrl Pts',(-3.38004404067381,-1.90736074161815,
-31.0762205463861)) ;
#61840 = CARTESIAN_POINT('Ctrl Pts',(-3.38011322017132,-1.9088364770218,-31.0765197951444)) ;
#61841 = CARTESIAN_POINT('Ctrl Pts',(-3.38015711441919,-1.90983085157814,
-31.0767217296534)) ;
#61842 = CARTESIAN_POINT('Ctrl Pts',(-3.38024253489509,-1.91183767688721,
-31.0771296138472)) ;
#61843 = CARTESIAN_POINT('Ctrl Pts',(-3.38028402232049,-1.91285012581093,
-31.0773355673717)) ;
#61844 = CARTESIAN_POINT('Ctrl Pts',(-3.38036541672939,-1.91489008539149,
-31.0777507773029)) ;
#61845 = CARTESIAN_POINT('Ctrl Pts',(-3.38040532114009,-1.91591759609217,
-31.0779600339982)) ;
#61846 = CARTESIAN_POINT('Ctrl Pts',(-3.38052330051655,-1.91901821585069,
-31.078591752673)) ;
#61847 = CARTESIAN_POINT('Ctrl Pts',(-3.38059968734525,-1.92110939731572,
-31.0790181550988)) ;
#61848 = CARTESIAN_POINT('Ctrl Pts',(-3.38074939599317,-1.92531591161341,
-31.0798763138211)) ;
#61849 = CARTESIAN_POINT('Ctrl Pts',(-3.38082268235303,-1.92743124490193,
-31.0803080740687)) ;
#61850 = CARTESIAN_POINT('Ctrl Pts',(-3.38103843251987,-1.93377741600093,
-31.0816038372784)) ;
#61851 = CARTESIAN_POINT('Ctrl Pts',(-3.3811768517012,-1.9380083719859,-31.0824683046859)) ;
#61852 = CARTESIAN_POINT('Ctrl Pts',(-3.38144167913154,-1.94627818587562,
-31.0841586128613)) ;
#61853 = CARTESIAN_POINT('Ctrl Pts',(-3.38156801504025,-1.95031704445984,
-31.084984461638)) ;
#61854 = CARTESIAN_POINT('Ctrl Pts',(-3.38180517498327,-1.95800520912717,
-31.0865568669311)) ;
#61855 = CARTESIAN_POINT('Ctrl Pts',(-3.3819222814648,-1.96185879110988,-31.0873452045946)) ;
#61856 = CARTESIAN_POINT('Ctrl Pts',(-3.38215453649361,-1.96958922519025,
-31.0889269301978)) ;
#61857 = CARTESIAN_POINT('Ctrl Pts',(-3.38226968324156,-1.97346607730139,
-31.0897203183359)) ;
#61858 = CARTESIAN_POINT('Ctrl Pts',(-3.38261296631772,-1.98513040932147,
-31.0921077385685)) ;
#61859 = CARTESIAN_POINT('Ctrl Pts',(-3.38283899223427,-1.99295166450382,
-31.0937090213102)) ;
#61860 = CARTESIAN_POINT('Ctrl Pts',(-3.38328779588863,-2.00867822988399,
-31.0969294132178)) ;
#61861 = CARTESIAN_POINT('Ctrl Pts',(-3.38351054522694,-2.01658353990714,
-31.0985485254358)) ;
#61862 = CARTESIAN_POINT('Ctrl Pts',(-3.38395399654487,-2.03247220787073,
-31.1018031969574)) ;
#61863 = CARTESIAN_POINT('Ctrl Pts',(-3.38417469770074,-2.04045556581573,
-31.1034387563511)) ;
#61864 = CARTESIAN_POINT('Ctrl Pts',(-3.38483479024306,-2.06451370586719,
-31.1083681177909)) ;
#61865 = CARTESIAN_POINT('Ctrl Pts',(-3.38527227156083,-2.08069655073069,
-31.1116845914063)) ;
#61866 = CARTESIAN_POINT('Ctrl Pts',(-3.3861448836398,-2.11330238314372,-31.1183677145852)) ;
#61867 = CARTESIAN_POINT('Ctrl Pts',(-3.38657996664064,-2.1297253708981,-31.1217343693854)) ;
#61868 = CARTESIAN_POINT('Ctrl Pts',(-3.38744869755865,-2.16276347024479,
-31.1285077733221)) ;
#61869 = CARTESIAN_POINT('Ctrl Pts',(-3.38788232782417,-2.17937857799855,
-31.1319145235804)) ;
#61870 = CARTESIAN_POINT('Ctrl Pts',(-3.38874828635231,-2.21275288640396,
-31.1387581193989)) ;
#61871 = CARTESIAN_POINT('Ctrl Pts',(-3.38918061235563,-2.22951208706357,
-31.1421949652061)) ;
#61872 = CARTESIAN_POINT('Ctrl Pts',(-3.39047522403265,-2.27993379582334,
-31.1525357165685)) ;
#61873 = CARTESIAN_POINT('Ctrl Pts',(-3.39133521532922,-2.31374041041457,
-31.159469828178)) ;
#61874 = CARTESIAN_POINT('Ctrl Pts',(-3.39304422259448,-2.38135375803524,
-31.1733392696568)) ;
#61875 = CARTESIAN_POINT('Ctrl Pts',(-3.39389319440513,-2.41516047740165,
-31.1802746014881)) ;
#61876 = CARTESIAN_POINT('Ctrl Pts',(-3.39557350849034,-2.4823898213473,-31.1940673377372)) ;
#61877 = CARTESIAN_POINT('Ctrl Pts',(-3.3964048330676,-2.51581244597206,-31.2009247440892)) ;
#61878 = CARTESIAN_POINT('Ctrl Pts',(-3.39886118328916,-2.6149279022379,-31.2212614930262)) ;
#61879 = CARTESIAN_POINT('Ctrl Pts',(-3.40044870012823,-2.67946831591532,
-31.2345053529434)) ;
#61880 = CARTESIAN_POINT('Ctrl Pts',(-3.40360177143294,-2.80821979403678,
-31.2609269969686)) ;
#61881 = CARTESIAN_POINT('Ctrl Pts',(-3.40524625729531,-2.87571441798806,
-31.2747787755693)) ;
#61882 = CARTESIAN_POINT('Ctrl Pts',(-3.40853282785513,-3.01111106389717,
-31.302567282874)) ;
#61883 = CARTESIAN_POINT('Ctrl Pts',(-3.41017487387755,-3.07901308592743,
-31.3165040157991)) ;
#61884 = CARTESIAN_POINT('Ctrl Pts',(-3.41345892963355,-3.21521138321956,
-31.3444594420512)) ;
#61885 = CARTESIAN_POINT('Ctrl Pts',(-3.41510092368816,-3.28350765846785,
-31.3584781370803)) ;
#61886 = CARTESIAN_POINT('Ctrl Pts',(-3.41838635957247,-3.42048131874613,
-31.3865945939094)) ;
#61887 = CARTESIAN_POINT('Ctrl Pts',(-3.42002979939743,-3.48915870377952,
-31.4006923559271)) ;
#61888 = CARTESIAN_POINT('Ctrl Pts',(-3.42496374500222,-3.69574280972321,
-31.4430999858881)) ;
#61889 = CARTESIAN_POINT('Ctrl Pts',(-3.42825798486587,-3.8342014808235,-31.4715241858609)) ;
#61890 = CARTESIAN_POINT('Ctrl Pts',(-3.43486056686863,-4.11248555386922,
-31.5286551649569)) ;
#61891 = CARTESIAN_POINT('Ctrl Pts',(-3.43816884992288,-4.25231095589393,
-31.5573619505224)) ;
#61892 = CARTESIAN_POINT('Ctrl Pts',(-3.44480102513381,-4.53322335765963,
-31.6150360820933)) ;
#61893 = CARTESIAN_POINT('Ctrl Pts',(-3.44812489090923,-4.67431035649286,
-31.6440034307791)) ;
#61894 = CARTESIAN_POINT('Ctrl Pts',(-3.45478843702903,-4.95764081678049,
-31.702176811003)) ;
#61895 = CARTESIAN_POINT('Ctrl Pts',(-3.458128104198,-5.09988427824991,-31.7313828439771)) ;
#61896 = CARTESIAN_POINT('Ctrl Pts',(-3.46482268996876,-5.38542253146676,
-31.7900117993526)) ;
#61897 = CARTESIAN_POINT('Ctrl Pts',(-3.46817760210812,-5.52871732321187,
-31.8194347224561)) ;
#61898 = CARTESIAN_POINT('Ctrl Pts',(-3.47490162628081,-5.81625310512141,
-31.8784757178839)) ;
#61899 = CARTESIAN_POINT('Ctrl Pts',(-3.47827073715131,-5.96049409528712,
-31.9080937903341)) ;
#61900 = CARTESIAN_POINT('Ctrl Pts',(-3.48839731486342,-6.3944786661344,-31.9972081732342)) ;
#61901 = CARTESIAN_POINT('Ctrl Pts',(-3.49517410239131,-6.68548384247647,
-32.0569646400372)) ;
#61902 = CARTESIAN_POINT('Ctrl Pts',(-3.50876576219942,-7.27001739496297,
-32.1769979486495)) ;
#61903 = CARTESIAN_POINT('Ctrl Pts',(-3.51558059633832,-7.56354577114107,
-32.2372747946138)) ;
#61904 = CARTESIAN_POINT('Ctrl Pts',(-3.52923293369486,-8.15228466666954,
-32.3581757011858)) ;
#61905 = CARTESIAN_POINT('Ctrl Pts',(-3.53607041801162,-8.44749518601661,
-32.4187997638484)) ;
#61906 = CARTESIAN_POINT('Ctrl Pts',(-3.54975155112279,-9.03875731206524,
-32.5402220620514)) ;
#61907 = CARTESIAN_POINT('Ctrl Pts',(-3.55659519106777,-9.33480891877373,
-32.6010202985551)) ;
#61908 = CARTESIAN_POINT('Ctrl Pts',(-3.57710956616611,-10.2229637870553,
-32.7834168174283)) ;
#61909 = CARTESIAN_POINT('Ctrl Pts',(-3.59076391219278,-10.8150670813697,
-32.9050168890259)) ;
#61910 = CARTESIAN_POINT('Ctrl Pts',(-3.61788642535806,-11.9925453014778,
-33.1468386026216)) ;
#61911 = CARTESIAN_POINT('Ctrl Pts',(-3.6313545159283,-12.5779202273231,-33.2670602529568)) ;
#61912 = CARTESIAN_POINT('Ctrl Pts',(-3.65795827616522,-13.7352132469821,
-33.5047423312816)) ;
#61913 = CARTESIAN_POINT('Ctrl Pts',(-3.67109390926027,-14.307131340793,-33.622202763248)) ;
#61914 = CARTESIAN_POINT('Ctrl Pts',(-3.68527448816673,-14.9249537986604,
-33.7490920441471)) ;
#61915 = CARTESIAN_POINT('Ctrl Pts',(-3.68655737279856,-14.9808505489368,
-33.7605722099422)) ;
#61916 = CARTESIAN_POINT('Ctrl Pts',(-3.68783779586363,-15.0366437072147,
-33.7720311089823)) ;
#61917 = CARTESIAN_POINT('Ctrl Pts',(-3.65837019675635,-15.0366437072147,
-33.775235903516)) ;
#61918 = CARTESIAN_POINT('Ctrl Pts',(-3.65715735966888,-14.9808505488501,
-33.7637696540398)) ;
#61919 = CARTESIAN_POINT('Ctrl Pts',(-3.65594235487438,-14.9249537984867,
-33.7522821058494)) ;
#61920 = CARTESIAN_POINT('Ctrl Pts',(-3.64251395514954,-14.3071313404433,
-33.625311020498)) ;
#61921 = CARTESIAN_POINT('Ctrl Pts',(-3.6300919636707,-13.7352132465421,-33.5077729753098)) ;
#61922 = CARTESIAN_POINT('Ctrl Pts',(-3.60497912176554,-12.5779202267003,
-33.2699287498069)) ;
#61923 = CARTESIAN_POINT('Ctrl Pts',(-3.59228823476317,-11.9925453007625,
-33.1496225734707)) ;
#61924 = CARTESIAN_POINT('Ctrl Pts',(-3.56679211841482,-10.8150670804683,
-32.9076239785231)) ;
#61925 = CARTESIAN_POINT('Ctrl Pts',(-3.55398681249849,-10.2229637860605,
-32.7859315682295)) ;
#61926 = CARTESIAN_POINT('Ctrl Pts',(-3.53481171294889,-9.33480891763853,
-32.6033893943336)) ;
#61927 = CARTESIAN_POINT('Ctrl Pts',(-3.52842552872936,-9.03875731088329,
-32.5425414065118)) ;
#61928 = CARTESIAN_POINT('Ctrl Pts',(-3.5156845996532,-8.44749518474126,-32.4210168549385)) ;
#61929 = CARTESIAN_POINT('Ctrl Pts',(-3.5093298459469,-8.15228466534754,-32.3603402921485)) ;
#61930 = CARTESIAN_POINT('Ctrl Pts',(-3.49667287813304,-7.56354576972608,
-32.2393311325957)) ;
#61931 = CARTESIAN_POINT('Ctrl Pts',(-3.49037064512079,-7.27001739350161,
-32.1789985378896)) ;
#61932 = CARTESIAN_POINT('Ctrl Pts',(-3.47784092628131,-6.68548384092276,
-32.0588497362179)) ;
#61933 = CARTESIAN_POINT('Ctrl Pts',(-3.47161340231218,-6.39447866453474,
-31.9990335333934)) ;
#61934 = CARTESIAN_POINT('Ctrl Pts',(-3.46234626814233,-5.96049409361887,
-31.9098256803611)) ;
#61935 = CARTESIAN_POINT('Ctrl Pts',(-3.45926960099435,-5.81625310343037,
-31.8801758027346)) ;
#61936 = CARTESIAN_POINT('Ctrl Pts',(-3.45314435244001,-5.52871732147542,
-31.8210696865245)) ;
#61937 = CARTESIAN_POINT('Ctrl Pts',(-3.45009576986793,-5.38542252970768,
-31.7916134480681)) ;
#61938 = CARTESIAN_POINT('Ctrl Pts',(-3.44403034759674,-5.09988427644571,
-31.7329160670292)) ;
#61939 = CARTESIAN_POINT('Ctrl Pts',(-3.44101350143869,-4.95764081495384,
-31.7036749251497)) ;
#61940 = CARTESIAN_POINT('Ctrl Pts',(-3.435015700397,-4.67431035462144,-31.645429140776)) ;
#61941 = CARTESIAN_POINT('Ctrl Pts',(-3.43203473233864,-4.53322335576592,
-31.6164244997114)) ;
#61942 = CARTESIAN_POINT('Ctrl Pts',(-3.42611361752552,-4.25231095395583,
-31.5586730356528)) ;
#61943 = CARTESIAN_POINT('Ctrl Pts',(-3.42317344443355,-4.11248555190906,
-31.5299262157117)) ;
#61944 = CARTESIAN_POINT('Ctrl Pts',(-3.41734019001161,-3.83420147881938,
-31.4727115671899)) ;
#61945 = CARTESIAN_POINT('Ctrl Pts',(-3.41444704959424,-3.69574280769723,
-31.444243745019)) ;
#61946 = CARTESIAN_POINT('Ctrl Pts',(-3.41014925541112,-3.48915870172089,
-31.4017669294148)) ;
#61947 = CARTESIAN_POINT('Ctrl Pts',(-3.40872367042118,-3.42048131667665,
-31.3876454742537)) ;
#61948 = CARTESIAN_POINT('Ctrl Pts',(-3.40588808753802,-3.28350765637674,
-31.3594800929579)) ;
#61949 = CARTESIAN_POINT('Ctrl Pts',(-3.40447808762632,-3.21521138111763,
-31.345436167043)) ;
#61950 = CARTESIAN_POINT('Ctrl Pts',(-3.40167577369564,-3.07901308380399,
-31.3174283482056)) ;
#61951 = CARTESIAN_POINT('Ctrl Pts',(-3.40028344398735,-3.011111061763,-31.3034644569924)) ;
#61952 = CARTESIAN_POINT('Ctrl Pts',(-3.39751946870557,-2.8757144158325,-31.2756191140218)) ;
#61953 = CARTESIAN_POINT('Ctrl Pts',(-3.39614778446167,-2.80821979187057,
-31.2617376664548)) ;
#61954 = CARTESIAN_POINT('Ctrl Pts',(-3.39354726626481,-2.67946831377512,
-31.2352559286632)) ;
#61955 = CARTESIAN_POINT('Ctrl Pts',(-3.39225062944861,-2.61492790013619,
-31.2219804336451)) ;
#61956 = CARTESIAN_POINT('Ctrl Pts',(-3.39027775169719,-2.51581244392945,
-31.2015911039206)) ;
#61957 = CARTESIAN_POINT('Ctrl Pts',(-3.38961550070132,-2.48238981932461,
-31.1947153097126)) ;
#61958 = CARTESIAN_POINT('Ctrl Pts',(-3.38829149939526,-2.41516047541903,
-31.1808838221218)) ;
#61959 = CARTESIAN_POINT('Ctrl Pts',(-3.38762973137363,-2.38135375607278,
-31.1739281306557)) ;
#61960 = CARTESIAN_POINT('Ctrl Pts',(-3.38631726306021,-2.31374040849244,
-31.1600155629754)) ;
#61961 = CARTESIAN_POINT('Ctrl Pts',(-3.38566651923091,-2.27993379392141,
-31.1530586943365)) ;
#61962 = CARTESIAN_POINT('Ctrl Pts',(-3.38470790773418,-2.22951208519171,
-31.1426814007587)) ;
#61963 = CARTESIAN_POINT('Ctrl Pts',(-3.38439130594481,-2.21275288454212,
-31.1392319691868)) ;
#61964 = CARTESIAN_POINT('Ctrl Pts',(-3.38376584803932,-2.17937857615662,
-31.1323622173535)) ;
#61965 = CARTESIAN_POINT('Ctrl Pts',(-3.38345698967685,-2.16276346841279,
-31.1289418973351)) ;
#61966 = CARTESIAN_POINT('Ctrl Pts',(-3.38284932852388,-2.12972536908577,
-31.1221401003545)) ;
#61967 = CARTESIAN_POINT('Ctrl Pts',(-3.38255050824406,-2.11330238134113,
-31.1187586260923)) ;
#61968 = CARTESIAN_POINT('Ctrl Pts',(-3.38196604520614,-2.08069654894753,
-31.1120441648207)) ;
#61969 = CARTESIAN_POINT('Ctrl Pts',(-3.38168035465867,-2.06451370409367,
-31.1087111829663)) ;
#61970 = CARTESIAN_POINT('Ctrl Pts',(-3.38126534760574,-2.04045556405656,
-31.1037551668761)) ;
#61971 = CARTESIAN_POINT('Ctrl Pts',(-3.38112929197016,-2.03247220611634,
-31.1021104017283)) ;
#61972 = CARTESIAN_POINT('Ctrl Pts',(-3.38086271747385,-2.01658353816223,
-31.098836493695)) ;
#61973 = CARTESIAN_POINT('Ctrl Pts',(-3.38073219780292,-2.00867822814386,
-31.0972073508972)) ;
#61974 = CARTESIAN_POINT('Ctrl Pts',(-3.38047821961298,-1.99295166277309,
-31.0939657704455)) ;
#61975 = CARTESIAN_POINT('Ctrl Pts',(-3.38035473270136,-1.98513040759533,
-31.0923533359159)) ;
#61976 = CARTESIAN_POINT('Ctrl Pts',(-3.38017676523144,-1.97346607558221,
-31.0899479365291)) ;
#61977 = CARTESIAN_POINT('Ctrl Pts',(-3.38011866495113,-1.96958922347363,
-31.0891483442143)) ;
#61978 = CARTESIAN_POINT('Ctrl Pts',(-3.38000546573751,-1.96185878939789,
-31.0875536705118)) ;
#61979 = CARTESIAN_POINT('Ctrl Pts',(-3.37995036499538,-1.95800520741715,
-31.0867585893183)) ;
#61980 = CARTESIAN_POINT('Ctrl Pts',(-3.37984395961066,-1.9503170426067,-31.0851719635802)) ;
#61981 = CARTESIAN_POINT('Ctrl Pts',(-3.37978980878068,-1.94627818386982,
-31.0843382641714)) ;
#61982 = CARTESIAN_POINT('Ctrl Pts',(-3.37968507839923,-1.93800836966755,
-31.0826305443277)) ;
#61983 = CARTESIAN_POINT('Ctrl Pts',(-3.37963442649015,-1.93377741352282,
-31.0817565316209)) ;
#61984 = CARTESIAN_POINT('Ctrl Pts',(-3.37956658174528,-1.9274312421839,-31.0804446826773)) ;
#61985 = CARTESIAN_POINT('Ctrl Pts',(-3.37954533904407,-1.9253159088158,-31.0800072623241)) ;
#61986 = CARTESIAN_POINT('Ctrl Pts',(-3.37950706883426,-1.9211093943593,-31.0791369839084)) ;
#61987 = CARTESIAN_POINT('Ctrl Pts',(-3.37949000588967,-1.91901821281563,
-31.078704129605)) ;
#61988 = CARTESIAN_POINT('Ctrl Pts',(-3.37946942613243,-1.91591759293996,
-31.0780618180589)) ;
#61989 = CARTESIAN_POINT('Ctrl Pts',(-3.3794634135807,-1.91489008220023,-31.0778488753936)) ;
#61990 = CARTESIAN_POINT('Ctrl Pts',(-3.37945364718064,-1.91285012254287,
-31.0774258754311)) ;
#61991 = CARTESIAN_POINT('Ctrl Pts',(-3.37944989077964,-1.91183767358176,
-31.0772158184026)) ;
#61992 = CARTESIAN_POINT('Ctrl Pts',(-3.37944563114251,-1.90983084819726,
-31.07679910742)) ;
#61993 = CARTESIAN_POINT('Ctrl Pts',(-3.37944508902013,-1.90883647359888,
-31.0765924580745)) ;
#61994 = CARTESIAN_POINT('Ctrl Pts',(-3.3794483215085,-1.9073607381399,-31.0762853340266)) ;
#61995 = CARTESIAN_POINT('Ctrl Pts',(-3.37945008313227,-1.90687146456539,
-31.0761834333729)) ;
#61996 = CARTESIAN_POINT('Ctrl Pts',(-3.37945558765507,-1.9058985790443,-31.0759805935151)) ;
#61997 = CARTESIAN_POINT('Ctrl Pts',(-3.37945930654473,-1.90541496644589,
-31.0758796567867)) ;
#61998 = CARTESIAN_POINT('Ctrl Pts',(-3.37946738816771,-1.9046871772366,-31.07572748671)) ;
#61999 = CARTESIAN_POINT('Ctrl Pts',(-3.3794707135693,-1.90442766478295,-31.0756731781987)) ;
#62000 = CARTESIAN_POINT('Ctrl Pts',(-3.37947905021081,-1.90389648362564,
-31.0755618508168)) ;
#62001 = CARTESIAN_POINT('Ctrl Pts',(-3.37948405653174,-1.90362481474057,
-31.0755048324435)) ;
#62002 = CARTESIAN_POINT('Ctrl Pts',(-3.37949676121262,-1.90308178972856,
-31.0753905679354)) ;
#62003 = CARTESIAN_POINT('Ctrl Pts',(-3.37950436512425,-1.90281047237712,
-31.0753333401331)) ;
#62004 = CARTESIAN_POINT('Ctrl Pts',(-3.37960751752133,-1.9016336939429,-31.0750774956391)) ;
#62005 = CARTESIAN_POINT('Ctrl Pts',(-3.37961178467659,-1.90158501357847,
-31.0750669119958)) ;
#62006 = CARTESIAN_POINT('Ctrl Pts',(-3.37961605183184,-1.90153633321405,
-31.0750563283525)) ;
#62007 = CARTESIAN_POINT('',(-10.8616065908228,-15.0366437072153,-32.189683675067)) ;
#62008 = CARTESIAN_POINT('',(-10.8335168660197,-15.0366437072153,-32.1991482053229)) ;
#62009 = CARTESIAN_POINT('Origin',(0.436147547989918,-21.6462763158694,1.2944397941978)) ;
#62010 = CARTESIAN_POINT('',(-9.98082103895569,-1.90153624240863,-29.6220212119843)) ;
#62011 = CARTESIAN_POINT('Ctrl Pts',(-9.98082104518866,-1.90153633324684,
-29.6220212296937)) ;
#62012 = CARTESIAN_POINT('Ctrl Pts',(-9.98083034329157,-1.90158489192866,
-29.6220286862145)) ;
#62013 = CARTESIAN_POINT('Ctrl Pts',(-9.98098989087541,-1.90241811784944,
-29.6221566338067)) ;
#62014 = CARTESIAN_POINT('Ctrl Pts',(-9.98103957355631,-1.90281781834771,
-29.6222270582998)) ;
#62015 = CARTESIAN_POINT('Ctrl Pts',(-9.98107064674613,-1.9030907157319,-29.6222761005186)) ;
#62016 = CARTESIAN_POINT('Ctrl Pts',(-9.9811304334122,-1.90363690104155,-29.6223750652033)) ;
#62017 = CARTESIAN_POINT('Ctrl Pts',(-9.98115905341219,-1.90391015014683,
-29.6224250106994)) ;
#62018 = CARTESIAN_POINT('Ctrl Pts',(-9.98121362464133,-1.90444442000563,
-29.622523134212)) ;
#62019 = CARTESIAN_POINT('Ctrl Pts',(-9.98123957102262,-1.9047054409468,-29.6225713139028)) ;
#62020 = CARTESIAN_POINT('Ctrl Pts',(-9.98131115116327,-1.90543750368787,
-29.6227068400549)) ;
#62021 = CARTESIAN_POINT('Ctrl Pts',(-9.98135713841576,-1.90592397086527,
-29.622797431294)) ;
#62022 = CARTESIAN_POINT('Ctrl Pts',(-9.98144776083572,-1.90690259879769,
-29.6229803109675)) ;
#62023 = CARTESIAN_POINT('Ctrl Pts',(-9.98149237318018,-1.9073947602025,-29.6230726072336)) ;
#62024 = CARTESIAN_POINT('Ctrl Pts',(-9.98162494237531,-1.90887920569416,
-29.6233516593688)) ;
#62025 = CARTESIAN_POINT('Ctrl Pts',(-9.98171166876545,-1.90987944903977,
-29.6235405655408)) ;
#62026 = CARTESIAN_POINT('Ctrl Pts',(-9.98188367149003,-1.91189811830544,
-29.6239228316236)) ;
#62027 = CARTESIAN_POINT('Ctrl Pts',(-9.98196891051252,-1.91291654239933,
-29.6241162037079)) ;
#62028 = CARTESIAN_POINT('Ctrl Pts',(-9.98213855534324,-1.91496854097824,
-29.6245065325352)) ;
#62029 = CARTESIAN_POINT('Ctrl Pts',(-9.98222295877125,-1.91600211550575,
-29.6247034900893)) ;
#62030 = CARTESIAN_POINT('Ctrl Pts',(-9.98247532544751,-1.91912103313602,
-29.6252986146565)) ;
#62031 = CARTESIAN_POINT('Ctrl Pts',(-9.9826424881391,-1.92122455503296,-29.6257010157422)) ;
#62032 = CARTESIAN_POINT('Ctrl Pts',(-9.98297497037919,-1.92545589204945,
-29.6265117366763)) ;
#62033 = CARTESIAN_POINT('Ctrl Pts',(-9.98314025600325,-1.92758370762544,
-29.6269200680547)) ;
#62034 = CARTESIAN_POINT('Ctrl Pts',(-9.98363219204553,-1.93396732561015,
-29.628146420618)) ;
#62035 = CARTESIAN_POINT('Ctrl Pts',(-9.98395498088245,-1.93822324620528,
-29.6289657686947)) ;
#62036 = CARTESIAN_POINT('Ctrl Pts',(-9.98458042813596,-1.94654185458999,
-29.6305691084042)) ;
#62037 = CARTESIAN_POINT('Ctrl Pts',(-9.98488301743629,-1.95060454305893,
-29.6313531234732)) ;
#62038 = CARTESIAN_POINT('Ctrl Pts',(-9.98545584580792,-1.9583382748244,-29.6328466457974)) ;
#62039 = CARTESIAN_POINT('Ctrl Pts',(-9.98574128637346,-1.96221480024253,
-29.6335958415099)) ;
#62040 = CARTESIAN_POINT('Ctrl Pts',(-9.98631134298126,-1.9699912596771,-29.6350996155706)) ;
#62041 = CARTESIAN_POINT('Ctrl Pts',(-9.98659595732225,-1.97389119370685,
-29.6358541944948)) ;
#62042 = CARTESIAN_POINT('Ctrl Pts',(-9.98744925814862,-1.9856249725075,-29.6381255234136)) ;
#62043 = CARTESIAN_POINT('Ctrl Pts',(-9.98801744723912,-1.99349279357557,
-29.6396498503683)) ;
#62044 = CARTESIAN_POINT('Ctrl Pts',(-9.9891545036605,-2.00931299105223,-29.6427167151263)) ;
#62045 = CARTESIAN_POINT('Ctrl Pts',(-9.98972334382125,-2.01726536728617,
-29.6442592620461)) ;
#62046 = CARTESIAN_POINT('Ctrl Pts',(-9.99086258006404,-2.03324863225896,
-29.6473609532205)) ;
#62047 = CARTESIAN_POINT('Ctrl Pts',(-9.99143297537365,-2.04127952100227,
-29.6489200977357)) ;
#62048 = CARTESIAN_POINT('Ctrl Pts',(-9.99314710341874,-2.06548089672393,
-29.6536202467501)) ;
#62049 = CARTESIAN_POINT('Ctrl Pts',(-9.99429387455137,-2.08176008973396,
-29.6567839335205)) ;
#62050 = CARTESIAN_POINT('Ctrl Pts',(-9.9965959799775,-2.11456004793966,-29.6631611025615)) ;
#62051 = CARTESIAN_POINT('Ctrl Pts',(-9.99775126858592,-2.13108081334029,
-29.6663746002696)) ;
#62052 = CARTESIAN_POINT('Ctrl Pts',(-10.000069122618,-2.16431561158016,-29.6728412905659)) ;
#62053 = CARTESIAN_POINT('Ctrl Pts',(-10.001231671007,-2.18102964058034,-29.6760944880565)) ;
#62054 = CARTESIAN_POINT('Ctrl Pts',(-10.0035620095714,-2.21460264917897,
-29.6826307269224)) ;
#62055 = CARTESIAN_POINT('Ctrl Pts',(-10.0047297976087,-2.23146162878534,
-29.6859137690194)) ;
#62056 = CARTESIAN_POINT('Ctrl Pts',(-10.0082373866525,-2.28218353208635,
-29.6957930848408)) ;
#62057 = CARTESIAN_POINT('Ctrl Pts',(-10.0105814813601,-2.31619141997308,
-29.7024195248609)) ;
#62058 = CARTESIAN_POINT('Ctrl Pts',(-10.0152591829867,-2.38420731419178,
-29.7156759644786)) ;
#62059 = CARTESIAN_POINT('Ctrl Pts',(-10.0175927470763,-2.4182153068596,-29.7223059755272)) ;
#62060 = CARTESIAN_POINT('Ctrl Pts',(-10.0222257294052,-2.48584491021547,
-29.7354932425945)) ;
#62061 = CARTESIAN_POINT('Ctrl Pts',(-10.0245251307189,-2.51946652094906,
-29.7420505043261)) ;
#62062 = CARTESIAN_POINT('Ctrl Pts',(-10.0313354853966,-2.61917207395672,
-29.7614990800057)) ;
#62063 = CARTESIAN_POINT('Ctrl Pts',(-10.0357586991564,-2.68409673668246,
-29.7741671474126)) ;
#62064 = CARTESIAN_POINT('Ctrl Pts',(-10.0445719574544,-2.81365376993385,
-29.7994507167258)) ;
#62065 = CARTESIAN_POINT('Ctrl Pts',(-10.0491852821836,-2.8815893713073,-29.8127113376134)) ;
#62066 = CARTESIAN_POINT('Ctrl Pts',(-10.0584279811638,-3.01787063373489,
-29.8393165952872)) ;
#62067 = CARTESIAN_POINT('Ctrl Pts',(-10.0630573183518,-3.08621629486166,
-29.8526612445772)) ;
#62068 = CARTESIAN_POINT('Ctrl Pts',(-10.0723337144261,-3.22330444615647,
-29.8794311103673)) ;
#62069 = CARTESIAN_POINT('Ctrl Pts',(-10.0769807582795,-3.29204693631097,
-29.8928563319293)) ;
#62070 = CARTESIAN_POINT('Ctrl Pts',(-10.0862933964167,-3.42991551634899,
-29.9197841780547)) ;
#62071 = CARTESIAN_POINT('Ctrl Pts',(-10.0909589887703,-3.49904160623596,
-29.9332868032681)) ;
#62072 = CARTESIAN_POINT('Ctrl Pts',(-10.104984095758,-3.70697543286987,-29.9739062863256)) ;
#62073 = CARTESIAN_POINT('Ctrl Pts',(-10.114372043631,-3.84633872593528,-30.0011347166327)) ;
#62074 = CARTESIAN_POINT('Ctrl Pts',(-10.133222992924,-4.1264409723699,-30.0558662853713)) ;
#62075 = CARTESIAN_POINT('Ctrl Pts',(-10.1426859377833,-4.26717992581852,
-30.0833694428775)) ;
#62076 = CARTESIAN_POINT('Ctrl Pts',(-10.1616835878252,-4.54992767301016,
-30.1386284989711)) ;
#62077 = CARTESIAN_POINT('Ctrl Pts',(-10.1712182677189,-4.69193646584414,
-30.1663844058811)) ;
#62078 = CARTESIAN_POINT('Ctrl Pts',(-10.1903548491206,-4.97711806982726,
-30.2221274129627)) ;
#62079 = CARTESIAN_POINT('Ctrl Pts',(-10.1999567380201,-5.12029088099143,
-30.2501145173859)) ;
#62080 = CARTESIAN_POINT('Ctrl Pts',(-10.219222463357,-5.40769470241093,-30.3062986200493)) ;
#62081 = CARTESIAN_POINT('Ctrl Pts',(-10.2288862936133,-5.55192571266397,
-30.3344956203714)) ;
#62082 = CARTESIAN_POINT('Ctrl Pts',(-10.2482701602761,-5.84134011352206,
-30.3910783729501)) ;
#62083 = CARTESIAN_POINT('Ctrl Pts',(-10.2579901955671,-5.98652350412846,
-30.419464125582)) ;
#62084 = CARTESIAN_POINT('Ctrl Pts',(-10.2872255418426,-6.4233435188767,-30.5048729525588)) ;
#62085 = CARTESIAN_POINT('Ctrl Pts',(-10.3068161653109,-6.71624998125329,
-30.5621475706734)) ;
#62086 = CARTESIAN_POINT('Ctrl Pts',(-10.3461475069765,-7.30460259096212,
-30.6772000749509)) ;
#62087 = CARTESIAN_POINT('Ctrl Pts',(-10.3658881886828,-7.60004873832798,
-30.7349779734165)) ;
#62088 = CARTESIAN_POINT('Ctrl Pts',(-10.4054670152996,-8.1926341663384,-30.8508701605798)) ;
#62089 = CARTESIAN_POINT('Ctrl Pts',(-10.4253051421279,-8.48977344697968,
-30.9089844553695)) ;
#62090 = CARTESIAN_POINT('Ctrl Pts',(-10.4650251857872,-9.08489859067703,
-31.0253829085238)) ;
#62091 = CARTESIAN_POINT('Ctrl Pts',(-10.484907094154,-9.38288445374,-31.0836670697413)) ;
#62092 = CARTESIAN_POINT('Ctrl Pts',(-10.5445370048436,-10.2768420911068,
-31.2585248923988)) ;
#62093 = CARTESIAN_POINT('Ctrl Pts',(-10.584269340941,-10.8728138981643,-31.3751038395442)) ;
#62094 = CARTESIAN_POINT('Ctrl Pts',(-10.6632528657959,-12.0579851834207,
-31.6069469781574)) ;
#62095 = CARTESIAN_POINT('Ctrl Pts',(-10.7025039813133,-12.6471846616712,
-31.7222111943129)) ;
#62096 = CARTESIAN_POINT('Ctrl Pts',(-10.7800820901393,-13.8120388654271,
-31.9500972327384)) ;
#62097 = CARTESIAN_POINT('Ctrl Pts',(-10.8202961136303,-14.4160365127297,
-32.0682641126275)) ;
#62098 = CARTESIAN_POINT('Ctrl Pts',(-10.8597565733816,-15.0088506100736,
-32.1842460492104)) ;
#62099 = CARTESIAN_POINT('Ctrl Pts',(-10.861606591113,-15.0366437072151,-32.189683674969)) ;
#62100 = CARTESIAN_POINT('Ctrl Pts',(-10.8335168657278,-15.0366437072152,
-32.1991482054211)) ;
#62101 = CARTESIAN_POINT('Ctrl Pts',(-10.8316989411165,-15.0088506101081,
-32.1936997662387)) ;
#62102 = CARTESIAN_POINT('Ctrl Pts',(-10.829879399171,-14.9810324825753,-32.188246413499)) ;
#62103 = CARTESIAN_POINT('Ctrl Pts',(-10.7910704227901,-14.3876935910683,
-32.0719305223189)) ;
#62104 = CARTESIAN_POINT('Ctrl Pts',(-10.7534264184998,-13.8120388656015,
-31.9590785742631)) ;
#62105 = CARTESIAN_POINT('Ctrl Pts',(-10.6772750585336,-12.647184661918,-31.7307118081906)) ;
#62106 = CARTESIAN_POINT('Ctrl Pts',(-10.6387676678708,-12.0579851837042,
-31.6151970019631)) ;
#62107 = CARTESIAN_POINT('Ctrl Pts',(-10.5613404148593,-10.8728138985215,
-31.3828294943288)) ;
#62108 = CARTESIAN_POINT('Ctrl Pts',(-10.5224204792644,-10.2768420915011,
-31.2659768175915)) ;
#62109 = CARTESIAN_POINT('Ctrl Pts',(-10.4640719920794,-9.38288445418984,
-31.0906872330967)) ;
#62110 = CARTESIAN_POINT('Ctrl Pts',(-10.4446277699413,-9.08489859114541,
-31.0322555982222)) ;
#62111 = CARTESIAN_POINT('Ctrl Pts',(-10.405807278733,-8.48977344748511,-30.9155540505654)) ;
#62112 = CARTESIAN_POINT('Ctrl Pts',(-10.3864310011991,-8.19263416686229,
-30.857284140634)) ;
#62113 = CARTESIAN_POINT('Ctrl Pts',(-10.3478044672062,-7.6000487388887,-30.7410710887349)) ;
#62114 = CARTESIAN_POINT('Ctrl Pts',(-10.3285541926651,-7.30460259154122,
-30.6831279528606)) ;
#62115 = CARTESIAN_POINT('Ctrl Pts',(-10.2902387920502,-6.716249981869,-30.5677331381953)) ;
#62116 = CARTESIAN_POINT('Ctrl Pts',(-10.2711736294812,-6.42334351951061,
-30.5102814716937)) ;
#62117 = CARTESIAN_POINT('Ctrl Pts',(-10.2427604660902,-5.98652350478954,
-30.4245956190545)) ;
#62118 = CARTESIAN_POINT('Ctrl Pts',(-10.2333201932118,-5.84134011419217,
-30.3961156034926)) ;
#62119 = CARTESIAN_POINT('Ctrl Pts',(-10.2145091321644,-5.55192571335207,
-30.3393398502347)) ;
#62120 = CARTESIAN_POINT('Ctrl Pts',(-10.2051383428801,-5.40769470310801,
-30.3110441129149)) ;
#62121 = CARTESIAN_POINT('Ctrl Pts',(-10.1864744829921,-5.12029088170639,
-30.2546572181743)) ;
#62122 = CARTESIAN_POINT('Ctrl Pts',(-10.1771814062092,-4.97711807055114,
-30.2265660628362)) ;
#62123 = CARTESIAN_POINT('Ctrl Pts',(-10.1586816754023,-4.69193646658576,
-30.1706084758092)) ;
#62124 = CARTESIAN_POINT('Ctrl Pts',(-10.1494750087662,-4.54992767376058,
-30.1427420483666)) ;
#62125 = CARTESIAN_POINT('Ctrl Pts',(-10.1311575503266,-4.26717992658653,
-30.0872538090418)) ;
#62126 = CARTESIAN_POINT('Ctrl Pts',(-10.1220467333525,-4.12644097314668,
-30.0596320058389)) ;
#62127 = CARTESIAN_POINT('Ctrl Pts',(-10.1039317092101,-3.84633872672947,
-30.0046524750503)) ;
#62128 = CARTESIAN_POINT('Ctrl Pts',(-10.0949274454705,-3.70697543367274,
-29.9772947665084)) ;
#62129 = CARTESIAN_POINT('Ctrl Pts',(-10.0815108721089,-3.49904160705175,
-29.9364702446021)) ;
#62130 = CARTESIAN_POINT('Ctrl Pts',(-10.0770536772167,-3.42991551716911,
-29.9228974021094)) ;
#62131 = CARTESIAN_POINT('Ctrl Pts',(-10.0681713657158,-3.29204693713965,
-29.8958245620603)) ;
#62132 = CARTESIAN_POINT('Ctrl Pts',(-10.0637462471753,-3.22330444698941,
-29.8823245651551)) ;
#62133 = CARTESIAN_POINT('Ctrl Pts',(-10.0549306892449,-3.08621629570312,
-29.8553994249173)) ;
#62134 = CARTESIAN_POINT('Ctrl Pts',(-10.0505402348198,-3.01787063458062,
-29.8419742866539)) ;
#62135 = CARTESIAN_POINT('Ctrl Pts',(-10.0417974674542,-2.88158937216149,
-29.8152005824085)) ;
#62136 = CARTESIAN_POINT('Ctrl Pts',(-10.0374451174447,-2.81365377079228,
-29.8018520289007)) ;
#62137 = CARTESIAN_POINT('Ctrl Pts',(-10.0291603270341,-2.6840967373633,-29.7763903979855)) ;
#62138 = CARTESIAN_POINT('Ctrl Pts',(-10.0250152290655,-2.61917207444665,
-29.7636286224163)) ;
#62139 = CARTESIAN_POINT('Ctrl Pts',(-10.0186671286565,-2.51946652114585,
-29.7440242950753)) ;
#62140 = CARTESIAN_POINT('Ctrl Pts',(-10.0165293803719,-2.48584491031341,
-29.737412566075)) ;
#62141 = CARTESIAN_POINT('Ctrl Pts',(-10.0122370714667,-2.41821530675869,
-29.7241105127231)) ;
#62142 = CARTESIAN_POINT('Ctrl Pts',(-10.0100824939169,-2.38420731399091,
-29.7174201940658)) ;
#62143 = CARTESIAN_POINT('Ctrl Pts',(-10.0057839242904,-2.31619141957223,
-29.7040360099601)) ;
#62144 = CARTESIAN_POINT('Ctrl Pts',(-10.0036398911843,-2.2821835315855,-29.6973421613161)) ;
#62145 = CARTESIAN_POINT('Ctrl Pts',(-10.0004535512912,-2.23146162813537,
-29.6873546040206)) ;
#62146 = CARTESIAN_POINT('Ctrl Pts',(-9.9993964068386,-2.21460264847951,-29.6840342817486)) ;
#62147 = CARTESIAN_POINT('Ctrl Pts',(-9.99729600997807,-2.18102963978215,
-29.6774205664804)) ;
#62148 = CARTESIAN_POINT('Ctrl Pts',(-9.99625275543195,-2.16431561073278,
-29.6741271742035)) ;
#62149 = CARTESIAN_POINT('Ctrl Pts',(-9.99418450872342,-2.1310808123952,-29.6675763813864)) ;
#62150 = CARTESIAN_POINT('Ctrl Pts',(-9.99315950002149,-2.11456004694601,
-29.6643189872563)) ;
#62151 = CARTESIAN_POINT('Ctrl Pts',(-9.9911328919117,-2.08176008864388,-29.6578489923406)) ;
#62152 = CARTESIAN_POINT('Ctrl Pts',(-9.99013124680192,-2.06548089558601,
-29.6546364069092)) ;
#62153 = CARTESIAN_POINT('Ctrl Pts',(-9.98865144325748,-2.0412795197932,-29.6498573047625)) ;
#62154 = CARTESIAN_POINT('Ctrl Pts',(-9.9881619769522,-2.03324863102629,-29.6482708920856)) ;
#62155 = CARTESIAN_POINT('Ctrl Pts',(-9.98719185150007,-2.0172653660065,-29.6451122208414)) ;
#62156 = CARTESIAN_POINT('Ctrl Pts',(-9.98671119156714,-2.00931298974907,
-29.6435399625384)) ;
#62157 = CARTESIAN_POINT('Ctrl Pts',(-9.98576040682444,-1.99349279222591,
-29.6404103355341)) ;
#62158 = CARTESIAN_POINT('Ctrl Pts',(-9.98529025485661,-1.98562497113475,
-29.6388529760218)) ;
#62159 = CARTESIAN_POINT('Ctrl Pts',(-9.98459501202897,-1.97389119229962,
-29.636528391155)) ;
#62160 = CARTESIAN_POINT('Ctrl Pts',(-9.98436493981971,-1.96999125825837,
-29.6357554348444)) ;
#62161 = CARTESIAN_POINT('Ctrl Pts',(-9.98390871264385,-1.96221479880093,
-29.6342133071775)) ;
#62162 = CARTESIAN_POINT('Ctrl Pts',(-9.983682555973,-1.95833827337143,-29.6334441363927)) ;
#62163 = CARTESIAN_POINT('Ctrl Pts',(-9.98323473947911,-1.95060454181405,
-29.6319084927081)) ;
#62164 = CARTESIAN_POINT('Ctrl Pts',(-9.98300116306043,-1.9465418535758,-29.6311012245421)) ;
#62165 = CARTESIAN_POINT('Ctrl Pts',(-9.98252877745729,-1.93822324566284,
-29.6294463124608)) ;
#62166 = CARTESIAN_POINT('Ctrl Pts',(-9.98228989910769,-1.93396732530918,
-29.6285986917018)) ;
#62167 = CARTESIAN_POINT('Ctrl Pts',(-9.98193936904879,-1.92758370768641,
-29.6273246939941)) ;
#62168 = CARTESIAN_POINT('Ctrl Pts',(-9.98182384014075,-1.92545589223065,
-29.6268995976523)) ;
#62169 = CARTESIAN_POINT('Ctrl Pts',(-9.98159789955204,-1.92122455545407,
-29.6260529787085)) ;
#62170 = CARTESIAN_POINT('Ctrl Pts',(-9.98148745389595,-1.91912103367696,
-29.6256314674547)) ;
#62171 = CARTESIAN_POINT('Ctrl Pts',(-9.98132820722381,-1.91600211622353,
-29.6250049671436)) ;
#62172 = CARTESIAN_POINT('Ctrl Pts',(-9.98127620657957,-1.91496854175463,
-29.6247970918333)) ;
#62173 = CARTESIAN_POINT('Ctrl Pts',(-9.98117504271719,-1.91291654329207,
-29.6243836891066)) ;
#62174 = CARTESIAN_POINT('Ctrl Pts',(-9.98112587708293,-1.91189811925535,
-29.624178162495)) ;
#62175 = CARTESIAN_POINT('Ctrl Pts',(-9.9810314696815,-1.90987945010399,-29.6237697515287)) ;
#62176 = CARTESIAN_POINT('Ctrl Pts',(-9.98098619082925,-1.90887920681535,
-29.6235668800677)) ;
#62177 = CARTESIAN_POINT('Ctrl Pts',(-9.98092285308603,-1.90739476140765,
-29.6232645011586)) ;
#62178 = CARTESIAN_POINT('Ctrl Pts',(-9.98090251330511,-1.90690260002959,
-29.6231640265195)) ;
#62179 = CARTESIAN_POINT('Ctrl Pts',(-9.9808639831162,-1.90592397215236,-29.6229635949418)) ;
#62180 = CARTESIAN_POINT('Ctrl Pts',(-9.98084576984047,-1.90543750500457,
-29.6228636455668)) ;
#62181 = CARTESIAN_POINT('Ctrl Pts',(-9.98082073735356,-1.90470544204056,
-29.6227124356354)) ;
#62182 = CARTESIAN_POINT('Ctrl Pts',(-9.98081223578881,-1.90444442082997,
-29.6226583780428)) ;
#62183 = CARTESIAN_POINT('Ctrl Pts',(-9.98079629773457,-1.90391015043467,
-29.622547237381)) ;
#62184 = CARTESIAN_POINT('Ctrl Pts',(-9.98078885639857,-1.90363690106332,
-29.6224901559041)) ;
#62185 = CARTESIAN_POINT('Ctrl Pts',(-9.98077656125721,-1.90309071520488,
-29.6223751893419)) ;
#62186 = CARTESIAN_POINT('Ctrl Pts',(-9.98077161921038,-1.90281781754094,
-29.622317342455)) ;
#62187 = CARTESIAN_POINT('Ctrl Pts',(-9.98081728992659,-1.90163369721464,
-29.6220437275998)) ;
#62188 = CARTESIAN_POINT('Ctrl Pts',(-9.98081916755763,-1.90158501523074,
-29.6220324786468)) ;
#62189 = CARTESIAN_POINT('Ctrl Pts',(-9.98082104518866,-1.90153633324684,
-29.6220212296937)) ;
#62190 = CARTESIAN_POINT('',(-23.3738245177975,-15.0366437072153,-24.6538954375548)) ;
#62191 = CARTESIAN_POINT('',(-23.3523050271304,-15.0366437072153,-24.674279781881)) ;
#62192 = CARTESIAN_POINT('Origin',(0.939357956114989,-21.6462763158693,0.99166813738465)) ;
#62193 = CARTESIAN_POINT('',(-21.4963117156553,-1.90153624017924,-22.6933803539597)) ;
#62194 = CARTESIAN_POINT('Ctrl Pts',(-21.4963117284258,-1.90153632878805,
-22.693380367086)) ;
#62195 = CARTESIAN_POINT('Ctrl Pts',(-21.4963232866611,-1.90158488951342,
-22.6933832416551)) ;
#62196 = CARTESIAN_POINT('Ctrl Pts',(-21.4965226828145,-1.90242263174387,
-22.6934328320992)) ;
#62197 = CARTESIAN_POINT('Ctrl Pts',(-21.4965976870093,-1.90282441414894,
-22.6934761542018)) ;
#62198 = CARTESIAN_POINT('Ctrl Pts',(-21.4966467084764,-1.90309873182999,
-22.6935078048281)) ;
#62199 = CARTESIAN_POINT('Ctrl Pts',(-21.4967429748708,-1.9036477578842,-22.6935729001217)) ;
#62200 = CARTESIAN_POINT('Ctrl Pts',(-21.4967901444201,-1.90392242741489,
-22.693606405134)) ;
#62201 = CARTESIAN_POINT('Ctrl Pts',(-21.4968813060532,-1.90445947365899,
-22.6936729257873)) ;
#62202 = CARTESIAN_POINT('Ctrl Pts',(-21.4969252944931,-1.90472185055691,
-22.6937059449324)) ;
#62203 = CARTESIAN_POINT('Ctrl Pts',(-21.4970477581099,-1.90545775489615,
-22.6937994209599)) ;
#62204 = CARTESIAN_POINT('Ctrl Pts',(-21.4971279264057,-1.90594678820076,
-22.6938626878748)) ;
#62205 = CARTESIAN_POINT('Ctrl Pts',(-21.497287749129,-1.9069305782757,-22.6939913376866)) ;
#62206 = CARTESIAN_POINT('Ctrl Pts',(-21.4973673860617,-1.90742533569666,
-22.6940567373406)) ;
#62207 = CARTESIAN_POINT('Ctrl Pts',(-21.497606056854,-1.90891761107545,-22.6942554417845)) ;
#62208 = CARTESIAN_POINT('Ctrl Pts',(-21.4977648791666,-1.90992313013283,
-22.694391224525)) ;
#62209 = CARTESIAN_POINT('Ctrl Pts',(-21.4980830859284,-1.91195244645976,
-22.6946674605282)) ;
#62210 = CARTESIAN_POINT('Ctrl Pts',(-21.4982424415412,-1.91297624190247,
-22.6948079405862)) ;
#62211 = CARTESIAN_POINT('Ctrl Pts',(-21.4985619093448,-1.91503906287447,
-22.6950925193719)) ;
#62212 = CARTESIAN_POINT('Ctrl Pts',(-21.4987220196732,-1.91607808844715,
-22.695236619876)) ;
#62213 = CARTESIAN_POINT('Ctrl Pts',(-21.4992033798014,-1.91921345485071,
-22.6956731528048)) ;
#62214 = CARTESIAN_POINT('Ctrl Pts',(-21.4995256903791,-1.92132807011153,
-22.6959697823368)) ;
#62215 = CARTESIAN_POINT('Ctrl Pts',(-21.5001711350599,-1.92558172137742,
-22.6965692128324)) ;
#62216 = CARTESIAN_POINT('Ctrl Pts',(-21.5004942431825,-1.92772075783832,
-22.6968720385356)) ;
#62217 = CARTESIAN_POINT('Ctrl Pts',(-21.5014605714309,-1.93413803849897,
-22.6977834024756)) ;
#62218 = CARTESIAN_POINT('Ctrl Pts',(-21.5021008361852,-1.93841640089627,
-22.6983947738345)) ;
#62219 = CARTESIAN_POINT('Ctrl Pts',(-21.5033480901722,-1.94677887282856,
-22.6995937415208)) ;
#62220 = CARTESIAN_POINT('Ctrl Pts',(-21.5039550263826,-1.95086298304285,
-22.7001813882667)) ;
#62221 = CARTESIAN_POINT('Ctrl Pts',(-21.5051079743681,-1.95863767898893,
-22.7013023732685)) ;
#62222 = CARTESIAN_POINT('Ctrl Pts',(-21.5056846047152,-1.96253483117455,
-22.7018655084924)) ;
#62223 = CARTESIAN_POINT('Ctrl Pts',(-21.5068393899876,-1.97035266864422,
-22.7029970336256)) ;
#62224 = CARTESIAN_POINT('Ctrl Pts',(-21.5074175436022,-1.97427335394165,
-22.7035654247798)) ;
#62225 = CARTESIAN_POINT('Ctrl Pts',(-21.5091547200953,-1.98606956727156,
-22.7052777489694)) ;
#62226 = CARTESIAN_POINT('Ctrl Pts',(-21.510316493032,-1.99397925232716,-22.7064288000193)) ;
#62227 = CARTESIAN_POINT('Ctrl Pts',(-21.5126483548276,-2.00988362758461,
-22.7087472221003)) ;
#62228 = CARTESIAN_POINT('Ctrl Pts',(-21.513818422781,-2.01787831761191,-22.7099146128845)) ;
#62229 = CARTESIAN_POINT('Ctrl Pts',(-21.5161669917595,-2.03394662784809,
-22.7122638741884)) ;
#62230 = CARTESIAN_POINT('Ctrl Pts',(-21.5173454921875,-2.0420202480614,-22.7134457452744)) ;
#62231 = CARTESIAN_POINT('Ctrl Pts',(-21.5208932751436,-2.06635039651484,
-22.7170108341686)) ;
#62232 = CARTESIAN_POINT('Ctrl Pts',(-21.5232749130048,-2.08271620910784,
-22.7194134568504)) ;
#62233 = CARTESIAN_POINT('Ctrl Pts',(-21.5280670365947,-2.11569069163832,
-22.7242605069101)) ;
#62234 = CARTESIAN_POINT('Ctrl Pts',(-21.5304774872622,-2.13229936178073,
-22.7267049675577)) ;
#62235 = CARTESIAN_POINT('Ctrl Pts',(-21.5353217952499,-2.16571099763217,
-22.73162702433)) ;
#62236 = CARTESIAN_POINT('Ctrl Pts',(-21.5377556391222,-2.18251395950177,
-22.7341046321001)) ;
#62237 = CARTESIAN_POINT('Ctrl Pts',(-21.5426407161461,-2.21626560493476,
-22.7390848562231)) ;
#62238 = CARTESIAN_POINT('Ctrl Pts',(-21.5450919476502,-2.23321428850602,
-22.7415874741381)) ;
#62239 = CARTESIAN_POINT('Ctrl Pts',(-21.5524622515727,-2.28420607479834,
-22.7491210791498)) ;
#62240 = CARTESIAN_POINT('Ctrl Pts',(-21.5573979862509,-2.31839491280777,
-22.7541777673676)) ;
#62241 = CARTESIAN_POINT('Ctrl Pts',(-21.5672614105418,-2.38677270727805,
-22.7642987982121)) ;
#62242 = CARTESIAN_POINT('Ctrl Pts',(-21.5721890660041,-2.42096165007377,
-22.7693631692978)) ;
#62243 = CARTESIAN_POINT('Ctrl Pts',(-21.581982528211,-2.48895109743765,-22.7794399263397)) ;
#62244 = CARTESIAN_POINT('Ctrl Pts',(-21.5868483219591,-2.52275160205135,
-22.7844523246197)) ;
#62245 = CARTESIAN_POINT('Ctrl Pts',(-21.6012713504402,-2.62298766794955,
-22.7993229231962)) ;
#62246 = CARTESIAN_POINT('Ctrl Pts',(-21.6106543166059,-2.68825778093597,
-22.809014447373)) ;
#62247 = CARTESIAN_POINT('Ctrl Pts',(-21.6293728962788,-2.81853945706393,
-22.8283687527329)) ;
#62248 = CARTESIAN_POINT('Ctrl Pts',(-21.6391845503111,-2.88687193745379,
-22.8385259240375)) ;
#62249 = CARTESIAN_POINT('Ctrl Pts',(-21.6588580128413,-3.02394935341697,
-22.8589101657353)) ;
#62250 = CARTESIAN_POINT('Ctrl Pts',(-21.6687197928116,-3.09269428906301,
-22.869137263172)) ;
#62251 = CARTESIAN_POINT('Ctrl Pts',(-21.6884935733421,-3.23058330762132,
-22.8896575063169)) ;
#62252 = CARTESIAN_POINT('Ctrl Pts',(-21.6984055623305,-3.29972739051995,
-22.8999506629822)) ;
#62253 = CARTESIAN_POINT('Ctrl Pts',(-21.7182791782898,-3.43840139699515,
-22.9205997886577)) ;
#62254 = CARTESIAN_POINT('Ctrl Pts',(-21.7282408037747,-3.50793132057516,
-22.930955759075)) ;
#62255 = CARTESIAN_POINT('Ctrl Pts',(-21.758198695169,-3.71707989379933,-22.9621135734917)) ;
#62256 = CARTESIAN_POINT('Ctrl Pts',(-21.7782680553984,-3.85725734527214,
-22.9830052452732)) ;
#62257 = CARTESIAN_POINT('Ctrl Pts',(-21.8185913442818,-4.13899594502097,
-23.0250076342015)) ;
#62258 = CARTESIAN_POINT('Ctrl Pts',(-21.8388452294421,-4.28055709337647,
-23.0461183925702)) ;
#62259 = CARTESIAN_POINT('Ctrl Pts',(-21.8795252773123,-4.56495664868979,
-23.0885402989146)) ;
#62260 = CARTESIAN_POINT('Ctrl Pts',(-21.8999514204951,-4.70779505473742,
-23.1098514651284)) ;
#62261 = CARTESIAN_POINT('Ctrl Pts',(-21.9409627358116,-4.99464268526103,
-23.1526564380478)) ;
#62262 = CARTESIAN_POINT('Ctrl Pts',(-21.9615478982523,-5.13865190975205,
-23.1741502539394)) ;
#62263 = CARTESIAN_POINT('Ctrl Pts',(-22.0028634384497,-5.42773473974678,
-23.217303313115)) ;
#62264 = CARTESIAN_POINT('Ctrl Pts',(-22.023593811453,-5.57280834524819,-23.2389625609007)) ;
#62265 = CARTESIAN_POINT('Ctrl Pts',(-22.0651855999471,-5.86391350033323,
-23.2824296111504)) ;
#62266 = CARTESIAN_POINT('Ctrl Pts',(-22.0860470145812,-6.00994504991818,
-23.3042374144253)) ;
#62267 = CARTESIAN_POINT('Ctrl Pts',(-22.1488062119652,-6.4493169599107,-23.3698586798306)) ;
#62268 = CARTESIAN_POINT('Ctrl Pts',(-22.1908790031683,-6.7439345768575,-23.4138699441313)) ;
#62269 = CARTESIAN_POINT('Ctrl Pts',(-22.2753741970227,-7.33572433231973,
-23.502288463561)) ;
#62270 = CARTESIAN_POINT('Ctrl Pts',(-22.3177965716302,-7.63289647086886,
-23.5466957452641)) ;
#62271 = CARTESIAN_POINT('Ctrl Pts',(-22.4028723995403,-8.22894377232508,
-23.6357761957328)) ;
#62272 = CARTESIAN_POINT('Ctrl Pts',(-22.4455258389439,-8.52781893522888,
-23.6804493776631)) ;
#62273 = CARTESIAN_POINT('Ctrl Pts',(-22.5309444631914,-9.12642078899722,
-23.7699322833272)) ;
#62274 = CARTESIAN_POINT('Ctrl Pts',(-22.5737096415316,-9.42614747986867,
-23.8147420132228)) ;
#62275 = CARTESIAN_POINT('Ctrl Pts',(-22.7019930343727,-10.3253276006806,
-23.9491827183168)) ;
#62276 = CARTESIAN_POINT('Ctrl Pts',(-22.7874992191758,-10.9247810633858,
-24.0388250979726)) ;
#62277 = CARTESIAN_POINT('Ctrl Pts',(-22.9575171690251,-12.1168760956996,
-24.2171127741637)) ;
#62278 = CARTESIAN_POINT('Ctrl Pts',(-23.0420288777932,-12.7095176653597,
-24.3057581240216)) ;
#62279 = CARTESIAN_POINT('Ctrl Pts',(-23.2094672465774,-13.8838032558862,
-24.4814197413028)) ;
#62280 = CARTESIAN_POINT('Ctrl Pts',(-23.2923850750004,-14.4653860626283,
-24.5684269494759)) ;
#62281 = CARTESIAN_POINT('Ctrl Pts',(-23.3738245177983,-15.0366437072153,
-24.6538954375541)) ;
#62282 = CARTESIAN_POINT('Ctrl Pts',(-23.3523050271281,-15.0366437072153,
-24.6742797818832)) ;
#62283 = CARTESIAN_POINT('Ctrl Pts',(-23.3519438108906,-15.0340941324353,
-24.6738961918291)) ;
#62284 = CARTESIAN_POINT('Ctrl Pts',(-23.3515825656427,-15.0315443519866,
-24.6735125707103)) ;
#62285 = CARTESIAN_POINT('Ctrl Pts',(-23.2706354764949,-14.4601946119446,
-24.58755148494)) ;
#62286 = CARTESIAN_POINT('Ctrl Pts',(-23.1886083812775,-13.8811769235724,
-24.500430706285)) ;
#62287 = CARTESIAN_POINT('Ctrl Pts',(-23.0226413408112,-12.7095176655682,
-24.324122974606)) ;
#62288 = CARTESIAN_POINT('Ctrl Pts',(-22.9387013686766,-12.116876095939,-24.2349360470503)) ;
#62289 = CARTESIAN_POINT('Ctrl Pts',(-22.7698797529755,-10.9247810636875,
-24.0555151429776)) ;
#62290 = CARTESIAN_POINT('Ctrl Pts',(-22.6849980531189,-10.3253276010136,
-23.965281219768)) ;
#62291 = CARTESIAN_POINT('Ctrl Pts',(-22.5576996397855,-9.42614748024864,
-23.8299074925378)) ;
#62292 = CARTESIAN_POINT('Ctrl Pts',(-22.5152708873019,-9.12642078939284,
-23.7847790831478)) ;
#62293 = CARTESIAN_POINT('Ctrl Pts',(-22.430543687122,-8.52781893565576,-23.6946412258264)) ;
#62294 = CARTESIAN_POINT('Ctrl Pts',(-22.3882452329189,-8.22894377276754,
-23.6496317840573)) ;
#62295 = CARTESIAN_POINT('Ctrl Pts',(-22.3039013390795,-7.63289647134248,
-23.5598580088181)) ;
#62296 = CARTESIAN_POINT('Ctrl Pts',(-22.2618558855447,-7.33572433280887,
-23.5150936885143)) ;
#62297 = CARTESIAN_POINT('Ctrl Pts',(-22.1781415170712,-6.74393457737753,
-23.4259355320049)) ;
#62298 = CARTESIAN_POINT('Ctrl Pts',(-22.1364725740781,-6.44931696044613,
-23.3815417223642)) ;
#62299 = CARTESIAN_POINT('Ctrl Pts',(-22.0743452623651,-6.00994505047655,
-23.3153219030641)) ;
#62300 = CARTESIAN_POINT('Ctrl Pts',(-22.053698856334,-5.86391350089923,-23.2933104328244)) ;
#62301 = CARTESIAN_POINT('Ctrl Pts',(-22.0125472882954,-5.5728083458294,-23.2494263836136)) ;
#62302 = CARTESIAN_POINT('Ctrl Pts',(-21.9920421254311,-5.42773474033559,
-23.2275538054548)) ;
#62303 = CARTESIAN_POINT('Ctrl Pts',(-21.9511891321905,-5.13865191035594,
-23.1839625985327)) ;
#62304 = CARTESIAN_POINT('Ctrl Pts',(-21.9308412970635,-4.99464268587244,
-23.1622439742704)) ;
#62305 = CARTESIAN_POINT('Ctrl Pts',(-21.8903194091775,-4.70779505536381,
-23.1189753910673)) ;
#62306 = CARTESIAN_POINT('Ctrl Pts',(-21.8701453467194,-4.56495664932364,
-23.0974254413096)) ;
#62307 = CARTESIAN_POINT('Ctrl Pts',(-21.82998802915,-4.28055709402517,-23.0545083785269)) ;
#62308 = CARTESIAN_POINT('Ctrl Pts',(-21.8100047547694,-4.13899594567707,
-23.0331412840139)) ;
#62309 = CARTESIAN_POINT('Ctrl Pts',(-21.7702470248157,-3.85725734594295,
-22.9906031692151)) ;
#62310 = CARTESIAN_POINT('Ctrl Pts',(-21.7504725257305,-3.71707989447745,
-22.9694321901238)) ;
#62311 = CARTESIAN_POINT('Ctrl Pts',(-21.720982294478,-3.50793132126421,-22.9378313844934)) ;
#62312 = CARTESIAN_POINT('Ctrl Pts',(-21.7111808235151,-3.43840139768783,
-22.9273237076555)) ;
#62313 = CARTESIAN_POINT('Ctrl Pts',(-21.69163791744,-3.29972739121987,-22.9063613169399)) ;
#62314 = CARTESIAN_POINT('Ctrl Pts',(-21.681896480842,-3.23058330832484,-22.8959066044699)) ;
#62315 = CARTESIAN_POINT('Ctrl Pts',(-21.6624768632991,-3.09269428977375,
-22.8750508803254)) ;
#62316 = CARTESIAN_POINT('Ctrl Pts',(-21.6527986707855,-3.02394935413129,
-22.8646498796134)) ;
#62317 = CARTESIAN_POINT('Ctrl Pts',(-21.6335094241247,-2.88687193817528,
-22.843901689314)) ;
#62318 = CARTESIAN_POINT('Ctrl Pts',(-21.6238983414308,-2.81853945778899,
-22.8335545267469)) ;
#62319 = CARTESIAN_POINT('Ctrl Pts',(-21.6055858243229,-2.68825778181904,
-22.8138155785391)) ;
#62320 = CARTESIAN_POINT('Ctrl Pts',(-21.5964164971659,-2.62298766899475,
-22.80392168479)) ;
#62321 = CARTESIAN_POINT('Ctrl Pts',(-21.582348554658,-2.5227516033456,-22.7887147309843)) ;
#62322 = CARTESIAN_POINT('Ctrl Pts',(-21.5776069362756,-2.48895109881591,
-22.7835847075738)) ;
#62323 = CARTESIAN_POINT('Ctrl Pts',(-21.5680751650442,-2.42096165162096,
-22.7732600637207)) ;
#62324 = CARTESIAN_POINT('Ctrl Pts',(-21.5632849991904,-2.38677270891016,
-22.7680654555843)) ;
#62325 = CARTESIAN_POINT('Ctrl Pts',(-21.5537128067588,-2.31839491460977,
-22.7576685553175)) ;
#62326 = CARTESIAN_POINT('Ctrl Pts',(-21.5489307499096,-2.28420607668529,
-22.7524662957519)) ;
#62327 = CARTESIAN_POINT('Ctrl Pts',(-21.5418072138063,-2.23321429051965,
-22.7446989398817)) ;
#62328 = CARTESIAN_POINT('Ctrl Pts',(-21.5394409731948,-2.21626560699046,
-22.7421158143287)) ;
#62329 = CARTESIAN_POINT('Ctrl Pts',(-21.5347325257493,-2.18251396164137,
-22.7369682778057)) ;
#62330 = CARTESIAN_POINT('Ctrl Pts',(-21.5323903172678,-2.16571099981351,
-22.7344038683946)) ;
#62331 = CARTESIAN_POINT('Ctrl Pts',(-21.5277377446746,-2.13229936404508,
-22.729300190233)) ;
#62332 = CARTESIAN_POINT('Ctrl Pts',(-21.5254273682071,-2.11569069394391,
-22.7267609342797)) ;
#62333 = CARTESIAN_POINT('Ctrl Pts',(-21.5208468671157,-2.08271621149533,
-22.7217134247648)) ;
#62334 = CARTESIAN_POINT('Ctrl Pts',(-21.5185767073711,-2.06635039894304,
-22.7192052044134)) ;
#62335 = CARTESIAN_POINT('Ctrl Pts',(-21.5152089200917,-2.04202025055005,
-22.7154696145748)) ;
#62336 = CARTESIAN_POINT('Ctrl Pts',(-21.5140925850502,-2.03394663035677,
-22.7142288573126)) ;
#62337 = CARTESIAN_POINT('Ctrl Pts',(-21.5118739181062,-2.01787832016053,
-22.7117565462768)) ;
#62338 = CARTESIAN_POINT('Ctrl Pts',(-21.5107715856034,-2.00988363015303,
-22.7105249930715)) ;
#62339 = CARTESIAN_POINT('Ctrl Pts',(-21.5085828081459,-1.9939792549351,-22.7080710343171)) ;
#62340 = CARTESIAN_POINT('Ctrl Pts',(-21.5074963423416,-1.98606956989922,
-22.706848648568)) ;
#62341 = CARTESIAN_POINT('Ctrl Pts',(-21.5058805782652,-1.97427335659861,
-22.7050213164367)) ;
#62342 = CARTESIAN_POINT('Ctrl Pts',(-21.5053443213055,-1.97035267131085,
-22.7044132386656)) ;
#62343 = CARTESIAN_POINT('Ctrl Pts',(-21.5042769744681,-1.96253483386059,
-22.7031988874529)) ;
#62344 = CARTESIAN_POINT('Ctrl Pts',(-21.5037458832862,-1.95863768168481,
-22.7025926152431)) ;
#62345 = CARTESIAN_POINT('Ctrl Pts',(-21.5026889616459,-1.95086298569985,
-22.7013806692445)) ;
#62346 = CARTESIAN_POINT('Ctrl Pts',(-21.502135035599,-1.9467788754347,-22.7007428085899)) ;
#62347 = CARTESIAN_POINT('Ctrl Pts',(-21.5010053512569,-1.93841640339806,
-22.6994324729907)) ;
#62348 = CARTESIAN_POINT('Ctrl Pts',(-21.5004295397412,-1.93413804094723,
-22.6987600482659)) ;
#62349 = CARTESIAN_POINT('Ctrl Pts',(-21.4995718283387,-1.92772076020648,
-22.6977457969615)) ;
#62350 = CARTESIAN_POINT('Ctrl Pts',(-21.4992869394374,-1.92558172371826,
-22.6974067680811)) ;
#62351 = CARTESIAN_POINT('Ctrl Pts',(-21.4987233317185,-1.92132807239916,
-22.6967298174825)) ;
#62352 = CARTESIAN_POINT('Ctrl Pts',(-21.4984445867594,-1.91921345711195,
-22.696391920397)) ;
#62353 = CARTESIAN_POINT('Ctrl Pts',(-21.4980347543484,-1.91607809066923,
-22.6958876328044)) ;
#62354 = CARTESIAN_POINT('Ctrl Pts',(-21.4978995333845,-1.91503906508375,
-22.6957199558382)) ;
#62355 = CARTESIAN_POINT('Ctrl Pts',(-21.4976326675899,-1.9129762440859,-22.6953855497755)) ;
#62356 = CARTESIAN_POINT('Ctrl Pts',(-21.4975010209054,-1.91195244863063,
-22.6952188224229)) ;
#62357 = CARTESIAN_POINT('Ctrl Pts',(-21.4972424173842,-1.90992313227818,
-22.694886127224)) ;
#62358 = CARTESIAN_POINT('Ctrl Pts',(-21.4971154322506,-1.90891761320832,
-22.6947201867021)) ;
#62359 = CARTESIAN_POINT('Ctrl Pts',(-21.4969299405941,-1.90742533781066,
-22.6944711082995)) ;
#62360 = CARTESIAN_POINT('Ctrl Pts',(-21.4968689482557,-1.90693058038146,
-22.6943880475454)) ;
#62361 = CARTESIAN_POINT('Ctrl Pts',(-21.4967491397467,-1.90594679029413,
-22.694221494253)) ;
#62362 = CARTESIAN_POINT('Ctrl Pts',(-21.4966903059277,-1.90545775698652,
-22.6941380182473)) ;
#62363 = CARTESIAN_POINT('Ctrl Pts',(-21.4966035970227,-1.90472185252296,
-22.6940106735224)) ;
#62364 = CARTESIAN_POINT('Ctrl Pts',(-21.4965730077366,-1.9044594754992,-22.6939649619888)) ;
#62365 = CARTESIAN_POINT('Ctrl Pts',(-21.4965115200034,-1.90392242900148,
-22.6938703326523)) ;
#62366 = CARTESIAN_POINT('Ctrl Pts',(-21.4964806178287,-1.90364775934146,
-22.6938214183275)) ;
#62367 = CARTESIAN_POINT('Ctrl Pts',(-21.4964208297127,-1.90309873302708,
-22.693721768899)) ;
#62368 = CARTESIAN_POINT('Ctrl Pts',(-21.4963918793817,-1.90282441521009,
-22.693671105844)) ;
#62369 = CARTESIAN_POINT('Ctrl Pts',(-21.4963177870611,-1.90163369563563,
-22.6934023441179)) ;
#62370 = CARTESIAN_POINT('Ctrl Pts',(-21.4963147577435,-1.90158501221184,
-22.6933913556019)) ;
#62371 = CARTESIAN_POINT('Ctrl Pts',(-21.4963117284258,-1.90153632878805,
-22.693380367086)) ;
#62372 = CARTESIAN_POINT('',(-31.5654106012916,-15.0366437072153,-12.5608553214559)) ;
#62373 = CARTESIAN_POINT('',(-31.5544392045422,-15.0366437072153,-12.5883914509173)) ;
#62374 = CARTESIAN_POINT('Origin',(1.26892883449471,-21.6462763158693,0.505587457724594)) ;
#62375 = CARTESIAN_POINT('',(-29.0382272152461,-1.90153624159665,-11.5698871852821)) ;
#62376 = CARTESIAN_POINT('Ctrl Pts',(-29.0382272326218,-1.90153633162286,
-11.5698871919368)) ;
#62377 = CARTESIAN_POINT('Ctrl Pts',(-29.0382389339435,-1.90158489075259,
-11.5698849358364)) ;
#62378 = CARTESIAN_POINT('Ctrl Pts',(-29.038439954612,-1.9024191032399,-11.5698461775814)) ;
#62379 = CARTESIAN_POINT('Ctrl Pts',(-29.0385258858908,-1.90281925831921,
-11.5698539247859)) ;
#62380 = CARTESIAN_POINT('Ctrl Pts',(-29.0385834427646,-1.90309246582992,
-11.5698620077834)) ;
#62381 = CARTESIAN_POINT('Ctrl Pts',(-29.0386976993411,-1.90363927141272,
-11.569880543178)) ;
#62382 = CARTESIAN_POINT('Ctrl Pts',(-29.0387543560843,-1.90391283065899,
-11.5698910817176)) ;
#62383 = CARTESIAN_POINT('Ctrl Pts',(-29.0388645914481,-1.90444770673756,
-11.569913048999)) ;
#62384 = CARTESIAN_POINT('Ctrl Pts',(-29.0389181682581,-1.90470902375223,
-11.5699244823868)) ;
#62385 = CARTESIAN_POINT('Ctrl Pts',(-29.0390679674835,-1.90544192542839,
-11.5699577154286)) ;
#62386 = CARTESIAN_POINT('Ctrl Pts',(-29.0391668949579,-1.90592895304488,
-11.5699813481566)) ;
#62387 = CARTESIAN_POINT('Ctrl Pts',(-29.0393651689924,-1.90690870838148,
-11.5700307443233)) ;
#62388 = CARTESIAN_POINT('Ctrl Pts',(-29.0394645067144,-1.90740143675332,
-11.570056530308)) ;
#62389 = CARTESIAN_POINT('Ctrl Pts',(-29.0397633492989,-1.90888759228089,
-11.5701362566965)) ;
#62390 = CARTESIAN_POINT('Ctrl Pts',(-29.0399636978026,-1.90988898783355,
-11.5701925287128)) ;
#62391 = CARTESIAN_POINT('Ctrl Pts',(-29.0403668539109,-1.91190998240188,
-11.5703090644009)) ;
#62392 = CARTESIAN_POINT('Ctrl Pts',(-29.0405696466344,-1.91292957959075,
-11.5703693644013)) ;
#62393 = CARTESIAN_POINT('Ctrl Pts',(-29.0409774276981,-1.91498394176463,
-11.570492922451)) ;
#62394 = CARTESIAN_POINT('Ctrl Pts',(-29.0411824151165,-1.91601870679206,
-11.5705561828368)) ;
#62395 = CARTESIAN_POINT('Ctrl Pts',(-29.0418000753912,-1.91914121681058,
-11.5707493624156)) ;
#62396 = CARTESIAN_POINT('Ctrl Pts',(-29.0422154605921,-1.9212471614821,-11.5708826355584)) ;
#62397 = CARTESIAN_POINT('Ctrl Pts',(-29.043049553386,-1.92548337189837,-11.5711544224452)) ;
#62398 = CARTESIAN_POINT('Ctrl Pts',(-29.0434682478049,-1.92761363809929,
-11.5712929695085)) ;
#62399 = CARTESIAN_POINT('Ctrl Pts',(-29.044722827206,-1.93400460796368,-11.5717124807114)) ;
#62400 = CARTESIAN_POINT('Ctrl Pts',(-29.0455572226705,-1.93826542981638,
-11.5719972492473)) ;
#62401 = CARTESIAN_POINT('Ctrl Pts',(-29.0471859897073,-1.94659361793648,
-11.5725592267218)) ;
#62402 = CARTESIAN_POINT('Ctrl Pts',(-29.0479803343802,-1.95066098488323,
-11.5728365035519)) ;
#62403 = CARTESIAN_POINT('Ctrl Pts',(-29.0494912134324,-1.95840366317408,
-11.5733674500498)) ;
#62404 = CARTESIAN_POINT('Ctrl Pts',(-29.0502478839205,-1.96228469345615,
-11.5736352446663)) ;
#62405 = CARTESIAN_POINT('Ctrl Pts',(-29.0517647982348,-1.97007018980902,
-11.5741749503929)) ;
#62406 = CARTESIAN_POINT('Ctrl Pts',(-29.0525250413989,-1.97397465589319,
-11.5744468631722)) ;
#62407 = CARTESIAN_POINT('Ctrl Pts',(-29.0548112132387,-1.98572207032782,
-11.5752679344914)) ;
#62408 = CARTESIAN_POINT('Ctrl Pts',(-29.0563426017227,-1.99359903444582,
-11.5758223819579)) ;
#62409 = CARTESIAN_POINT('Ctrl Pts',(-29.0594197151388,-2.00943761625919,
-11.5769425597229)) ;
#62410 = CARTESIAN_POINT('Ctrl Pts',(-29.0609654294151,-2.01739923378007,
-11.5775083166679)) ;
#62411 = CARTESIAN_POINT('Ctrl Pts',(-29.0640705317916,-2.03340107254685,
-11.5786493986402)) ;
#62412 = CARTESIAN_POINT('Ctrl Pts',(-29.0656299195902,-2.04144129379721,
-11.5792247244255)) ;
#62413 = CARTESIAN_POINT('Ctrl Pts',(-29.070327323818,-2.06567079334489,-11.5809631771912)) ;
#62414 = CARTESIAN_POINT('Ctrl Pts',(-29.073484618138,-2.08196890397857,-11.5821386846341)) ;
#62415 = CARTESIAN_POINT('Ctrl Pts',(-29.0798427548892,-2.11480697810897,
-11.5845154356313)) ;
#62416 = CARTESIAN_POINT('Ctrl Pts',(-29.0830435795052,-2.13134694181059,
-11.5857167240125)) ;
#62417 = CARTESIAN_POINT('Ctrl Pts',(-29.0894802354408,-2.16462036119451,
-11.5881394728866)) ;
#62418 = CARTESIAN_POINT('Ctrl Pts',(-29.09271605946,-2.18135381303769,-11.5893609495587)) ;
#62419 = CARTESIAN_POINT('Ctrl Pts',(-29.0992138781996,-2.21496583572871,
-11.5918192436418)) ;
#62420 = CARTESIAN_POINT('Ctrl Pts',(-29.1024758720817,-2.23184440658444,
-11.5930560631602)) ;
#62421 = CARTESIAN_POINT('Ctrl Pts',(-29.1122876293211,-2.2826252520403,-11.5967828618532)) ;
#62422 = CARTESIAN_POINT('Ctrl Pts',(-29.1188631951064,-2.31667265923911,
-11.5992891136516)) ;
#62423 = CARTESIAN_POINT('Ctrl Pts',(-29.1320102476389,-2.38476759208326,
-11.6043119209944)) ;
#62424 = CARTESIAN_POINT('Ctrl Pts',(-29.138581715377,-2.41881510406427,-11.6068285166186)) ;
#62425 = CARTESIAN_POINT('Ctrl Pts',(-29.1516470060032,-2.48652329696422,
-11.6118406024886)) ;
#62426 = CARTESIAN_POINT('Ctrl Pts',(-29.1581408222881,-2.52018397792869,
-11.6143361093325)) ;
#62427 = CARTESIAN_POINT('Ctrl Pts',(-29.1773950156982,-2.62000539438071,
-11.6217449858488)) ;
#62428 = CARTESIAN_POINT('Ctrl Pts',(-29.1899281801797,-2.68500550307164,
-11.6265806038851)) ;
#62429 = CARTESIAN_POINT('Ctrl Pts',(-29.2149343835133,-2.81472076277575,
-11.6362436435832)) ;
#62430 = CARTESIAN_POINT('Ctrl Pts',(-29.2280443982007,-2.88274300721894,
-11.6413188248167)) ;
#62431 = CARTESIAN_POINT('Ctrl Pts',(-29.2543389486577,-3.0191980787507,-11.6515113939421)) ;
#62432 = CARTESIAN_POINT('Ctrl Pts',(-29.2675234699474,-3.08763090591191,
-11.6566288182163)) ;
#62433 = CARTESIAN_POINT('Ctrl Pts',(-29.2939654853015,-3.22489389536975,
-11.6669023629037)) ;
#62434 = CARTESIAN_POINT('Ctrl Pts',(-29.3072229734857,-3.29372405765274,
-11.6720584980668)) ;
#62435 = CARTESIAN_POINT('Ctrl Pts',(-29.3338090447939,-3.43176847117171,
-11.6824067818085)) ;
#62436 = CARTESIAN_POINT('Ctrl Pts',(-29.3471376271619,-3.50098272241108,
-11.6875989322834)) ;
#62437 = CARTESIAN_POINT('Ctrl Pts',(-29.3872269113491,-3.70918174163314,
-11.7032261047598)) ;
#62438 = CARTESIAN_POINT('Ctrl Pts',(-29.4140911905175,-3.84872277446492,
-11.7137117463827)) ;
#62439 = CARTESIAN_POINT('Ctrl Pts',(-29.4680780422506,-4.1291822548889,-11.7348038136094)) ;
#62440 = CARTESIAN_POINT('Ctrl Pts',(-29.4952005927186,-4.27010070256046,
-11.7454102947159)) ;
#62441 = CARTESIAN_POINT('Ctrl Pts',(-29.5496850877767,-4.5532090576965,-11.7667323167097)) ;
#62442 = CARTESIAN_POINT('Ctrl Pts',(-29.5770470223282,-4.69539896425168,
-11.7774478822838)) ;
#62443 = CARTESIAN_POINT('Ctrl Pts',(-29.6319908991029,-4.98094428021694,
-11.7989775706329)) ;
#62444 = CARTESIAN_POINT('Ctrl Pts',(-29.6595728364002,-5.12429968964207,
-11.8097917057789)) ;
#62445 = CARTESIAN_POINT('Ctrl Pts',(-29.7149370452325,-5.41207005716519,
-11.8315087525043)) ;
#62446 = CARTESIAN_POINT('Ctrl Pts',(-29.742719314352,-5.55648501526087,-11.8424116701445)) ;
#62447 = CARTESIAN_POINT('Ctrl Pts',(-29.7984643308215,-5.846268526428,-11.8642969595879)) ;
#62448 = CARTESIAN_POINT('Ctrl Pts',(-29.8264270777348,-5.99163707950077,
-11.875279332486)) ;
#62449 = CARTESIAN_POINT('Ctrl Pts',(-29.9105560733675,-6.42901420114677,
-11.9083320971568)) ;
#62450 = CARTESIAN_POINT('Ctrl Pts',(-29.966963104371,-6.72229422745249,-11.9305080635348)) ;
#62451 = CARTESIAN_POINT('Ctrl Pts',(-30.0802585252516,-7.31139720401595,
-11.9750716664965)) ;
#62452 = CARTESIAN_POINT('Ctrl Pts',(-30.137146900872,-7.60722015430732,-11.9974593388803)) ;
#62453 = CARTESIAN_POINT('Ctrl Pts',(-30.2512435436636,-8.20056134750055,
-12.0423783485521)) ;
#62454 = CARTESIAN_POINT('Ctrl Pts',(-30.3084518037675,-8.49807959039912,
-12.0649097035758)) ;
#62455 = CARTESIAN_POINT('Ctrl Pts',(-30.4230263411922,-9.0939637382783,-12.1100490952004)) ;
#62456 = CARTESIAN_POINT('Ctrl Pts',(-30.4803926152054,-9.39232964326583,
-12.1326571401055)) ;
#62457 = CARTESIAN_POINT('Ctrl Pts',(-30.6524852649241,-10.2874274064106,
-12.2004967930873)) ;
#62458 = CARTESIAN_POINT('Ctrl Pts',(-30.7672055236576,-10.8841592973239,
-12.2457437718867)) ;
#62459 = CARTESIAN_POINT('Ctrl Pts',(-30.9953308302806,-12.0708421129822,
-12.3357526452282)) ;
#62460 = CARTESIAN_POINT('Ctrl Pts',(-31.1087358495527,-12.6607930377786,
-12.3805146116206)) ;
#62461 = CARTESIAN_POINT('Ctrl Pts',(-31.3329303683718,-13.8271328599994,
-12.4690309217136)) ;
#62462 = CARTESIAN_POINT('Ctrl Pts',(-31.4480866112795,-14.4262400709299,
-12.5145098743794)) ;
#62463 = CARTESIAN_POINT('Ctrl Pts',(-31.5611271543905,-15.0143581154364,
-12.5591632555183)) ;
#62464 = CARTESIAN_POINT('Ctrl Pts',(-31.5654106013656,-15.0366437072152,
-12.5608553212698)) ;
#62465 = CARTESIAN_POINT('Ctrl Pts',(-31.554439204468,-15.0366437072152,-12.5883914511032)) ;
#62466 = CARTESIAN_POINT('Ctrl Pts',(-31.5501658085698,-15.014358115422,-12.5866741590429)) ;
#62467 = CARTESIAN_POINT('Ctrl Pts',(-31.5458893477546,-14.9920565141722,
-12.5849556207893)) ;
#62468 = CARTESIAN_POINT('Ctrl Pts',(-31.4330345428413,-14.4035217573628,
-12.5396034090853)) ;
#62469 = CARTESIAN_POINT('Ctrl Pts',(-31.3225120134546,-13.8271328599263,
-12.4951790208008)) ;
#62470 = CARTESIAN_POINT('Ctrl Pts',(-31.0988751849215,-12.6607930376751,
-12.4052630136179)) ;
#62471 = CARTESIAN_POINT('Ctrl Pts',(-30.9857608721003,-12.0708421128632,
-12.3597714290424)) ;
#62472 = CARTESIAN_POINT('Ctrl Pts',(-30.7582438744036,-10.8841592971741,
-12.2682358154036)) ;
#62473 = CARTESIAN_POINT('Ctrl Pts',(-30.6438411608924,-10.2874274062452,
-12.2221918581842)) ;
#62474 = CARTESIAN_POINT('Ctrl Pts',(-30.4722493803547,-9.39232964307708,
-12.1530951183366)) ;
#62475 = CARTESIAN_POINT('Ctrl Pts',(-30.4150541837849,-9.09396373808178,
-12.1300577014212)) ;
#62476 = CARTESIAN_POINT('Ctrl Pts',(-30.3008312509292,-8.49807959018708,
-12.0840358488622)) ;
#62477 = CARTESIAN_POINT('Ctrl Pts',(-30.2438035113338,-8.20056134728074,
-12.0610514215222)) ;
#62478 = CARTESIAN_POINT('Ctrl Pts',(-30.130079084377,-7.60722015407205,-12.0151982205396)) ;
#62479 = CARTESIAN_POINT('Ctrl Pts',(-30.0733823899492,-7.31139720377296,
-11.9923294646345)) ;
#62480 = CARTESIAN_POINT('Ctrl Pts',(-29.9604840594901,-6.72229422719415,
-11.9467692398571)) ;
#62481 = CARTESIAN_POINT('Ctrl Pts',(-29.9042824091886,-6.42901420088078,
-11.9240778067818)) ;
#62482 = CARTESIAN_POINT('Ctrl Pts',(-29.8204747692394,-5.99163707922339,
-11.890218500157)) ;
#62483 = CARTESIAN_POINT('Ctrl Pts',(-29.7926213691401,-5.84626852614684,
-11.878961687448)) ;
#62484 = CARTESIAN_POINT('Ctrl Pts',(-29.7371002367776,-5.55648501497217,
-11.8565144912627)) ;
#62485 = CARTESIAN_POINT('Ctrl Pts',(-29.7094325040801,-5.41207005687272,
-11.8453241088778)) ;
#62486 = CARTESIAN_POINT('Ctrl Pts',(-29.6543035367715,-5.12429968934209,
-11.8230166504439)) ;
#62487 = CARTESIAN_POINT('Ctrl Pts',(-29.6268422997454,-4.98094427991323,
-11.8118995804582)) ;
#62488 = CARTESIAN_POINT('Ctrl Pts',(-29.5721473378698,-4.69539896394052,
-11.7897451628163)) ;
#62489 = CARTESIAN_POINT('Ctrl Pts',(-29.5449136080874,-4.55320905738164,
-11.7787078275328)) ;
#62490 = CARTESIAN_POINT('Ctrl Pts',(-29.4906949673073,-4.27010070223822,
-11.7567185616112)) ;
#62491 = CARTESIAN_POINT('Ctrl Pts',(-29.4637100466217,-4.129182254563,-11.7457666557959)) ;
#62492 = CARTESIAN_POINT('Ctrl Pts',(-29.4100108324211,-3.84872277413171,
-11.723952672795)) ;
#62493 = CARTESIAN_POINT('Ctrl Pts',(-29.3832965167786,-3.70918174129627,
-11.7130906511012)) ;
#62494 = CARTESIAN_POINT('Ctrl Pts',(-29.3434450791279,-3.5009827220688,-11.6968665288286)) ;
#62495 = CARTESIAN_POINT('Ctrl Pts',(-29.3301979493458,-3.43176847082764,
-11.6914699477771)) ;
#62496 = CARTESIAN_POINT('Ctrl Pts',(-29.3037800722982,-3.29372405730508,
-11.6806995282709)) ;
#62497 = CARTESIAN_POINT('Ctrl Pts',(-29.2906093242772,-3.22489389502025,
-11.6753256917129)) ;
#62498 = CARTESIAN_POINT('Ctrl Pts',(-29.2643474292101,-3.08763090555886,
-11.6646000791918)) ;
#62499 = CARTESIAN_POINT('Ctrl Pts',(-29.2512562762877,-3.01919807839586,
-11.6592483179852)) ;
#62500 = CARTESIAN_POINT('Ctrl Pts',(-29.2251571269213,-2.88274300686055,
-11.6485653291006)) ;
#62501 = CARTESIAN_POINT('Ctrl Pts',(-29.2121491159705,-2.81472076241558,
-11.6432341377916)) ;
#62502 = CARTESIAN_POINT('Ctrl Pts',(-29.1873494579291,-2.68500550281629,
-11.6330527085583)) ;
#62503 = CARTESIAN_POINT('Ctrl Pts',(-29.1749249851303,-2.62000539423729,
-11.6279442950313)) ;
#62504 = CARTESIAN_POINT('Ctrl Pts',(-29.1558514471759,-2.52018397795713,
-11.6200820076069)) ;
#62505 = CARTESIAN_POINT('Ctrl Pts',(-29.1494208071324,-2.48652329705063,
-11.6174279403858)) ;
#62506 = CARTESIAN_POINT('Ctrl Pts',(-29.1364886563188,-2.41881510426724,
-11.6120816988483)) ;
#62507 = CARTESIAN_POINT('Ctrl Pts',(-29.1299871389251,-2.38476759234486,
-11.6093895411308)) ;
#62508 = CARTESIAN_POINT('Ctrl Pts',(-29.1169882561854,-2.31667265961795,
-11.6039948557154)) ;
#62509 = CARTESIAN_POINT('Ctrl Pts',(-29.1104908770745,-2.28262525247775,
-11.601292370194)) ;
#62510 = CARTESIAN_POINT('Ctrl Pts',(-29.1008046681233,-2.23184440710932,
-11.5972504691071)) ;
#62511 = CARTESIAN_POINT('Ctrl Pts',(-29.0975859151669,-2.2149658362827,-11.5959051230648)) ;
#62512 = CARTESIAN_POINT('Ctrl Pts',(-29.0911779605547,-2.18135381364955,
-11.5932212870612)) ;
#62513 = CARTESIAN_POINT('Ctrl Pts',(-29.0879887580595,-2.16462036183514,
-11.5918827992034)) ;
#62514 = CARTESIAN_POINT('Ctrl Pts',(-29.0816496517882,-2.13134694250851,
-11.5892152191654)) ;
#62515 = CARTESIAN_POINT('Ctrl Pts',(-29.0784997421844,-2.1148069788354,-11.5878861437555)) ;
#62516 = CARTESIAN_POINT('Ctrl Pts',(-29.0722492732017,-2.08196890476153,
-11.5852391670673)) ;
#62517 = CARTESIAN_POINT('Ctrl Pts',(-29.0691486959344,-2.06567079415595,
-11.5839213105721)) ;
#62518 = CARTESIAN_POINT('Ctrl Pts',(-29.0645428686228,-2.04144129464998,
-11.5819530171012)) ;
#62519 = CARTESIAN_POINT('Ctrl Pts',(-29.06301510888,-2.03340107341341,-11.5812983108891)) ;
#62520 = CARTESIAN_POINT('Ctrl Pts',(-29.0599760971031,-2.0173992346742,-11.5799913540353)) ;
#62521 = CARTESIAN_POINT('Ctrl Pts',(-29.0584648447653,-2.00943761716704,
-11.5793391041545)) ;
#62522 = CARTESIAN_POINT('Ctrl Pts',(-29.0554605286591,-1.99359903538093,
-11.5780362189339)) ;
#62523 = CARTESIAN_POINT('Ctrl Pts',(-29.0539674543051,-1.98572207127651,
-11.5773856102598)) ;
#62524 = CARTESIAN_POINT('Ctrl Pts',(-29.0517430535571,-1.9739746568621,-11.5764095052018)) ;
#62525 = CARTESIAN_POINT('Ctrl Pts',(-29.0510041261744,-1.97007019078463,
-11.576084093849)) ;
#62526 = CARTESIAN_POINT('Ctrl Pts',(-29.049531697887,-1.96228469444513,-11.5754327366215)) ;
#62527 = CARTESIAN_POINT('Ctrl Pts',(-29.0487981963141,-1.9584036641698,-11.5751067924166)) ;
#62528 = CARTESIAN_POINT('Ctrl Pts',(-29.047336173308,-1.95066098584731,-11.5744532264714)) ;
#62529 = CARTESIAN_POINT('Ctrl Pts',(-29.0465687995152,-1.9465936188602,-11.574108257814)) ;
#62530 = CARTESIAN_POINT('Ctrl Pts',(-29.0449998503682,-1.93826543065782,
-11.573396148711)) ;
#62531 = CARTESIAN_POINT('Ctrl Pts',(-29.0441982478596,-1.93400460876335,
-11.5730290760388)) ;
#62532 = CARTESIAN_POINT('Ctrl Pts',(-29.0429989312286,-1.92761363883573,
-11.5724708657062)) ;
#62533 = CARTESIAN_POINT('Ctrl Pts',(-29.0425996822224,-1.92548337261373,
-11.5722835143255)) ;
#62534 = CARTESIAN_POINT('Ctrl Pts',(-29.0418072269102,-1.92124716215557,
-11.5719072252163)) ;
#62535 = CARTESIAN_POINT('Ctrl Pts',(-29.0414140072555,-1.91914121746326,
-11.5717183207359)) ;
#62536 = CARTESIAN_POINT('Ctrl Pts',(-29.0408327391823,-1.91601870741386,
-11.5714338036012)) ;
#62537 = CARTESIAN_POINT('Ctrl Pts',(-29.0406404150943,-1.91498394237568,
-11.5713387606467)) ;
#62538 = CARTESIAN_POINT('Ctrl Pts',(-29.0402593970723,-1.91292958018145,
-11.5711480324161)) ;
#62539 = CARTESIAN_POINT('Ctrl Pts',(-29.0400707021886,-1.91190998298244,
-11.5710523495)) ;
#62540 = CARTESIAN_POINT('Ctrl Pts',(-29.0396978711363,-1.90988898839402,
-11.5708597036493)) ;
#62541 = CARTESIAN_POINT('Ctrl Pts',(-29.0395137207856,-1.90888759283122,
-11.5707627773289)) ;
#62542 = CARTESIAN_POINT('Ctrl Pts',(-29.039241934621,-1.90740143728902,-11.570615144439)) ;
#62543 = CARTESIAN_POINT('Ctrl Pts',(-29.0391520828946,-1.90690870891373,
-11.5705655503985)) ;
#62544 = CARTESIAN_POINT('Ctrl Pts',(-29.0389741671165,-1.90592895356708,
-11.5704650588555)) ;
#62545 = CARTESIAN_POINT('Ctrl Pts',(-29.0388860939987,-1.90544192594556,
-11.570414183744)) ;
#62546 = CARTESIAN_POINT('Ctrl Pts',(-29.0387544860605,-1.90470902409679,
-11.5703352939177)) ;
#62547 = CARTESIAN_POINT('Ctrl Pts',(-29.0387077267517,-1.90444770690439,
-11.5703067497927)) ;
#62548 = CARTESIAN_POINT('Ctrl Pts',(-29.0386125894249,-1.90391283046634,
-11.5702468890951)) ;
#62549 = CARTESIAN_POINT('Ctrl Pts',(-29.0385642095461,-1.90363927104027,
-11.5702155770922)) ;
#62550 = CARTESIAN_POINT('Ctrl Pts',(-29.0384685129407,-1.90309246508965,
-11.5701504594772)) ;
#62551 = CARTESIAN_POINT('Ctrl Pts',(-29.0384211681404,-1.90281925738603,
-11.5701167460003)) ;
#62552 = CARTESIAN_POINT('Ctrl Pts',(-29.0382419508967,-1.90163369622182,
-11.5699046133964)) ;
#62553 = CARTESIAN_POINT('Ctrl Pts',(-29.0382345917593,-1.90158501392234,
-11.5698959026666)) ;
#62554 = CARTESIAN_POINT('Ctrl Pts',(-29.0382272326218,-1.90153633162286,
-11.5698871919368)) ;
#62555 = CARTESIAN_POINT('',(-33.9221570292818,-15.0366437072151,1.85404835843691)) ;
#62556 = CARTESIAN_POINT('',(-33.9237617799843,-15.0366437072151,1.82445047330719)) ;
#62557 = CARTESIAN_POINT('Origin',(1.36393928288322,-21.6462763158694,-0.0739506391351341)) ;
#62558 = CARTESIAN_POINT('',(-31.2124507867215,-1.90153624137795,1.69228991844779)) ;
#62559 = CARTESIAN_POINT('Ctrl Pts',(-31.2124508052405,-1.90153633118548,
1.69228991969808)) ;
#62560 = CARTESIAN_POINT('Ctrl Pts',(-31.2124604755823,-1.90158488686852,
1.69229690755422)) ;
#62561 = CARTESIAN_POINT('Ctrl Pts',(-31.2126251204459,-1.90241158399461,
1.69241588107553)) ;
#62562 = CARTESIAN_POINT('Ctrl Pts',(-31.212705653647,-1.90280827544799,1.69244478471387)) ;
#62563 = CARTESIAN_POINT('Ctrl Pts',(-31.212760800475,-1.90307912005623,1.69246152971225)) ;
#62564 = CARTESIAN_POINT('Ctrl Pts',(-31.2128713104034,-1.90362119954096,
1.69249252053007)) ;
#62565 = CARTESIAN_POINT('Ctrl Pts',(-31.212926670686,-1.90389239564668,1.69250667032759)) ;
#62566 = CARTESIAN_POINT('Ctrl Pts',(-31.2130349930476,-1.90442265270014,
1.69253287984097)) ;
#62567 = CARTESIAN_POINT('Ctrl Pts',(-31.2130879554519,-1.90468171384137,
1.69254493429805)) ;
#62568 = CARTESIAN_POINT('Ctrl Pts',(-31.2132365506487,-1.90540822375625,
1.69257749175176)) ;
#62569 = CARTESIAN_POINT('Ctrl Pts',(-31.2133353803456,-1.90589098158148,
1.69259746904939)) ;
#62570 = CARTESIAN_POINT('Ctrl Pts',(-31.2135343040682,-1.90686214761777,
1.69263567313032)) ;
#62571 = CARTESIAN_POINT('Ctrl Pts',(-31.2136343995226,-1.90735055647549,
1.69265387603227)) ;
#62572 = CARTESIAN_POINT('Ctrl Pts',(-31.2139364182847,-1.90882368383591,
1.69270669141445)) ;
#62573 = CARTESIAN_POINT('Ctrl Pts',(-31.2141400714612,-1.90981630111776,
1.69273954957263)) ;
#62574 = CARTESIAN_POINT('Ctrl Pts',(-31.214551252172,-1.91181958001539,1.69280268642164)) ;
#62575 = CARTESIAN_POINT('Ctrl Pts',(-31.2147587814458,-1.91283023980567,
1.69283292605898)) ;
#62576 = CARTESIAN_POINT('Ctrl Pts',(-31.2151770468983,-1.91486659457386,
1.69289164979098)) ;
#62577 = CARTESIAN_POINT('Ctrl Pts',(-31.2153877832248,-1.91589228959527,
1.69292013132606)) ;
#62578 = CARTESIAN_POINT('Ctrl Pts',(-31.2160238344561,-1.91898743046011,
1.69300363239075)) ;
#62579 = CARTESIAN_POINT('Ctrl Pts',(-31.2164529859612,-1.9210749168561,1.69305675441327)) ;
#62580 = CARTESIAN_POINT('Ctrl Pts',(-31.2173164601078,-1.92527399853841,
1.69315965094693)) ;
#62581 = CARTESIAN_POINT('Ctrl Pts',(-31.2177507847721,-1.92738559428033,
1.69320938988903)) ;
#62582 = CARTESIAN_POINT('Ctrl Pts',(-31.2190540178841,-1.93372055273571,
1.69335448116223)) ;
#62583 = CARTESIAN_POINT('Ctrl Pts',(-31.2199231709228,-1.93794403361868,
1.69344577335652)) ;
#62584 = CARTESIAN_POINT('Ctrl Pts',(-31.2216223264932,-1.94619923707333,
1.69361846627839)) ;
#62585 = CARTESIAN_POINT('Ctrl Pts',(-31.2224523331006,-1.95023096032421,
1.69369979442831)) ;
#62586 = CARTESIAN_POINT('Ctrl Pts',(-31.2240324597143,-1.95790548170987,
1.69385126692986)) ;
#62587 = CARTESIAN_POINT('Ctrl Pts',(-31.2248245652681,-1.96175219457053,
1.69392541697728)) ;
#62588 = CARTESIAN_POINT('Ctrl Pts',(-31.2264137045607,-1.96946884894499,
1.69407149049838)) ;
#62589 = CARTESIAN_POINT('Ctrl Pts',(-31.2272107384001,-1.97333879047229,
1.69414341216294)) ;
#62590 = CARTESIAN_POINT('Ctrl Pts',(-31.2296089557526,-1.9849823305565,1.69435663218088)) ;
#62591 = CARTESIAN_POINT('Ctrl Pts',(-31.2312172524603,-1.99278964420127,
1.69449543265273)) ;
#62592 = CARTESIAN_POINT('Ctrl Pts',(-31.2344514391384,-2.00848817671179,
1.69476882808044)) ;
#62593 = CARTESIAN_POINT('Ctrl Pts',(-31.2360773306178,-2.01637939540296,
1.69490339453578)) ;
#62594 = CARTESIAN_POINT('Ctrl Pts',(-31.2393453968111,-2.03223974160802,
1.69516959452397)) ;
#62595 = CARTESIAN_POINT('Ctrl Pts',(-31.2409875715695,-2.0402088691264,1.69530122724354)) ;
#62596 = CARTESIAN_POINT('Ctrl Pts',(-31.2459365970091,-2.06422412530555,
1.69569289120128)) ;
#62597 = CARTESIAN_POINT('Ctrl Pts',(-31.2492659426475,-2.08037812413097,
1.6959497894869)) ;
#62598 = CARTESIAN_POINT('Ctrl Pts',(-31.2559745203328,-2.1129258364843,1.69645852467273)) ;
#62599 = CARTESIAN_POINT('Ctrl Pts',(-31.259353755023,-2.12931955021719,1.69671031360131)) ;
#62600 = CARTESIAN_POINT('Ctrl Pts',(-31.2661521113103,-2.16229875913384,
1.69721028915278)) ;
#62601 = CARTESIAN_POINT('Ctrl Pts',(-31.2695712330708,-2.17888425047914,
1.69745845810773)) ;
#62602 = CARTESIAN_POINT('Ctrl Pts',(-31.2764394040602,-2.21219906927763,
1.6979518677282)) ;
#62603 = CARTESIAN_POINT('Ctrl Pts',(-31.2798884534117,-2.22892839673869,
1.69819710615362)) ;
#62604 = CARTESIAN_POINT('Ctrl Pts',(-31.2902655897258,-2.27926022911249,
1.69892882490881)) ;
#62605 = CARTESIAN_POINT('Ctrl Pts',(-31.2972236609703,-2.31300658372593,
1.6994113809596)) ;
#62606 = CARTESIAN_POINT('Ctrl Pts',(-31.3111404252094,-2.38049941138889,
1.70036547765197)) ;
#62607 = CARTESIAN_POINT('Ctrl Pts',(-31.3180991177708,-2.41424587077575,
1.70083697412828)) ;
#62608 = CARTESIAN_POINT('Ctrl Pts',(-31.331937876193,-2.48135537953355,1.70176659803113)) ;
#62609 = CARTESIAN_POINT('Ctrl Pts',(-31.3388179430265,-2.51471842895004,
1.70222470769067)) ;
#62610 = CARTESIAN_POINT('Ctrl Pts',(-31.3592214051958,-2.61365721390697,
1.70357425000709)) ;
#62611 = CARTESIAN_POINT('Ctrl Pts',(-31.3725080558855,-2.67808258579967,
1.70444101111377)) ;
#62612 = CARTESIAN_POINT('Ctrl Pts',(-31.399011920675,-2.80659298322074,1.70615604528631)) ;
#62613 = CARTESIAN_POINT('Ctrl Pts',(-31.412905198914,-2.87395567908353,1.70704657648263)) ;
#62614 = CARTESIAN_POINT('Ctrl Pts',(-31.4407762858584,-3.00908767251738,
1.7088206467358)) ;
#62615 = CARTESIAN_POINT('Ctrl Pts',(-31.4547540966814,-3.07685697016082,
1.7097041470078)) ;
#62616 = CARTESIAN_POINT('Ctrl Pts',(-31.4827913969966,-3.21278904806916,
1.71146667551889)) ;
#62617 = CARTESIAN_POINT('Ctrl Pts',(-31.4968508873389,-3.28095182832054,
1.7123456880226)) ;
#62618 = CARTESIAN_POINT('Ctrl Pts',(-31.5250487430717,-3.41765775368248,
1.71410087761831)) ;
#62619 = CARTESIAN_POINT('Ctrl Pts',(-31.5391871085716,-3.48620089879647,
1.71497705268787)) ;
#62620 = CARTESIAN_POINT('Ctrl Pts',(-31.5817163544578,-3.69238120612899,
1.71760300564436)) ;
#62621 = CARTESIAN_POINT('Ctrl Pts',(-31.6102213782223,-3.83056923968495,
1.71935031957216)) ;
#62622 = CARTESIAN_POINT('Ctrl Pts',(-31.6675138017569,-4.10830936619815,
1.72284371778677)) ;
#62623 = CARTESIAN_POINT('Ctrl Pts',(-31.6963012047564,-4.24786145923466,
1.72458974280963)) ;
#62624 = CARTESIAN_POINT('Ctrl Pts',(-31.7541365245639,-4.52822477707554,
1.72808325781092)) ;
#62625 = CARTESIAN_POINT('Ctrl Pts',(-31.7831844426181,-4.66903600097254,
1.72983072133869)) ;
#62626 = CARTESIAN_POINT('Ctrl Pts',(-31.8415190007151,-4.95181265093575,
1.73332850241756)) ;
#62627 = CARTESIAN_POINT('Ctrl Pts',(-31.8708056414777,-5.09377807701703,
1.7350788067485)) ;
#62628 = CARTESIAN_POINT('Ctrl Pts',(-31.9295958955513,-5.3787582045011,1.73858288735192)) ;
#62629 = CARTESIAN_POINT('Ctrl Pts',(-31.9590995092129,-5.52177290590162,
1.74033665714628)) ;
#62630 = CARTESIAN_POINT('Ctrl Pts',(-32.0183019863142,-5.80874665766087,
1.74384779656397)) ;
#62631 = CARTESIAN_POINT('Ctrl Pts',(-32.0480008498168,-5.95270570802092,
1.74560516501718)) ;
#62632 = CARTESIAN_POINT('Ctrl Pts',(-32.1373577569072,-6.38584199350258,
1.75088238301387)) ;
#62633 = CARTESIAN_POINT('Ctrl Pts',(-32.1972761119937,-6.67627835833736,
1.75440742104842)) ;
#62634 = CARTESIAN_POINT('Ctrl Pts',(-32.3176334772365,-7.25966935591344,
1.76146731493516)) ;
#62635 = CARTESIAN_POINT('Ctrl Pts',(-32.3780724894743,-7.55262398868834,
1.76500213252553)) ;
#62636 = CARTESIAN_POINT('Ctrl Pts',(-32.4992977674486,-8.14021210947855,
1.77207558219639)) ;
#62637 = CARTESIAN_POINT('Ctrl Pts',(-32.5600840342126,-8.43484559749056,
1.77561419531164)) ;
#62638 = CARTESIAN_POINT('Ctrl Pts',(-32.6818304790745,-9.02495201690094,
1.78268814011636)) ;
#62639 = CARTESIAN_POINT('Ctrl Pts',(-32.7427906576548,-9.32042494830625,
1.7862234629264)) ;
#62640 = CARTESIAN_POINT('Ctrl Pts',(-32.9256721036102,-10.2068437906719,
1.79681282728755)) ;
#62641 = CARTESIAN_POINT('Ctrl Pts',(-33.0475942695293,-10.7977897343697,
1.80385042107764)) ;
#62642 = CARTESIAN_POINT('Ctrl Pts',(-33.2900548260716,-11.9729664049461,
1.81781450787256)) ;
#62643 = CARTESIAN_POINT('Ctrl Pts',(-33.4105932208701,-12.5571971318763,
1.82474092404302)) ;
#62644 = CARTESIAN_POINT('Ctrl Pts',(-33.6489002671063,-13.7122280571188,
1.83841163542805)) ;
#62645 = CARTESIAN_POINT('Ctrl Pts',(-33.766668920533,-14.2830282554284,1.84515589394605)) ;
#62646 = CARTESIAN_POINT('Ctrl Pts',(-33.8956533090018,-14.9081862857511,
1.85253287884652)) ;
#62647 = CARTESIAN_POINT('Ctrl Pts',(-33.9089194116541,-14.9724840414645,
1.85329148954973)) ;
#62648 = CARTESIAN_POINT('Ctrl Pts',(-33.9221570292297,-15.0366437072146,
1.85404835938948)) ;
#62649 = CARTESIAN_POINT('Ctrl Pts',(-33.9237617800355,-15.0366437072146,
1.82445047235329)) ;
#62650 = CARTESIAN_POINT('Ctrl Pts',(-33.910519929938,-14.972484041565,1.82377166717211)) ;
#62651 = CARTESIAN_POINT('Ctrl Pts',(-33.897249573524,-14.9081862859525,1.82309151287087)) ;
#62652 = CARTESIAN_POINT('Ctrl Pts',(-33.7682237047426,-14.2830282558342,
1.81647958809875)) ;
#62653 = CARTESIAN_POINT('Ctrl Pts',(-33.6504162336189,-13.7122280576294,
1.81045128027728)) ;
#62654 = CARTESIAN_POINT('Ctrl Pts',(-33.4120280896458,-12.557197132599,1.7982763294461)) ;
#62655 = CARTESIAN_POINT('Ctrl Pts',(-33.2914474187869,-11.9729664057762,
1.79212964973725)) ;
#62656 = CARTESIAN_POINT('Ctrl Pts',(-33.0488983931026,-10.7977897354156,
1.77979728107933)) ;
#62657 = CARTESIAN_POINT('Ctrl Pts',(-32.9269300424333,-10.2068437918263,
1.77361151529792)) ;
#62658 = CARTESIAN_POINT('Ctrl Pts',(-32.7439757437029,-9.3204249496235,1.76436584192825)) ;
#62659 = CARTESIAN_POINT('Ctrl Pts',(-32.6829906806809,-9.02495201827243,
1.76128948584647)) ;
#62660 = CARTESIAN_POINT('Ctrl Pts',(-32.5611930907488,-8.43484559897041,
1.75515885676957)) ;
#62661 = CARTESIAN_POINT('Ctrl Pts',(-32.5003805643192,-8.14021211101255,
1.75210457489359)) ;
#62662 = CARTESIAN_POINT('Ctrl Pts',(-32.3791011397054,-7.55262399033026,
1.74602980163758)) ;
#62663 = CARTESIAN_POINT('Ctrl Pts',(-32.31863424255,-7.25966935760917,1.74300929129468)) ;
#62664 = CARTESIAN_POINT('Ctrl Pts',(-32.1982191085639,-6.67627836014022,
1.73701487959174)) ;
#62665 = CARTESIAN_POINT('Ctrl Pts',(-32.1382708738013,-6.38584199535877,
1.7340409399602)) ;
#62666 = CARTESIAN_POINT('Ctrl Pts',(-32.0488672131155,-5.95270570995667,
1.729626041596)) ;
#62667 = CARTESIAN_POINT('Ctrl Pts',(-32.0191524406759,-5.80874665962307,
1.72816209632065)) ;
#62668 = CARTESIAN_POINT('Ctrl Pts',(-31.9599173900955,-5.52177290791652,
1.72525173957642)) ;
#62669 = CARTESIAN_POINT('Ctrl Pts',(-31.9303971120183,-5.37875820654228,
1.72380532694195)) ;
#62670 = CARTESIAN_POINT('Ctrl Pts',(-31.8715726311884,-5.09377807911053,
1.7209325219118)) ;
#62671 = CARTESIAN_POINT('Ctrl Pts',(-31.8422684287877,-4.95181265305536,
1.71950612303628)) ;
#62672 = CARTESIAN_POINT('Ctrl Pts',(-31.7838976537235,-4.66903600314406,
1.71667632481136)) ;
#62673 = CARTESIAN_POINT('Ctrl Pts',(-31.7548310817732,-4.52822477927292,
1.71527291224978)) ;
#62674 = CARTESIAN_POINT('Ctrl Pts',(-31.6969570796863,-4.24786146148353,
1.71249285010884)) ;
#62675 = CARTESIAN_POINT('Ctrl Pts',(-31.6681496511704,-4.10830936847265,
1.71111617410036)) ;
#62676 = CARTESIAN_POINT('Ctrl Pts',(-31.610815375502,-3.83056924201046,1.70839469326928)) ;
#62677 = CARTESIAN_POINT('Ctrl Pts',(-31.5822885315467,-3.6923812084799,1.70704982917742)) ;
#62678 = CARTESIAN_POINT('Ctrl Pts',(-31.5397246784737,-3.48620090118523,
1.70506216836613)) ;
#62679 = CARTESIAN_POINT('Ctrl Pts',(-31.5255744614924,-3.41765775608383,
1.70440458105773)) ;
#62680 = CARTESIAN_POINT('Ctrl Pts',(-31.497352133427,-3.28095183074698,1.70310075717327)) ;
#62681 = CARTESIAN_POINT('Ctrl Pts',(-31.4832800224533,-3.21278905050812,
1.70245451856732)) ;
#62682 = CARTESIAN_POINT('Ctrl Pts',(-31.4552165151465,-3.07685697262473,
1.70117534967155)) ;
#62683 = CARTESIAN_POINT('Ctrl Pts',(-31.4412251196694,-3.00908767499377,
1.70054240364651)) ;
#62684 = CARTESIAN_POINT('Ctrl Pts',(-31.4133256035017,-2.87395568158474,
1.69929267966148)) ;
#62685 = CARTESIAN_POINT('Ctrl Pts',(-31.3994174848983,-2.80659298573433,
1.69867586292556)) ;
#62686 = CARTESIAN_POINT('Ctrl Pts',(-31.3728835590771,-2.67808258825811,
1.69751527164832)) ;
#62687 = CARTESIAN_POINT('Ctrl Pts',(-31.3595810819296,-2.61365721629451,
1.6969404121094)) ;
#62688 = CARTESIAN_POINT('Ctrl Pts',(-31.3391513145168,-2.51471843122878,
1.69607604104657)) ;
#62689 = CARTESIAN_POINT('Ctrl Pts',(-31.3322620485548,-2.48135538177564,
1.69578759918871)) ;
#62690 = CARTESIAN_POINT('Ctrl Pts',(-31.3184039034883,-2.41424587294404,
1.69521554061912)) ;
#62691 = CARTESIAN_POINT('Ctrl Pts',(-31.3114350253373,-2.38049941352006,
1.69493190614639)) ;
#62692 = CARTESIAN_POINT('Ctrl Pts',(-31.2974966857533,-2.31300658578286,
1.69437574299248)) ;
#62693 = CARTESIAN_POINT('Ctrl Pts',(-31.2905272295257,-2.27926023113236,
1.69410317045799)) ;
#62694 = CARTESIAN_POINT('Ctrl Pts',(-31.2801318117043,-2.2289283987032,1.69370863405332)) ;
#62695 = CARTESIAN_POINT('Ctrl Pts',(-31.276676465886,-2.21219907122377,1.69357952705449)) ;
#62696 = CARTESIAN_POINT('Ctrl Pts',(-31.2697952094378,-2.17888425238866,
1.69332746438019)) ;
#62697 = CARTESIAN_POINT('Ctrl Pts',(-31.2663692989285,-2.16229876102506,
1.69320450646045)) ;
#62698 = CARTESIAN_POINT('Ctrl Pts',(-31.2595567380237,-2.12931955207216,
1.69296651952424)) ;
#62699 = CARTESIAN_POINT('Ctrl Pts',(-31.2561700893765,-2.11292583832124,
1.69285147291781)) ;
#62700 = CARTESIAN_POINT('Ctrl Pts',(-31.2494458337047,-2.08037812593213,
1.69263190104062)) ;
#62701 = CARTESIAN_POINT('Ctrl Pts',(-31.246108229238,-2.06422412708902,1.69252732781365)) ;
#62702 = CARTESIAN_POINT('Ctrl Pts',(-31.2411458688696,-2.04020887088343,
1.69238161204554)) ;
#62703 = CARTESIAN_POINT('Ctrl Pts',(-31.2394990886085,-2.0322397433562,1.69233492279027)) ;
#62704 = CARTESIAN_POINT('Ctrl Pts',(-31.2362213986742,-2.01637939713371,
1.69224622219386)) ;
#62705 = CARTESIAN_POINT('Ctrl Pts',(-31.234590489045,-2.00848817843392,1.69220421003294)) ;
#62706 = CARTESIAN_POINT('Ctrl Pts',(-31.2313457020589,-1.99278964590612,
1.6921263257159)) ;
#62707 = CARTESIAN_POINT('Ctrl Pts',(-31.2297318262819,-1.98498233225289,
1.69209042508881)) ;
#62708 = CARTESIAN_POINT('Ctrl Pts',(-31.2273246142407,-1.97333879215588,
1.6920431022953)) ;
#62709 = CARTESIAN_POINT('Ctrl Pts',(-31.2265244765495,-1.96946885062398,
1.69202842779028)) ;
#62710 = CARTESIAN_POINT('Ctrl Pts',(-31.2249288595321,-1.96175219624107,
1.69200182884216)) ;
#62711 = CARTESIAN_POINT('Ctrl Pts',(-31.2241333803023,-1.95790548337636,
1.69198990257096)) ;
#62712 = CARTESIAN_POINT('Ctrl Pts',(-31.2225461393377,-1.95023096168779,
1.69196964539493)) ;
#62713 = CARTESIAN_POINT('Ctrl Pts',(-31.2217122050812,-1.94619923812308,
1.69196075727152)) ;
#62714 = CARTESIAN_POINT('Ctrl Pts',(-31.2200043385117,-1.93794403402632,
1.6919487268236)) ;
#62715 = CARTESIAN_POINT('Ctrl Pts',(-31.2191304099921,-1.93372055281537,
1.69194551194037)) ;
#62716 = CARTESIAN_POINT('Ctrl Pts',(-31.2178191292608,-1.92738559386717,
1.6919488483903)) ;
#62717 = CARTESIAN_POINT('Ctrl Pts',(-31.2173819728692,-1.92527399796036,
1.69195133695555)) ;
#62718 = CARTESIAN_POINT('Ctrl Pts',(-31.2165124353052,-1.92107491595138,
1.69196027232917)) ;
#62719 = CARTESIAN_POINT('Ctrl Pts',(-31.2160800559731,-1.91898742939227,
1.69196668344944)) ;
#62720 = CARTESIAN_POINT('Ctrl Pts',(-31.2154387051982,-1.91589228828676,
1.69198092579564)) ;
#62721 = CARTESIAN_POINT('Ctrl Pts',(-31.2152261248002,-1.91486659318724,
1.69198645586048)) ;
#62722 = CARTESIAN_POINT('Ctrl Pts',(-31.2148039620526,-1.91283023826074,
1.69199961290183)) ;
#62723 = CARTESIAN_POINT('Ctrl Pts',(-31.2145943798285,-1.91181957839179,
1.6920072374057)) ;
#62724 = CARTESIAN_POINT('Ctrl Pts',(-31.2141787831505,-1.90981629933822,
1.69202554768463)) ;
#62725 = CARTESIAN_POINT('Ctrl Pts',(-31.2139727711923,-1.90882368197796,
1.69203619439398)) ;
#62726 = CARTESIAN_POINT('Ctrl Pts',(-31.2136668125056,-1.90735055450323,
1.69205604620806)) ;
#62727 = CARTESIAN_POINT('Ctrl Pts',(-31.2135653357217,-1.90686214561062,
1.69206332029631)) ;
#62728 = CARTESIAN_POINT('Ctrl Pts',(-31.2133634474945,-1.90589097949916,
1.69207979299927)) ;
#62729 = CARTESIAN_POINT('Ctrl Pts',(-31.2132630372143,-1.90540822163286,
1.69208896768993)) ;
#62730 = CARTESIAN_POINT('Ctrl Pts',(-31.2131117930028,-1.90468171168872,
1.6921052683243)) ;
#62731 = CARTESIAN_POINT('Ctrl Pts',(-31.2130578377534,-1.9044226505553,1.69211152584795)) ;
#62732 = CARTESIAN_POINT('Ctrl Pts',(-31.2129473166385,-1.90389239352006,
1.69212587002178)) ;
#62733 = CARTESIAN_POINT('Ctrl Pts',(-31.2128907510105,-1.90362119743088,
1.69213395157609)) ;
#62734 = CARTESIAN_POINT('Ctrl Pts',(-31.212777538204,-1.90307911796257,1.69215281247392)) ;
#62735 = CARTESIAN_POINT('Ctrl Pts',(-31.2127209042014,-1.90280827335977,
1.69216349681887)) ;
#62736 = CARTESIAN_POINT('Ctrl Pts',(-31.2124714797407,-1.90163369094096,
1.69228024276397)) ;
#62737 = CARTESIAN_POINT('Ctrl Pts',(-31.2124611424906,-1.90158501106322,
1.69228508123103)) ;
#62738 = CARTESIAN_POINT('Ctrl Pts',(-31.2124508052405,-1.90153633118548,
1.69228991969808)) ;
#62739 = CARTESIAN_POINT('',(-30.0084212027444,-15.0366437072153,15.9262327545894)) ;
#62740 = CARTESIAN_POINT('',(-30.0223054639863,-15.0366437072153,15.9000442597427)) ;
#62741 = CARTESIAN_POINT('Origin',(1.20682669964218,-21.6462763158694,-0.639819022420596)) ;
#62742 = CARTESIAN_POINT('',(-27.6170790284909,-1.90153624302636,14.6416486516027)) ;
#62743 = CARTESIAN_POINT('Ctrl Pts',(-27.617079045072,-1.9015363344823,14.6416486606773)) ;
#62744 = CARTESIAN_POINT('Ctrl Pts',(-27.6170849036807,-1.90158489434699,
14.6416590345023)) ;
#62745 = CARTESIAN_POINT('Ctrl Pts',(-27.6171857446532,-1.90242072828766,
14.641837593382)) ;
#62746 = CARTESIAN_POINT('Ctrl Pts',(-27.6172474058173,-1.90282163229673,
14.6418981646337)) ;
#62747 = CARTESIAN_POINT('Ctrl Pts',(-27.617290915074,-1.90309535072763,14.6419368604685)) ;
#62748 = CARTESIAN_POINT('Ctrl Pts',(-27.6173791857354,-1.90364317822138,
14.642012062681)) ;
#62749 = CARTESIAN_POINT('Ctrl Pts',(-27.6174239850381,-1.90391724844841,
14.6420484804412)) ;
#62750 = CARTESIAN_POINT('Ctrl Pts',(-27.6175122659352,-1.90445312328647,
14.6421183899042)) ;
#62751 = CARTESIAN_POINT('Ctrl Pts',(-27.6175557499699,-1.90471492808516,
14.6421518770866)) ;
#62752 = CARTESIAN_POINT('Ctrl Pts',(-27.6176782981338,-1.90544921113751,
14.6422446881917)) ;
#62753 = CARTESIAN_POINT('Ctrl Pts',(-27.6177605162274,-1.90593716129565,
14.6423048892218)) ;
#62754 = CARTESIAN_POINT('Ctrl Pts',(-27.6179268505096,-1.9069187724624,14.6424242306893)) ;
#62755 = CARTESIAN_POINT('Ctrl Pts',(-27.6180109781392,-1.90741243412097,
14.6424833498336)) ;
#62756 = CARTESIAN_POINT('Ctrl Pts',(-27.6182657067604,-1.90890140455296,
14.6426598058831)) ;
#62757 = CARTESIAN_POINT('Ctrl Pts',(-27.6184386345518,-1.90990469676427,
14.6427762762253)) ;
#62758 = CARTESIAN_POINT('Ctrl Pts',(-27.6187891319733,-1.91192951903267,
14.6430085079058)) ;
#62759 = CARTESIAN_POINT('Ctrl Pts',(-27.6189667196568,-1.912951047262,14.6431242343853)) ;
#62760 = CARTESIAN_POINT('Ctrl Pts',(-27.6193255770666,-1.91500930016886,
14.6433554468608)) ;
#62761 = CARTESIAN_POINT('Ctrl Pts',(-27.6195068479783,-1.91604602488884,
14.6434709306392)) ;
#62762 = CARTESIAN_POINT('Ctrl Pts',(-27.6200550047461,-1.91917444836702,
14.6438172397545)) ;
#62763 = CARTESIAN_POINT('Ctrl Pts',(-27.6204262100252,-1.9212843811877,14.6440479625586)) ;
#62764 = CARTESIAN_POINT('Ctrl Pts',(-27.6211747756337,-1.92552861374704,
14.6445085490547)) ;
#62765 = CARTESIAN_POINT('Ctrl Pts',(-27.621552152844,-1.92766291394181,14.6447383811071)) ;
#62766 = CARTESIAN_POINT('Ctrl Pts',(-27.6226862623404,-1.93406598579517,
14.645424222177)) ;
#62767 = CARTESIAN_POINT('Ctrl Pts',(-27.6234449317066,-1.9383348756467,14.6458766296199)) ;
#62768 = CARTESIAN_POINT('Ctrl Pts',(-27.6249305344079,-1.94667883304679,
14.6467557917244)) ;
#62769 = CARTESIAN_POINT('Ctrl Pts',(-27.6256575020925,-1.95075390127448,
14.6471824818955)) ;
#62770 = CARTESIAN_POINT('Ctrl Pts',(-27.6270429511285,-1.95851130668981,
14.6479917704875)) ;
#62771 = CARTESIAN_POINT('Ctrl Pts',(-27.6277382519714,-1.96239975264163,
14.6483958539826)) ;
#62772 = CARTESIAN_POINT('Ctrl Pts',(-27.6291343137498,-1.97020012509417,
14.649204081629)) ;
#62773 = CARTESIAN_POINT('Ctrl Pts',(-27.6298350755349,-1.97411205160832,
14.6496082241834)) ;
#62774 = CARTESIAN_POINT('Ctrl Pts',(-27.6319449619627,-1.98588191230647,
14.6508213511136)) ;
#62775 = CARTESIAN_POINT('Ctrl Pts',(-27.633361665421,-1.99377392723216,14.6516310765538)) ;
#62776 = CARTESIAN_POINT('Ctrl Pts',(-27.6362129847788,-2.00964277237373,
14.6532541610047)) ;
#62777 = CARTESIAN_POINT('Ctrl Pts',(-27.6376476141085,-2.01761960241516,
14.6540674946062)) ;
#62778 = CARTESIAN_POINT('Ctrl Pts',(-27.6405330465774,-2.03365201638472,
14.6556984005312)) ;
#62779 = CARTESIAN_POINT('Ctrl Pts',(-27.6419838501062,-2.04170760031738,
14.656515972121)) ;
#62780 = CARTESIAN_POINT('Ctrl Pts',(-27.6463582652038,-2.06598339582831,
14.6589752914403)) ;
#62781 = CARTESIAN_POINT('Ctrl Pts',(-27.6493038328558,-2.08231264765909,
14.660623733535)) ;
#62782 = CARTESIAN_POINT('Ctrl Pts',(-27.6552428635702,-2.11521346622004,
14.6639371853392)) ;
#62783 = CARTESIAN_POINT('Ctrl Pts',(-27.6582363492858,-2.13178503315512,
14.6656021524101)) ;
#62784 = CARTESIAN_POINT('Ctrl Pts',(-27.6642614280585,-2.16512202863509,
14.6689457391089)) ;
#62785 = CARTESIAN_POINT('Ctrl Pts',(-27.6672930287337,-2.1818874533408,14.6706243426738)) ;
#62786 = CARTESIAN_POINT('Ctrl Pts',(-27.6733849174245,-2.21556369897872,
14.6739915877195)) ;
#62787 = CARTESIAN_POINT('Ctrl Pts',(-27.6764452065005,-2.23247451991884,
14.6756802272031)) ;
#62788 = CARTESIAN_POINT('Ctrl Pts',(-27.6856552674657,-2.28335239284995,
14.6807552345299)) ;
#62789 = CARTESIAN_POINT('Ctrl Pts',(-27.6918341989637,-2.31746485466174,
14.6841507554935)) ;
#62790 = CARTESIAN_POINT('Ctrl Pts',(-27.704197279302,-2.38568989673412,14.6909320087283)) ;
#62791 = CARTESIAN_POINT('Ctrl Pts',(-27.7103814464014,-2.41980246332999,
14.69431770053)) ;
#62792 = CARTESIAN_POINT('Ctrl Pts',(-27.7226832977556,-2.48764002620402,
14.7010434902844)) ;
#62793 = CARTESIAN_POINT('Ctrl Pts',(-27.7288009903973,-2.5213650225277,14.7043835724376)) ;
#62794 = CARTESIAN_POINT('Ctrl Pts',(-27.7469473693318,-2.62137716728801,
14.7142806543689)) ;
#62795 = CARTESIAN_POINT('Ctrl Pts',(-27.7587693022826,-2.68650147115872,
14.7207145919794)) ;
#62796 = CARTESIAN_POINT('Ctrl Pts',(-27.7823702026186,-2.81647723714774,
14.733543132641)) ;
#62797 = CARTESIAN_POINT('Ctrl Pts',(-27.7947515322033,-2.88464215120766,
14.7402634360118)) ;
#62798 = CARTESIAN_POINT('Ctrl Pts',(-27.8195947676845,-3.02138342310543,
14.753733586337)) ;
#62799 = CARTESIAN_POINT('Ctrl Pts',(-27.8320566919655,-3.08995978101598,
14.7604833986468)) ;
#62800 = CARTESIAN_POINT('Ctrl Pts',(-27.857057432086,-3.22751066532536,14.7740136600503)) ;
#62801 = CARTESIAN_POINT('Ctrl Pts',(-27.8695962553744,-3.29648519171056,
14.7807940950877)) ;
#62802 = CARTESIAN_POINT('Ctrl Pts',(-27.8947475269405,-3.43481913900766,
14.7943859069561)) ;
#62803 = CARTESIAN_POINT('Ctrl Pts',(-27.9073599761762,-3.50417855992295,
14.8011972819796)) ;
#62804 = CARTESIAN_POINT('Ctrl Pts',(-27.9453032278437,-3.71281425486547,
14.8216775868742)) ;
#62805 = CARTESIAN_POINT('Ctrl Pts',(-27.9707398829137,-3.85264796043412,
14.8353927930809)) ;
#62806 = CARTESIAN_POINT('Ctrl Pts',(-28.0218730017821,-4.13369567528339,
14.8629421363133)) ;
#62807 = CARTESIAN_POINT('Ctrl Pts',(-28.047569493618,-4.27490968464348,14.8767762204895)) ;
#62808 = CARTESIAN_POINT('Ctrl Pts',(-28.0992010723601,-4.5586118298814,14.9045564880959)) ;
#62809 = CARTESIAN_POINT('Ctrl Pts',(-28.125136171597,-4.70109996484956,14.9185026478667)) ;
#62810 = CARTESIAN_POINT('Ctrl Pts',(-28.1772243679445,-4.98724418213772,
14.946499071459)) ;
#62811 = CARTESIAN_POINT('Ctrl Pts',(-28.2033774713037,-5.13090026447277,
14.9605493235009)) ;
#62812 = CARTESIAN_POINT('Ctrl Pts',(-28.255881443487,-5.41927420008585,14.9887452495852)) ;
#62813 = CARTESIAN_POINT('Ctrl Pts',(-28.2822323153732,-5.56399205336157,
15.0028909178505)) ;
#62814 = CARTESIAN_POINT('Ctrl Pts',(-28.3351118237506,-5.85438335493212,
15.0312685577992)) ;
#62815 = CARTESIAN_POINT('Ctrl Pts',(-28.361640460793,-6.00005680322832,15.0455005284421)) ;
#62816 = CARTESIAN_POINT('Ctrl Pts',(-28.4414632438374,-6.43835127726969,
15.0883117910004)) ;
#62817 = CARTESIAN_POINT('Ctrl Pts',(-28.4949942250459,-6.73224642747102,
15.1170065007152)) ;
#62818 = CARTESIAN_POINT('Ctrl Pts',(-28.602530121798,-7.32258498527443,15.17462626168)) ;
#62819 = CARTESIAN_POINT('Ctrl Pts',(-28.6565350554198,-7.61902839291019,
15.2035512788457)) ;
#62820 = CARTESIAN_POINT('Ctrl Pts',(-28.7648621679001,-8.21361405642605,
15.2615524472652)) ;
#62821 = CARTESIAN_POINT('Ctrl Pts',(-28.819184355712,-8.5117563123029,15.2906285816295)) ;
#62822 = CARTESIAN_POINT('Ctrl Pts',(-28.9279898034778,-9.10889026395786,
15.3488518040726)) ;
#62823 = CARTESIAN_POINT('Ctrl Pts',(-28.9824730676241,-9.40788195974288,
15.3779988842453)) ;
#62824 = CARTESIAN_POINT('Ctrl Pts',(-29.145930698864,-10.3048570952872,15.4654253604834)) ;
#62825 = CARTESIAN_POINT('Ctrl Pts',(-29.2549128280494,-10.9028405678066,
15.5236901301374)) ;
#62826 = CARTESIAN_POINT('Ctrl Pts',(-29.4716533430531,-12.0920123241697,
15.6395298961061)) ;
#62827 = CARTESIAN_POINT('Ctrl Pts',(-29.5794117651472,-12.683200608065,15.6971048240178)) ;
#62828 = CARTESIAN_POINT('Ctrl Pts',(-29.7949448266547,-13.8656062560031,
15.8122369207257)) ;
#62829 = CARTESIAN_POINT('Ctrl Pts',(-29.9026613337374,-14.4565031969479,
15.8697623699)) ;
#62830 = CARTESIAN_POINT('Ctrl Pts',(-30.00842120271,-15.0366437072152,15.9262327546544)) ;
#62831 = CARTESIAN_POINT('Ctrl Pts',(-30.0223054640204,-15.0366437072153,
15.9000442596783)) ;
#62832 = CARTESIAN_POINT('Ctrl Pts',(-30.0198892745065,-15.0234311858862,
15.8987723880774)) ;
#62833 = CARTESIAN_POINT('Ctrl Pts',(-30.017472062495,-15.0102130853408,15.8974999835935)) ;
#62834 = CARTESIAN_POINT('Ctrl Pts',(-29.9112916285261,-14.4295845144665,
15.8416075390388)) ;
#62835 = CARTESIAN_POINT('Ctrl Pts',(-29.8056613310825,-13.8519867028476,
15.7860145804868)) ;
#62836 = CARTESIAN_POINT('Ctrl Pts',(-29.5919042492259,-12.6832006072026,
15.6735414990053)) ;
#62837 = CARTESIAN_POINT('Ctrl Pts',(-29.4837774821379,-12.0920123231792,
15.6166613433989)) ;
#62838 = CARTESIAN_POINT('Ctrl Pts',(-29.2662662086894,-10.9028405665586,
15.5022753819669)) ;
#62839 = CARTESIAN_POINT('Ctrl Pts',(-29.1568817385884,-10.3048570939097,
15.4447695077282)) ;
#62840 = CARTESIAN_POINT('Ctrl Pts',(-28.9927894976363,-9.40788195817102,
15.3585400323025)) ;
#62841 = CARTESIAN_POINT('Ctrl Pts',(-28.9380894769186,-9.10889026232123,
15.3298017983665)) ;
#62842 = CARTESIAN_POINT('Ctrl Pts',(-28.8288385463144,-8.51175631053695,
15.2724188456376)) ;
#62843 = CARTESIAN_POINT('Ctrl Pts',(-28.7742876406181,-8.21361405459552,
15.2437741189394)) ;
#62844 = CARTESIAN_POINT('Ctrl Pts',(-28.6654889372615,-7.61902839095087,
15.186662465218)) ;
#62845 = CARTESIAN_POINT('Ctrl Pts',(-28.6112411485568,-7.32258498325092,
15.158195521304)) ;
#62846 = CARTESIAN_POINT('Ctrl Pts',(-28.503202151987,-6.73224642531964,15.1015247072058)) ;
#62847 = CARTESIAN_POINT('Ctrl Pts',(-28.4494109621869,-6.43835127505464,
15.0733208029325)) ;
#62848 = CARTESIAN_POINT('Ctrl Pts',(-28.369181037787,-6.00005680091835,15.0312774903949)) ;
#62849 = CARTESIAN_POINT('Ctrl Pts',(-28.3425138642898,-5.85438335259064,
15.0173068272121)) ;
#62850 = CARTESIAN_POINT('Ctrl Pts',(-28.289350707775,-5.56399205095715,14.9894642043788)) ;
#62851 = CARTESIAN_POINT('Ctrl Pts',(-28.2628547253106,-5.41927419765009,
14.9755922436859)) ;
#62852 = CARTESIAN_POINT('Ctrl Pts',(-28.2100527174169,-5.13090026197456,
14.9479584725587)) ;
#62853 = CARTESIAN_POINT('Ctrl Pts',(-28.1837466950485,-4.9872441796084,14.9341966563524)) ;
#62854 = CARTESIAN_POINT('Ctrl Pts',(-28.1313431411937,-4.70109996225825,
14.9067950600924)) ;
#62855 = CARTESIAN_POINT('Ctrl Pts',(-28.1052456159516,-4.55861182725925,
14.8931552682541)) ;
#62856 = CARTESIAN_POINT('Ctrl Pts',(-28.0532772199223,-4.27490968195984,
14.866010305419)) ;
#62857 = CARTESIAN_POINT('Ctrl Pts',(-28.0274063617978,-4.13369567256921,
14.8525051109391)) ;
#62858 = CARTESIAN_POINT('Ctrl Pts',(-27.975908828566,-3.85264795765906,14.825643126086)) ;
#62859 = CARTESIAN_POINT('Ctrl Pts',(-27.9502821814665,-3.71281425206012,
14.8122862828497)) ;
#62860 = CARTESIAN_POINT('Ctrl Pts',(-27.9120375963644,-3.50417855707243,
14.7923743530876)) ;
#62861 = CARTESIAN_POINT('Ctrl Pts',(-27.8993219528192,-3.43481913614209,
14.7857576231735)) ;
#62862 = CARTESIAN_POINT('Ctrl Pts',(-27.8739575913849,-3.29648518881505,
14.7725677414212)) ;
#62863 = CARTESIAN_POINT('Ctrl Pts',(-27.8613088744532,-3.22751066241491,
14.7659945877775)) ;
#62864 = CARTESIAN_POINT('Ctrl Pts',(-27.8360799339616,-3.08995977807574,
14.7528947579221)) ;
#62865 = CARTESIAN_POINT('Ctrl Pts',(-27.823499717855,-3.02138342015034,14.7463680676582)) ;
#62866 = CARTESIAN_POINT('Ctrl Pts',(-27.7984089202078,-2.88464214822294,
14.7333648691004)) ;
#62867 = CARTESIAN_POINT('Ctrl Pts',(-27.7858983570277,-2.81647723414827,
14.7268883261428)) ;
#62868 = CARTESIAN_POINT('Ctrl Pts',(-27.7620357951218,-2.68650146849467,
14.7145533317067)) ;
#62869 = CARTESIAN_POINT('Ctrl Pts',(-27.7500761799523,-2.62137716499163,
14.7083790904721)) ;
#62870 = CARTESIAN_POINT('Ctrl Pts',(-27.7317009610864,-2.52136502079594,
14.6989136466899)) ;
#62871 = CARTESIAN_POINT('Ctrl Pts',(-27.7255032418861,-2.48764002466267,
14.695724510723)) ;
#62872 = CARTESIAN_POINT('Ctrl Pts',(-27.7130327399128,-2.41980246217161,
14.6893168299511)) ;
#62873 = CARTESIAN_POINT('Ctrl Pts',(-27.7067599655119,-2.3856898957683,14.6860982693346)) ;
#62874 = CARTESIAN_POINT('Ctrl Pts',(-27.6942091961128,-2.31746485408108,
14.6796710353937)) ;
#62875 = CARTESIAN_POINT('Ctrl Pts',(-27.687931224366,-2.28335239246188,14.6764623242415)) ;
#62876 = CARTESIAN_POINT('Ctrl Pts',(-27.6785621296037,-2.232474519818,14.6716872866043)) ;
#62877 = CARTESIAN_POINT('Ctrl Pts',(-27.675447066653,-2.21556369897336,14.6701019616504)) ;
#62878 = CARTESIAN_POINT('Ctrl Pts',(-27.6692413458727,-2.18188745352556,
14.6669494267863)) ;
#62879 = CARTESIAN_POINT('Ctrl Pts',(-27.6661506891041,-2.16512202891445,
14.6653822148722)) ;
#62880 = CARTESIAN_POINT('Ctrl Pts',(-27.6600020429387,-2.13178503362268,
14.6622717010839)) ;
#62881 = CARTESIAN_POINT('Ctrl Pts',(-27.6569440625584,-2.11521346678123,
14.660728383897)) ;
#62882 = CARTESIAN_POINT('Ctrl Pts',(-27.6508686477712,-2.08231264840602,
14.6576721798256)) ;
#62883 = CARTESIAN_POINT('Ctrl Pts',(-27.6478512359416,-2.06598339666736,
14.6561592502659)) ;
#62884 = CARTESIAN_POINT('Ctrl Pts',(-27.6433608192526,-2.04170760129347,
14.6539187332194)) ;
#62885 = CARTESIAN_POINT('Ctrl Pts',(-27.641869952078,-2.03365201740627,14.6531767297022)) ;
#62886 = CARTESIAN_POINT('Ctrl Pts',(-27.6389008018245,-2.01761960352721,
14.6517037323102)) ;
#62887 = CARTESIAN_POINT('Ctrl Pts',(-27.637422519138,-2.00964277353076,14.6509727376943)) ;
#62888 = CARTESIAN_POINT('Ctrl Pts',(-27.6344789864692,-1.99377392847877,
14.6495235860387)) ;
#62889 = CARTESIAN_POINT('Ctrl Pts',(-27.6330137499688,-1.98588191359784,
14.6488054036467)) ;
#62890 = CARTESIAN_POINT('Ctrl Pts',(-27.6308256171952,-1.97411205296613,
14.6477398650107)) ;
#62891 = CARTESIAN_POINT('Ctrl Pts',(-27.6300978544014,-1.97020012647409,
14.647386651771)) ;
#62892 = CARTESIAN_POINT('Ctrl Pts',(-27.628645441466,-1.96239975406557,14.6466847137016)) ;
#62893 = CARTESIAN_POINT('Ctrl Pts',(-27.6279207921727,-1.95851130813563,
14.6463359872661)) ;
#62894 = CARTESIAN_POINT('Ctrl Pts',(-27.6264734567956,-1.95075390253628,
14.6456434286151)) ;
#62895 = CARTESIAN_POINT('Ctrl Pts',(-27.6257123251301,-1.9466788340925,14.6452811784527)) ;
#62896 = CARTESIAN_POINT('Ctrl Pts',(-27.6241509512269,-1.93833487624977,
14.644544935801)) ;
#62897 = CARTESIAN_POINT('Ctrl Pts',(-27.6233507430922,-1.93406598617168,
14.6441708786873)) ;
#62898 = CARTESIAN_POINT('Ctrl Pts',(-27.6221466323401,-1.92766291397871,
14.6436170738425)) ;
#62899 = CARTESIAN_POINT('Ctrl Pts',(-27.6217446236619,-1.92552861367038,
14.6434337016171)) ;
#62900 = CARTESIAN_POINT('Ctrl Pts',(-27.6209433159066,-1.92128438088597,
14.643072597264)) ;
#62901 = CARTESIAN_POINT('Ctrl Pts',(-27.6205440335406,-1.91917444795388,
14.6428948334146)) ;
#62902 = CARTESIAN_POINT('Ctrl Pts',(-27.6199497787747,-1.91604602430983,
14.6426354742745)) ;
#62903 = CARTESIAN_POINT('Ctrl Pts',(-27.6197524672339,-1.91500929953434,
14.6425502463075)) ;
#62904 = CARTESIAN_POINT('Ctrl Pts',(-27.6193597090545,-1.91295104651823,
14.6423829774186)) ;
#62905 = CARTESIAN_POINT('Ctrl Pts',(-27.619164263621,-1.91192951823391,14.6423009342046)) ;
#62906 = CARTESIAN_POINT('Ctrl Pts',(-27.6187753533729,-1.9099046958582,14.6421411567538)) ;
#62907 = CARTESIAN_POINT('Ctrl Pts',(-27.6185819073017,-1.90890140359366,
14.6420633879694)) ;
#62908 = CARTESIAN_POINT('Ctrl Pts',(-27.6182929061471,-1.90741243308273,
14.6419515767408)) ;
#62909 = CARTESIAN_POINT('Ctrl Pts',(-27.6181967625174,-1.9069187713992,14.6419151221661)) ;
#62910 = CARTESIAN_POINT('Ctrl Pts',(-27.6180046402354,-1.90593716018056,
14.6418444220033)) ;
#62911 = CARTESIAN_POINT('Ctrl Pts',(-27.617908672781,-1.90544920999584,14.641810155007)) ;
#62912 = CARTESIAN_POINT('Ctrl Pts',(-27.617763081606,-1.90471492694364,14.6417608076318)) ;
#62913 = CARTESIAN_POINT('Ctrl Pts',(-27.6177109619107,-1.90445312217609,
14.6417436090468)) ;
#62914 = CARTESIAN_POINT('Ctrl Pts',(-27.6176035565294,-1.90391724739378,
14.6417097722123)) ;
#62915 = CARTESIAN_POINT('Ctrl Pts',(-27.6175482731852,-1.90364317719369,
14.6416931294639)) ;
#62916 = CARTESIAN_POINT('Ctrl Pts',(-27.6174364927896,-1.90309534975757,
14.6416622713397)) ;
#62917 = CARTESIAN_POINT('Ctrl Pts',(-27.617380047885,-1.90282163135034,14.6416479747356)) ;
#62918 = CARTESIAN_POINT('Ctrl Pts',(-27.6171018470644,-1.90163370011507,
14.6416486087149)) ;
#62919 = CARTESIAN_POINT('Ctrl Pts',(-27.6170904460682,-1.90158501729869,
14.6416486346961)) ;
#62920 = CARTESIAN_POINT('Ctrl Pts',(-27.617079045072,-1.9015363344823,14.6416486606773)) ;
#62921 = CARTESIAN_POINT('',(-20.5476539041775,-15.0366437072153,27.0544663940876)) ;
#62922 = CARTESIAN_POINT('',(-20.5712511819771,-15.0366437072153,27.0365282098624)) ;
#62923 = CARTESIAN_POINT('Origin',(0.826633213912537,-21.6462763158694,-1.08741739643853)) ;
#62924 = CARTESIAN_POINT('',(-18.9167133915938,-1.90153624328746,24.8845109207828)) ;
#62925 = CARTESIAN_POINT('Ctrl Pts',(-18.9167134028615,-1.9015363350045,24.8845109360263)) ;
#62926 = CARTESIAN_POINT('Ctrl Pts',(-18.9167143685661,-1.90158489556102,
24.8845228078318)) ;
#62927 = CARTESIAN_POINT('Ctrl Pts',(-18.9167310208152,-1.90242225567914,
24.8847275208156)) ;
#62928 = CARTESIAN_POINT('Ctrl Pts',(-18.9167616201006,-1.90282386086443,
24.8848085131963)) ;
#62929 = CARTESIAN_POINT('Ctrl Pts',(-18.9167849102915,-1.90309805764489,
24.8848619876481)) ;
#62930 = CARTESIAN_POINT('Ctrl Pts',(-18.9168335480839,-1.90364684188482,
24.8849674739658)) ;
#62931 = CARTESIAN_POINT('Ctrl Pts',(-18.9168589674186,-1.90392139050459,
24.8850194212191)) ;
#62932 = CARTESIAN_POINT('Ctrl Pts',(-18.9169098374949,-1.90445820041271,
24.8851201021622)) ;
#62933 = CARTESIAN_POINT('Ctrl Pts',(-18.9169352923059,-1.90472046188661,
24.8851688328067)) ;
#62934 = CARTESIAN_POINT('Ctrl Pts',(-18.9170076880584,-1.90545603941596,
24.8853047487709)) ;
#62935 = CARTESIAN_POINT('Ctrl Pts',(-18.9170571270611,-1.9059448544838,24.8853940585281)) ;
#62936 = CARTESIAN_POINT('Ctrl Pts',(-18.9171581757274,-1.90692820554584,
24.8855725130536)) ;
#62937 = CARTESIAN_POINT('Ctrl Pts',(-18.9172098047175,-1.90742274218952,
24.885661643299)) ;
#62938 = CARTESIAN_POINT('Ctrl Pts',(-18.9173672021873,-1.90891435167757,
24.8859292022212)) ;
#62939 = CARTESIAN_POINT('Ctrl Pts',(-18.9174754494137,-1.90991942206317,
24.8861078226986)) ;
#62940 = CARTESIAN_POINT('Ctrl Pts',(-18.9176964604024,-1.9119478329134,24.8864663730323)) ;
#62941 = CARTESIAN_POINT('Ctrl Pts',(-18.9178092552605,-1.91297117155114,
24.8866462787757)) ;
#62942 = CARTESIAN_POINT('Ctrl Pts',(-18.9180382923743,-1.91503307213536,
24.8870074214629)) ;
#62943 = CARTESIAN_POINT('Ctrl Pts',(-18.9181545367088,-1.91607163412574,
24.8871886568378)) ;
#62944 = CARTESIAN_POINT('Ctrl Pts',(-18.9185072774196,-1.91920560164744,
24.8877340621205)) ;
#62945 = CARTESIAN_POINT('Ctrl Pts',(-18.9187477425563,-1.92131927347479,
24.888099956833)) ;
#62946 = CARTESIAN_POINT('Ctrl Pts',(-18.9192346278442,-1.92557102703072,
24.8888335559801)) ;
#62947 = CARTESIAN_POINT('Ctrl Pts',(-18.9194810765899,-1.92770910921484,
24.8892012387961)) ;
#62948 = CARTESIAN_POINT('Ctrl Pts',(-18.9202237554663,-1.93412352704139,
24.8903017982988)) ;
#62949 = CARTESIAN_POINT('Ctrl Pts',(-18.920723258853,-1.93839998088127,24.8910322174041)) ;
#62950 = CARTESIAN_POINT('Ctrl Pts',(-18.9217041965976,-1.94675872244878,
24.8924563874319)) ;
#62951 = CARTESIAN_POINT('Ctrl Pts',(-18.9221856892737,-1.95084101085567,
24.8931500941983)) ;
#62952 = CARTESIAN_POINT('Ctrl Pts',(-18.9231049569439,-1.95861222293703,
24.8944686268492)) ;
#62953 = CARTESIAN_POINT('Ctrl Pts',(-18.9235671715973,-1.96250762084814,
24.8951284731753)) ;
#62954 = CARTESIAN_POINT('Ctrl Pts',(-18.9244965379162,-1.97032193918007,
24.8964505190558)) ;
#62955 = CARTESIAN_POINT('Ctrl Pts',(-18.9249636910165,-1.97424085961422,
24.8971127175227)) ;
#62956 = CARTESIAN_POINT('Ctrl Pts',(-18.9263717650827,-1.98603176298418,
24.8991031475054)) ;
#62957 = CARTESIAN_POINT('Ctrl Pts',(-18.9273192629094,-1.99393788757247,
24.9004352423095)) ;
#62958 = CARTESIAN_POINT('Ctrl Pts',(-18.9292290124779,-2.00983510364014,
24.9031102729783)) ;
#62959 = CARTESIAN_POINT('Ctrl Pts',(-18.9301912870776,-2.01782619494491,
24.9044531914216)) ;
#62960 = CARTESIAN_POINT('Ctrl Pts',(-18.9321287558131,-2.03388727221324,
24.9071496875273)) ;
#62961 = CARTESIAN_POINT('Ctrl Pts',(-18.9331039506085,-2.04195725818132,
24.9085032646887)) ;
#62962 = CARTESIAN_POINT('Ctrl Pts',(-18.9360467601344,-2.0662764547135,24.9125792593993)) ;
#62963 = CARTESIAN_POINT('Ctrl Pts',(-18.9380315183021,-2.08263490044522,
24.9153170013827)) ;
#62964 = CARTESIAN_POINT('Ctrl Pts',(-18.9420376064851,-2.11559453995239,
24.9208276995194)) ;
#62965 = CARTESIAN_POINT('Ctrl Pts',(-18.944058974998,-2.13219573393279,24.9236006264605)) ;
#62966 = CARTESIAN_POINT('Ctrl Pts',(-18.9481306122324,-2.16559233001946,
24.9291749257832)) ;
#62967 = CARTESIAN_POINT('Ctrl Pts',(-18.950180894613,-2.18238772828634,24.9319762867846)) ;
#62968 = CARTESIAN_POINT('Ctrl Pts',(-18.9543033162345,-2.21612418093343,
24.9376002047454)) ;
#62969 = CARTESIAN_POINT('Ctrl Pts',(-18.9563754572838,-2.23306523532159,
24.9404227603317)) ;
#62970 = CARTESIAN_POINT('Ctrl Pts',(-18.9626145961174,-2.28403406848378,
24.9489109737907)) ;
#62971 = CARTESIAN_POINT('Ctrl Pts',(-18.9668042516112,-2.31820751696578,
24.95459722236)) ;
#62972 = CARTESIAN_POINT('Ctrl Pts',(-18.975192415737,-2.38655453238059,24.965963020267)) ;
#62973 = CARTESIAN_POINT('Ctrl Pts',(-18.97939095797,-2.42072808564842,24.9716425405143)) ;
#62974 = CARTESIAN_POINT('Ctrl Pts',(-18.9877467683852,-2.48868692883717,
24.9829321668039)) ;
#62975 = CARTESIAN_POINT('Ctrl Pts',(-18.991904050825,-2.52247221880362,24.9885422620198)) ;
#62976 = CARTESIAN_POINT('Ctrl Pts',(-19.004239767148,-2.62266316540279,25.0051736273985)) ;
#62977 = CARTESIAN_POINT('Ctrl Pts',(-19.0122819776285,-2.68790389838004,
25.0159960474464)) ;
#62978 = CARTESIAN_POINT('Ctrl Pts',(-19.0283453367079,-2.81812392893152,
25.0375890319205)) ;
#62979 = CARTESIAN_POINT('Ctrl Pts',(-19.036777160132,-2.88642263950378,25.0489091013579)) ;
#62980 = CARTESIAN_POINT('Ctrl Pts',(-19.053701642929,-3.02343231200211,25.0716100109559)) ;
#62981 = CARTESIAN_POINT('Ctrl Pts',(-19.0621943335895,-3.09214327400093,
25.0829908273511)) ;
#62982 = CARTESIAN_POINT('Ctrl Pts',(-19.0792367415917,-3.22996414801061,
25.1058126736773)) ;
#62983 = CARTESIAN_POINT('Ctrl Pts',(-19.087786471612,-3.29907406000788,25.1172536939666)) ;
#62984 = CARTESIAN_POINT('Ctrl Pts',(-19.1049398605727,-3.43767953400148,
25.1401948503665)) ;
#62985 = CARTESIAN_POINT('Ctrl Pts',(-19.1135435211405,-3.50717509600125,
25.1516949852397)) ;
#62986 = CARTESIAN_POINT('Ctrl Pts',(-19.1394313727074,-3.71622030832927,
25.1862819436808)) ;
#62987 = CARTESIAN_POINT('Ctrl Pts',(-19.1567923463698,-3.85632848433072,
25.2094553871857)) ;
#62988 = CARTESIAN_POINT('Ctrl Pts',(-19.1917005046174,-4.13792784932362,
25.2560197389565)) ;
#62989 = CARTESIAN_POINT('Ctrl Pts',(-19.2092477369008,-4.27941903839452,
25.2794106109836)) ;
#62990 = CARTESIAN_POINT('Ctrl Pts',(-19.2445119983007,-4.56367804392642,
25.3263946806514)) ;
#62991 = CARTESIAN_POINT('Ctrl Pts',(-19.2622290485708,-4.70644585947729,
25.3499878619754)) ;
#62992 = CARTESIAN_POINT('Ctrl Pts',(-19.2978175811806,-4.99315173039635,
25.397360612901)) ;
#62993 = CARTESIAN_POINT('Ctrl Pts',(-19.3156890741506,-5.13708978577956,
25.4211401744257)) ;
#62994 = CARTESIAN_POINT('Ctrl Pts',(-19.3515717475988,-5.42602975154862,
25.4688692776673)) ;
#62995 = CARTESIAN_POINT('Ctrl Pts',(-19.3695829332874,-5.57103166193216,
25.4928188154226)) ;
#62996 = CARTESIAN_POINT('Ctrl Pts',(-19.4057306414897,-5.8619929533723,25.5408711637485)) ;
#62997 = CARTESIAN_POINT('Ctrl Pts',(-19.4238671649456,-6.00795233443024,
25.5649739736022)) ;
#62998 = CARTESIAN_POINT('Ctrl Pts',(-19.4784435994783,-6.44710710762938,
25.6374869588184)) ;
#62999 = CARTESIAN_POINT('Ctrl Pts',(-19.5150503131399,-6.74157912509782,
25.686101735427)) ;
#63000 = CARTESIAN_POINT('Ctrl Pts',(-19.5885977926232,-7.33307641917909,
25.7837401535482)) ;
#63001 = CARTESIAN_POINT('Ctrl Pts',(-19.6255385891958,-7.63010169582556,
25.8327637716931)) ;
#63002 = CARTESIAN_POINT('Ctrl Pts',(-19.6996450744351,-8.22585443185994,
25.931081921884)) ;
#63003 = CARTESIAN_POINT('Ctrl Pts',(-19.7368107783377,-8.52458189124458,
25.9803764423469)) ;
#63004 = CARTESIAN_POINT('Ctrl Pts',(-19.8112587959478,-9.12288791716573,
26.0790977791134)) ;
#63005 = CARTESIAN_POINT('Ctrl Pts',(-19.8485411167872,-9.4224664837092,26.1285245899967)) ;
#63006 = CARTESIAN_POINT('Ctrl Pts',(-19.9604014044967,-10.3212022315355,
26.2767949056143)) ;
#63007 = CARTESIAN_POINT('Ctrl Pts',(-20.0349925689043,-10.9203594455821,
26.3756283863428)) ;
#63008 = CARTESIAN_POINT('Ctrl Pts',(-20.1833522435728,-12.1118653470381,
26.5721532765629)) ;
#63009 = CARTESIAN_POINT('Ctrl Pts',(-20.2571208155407,-12.7042140344991,
26.6698446391582)) ;
#63010 = CARTESIAN_POINT('Ctrl Pts',(-20.4035834685688,-13.8801354421801,
26.8637660032857)) ;
#63011 = CARTESIAN_POINT('Ctrl Pts',(-20.4762636531478,-14.4635951118959,
26.9599772216812)) ;
#63012 = CARTESIAN_POINT('Ctrl Pts',(-20.5476539041704,-15.0366437072153,
27.0544663940931)) ;
#63013 = CARTESIAN_POINT('Ctrl Pts',(-20.5712511819829,-15.0366437072153,
27.036528209858)) ;
#63014 = CARTESIAN_POINT('Ctrl Pts',(-20.5706612171046,-15.0319446557972,
27.0357568549883)) ;
#63015 = CARTESIAN_POINT('Ctrl Pts',(-20.5700711638574,-15.0272449043228,
27.034985385566)) ;
#63016 = CARTESIAN_POINT('Ctrl Pts',(-20.4981035141431,-14.4540257999816,
26.94089087751)) ;
#63017 = CARTESIAN_POINT('Ctrl Pts',(-20.4254367995802,-13.8752942607969,
26.84589680268)) ;
#63018 = CARTESIAN_POINT('Ctrl Pts',(-20.2783747273307,-12.7042140340873,
26.6536878353541)) ;
#63019 = CARTESIAN_POINT('Ctrl Pts',(-20.2039793991207,-12.1118653465652,
26.5564729204515)) ;
#63020 = CARTESIAN_POINT('Ctrl Pts',(-20.0543082598726,-10.9203594449863,
26.3609449796542)) ;
#63021 = CARTESIAN_POINT('Ctrl Pts',(-19.9790325105307,-10.3212022308778,
26.262631906847)) ;
#63022 = CARTESIAN_POINT('Ctrl Pts',(-19.8660924459332,-9.4224664829588,26.1151824162557)) ;
#63023 = CARTESIAN_POINT('Ctrl Pts',(-19.8284413200228,-9.12288791638442,
26.0660359636907)) ;
#63024 = CARTESIAN_POINT('Ctrl Pts',(-19.7532353311701,-8.5245818904015,25.9678908216667)) ;
#63025 = CARTESIAN_POINT('Ctrl Pts',(-19.7156804753596,-8.22585443098604,
25.9188921267852)) ;
#63026 = CARTESIAN_POINT('Ctrl Pts',(-19.6407716073414,-7.63010169489019,
25.8211839321094)) ;
#63027 = CARTESIAN_POINT('Ctrl Pts',(-19.6034176103687,-7.33307641821306,
25.7724744207345)) ;
#63028 = CARTESIAN_POINT('Ctrl Pts',(-19.5290141482999,-6.74157912407075,
25.675486703642)) ;
#63029 = CARTESIAN_POINT('Ctrl Pts',(-19.4919647139464,-6.44710710657191,
25.6272084745458)) ;
#63030 = CARTESIAN_POINT('Ctrl Pts',(-19.4366955704313,-6.00795233332746,
25.5552220729962)) ;
#63031 = CARTESIAN_POINT('Ctrl Pts',(-19.4183233421613,-5.86199295225445,
25.5312984412799)) ;
#63032 = CARTESIAN_POINT('Ctrl Pts',(-19.3816930386047,-5.57103166078429,
25.483612952397)) ;
#63033 = CARTESIAN_POINT('Ctrl Pts',(-19.36343496426,-5.42602975038579,25.4598510945148)) ;
#63034 = CARTESIAN_POINT('Ctrl Pts',(-19.3270452191944,-5.13708978458693,
25.4125074570877)) ;
#63035 = CARTESIAN_POINT('Ctrl Pts',(-19.3089135536827,-4.99315172918884,
25.3889256735835)) ;
#63036 = CARTESIAN_POINT('Ctrl Pts',(-19.2727884808785,-4.70644585824021,
25.3419607899022)) ;
#63037 = CARTESIAN_POINT('Ctrl Pts',(-19.2547950842114,-4.5636780426746,25.3185776816439)) ;
#63038 = CARTESIAN_POINT('Ctrl Pts',(-19.2189577734926,-4.27941903711337,
25.2720292327354)) ;
#63039 = CARTESIAN_POINT('Ctrl Pts',(-19.2011138808186,-4.13792784802786,
25.2488638760705)) ;
#63040 = CARTESIAN_POINT('Ctrl Pts',(-19.1655857215916,-3.8563284830059,25.2027708367835)) ;
#63041 = CARTESIAN_POINT('Ctrl Pts',(-19.1479015027164,-3.71622030698998,
25.1798431178972)) ;
#63042 = CARTESIAN_POINT('Ctrl Pts',(-19.1215009730845,-3.50717509464039,
25.1456458871834)) ;
#63043 = CARTESIAN_POINT('Ctrl Pts',(-19.1127217412279,-3.43767953263345,
25.1342792181322)) ;
#63044 = CARTESIAN_POINT('Ctrl Pts',(-19.0952058077974,-3.29907405862555,
25.1116136608695)) ;
#63045 = CARTESIAN_POINT('Ctrl Pts',(-19.0864691078549,-3.22996414662115,
25.1003147714182)) ;
#63046 = CARTESIAN_POINT('Ctrl Pts',(-19.0690384450932,-3.09214327259721,
25.0777880686832)) ;
#63047 = CARTESIAN_POINT('Ctrl Pts',(-19.0603444949595,-3.02343231059132,
25.0665602457601)) ;
#63048 = CARTESIAN_POINT('Ctrl Pts',(-19.0429988124476,-2.88642263807886,
25.0441795238575)) ;
#63049 = CARTESIAN_POINT('Ctrl Pts',(-19.0343471113395,-2.81812392749956,
25.0330266010882)) ;
#63050 = CARTESIAN_POINT('Ctrl Pts',(-19.0178385950926,-2.68790389707261,
25.0117720163273)) ;
#63051 = CARTESIAN_POINT('Ctrl Pts',(-19.0095621715615,-2.62266316423356,
25.0011276404477)) ;
#63052 = CARTESIAN_POINT('Ctrl Pts',(-18.9968371732943,-2.52247221784659,
24.9847921995644)) ;
#63053 = CARTESIAN_POINT('Ctrl Pts',(-18.9925437569551,-2.48868692795171,
24.9792855906672)) ;
#63054 = CARTESIAN_POINT('Ctrl Pts',(-18.9839010537239,-2.42072808490687,
24.9682140546636)) ;
#63055 = CARTESIAN_POINT('Ctrl Pts',(-18.979551781078,-2.38655453171139,24.9626491167161)) ;
#63056 = CARTESIAN_POINT('Ctrl Pts',(-18.9708443382193,-2.31820751644134,
24.9515260282295)) ;
#63057 = CARTESIAN_POINT('Ctrl Pts',(-18.9664862050282,-2.28403406803175,
24.9459678530947)) ;
#63058 = CARTESIAN_POINT('Ctrl Pts',(-18.9599765334731,-2.23306523497749,
24.9376852932921)) ;
#63059 = CARTESIAN_POINT('Ctrl Pts',(-18.9578112165184,-2.2161241806252,24.934933568197)) ;
#63060 = CARTESIAN_POINT('Ctrl Pts',(-18.9534951550256,-2.18238772804956,
24.929456851458)) ;
#63061 = CARTESIAN_POINT('Ctrl Pts',(-18.9513444122986,-2.16559232981822,
24.9267318584357)) ;
#63062 = CARTESIAN_POINT('Ctrl Pts',(-18.9470625745811,-2.1321957338023,24.9213173493843)) ;
#63063 = CARTESIAN_POINT('Ctrl Pts',(-18.9449314942107,-2.11559453985707,
24.9186278232381)) ;
#63064 = CARTESIAN_POINT('Ctrl Pts',(-18.9406934031869,-2.08263490041971,
24.913293489094)) ;
#63065 = CARTESIAN_POINT('Ctrl Pts',(-18.938586430973,-2.06627645472267,24.9106486518222)) ;
#63066 = CARTESIAN_POINT('Ctrl Pts',(-18.9354462912493,-2.04195725824198,
24.9067226636415)) ;
#63067 = CARTESIAN_POINT('Ctrl Pts',(-18.9344029442324,-2.03388727229097,
24.9054208944563)) ;
#63068 = CARTESIAN_POINT('Ctrl Pts',(-18.9323230632261,-2.01782619505665,
24.9028326573533)) ;
#63069 = CARTESIAN_POINT('Ctrl Pts',(-18.931286529905,-2.00983510376875,24.9015461889268)) ;
#63070 = CARTESIAN_POINT('Ctrl Pts',(-18.9292199162578,-1.99393788773474,
24.8989904032391)) ;
#63071 = CARTESIAN_POINT('Ctrl Pts',(-18.928189858838,-1.98603176316325,24.8977210686105)) ;
#63072 = CARTESIAN_POINT('Ctrl Pts',(-18.9266486797622,-1.97424085981823,
24.8958318224319)) ;
#63073 = CARTESIAN_POINT('Ctrl Pts',(-18.9261355951483,-1.97032193939221,
24.895204540196)) ;
#63074 = CARTESIAN_POINT('Ctrl Pts',(-18.9251103696795,-1.96250762107683,
24.8939553645511)) ;
#63075 = CARTESIAN_POINT('Ctrl Pts',(-18.924598230256,-1.95861222317414,24.8933334700507)) ;
#63076 = CARTESIAN_POINT('Ctrl Pts',(-18.9235736882859,-1.95084101111684,
24.8920949648484)) ;
#63077 = CARTESIAN_POINT('Ctrl Pts',(-18.9230340800797,-1.94675872272648,
24.8914454363637)) ;
#63078 = CARTESIAN_POINT('Ctrl Pts',(-18.9219242497106,-1.93839998119292,
24.8901192479705)) ;
#63079 = CARTESIAN_POINT('Ctrl Pts',(-18.9213540857047,-1.93412352737036,
24.889442543676)) ;
#63080 = CARTESIAN_POINT('Ctrl Pts',(-18.9204923292509,-1.92770910956992,
24.888432504601)) ;
#63081 = CARTESIAN_POINT('Ctrl Pts',(-18.9202039804729,-1.9255710273949,24.8880966733639)) ;
#63082 = CARTESIAN_POINT('Ctrl Pts',(-18.9196273766362,-1.92131927385614,
24.8874312764888)) ;
#63083 = CARTESIAN_POINT('Ctrl Pts',(-18.9193391500849,-1.91920560203643,
24.8871016890618)) ;
#63084 = CARTESIAN_POINT('Ctrl Pts',(-18.9189079929671,-1.91607163452743,
24.8866158943853)) ;
#63085 = CARTESIAN_POINT('Ctrl Pts',(-18.9187644622541,-1.91503307254177,
24.8864554015773)) ;
#63086 = CARTESIAN_POINT('Ctrl Pts',(-18.9184777571413,-1.91297117196593,
24.8861380969653)) ;
#63087 = CARTESIAN_POINT('Ctrl Pts',(-18.9183345847531,-1.91194783333305,
24.8859812836212)) ;
#63088 = CARTESIAN_POINT('Ctrl Pts',(-18.9180482302814,-1.90991942249111,
24.8856724061141)) ;
#63089 = CARTESIAN_POINT('Ctrl Pts',(-18.9179050797004,-1.90891435211023,
24.8855203184782)) ;
#63090 = CARTESIAN_POINT('Ctrl Pts',(-18.9176893815891,-1.90742274262821,
24.8852970785531)) ;
#63091 = CARTESIAN_POINT('Ctrl Pts',(-18.9176173123751,-1.90692820598606,
24.8852234865624)) ;
#63092 = CARTESIAN_POINT('Ctrl Pts',(-18.9174723958912,-1.90594485492843,
24.8850783794859)) ;
#63093 = CARTESIAN_POINT('Ctrl Pts',(-18.9173995678447,-1.90545603986145,
24.8850068496178)) ;
#63094 = CARTESIAN_POINT('Ctrl Pts',(-18.9172879738986,-1.90472046209792,
24.8849007312849)) ;
#63095 = CARTESIAN_POINT('Ctrl Pts',(-18.9172478292892,-1.9044582003785,24.8848631674712)) ;
#63096 = CARTESIAN_POINT('Ctrl Pts',(-18.9171644272708,-1.90392138996427,
24.8847872165361)) ;
#63097 = CARTESIAN_POINT('Ctrl Pts',(-18.9171211738375,-1.9036468410861,24.884748826345)) ;
#63098 = CARTESIAN_POINT('Ctrl Pts',(-18.9170325444076,-1.90309805632819,
24.8846737407453)) ;
#63099 = CARTESIAN_POINT('Ctrl Pts',(-18.9169872500073,-1.90282385927809,
24.8846369933886)) ;
#63100 = CARTESIAN_POINT('Ctrl Pts',(-18.9167341120365,-1.90163370160465,
24.8845204688771)) ;
#63101 = CARTESIAN_POINT('Ctrl Pts',(-18.916723757449,-1.90158501830458,24.8845157024517)) ;
#63102 = CARTESIAN_POINT('Ctrl Pts',(-18.9167134028615,-1.9015363350045,24.8845109360263)) ;
#63103 = CARTESIAN_POINT('',(-7.28867002793326,-15.0366437072153,33.1817046285839)) ;
#63104 = CARTESIAN_POINT('',(-7.31761838529145,-15.0366437072153,33.1753326132824)) ;
#63105 = CARTESIAN_POINT('Origin',(0.293637272419048,-21.6462763158694,-1.3340075774398)) ;
#63106 = CARTESIAN_POINT('',(-6.71960916186913,-1.90153624397926,30.5274922328533)) ;
#63107 = CARTESIAN_POINT('Ctrl Pts',(-6.71960916572461,-1.9015363363881,30.527492251559)) ;
#63108 = CARTESIAN_POINT('Ctrl Pts',(-6.71960503468368,-1.90158489401769,
30.5275034359727)) ;
#63109 = CARTESIAN_POINT('Ctrl Pts',(-6.71953434398448,-1.90241581601747,
30.5276948245448)) ;
#63110 = CARTESIAN_POINT('Ctrl Pts',(-6.71952806587547,-1.90281445409125,
30.5277805608094)) ;
#63111 = CARTESIAN_POINT('Ctrl Pts',(-6.71952671045772,-1.90308662669026,
30.52783845261)) ;
#63112 = CARTESIAN_POINT('Ctrl Pts',(-6.71952647178206,-1.9036313623249,30.5279537746666)) ;
#63113 = CARTESIAN_POINT('Ctrl Pts',(-6.71952768038816,-1.90390388655798,
30.5280111764909)) ;
#63114 = CARTESIAN_POINT('Ctrl Pts',(-6.71953147217083,-1.90443673958349,
30.5281230969409)) ;
#63115 = CARTESIAN_POINT('Ctrl Pts',(-6.71953406034505,-1.90469706856311,
30.5281776145062)) ;
#63116 = CARTESIAN_POINT('Ctrl Pts',(-6.71954254288055,-1.90542717101058,
30.5283302416739)) ;
#63117 = CARTESIAN_POINT('Ctrl Pts',(-6.71954980436227,-1.90591232878685,
30.5284313057678)) ;
#63118 = CARTESIAN_POINT('Ctrl Pts',(-6.71956635780412,-1.90688832266939,
30.5286341885841)) ;
#63119 = CARTESIAN_POINT('Ctrl Pts',(-6.71957567329605,-1.90737915942458,
30.5287360022641)) ;
#63120 = CARTESIAN_POINT('Ctrl Pts',(-6.71960581785518,-1.9088596096152,30.5290426396081)) ;
#63121 = CARTESIAN_POINT('Ctrl Pts',(-6.71962880637323,-1.90985716095924,
30.5292486676527)) ;
#63122 = CARTESIAN_POINT('Ctrl Pts',(-6.71967831619922,-1.91187039742389,
30.5296637833386)) ;
#63123 = CARTESIAN_POINT('Ctrl Pts',(-6.71970487569611,-1.91288608071834,
30.5298728621872)) ;
#63124 = CARTESIAN_POINT('Ctrl Pts',(-6.7197605522653,-1.91493255703098,30.5302936542332)) ;
#63125 = CARTESIAN_POINT('Ctrl Pts',(-6.71978967180336,-1.91596335009186,
30.5305053668967)) ;
#63126 = CARTESIAN_POINT('Ctrl Pts',(-6.71987994037281,-1.91907387452225,
30.5311437040075)) ;
#63127 = CARTESIAN_POINT('Ctrl Pts',(-6.71994395324573,-1.92117173588608,
30.5315735344974)) ;
#63128 = CARTESIAN_POINT('Ctrl Pts',(-6.72007660206596,-1.92539168676737,
30.5324373046928)) ;
#63129 = CARTESIAN_POINT('Ctrl Pts',(-6.72014527296858,-1.92751377674115,
30.5328712368007)) ;
#63130 = CARTESIAN_POINT('Ctrl Pts',(-6.72035534009416,-1.93388021790867,
30.5341721769161)) ;
#63131 = CARTESIAN_POINT('Ctrl Pts',(-6.7205007238618,-1.93812468728337,30.5350383322065)) ;
#63132 = CARTESIAN_POINT('Ctrl Pts',(-6.7207905249419,-1.94642091372353,30.5367300763717)) ;
#63133 = CARTESIAN_POINT('Ctrl Pts',(-6.72093501344642,-1.95047267146818,
30.5375556497196)) ;
#63134 = CARTESIAN_POINT('Ctrl Pts',(-6.7212133316577,-1.9581855017446,30.5391264711218)) ;
#63135 = CARTESIAN_POINT('Ctrl Pts',(-6.72135457498788,-1.96205150310624,
30.5399134515561)) ;
#63136 = CARTESIAN_POINT('Ctrl Pts',(-6.72164053693774,-1.9698068509058,30.5414915874222)) ;
#63137 = CARTESIAN_POINT('Ctrl Pts',(-6.72178525732577,-1.97369619735714,
30.5422827424674)) ;
#63138 = CARTESIAN_POINT('Ctrl Pts',(-6.72222378915863,-1.98539812121369,
30.5446624157223)) ;
#63139 = CARTESIAN_POINT('Ctrl Pts',(-6.72252192512217,-1.99324458270728,
30.5462571521216)) ;
#63140 = CARTESIAN_POINT('Ctrl Pts',(-6.72312698742384,-2.0090218315379,30.5494625338965)) ;
#63141 = CARTESIAN_POINT('Ctrl Pts',(-6.7234339417142,-2.01695261870037,30.5510731730823)) ;
#63142 = CARTESIAN_POINT('Ctrl Pts',(-6.72405505928695,-2.03289249242576,
30.5543094332857)) ;
#63143 = CARTESIAN_POINT('Ctrl Pts',(-6.72436922337813,-2.0409015789932,30.5559350541256)) ;
#63144 = CARTESIAN_POINT('Ctrl Pts',(-6.72532088665166,-2.06503725311967,
30.5608328391374)) ;
#63145 = CARTESIAN_POINT('Ctrl Pts',(-6.72596745733348,-2.08127225164298,
30.564125946969)) ;
#63146 = CARTESIAN_POINT('Ctrl Pts',(-6.7272788940997,-2.1139831651699,30.5707591149674)) ;
#63147 = CARTESIAN_POINT('Ctrl Pts',(-6.72794380721284,-2.13045908037843,
30.5740991648255)) ;
#63148 = CARTESIAN_POINT('Ctrl Pts',(-6.72928783210369,-2.16360365366924,
30.5808169247956)) ;
#63149 = CARTESIAN_POINT('Ctrl Pts',(-6.72996696100518,-2.18027230791273,
30.5841946303259)) ;
#63150 = CARTESIAN_POINT('Ctrl Pts',(-6.73133608992497,-2.21375417357443,
30.5909782376895)) ;
#63151 = CARTESIAN_POINT('Ctrl Pts',(-6.73202609214606,-2.23056738500055,
30.5943841390392)) ;
#63152 = CARTESIAN_POINT('Ctrl Pts',(-6.73410801808508,-2.28115159033711,
30.6046298116117)) ;
#63153 = CARTESIAN_POINT('Ctrl Pts',(-6.73551179022772,-2.31506715501583,
30.6114975668916)) ;
#63154 = CARTESIAN_POINT('Ctrl Pts',(-6.73833014157579,-2.38289840281523,
30.6252307237003)) ;
#63155 = CARTESIAN_POINT('Ctrl Pts',(-6.73974476333159,-2.41681407227232,
30.6320961129715)) ;
#63156 = CARTESIAN_POINT('Ctrl Pts',(-6.7425657903985,-2.48426007833226,30.645747161211)) ;
#63157 = CARTESIAN_POINT('Ctrl Pts',(-6.74397221312697,-2.51779041498063,
30.652532816355)) ;
#63158 = CARTESIAN_POINT('Ctrl Pts',(-6.74815180308299,-2.61722529311255,
30.672653870791)) ;
#63159 = CARTESIAN_POINT('Ctrl Pts',(-6.75088517916712,-2.68197370242755,
30.6857533838662)) ;
#63160 = CARTESIAN_POINT('Ctrl Pts',(-6.75635251277483,-2.81116116865304,
30.7118868210986)) ;
#63161 = CARTESIAN_POINT('Ctrl Pts',(-6.75922734717377,-2.87889443305604,
30.7255868111386)) ;
#63162 = CARTESIAN_POINT('Ctrl Pts',(-6.76500650404872,-3.01476980026688,
30.7530668132049)) ;
#63163 = CARTESIAN_POINT('Ctrl Pts',(-6.76791086463308,-3.08291190314725,
30.7668468168585)) ;
#63164 = CARTESIAN_POINT('Ctrl Pts',(-6.77374586998526,-3.21959175607126,
30.7944847600319)) ;
#63165 = CARTESIAN_POINT('Ctrl Pts',(-6.77667653020986,-3.28812950610133,
30.8083426961463)) ;
#63166 = CARTESIAN_POINT('Ctrl Pts',(-6.78256179851678,-3.42558746340932,
30.8361342274369)) ;
#63167 = CARTESIAN_POINT('Ctrl Pts',(-6.78551640858651,-3.49450767069068,
30.8500678221752)) ;
#63168 = CARTESIAN_POINT('Ctrl Pts',(-6.79441341605667,-3.70182219488036,
30.8919785127782)) ;
#63169 = CARTESIAN_POINT('Ctrl Pts',(-6.80038888440015,-3.84077041348023,
30.9200655382932)) ;
#63170 = CARTESIAN_POINT('Ctrl Pts',(-6.81241693001848,-4.12003841381346,
30.9765128478343)) ;
#63171 = CARTESIAN_POINT('Ctrl Pts',(-6.81846956547146,-4.26035819562616,
31.0048731190712)) ;
#63172 = CARTESIAN_POINT('Ctrl Pts',(-6.83064346250994,-4.54226381754215,
31.0618464617664)) ;
#63173 = CARTESIAN_POINT('Ctrl Pts',(-6.83676475000264,-4.68384965673699,
31.0904595273298)) ;
#63174 = CARTESIAN_POINT('Ctrl Pts',(-6.84906874931766,-4.96818188660624,
31.1479177180033)) ;
#63175 = CARTESIAN_POINT('Ctrl Pts',(-6.85525147411698,-5.11092827729567,
31.1767628402602)) ;
#63176 = CARTESIAN_POINT('Ctrl Pts',(-6.8676719030735,-5.39747610609673,31.2346642376376)) ;
#63177 = CARTESIAN_POINT('Ctrl Pts',(-6.87390961359172,-5.54127754420606,
31.2637205113573)) ;
#63178 = CARTESIAN_POINT('Ctrl Pts',(-6.8864340498454,-5.82982996427431,31.3220231992416)) ;
#63179 = CARTESIAN_POINT('Ctrl Pts',(-6.89272077672559,-5.97458094623454,
31.3512696131538)) ;
#63180 = CARTESIAN_POINT('Ctrl Pts',(-6.91164600392969,-6.41009995304015,
31.4392624435926)) ;
#63181 = CARTESIAN_POINT('Ctrl Pts',(-6.92434947612127,-6.70213403411822,
31.4982624642693)) ;
#63182 = CARTESIAN_POINT('Ctrl Pts',(-6.94988691163196,-7.28873431722379,
31.6167695952287)) ;
#63183 = CARTESIAN_POINT('Ctrl Pts',(-6.96272091249833,-7.58330051928491,
31.6762766972538)) ;
#63184 = CARTESIAN_POINT('Ctrl Pts',(-6.98847858561803,-8.17412101401313,
31.7956283738327)) ;
#63185 = CARTESIAN_POINT('Ctrl Pts',(-7.00140227647572,-8.47037530667691,
31.8554729442908)) ;
#63186 = CARTESIAN_POINT('Ctrl Pts',(-7.02729958170605,-9.0637279530796,31.9753297048947)) ;
#63187 = CARTESIAN_POINT('Ctrl Pts',(-7.04027320479137,-9.36082630682544,
32.0353418931237)) ;
#63188 = CARTESIAN_POINT('Ctrl Pts',(-7.07921035581026,-10.2521214162309,
32.2153748841193)) ;
#63189 = CARTESIAN_POINT('Ctrl Pts',(-7.10519001132179,-10.8463182046384,
32.335392143864)) ;
#63190 = CARTESIAN_POINT('Ctrl Pts',(-7.15688461897129,-12.0279596232458,
32.574056129412)) ;
#63191 = CARTESIAN_POINT('Ctrl Pts',(-7.18259964647311,-12.6154042534972,
32.6927028386364)) ;
#63192 = CARTESIAN_POINT('Ctrl Pts',(-7.23346099536655,-13.7767891025737,
32.9272638195374)) ;
#63193 = CARTESIAN_POINT('Ctrl Pts',(-7.25860735275444,-14.3507293213961,
33.0431780832901)) ;
#63194 = CARTESIAN_POINT('Ctrl Pts',(-7.28510452610227,-14.9552953856552,
33.1652756333742)) ;
#63195 = CARTESIAN_POINT('Ctrl Pts',(-7.28688844246384,-14.995996643595,33.173495608376)) ;
#63196 = CARTESIAN_POINT('Ctrl Pts',(-7.28867002731916,-15.036643707215,33.1817046287187)) ;
#63197 = CARTESIAN_POINT('Ctrl Pts',(-7.31761838590095,-15.036643707215,33.175332613148)) ;
#63198 = CARTESIAN_POINT('Ctrl Pts',(-7.31578843034696,-14.9959966435885,
33.1671342399998)) ;
#63199 = CARTESIAN_POINT('Ctrl Pts',(-7.31395599106881,-14.9552953856421,
33.1589249456982)) ;
#63200 = CARTESIAN_POINT('Ctrl Pts',(-7.28673674368188,-14.3507293213698,
33.0369863361262)) ;
#63201 = CARTESIAN_POINT('Ctrl Pts',(-7.26088782347941,-13.7767891025407,
32.9212267181418)) ;
#63202 = CARTESIAN_POINT('Ctrl Pts',(-7.20855873401436,-12.6154042534504,
32.6869888113683)) ;
#63203 = CARTESIAN_POINT('Ctrl Pts',(-7.18207860074982,-12.0279596231921,
32.5685105146561)) ;
#63204 = CARTESIAN_POINT('Ctrl Pts',(-7.12878294951492,-10.8463182045707,
32.3301989454477)) ;
#63205 = CARTESIAN_POINT('Ctrl Pts',(-7.10196750690673,-10.2521214161561,
32.2103656563531)) ;
#63206 = CARTESIAN_POINT('Ctrl Pts',(-7.06171201724267,-9.36082630674012,
32.030622853635)) ;
#63207 = CARTESIAN_POINT('Ctrl Pts',(-7.04828809485541,-9.06372795299079,
31.9707097837769)) ;
#63208 = CARTESIAN_POINT('Ctrl Pts',(-7.02146530499196,-8.47037530658109,
31.851056737744)) ;
#63209 = CARTESIAN_POINT('Ctrl Pts',(-7.00806644622269,-8.17412101391379,
31.7913167596517)) ;
#63210 = CARTESIAN_POINT('Ctrl Pts',(-6.98132900896538,-7.5833005191786,31.6721807454662)) ;
#63211 = CARTESIAN_POINT('Ctrl Pts',(-6.96799044908368,-7.28873431711399,
31.6127847052781)) ;
#63212 = CARTESIAN_POINT('Ctrl Pts',(-6.94140774508735,-6.70213403400147,
31.4945076553094)) ;
#63213 = CARTESIAN_POINT('Ctrl Pts',(-6.92816363851496,-6.41009995291992,
31.4356266372581)) ;
#63214 = CARTESIAN_POINT('Ctrl Pts',(-6.90839247902012,-5.9745809461092,31.347820010596)) ;
#63215 = CARTESIAN_POINT('Ctrl Pts',(-6.90181790735092,-5.82982996414724,
31.3186369561127)) ;
#63216 = CARTESIAN_POINT('Ctrl Pts',(-6.88870411460551,-5.54127754407557,
31.2604639954013)) ;
#63217 = CARTESIAN_POINT('Ctrl Pts',(-6.88216489467994,-5.39747610596454,
31.2314740889205)) ;
#63218 = CARTESIAN_POINT('Ctrl Pts',(-6.86912520497875,-5.11092827716008,
31.1737090011399)) ;
#63219 = CARTESIAN_POINT('Ctrl Pts',(-6.86262474155889,-4.96818188646899,
31.1449338184418)) ;
#63220 = CARTESIAN_POINT('Ctrl Pts',(-6.84966548084162,-4.68384965659638,
31.087619861709)) ;
#63221 = CARTESIAN_POINT('Ctrl Pts',(-6.84320669651301,-4.54226381739987,
31.0590810848165)) ;
#63222 = CARTESIAN_POINT('Ctrl Pts',(-6.83033294054922,-4.26035819548053,
31.0022617927193)) ;
#63223 = CARTESIAN_POINT('Ctrl Pts',(-6.82391799490403,-4.12003841366617,
30.973981271986)) ;
#63224 = CARTESIAN_POINT('Ctrl Pts',(-6.81113274336521,-3.84077041332965,
30.917700636071)) ;
#63225 = CARTESIAN_POINT('Ctrl Pts',(-6.80476249564617,-3.70182219472812,
30.8897005080674)) ;
#63226 = CARTESIAN_POINT('Ctrl Pts',(-6.7952393587118,-3.494507670536,30.8479276389809)) ;
#63227 = CARTESIAN_POINT('Ctrl Pts',(-6.79207032560784,-3.42558746325382,
30.8340412423213)) ;
#63228 = CARTESIAN_POINT('Ctrl Pts',(-6.78574228935676,-3.28812950594421,
30.8063471716248)) ;
#63229 = CARTESIAN_POINT('Ctrl Pts',(-6.78258328820021,-3.21959175591332,
30.7925394971501)) ;
#63230 = CARTESIAN_POINT('Ctrl Pts',(-6.77627412450336,-3.08291190298769,
30.7650059241204)) ;
#63231 = CARTESIAN_POINT('Ctrl Pts',(-6.77312397742212,-3.01476980010652,
30.7512800221658)) ;
#63232 = CARTESIAN_POINT('Ctrl Pts',(-6.76683044476954,-2.87889443289408,
30.7239132427695)) ;
#63233 = CARTESIAN_POINT('Ctrl Pts',(-6.763687097298,-2.81116116849028,30.7102723569261)) ;
#63234 = CARTESIAN_POINT('Ctrl Pts',(-6.75767596940615,-2.68197370215285,
30.6842586178435)) ;
#63235 = CARTESIAN_POINT('Ctrl Pts',(-6.75465637157047,-2.61722529272117,
30.6712221069152)) ;
#63236 = CARTESIAN_POINT('Ctrl Pts',(-6.7500010532002,-2.51779041441006,30.6512057681838)) ;
#63237 = CARTESIAN_POINT('Ctrl Pts',(-6.74842826525773,-2.48426007770124,
30.6444567327798)) ;
#63238 = CARTESIAN_POINT('Ctrl Pts',(-6.74525663369543,-2.41681407151976,
30.6308828583998)) ;
#63239 = CARTESIAN_POINT('Ctrl Pts',(-6.74365780749008,-2.38289840200156,
30.6240580155811)) ;
#63240 = CARTESIAN_POINT('Ctrl Pts',(-6.74044927101749,-2.31506715407992,
30.6104107449871)) ;
#63241 = CARTESIAN_POINT('Ctrl Pts',(-6.73883960450799,-2.28115158934011,
30.6035883104715)) ;
#63242 = CARTESIAN_POINT('Ctrl Pts',(-6.7364270630604,-2.23056738391237,30.5934154118563)) ;
#63243 = CARTESIAN_POINT('Ctrl Pts',(-6.7356231912688,-2.2137541724559,30.5900345750881)) ;
#63244 = CARTESIAN_POINT('Ctrl Pts',(-6.73401741621857,-2.18027230673386,
30.583303057464)) ;
#63245 = CARTESIAN_POINT('Ctrl Pts',(-6.73321551517332,-2.16360365246034,
30.5799523761197)) ;
#63246 = CARTESIAN_POINT('Ctrl Pts',(-6.73161460492591,-2.13045907910981,
30.5732911608798)) ;
#63247 = CARTESIAN_POINT('Ctrl Pts',(-6.73081561316648,-2.11398316387167,
30.5699806239572)) ;
#63248 = CARTESIAN_POINT('Ctrl Pts',(-6.72922064598632,-2.0812722502858,30.5634098657098)) ;
#63249 = CARTESIAN_POINT('Ctrl Pts',(-6.72842471756409,-2.06503725173321,
30.5601496339967)) ;
#63250 = CARTESIAN_POINT('Ctrl Pts',(-6.727231897208,-2.04090157756323,30.5553049316637)) ;
#63251 = CARTESIAN_POINT('Ctrl Pts',(-6.72683444433809,-2.03289249098137,
30.5536976440673)) ;
#63252 = CARTESIAN_POINT('Ctrl Pts',(-6.72603928498888,-2.01695261722727,
30.5504996933498)) ;
#63253 = CARTESIAN_POINT('Ctrl Pts',(-6.72564157932666,-2.00902183005043,
30.5489090300484)) ;
#63254 = CARTESIAN_POINT('Ctrl Pts',(-6.72484481412258,-1.9932445811914,30.5457458452672)) ;
#63255 = CARTESIAN_POINT('Ctrl Pts',(-6.72444578254945,-1.98539811968377,
30.544173317668)) ;
#63256 = CARTESIAN_POINT('Ctrl Pts',(-6.72384458439613,-1.97369619580611,
30.5418294499734)) ;
#63257 = CARTESIAN_POINT('Ctrl Pts',(-6.72364373167107,-1.96980684934784,
30.5410506505884)) ;
#63258 = CARTESIAN_POINT('Ctrl Pts',(-6.72324062165561,-1.9620515015343,30.5394983009585)) ;
#63259 = CARTESIAN_POINT('Ctrl Pts',(-6.72303836614614,-1.95818550016552,
30.5387247503189)) ;
#63260 = CARTESIAN_POINT('Ctrl Pts',(-6.72263139013325,-1.95047267002259,
30.5371822486687)) ;
#63261 = CARTESIAN_POINT('Ctrl Pts',(-6.7224158750706,-1.9464209124257,30.5363723094797)) ;
#63262 = CARTESIAN_POINT('Ctrl Pts',(-6.72196854648401,-1.93812468628743,
30.5347152398046)) ;
#63263 = CARTESIAN_POINT('Ctrl Pts',(-6.72173680408808,-1.93388021706691,
30.5338680935183)) ;
#63264 = CARTESIAN_POINT('Ctrl Pts',(-6.72138120528657,-1.92751377613103,
30.5325991873962)) ;
#63265 = CARTESIAN_POINT('Ctrl Pts',(-6.72126132591748,-1.9253916862349,30.5321765271407)) ;
#63266 = CARTESIAN_POINT('Ctrl Pts',(-6.72101902704608,-1.92117173550713,
30.5313368927791)) ;
#63267 = CARTESIAN_POINT('Ctrl Pts',(-6.72089664243418,-1.91907387421947,
30.5309199108966)) ;
#63268 = CARTESIAN_POINT('Ctrl Pts',(-6.72071053717591,-1.91596334990232,
30.5303026690603)) ;
#63269 = CARTESIAN_POINT('Ctrl Pts',(-6.72064806954126,-1.91493255687844,
30.5300982968757)) ;
#63270 = CARTESIAN_POINT('Ctrl Pts',(-6.72052191423922,-1.91288608064014,
30.5296930183877)) ;
#63271 = CARTESIAN_POINT('Ctrl Pts',(-6.72045822910459,-1.91187039738182,
30.5294921115175)) ;
#63272 = CARTESIAN_POINT('Ctrl Pts',(-6.72032886046213,-1.90985716099034,
30.5290945741019)) ;
#63273 = CARTESIAN_POINT('Ctrl Pts',(-6.7202632152564,-1.90885960968473,30.5288979355123)) ;
#63274 = CARTESIAN_POINT('Ctrl Pts',(-6.72016182003858,-1.90737915954795,
30.5286069816358)) ;
#63275 = CARTESIAN_POINT('Ctrl Pts',(-6.72012752413129,-1.90688832280964,
30.5285106665645)) ;
#63276 = CARTESIAN_POINT('Ctrl Pts',(-6.72005735934882,-1.90591232896256,
30.5283195845042)) ;
#63277 = CARTESIAN_POINT('Ctrl Pts',(-6.72002151396779,-1.90542717120432,
30.5282248122061)) ;
#63278 = CARTESIAN_POINT('Ctrl Pts',(-6.7199651260212,-1.90469706871886,30.5280827298087)) ;
#63279 = CARTESIAN_POINT('Ctrl Pts',(-6.71994458374831,-1.9044367396773,30.5280321642263)) ;
#63280 = CARTESIAN_POINT('Ctrl Pts',(-6.71990103088977,-1.90390388653279,
30.5279289958257)) ;
#63281 = CARTESIAN_POINT('Ctrl Pts',(-6.71987802529109,-1.90363136224242,
30.5278763918702)) ;
#63282 = CARTESIAN_POINT('Ctrl Pts',(-6.7198293861869,-1.90308662648624,30.5277718286008)) ;
#63283 = CARTESIAN_POINT('Ctrl Pts',(-6.71980384794353,-1.90281445382391,
30.5277198565293)) ;
#63284 = CARTESIAN_POINT('Ctrl Pts',(-6.71962399593059,-1.90163369887425,
30.5275095897043)) ;
#63285 = CARTESIAN_POINT('Ctrl Pts',(-6.7196165808276,-1.90158501763117,30.5275009206317)) ;
#63286 = CARTESIAN_POINT('Ctrl Pts',(-6.71960916572461,-1.9015363363881,30.527492251559)) ;
#63287 = CARTESIAN_POINT('Origin',(-2.46380912372341E-16,-1.34123521733712,
0.)) ;
#63288 = CARTESIAN_POINT('',(1.65824532362911E-15,-1.55431223447522E-15,-27.082990178354)) ;
#63289 = CARTESIAN_POINT('Origin',(-3.0463484597791E-31,-1.65835486166302E-15,
0.)) ;
#63290 = CARTESIAN_POINT('',(-5.46782640973375E-15,-2.68247043467423,-27.082990178354)) ;
#63291 = CARTESIAN_POINT('',(-5.22144549736141E-15,-1.34123521733712,-27.082990178354)) ;
#63292 = CARTESIAN_POINT('Origin',(-4.92761824744681E-16,-2.68247043467423,
0.)) ;
#63293 = CARTESIAN_POINT('Origin',(-3.49024337756996E-15,-19.,0.)) ;
#63294 = CARTESIAN_POINT('',(-7.96115465959473E-16,-20.,-23.5)) ;
#63295 = CARTESIAN_POINT('Origin',(-3.67394039744206E-15,-20.,0.)) ;
#63296 = CARTESIAN_POINT('',(-2.11260673051038E-15,-19.,-22.5)) ;
#63297 = CARTESIAN_POINT('Origin',(-6.36816335556624E-15,-19.,-23.5)) ;
#63298 = CARTESIAN_POINT('Origin',(-3.49024337756996E-15,-19.,0.)) ;
#63299 = CARTESIAN_POINT('Origin',(-1.83697019872104E-16,-1.,0.)) ;
#63300 = CARTESIAN_POINT('',(4.46981319145168E-15,-2.22044604925031E-15,-36.5)) ;
#63301 = CARTESIAN_POINT('Origin',(-4.10559240503683E-31,-2.23498040844392E-15,
0.)) ;
#63302 = CARTESIAN_POINT('',(2.11236405856052E-15,-1.,-37.5)) ;
#63303 = CARTESIAN_POINT('Origin',(-4.65365783675994E-15,-1.,-36.5)) ;
#63304 = CARTESIAN_POINT('Origin',(-1.83697019872103E-16,-1.,0.)) ;
#63305 = CARTESIAN_POINT('Origin',(-2.80137955304957E-15,-15.25,0.)) ;
#63306 = CARTESIAN_POINT('',(-5.05318474616943E-16,-15.25,-37.5)) ;
#63307 = CARTESIAN_POINT('Origin',(-2.80137955304957E-15,-15.25,0.)) ;
#63308 = CARTESIAN_POINT('',(1.71435485997076E-15,-15.5,-37.25)) ;
#63309 = CARTESIAN_POINT('Origin',(-7.36318887987346E-15,-15.25,-37.25)) ;
#63310 = CARTESIAN_POINT('Origin',(-2.8473038080176E-15,-15.5,0.)) ;
#63311 = CARTESIAN_POINT('Origin',(-1.76808381626899E-15,-9.625,0.)) ;
#63312 = CARTESIAN_POINT('',(2.70944004113232E-15,-0.250000000000001,-22.5)) ;
#63313 = CARTESIAN_POINT('',(-5.90126676339131E-15,-9.625,-22.5)) ;
#63314 = CARTESIAN_POINT('Origin',(-4.59242549680259E-17,-0.250000000000001,
0.)) ;
#63315 = CARTESIAN_POINT('Origin',(-4.59242549680255E-17,-0.249999999999999,
0.)) ;
#63316 = CARTESIAN_POINT('',(2.78597945494591E-15,-8.60422844084497E-16,-22.75)) ;
#63317 = CARTESIAN_POINT('Origin',(-2.83199572302825E-15,-0.249999999999999,
-22.75)) ;
#63318 = CARTESIAN_POINT('Origin',(-1.58419846794218E-31,-8.62397478764305E-16,
0.)) ;
#63319 = CARTESIAN_POINT('Origin',(-1.49253828646084E-15,-8.125,0.)) ;
#63320 = CARTESIAN_POINT('',(-8.3811765316647E-15,-8.125,-37.5)) ;
#63321 = CARTESIAN_POINT('Origin',(1.52569529784657E-15,-1.26037617021366E-15,
24.916495089177)) ;
#63322 = CARTESIAN_POINT('Origin',(-6.63803155591999E-16,-15.5,35.6592717826207)) ;
#63323 = CARTESIAN_POINT('Origin',(2.06246819519177E-15,-2.06246819519177E-15,
33.6826617540297)) ;
#63324 = CARTESIAN_POINT('Origin',(-3.58514725819224E-16,-2.169721598032,
29.82442706361)) ;
#63325 = CARTESIAN_POINT('Origin',(-4.47836258798674E-16,-2.43790704449357,
28.3905603778595)) ;
#63326 = CARTESIAN_POINT('Origin',(-4.47836258798674E-16,-2.43790704449357,
28.3905603778595)) ;
#63327 = CARTESIAN_POINT('Origin',(-6.41137021490582,-2.169721598032,29.1271485325977)) ;
#63328 = CARTESIAN_POINT('Origin',(-6.10313126226612,-2.43790704449357,27.7268048531459)) ;
#63329 = CARTESIAN_POINT('Origin',(-6.10313126226612,-2.43790704449357,27.7268048531459)) ;
#63330 = CARTESIAN_POINT('Origin',(-12.5229518842888,-2.169721598032,27.0679169087017)) ;
#63331 = CARTESIAN_POINT('Origin',(-11.9208868898519,-2.43790704449357,25.7665747496295)) ;
#63332 = CARTESIAN_POINT('Origin',(-11.9208868898519,-2.43790704449357,25.7665747496295)) ;
#63333 = CARTESIAN_POINT('Origin',(-18.0489742418239,-2.169721598032,23.7430195739836)) ;
#63334 = CARTESIAN_POINT('Origin',(-17.1812350955823,-2.43790704449357,22.6015282483114)) ;
#63335 = CARTESIAN_POINT('Origin',(-17.1812350955823,-2.43790704449357,22.6015282483114)) ;
#63336 = CARTESIAN_POINT('Origin',(-22.7310466238053,-2.169721598032,19.3079250324571)) ;
#63337 = CARTESIAN_POINT('Origin',(-21.6382078438147,-2.43790704449357,18.3796594058966)) ;
#63338 = CARTESIAN_POINT('Origin',(-21.6382078438147,-2.43790704449357,18.3796594058966)) ;
#63339 = CARTESIAN_POINT('Origin',(-26.3502405294014,-2.169721598032,13.9700133756302)) ;
#63340 = CARTESIAN_POINT('Origin',(-25.0834020424109,-2.43790704449357,13.2983781171864)) ;
#63341 = CARTESIAN_POINT('Origin',(-25.0834020424109,-2.43790704449357,13.2983781171864)) ;
#63342 = CARTESIAN_POINT('Origin',(-28.7373264740315,-2.169721598032,7.97887941991351)) ;
#63343 = CARTESIAN_POINT('Origin',(-27.3557242397031,-2.43790704449357,7.59527944780228)) ;
#63344 = CARTESIAN_POINT('Origin',(-27.3557242397031,-2.43790704449357,7.59527944780228)) ;
#63345 = CARTESIAN_POINT('Origin',(-29.7806869719803,-2.169721598032,1.61466193040923)) ;
#63346 = CARTESIAN_POINT('Origin',(-28.3489231752505,-2.43790704449357,1.53703395298571)) ;
#63347 = CARTESIAN_POINT('Origin',(-28.3489231752505,-2.43790704449357,1.53703395298571)) ;
#63348 = CARTESIAN_POINT('Origin',(-29.4315356459756,-2.169721598032,-4.82505535639315)) ;
#63349 = CARTESIAN_POINT('Origin',(-28.0165579706883,-2.43790704449357,-4.59308154118194)) ;
#63350 = CARTESIAN_POINT('Origin',(-28.0165579706883,-2.43790704449357,-4.59308154118194)) ;
#63351 = CARTESIAN_POINT('Origin',(-27.7061984239676,-2.169721598032,-11.0391584173944)) ;
#63352 = CARTESIAN_POINT('Origin',(-26.3741696535845,-2.43790704449357,-10.5084296473274)) ;
#63353 = CARTESIAN_POINT('Origin',(-26.3741696535845,-2.43790704449357,-10.5084296473274)) ;
#63354 = CARTESIAN_POINT('Origin',(-24.6853501568826,-2.169721598032,-16.7370826999417)) ;
#63355 = CARTESIAN_POINT('Origin',(-23.4985544762632,-2.43790704449357,-15.9324152624445)) ;
#63356 = CARTESIAN_POINT('Origin',(-23.4985544762632,-2.43790704449357,-15.9324152624445)) ;
#63357 = CARTESIAN_POINT('Origin',(-20.510242352258,-2.169721598032,-21.6523995973711)) ;
#63358 = CARTESIAN_POINT('Origin',(-19.5241730083994,-2.43790704449357,-20.6114188474975)) ;
#63359 = CARTESIAN_POINT('Origin',(-19.5241730083994,-2.43790704449357,-20.6114188474975)) ;
#63360 = CARTESIAN_POINT('Origin',(-15.3760984107389,-2.169721598032,-25.5552743545411)) ;
#63361 = CARTESIAN_POINT('Origin',(-14.6368629102226,-2.43790704449357,-24.3266553951882)) ;
#63362 = CARTESIAN_POINT('Origin',(-14.6368629102226,-2.43790704449357,-24.3266553951882)) ;
#63363 = CARTESIAN_POINT('Origin',(-9.52298519683959,-2.169721598032,-28.2632128855402)) ;
#63364 = CARTESIAN_POINT('Origin',(-9.06514937006846,-2.43790704449357,-26.9044045737354)) ;
#63365 = CARTESIAN_POINT('Origin',(-9.06514937006846,-2.43790704449357,-26.9044045737354)) ;
#63366 = CARTESIAN_POINT('Origin',(-3.22458777917394,-2.169721598032,-29.6495949943164)) ;
#63367 = CARTESIAN_POINT('Origin',(-3.0695595205598,-2.43790704449357,-28.2241336965128)) ;
#63368 = CARTESIAN_POINT('Origin',(-3.0695595205598,-2.43790704449357,-28.2241336965128)) ;
#63369 = CARTESIAN_POINT('Origin',(3.22458777917398,-2.169721598032,-29.6495949943164)) ;
#63370 = CARTESIAN_POINT('Origin',(3.06955952055985,-2.43790704449357,-28.2241336965128)) ;
#63371 = CARTESIAN_POINT('Origin',(3.06955952055985,-2.43790704449357,-28.2241336965128)) ;
#63372 = CARTESIAN_POINT('Origin',(9.52298519683963,-2.169721598032,-28.2632128855402)) ;
#63373 = CARTESIAN_POINT('Origin',(9.0651493700685,-2.43790704449358,-26.9044045737354)) ;
#63374 = CARTESIAN_POINT('Origin',(9.0651493700685,-2.43790704449358,-26.9044045737354)) ;
#63375 = CARTESIAN_POINT('Origin',(15.3760984107389,-2.16972159803201,-25.5552743545411)) ;
#63376 = CARTESIAN_POINT('Origin',(14.6368629102226,-2.43790704449358,-24.3266553951881)) ;
#63377 = CARTESIAN_POINT('Origin',(14.6368629102226,-2.43790704449358,-24.3266553951881)) ;
#63378 = CARTESIAN_POINT('Origin',(20.510242352258,-2.16972159803201,-21.6523995973711)) ;
#63379 = CARTESIAN_POINT('Origin',(19.5241730083995,-2.43790704449358,-20.6114188474975)) ;
#63380 = CARTESIAN_POINT('Origin',(19.5241730083995,-2.43790704449358,-20.6114188474975)) ;
#63381 = CARTESIAN_POINT('Origin',(24.6853501568826,-2.16972159803201,-16.7370826999417)) ;
#63382 = CARTESIAN_POINT('Origin',(23.4985544762633,-2.43790704449358,-15.9324152624445)) ;
#63383 = CARTESIAN_POINT('Origin',(23.4985544762633,-2.43790704449358,-15.9324152624445)) ;
#63384 = CARTESIAN_POINT('Origin',(27.7061984239676,-2.16972159803201,-11.0391584173944)) ;
#63385 = CARTESIAN_POINT('Origin',(26.3741696535845,-2.43790704449358,-10.5084296473274)) ;
#63386 = CARTESIAN_POINT('Origin',(26.3741696535845,-2.43790704449358,-10.5084296473274)) ;
#63387 = CARTESIAN_POINT('Origin',(29.4315356459756,-2.16972159803201,-4.82505535639311)) ;
#63388 = CARTESIAN_POINT('Origin',(28.0165579706883,-2.43790704449358,-4.5930815411819)) ;
#63389 = CARTESIAN_POINT('Origin',(28.0165579706883,-2.43790704449358,-4.5930815411819)) ;
#63390 = CARTESIAN_POINT('Origin',(29.7806869719803,-2.16972159803201,1.61466193040926)) ;
#63391 = CARTESIAN_POINT('Origin',(28.3489231752505,-2.43790704449358,1.53703395298574)) ;
#63392 = CARTESIAN_POINT('Origin',(28.3489231752505,-2.43790704449358,1.53703395298574)) ;
#63393 = CARTESIAN_POINT('Origin',(28.7373264740315,-2.16972159803201,7.97887941991354)) ;
#63394 = CARTESIAN_POINT('Origin',(27.3557242397031,-2.43790704449358,7.59527944780231)) ;
#63395 = CARTESIAN_POINT('Origin',(27.3557242397031,-2.43790704449358,7.59527944780231)) ;
#63396 = CARTESIAN_POINT('Origin',(26.3502405294014,-2.16972159803201,13.9700133756302)) ;
#63397 = CARTESIAN_POINT('Origin',(25.0834020424109,-2.43790704449358,13.2983781171864)) ;
#63398 = CARTESIAN_POINT('Origin',(25.0834020424109,-2.43790704449358,13.2983781171864)) ;
#63399 = CARTESIAN_POINT('Origin',(22.7310466238053,-2.169721598032,19.3079250324571)) ;
#63400 = CARTESIAN_POINT('Origin',(21.6382078438146,-2.43790704449357,18.3796594058967)) ;
#63401 = CARTESIAN_POINT('Origin',(21.6382078438146,-2.43790704449357,18.3796594058967)) ;
#63402 = CARTESIAN_POINT('Origin',(18.0489742418238,-2.16972159803201,23.7430195739837)) ;
#63403 = CARTESIAN_POINT('Origin',(17.1812350955823,-2.43790704449358,22.6015282483114)) ;
#63404 = CARTESIAN_POINT('Origin',(17.1812350955823,-2.43790704449358,22.6015282483114)) ;
#63405 = CARTESIAN_POINT('Origin',(12.5229518842888,-2.169721598032,27.0679169087017)) ;
#63406 = CARTESIAN_POINT('Origin',(11.9208868898518,-2.43790704449357,25.7665747496295)) ;
#63407 = CARTESIAN_POINT('Origin',(11.9208868898518,-2.43790704449357,25.7665747496295)) ;
#63408 = CARTESIAN_POINT('Origin',(-2.05716802131569E-15,-20.,26.4038966541541)) ;
#63409 = CARTESIAN_POINT('Origin',(6.41137021490578,-2.169721598032,29.1271485325977)) ;
#63410 = CARTESIAN_POINT('Origin',(6.10313126226608,-2.43790704449357,27.7268048531459)) ;
#63411 = CARTESIAN_POINT('Origin',(6.10313126226608,-2.43790704449357,27.7268048531459)) ;
#63412 = CARTESIAN_POINT('Origin',(-5.19563909059739E-16,-2.82837418604547,
0.)) ;
#63413 = CARTESIAN_POINT('',(-5.35132983144392E-15,-2.82837418604547,-26.3029085923563)) ;
#63414 = CARTESIAN_POINT('Origin',(-1.65855445878407E-15,-9.028749948904,
29.6232887510362)) ;
#63415 = CARTESIAN_POINT('Origin',(-2.86927265876946E-15,-15.6195928533144,
30.8560171242128)) ;
#63416 = CARTESIAN_POINT('Origin',(-2.86927265876946E-15,-15.6195928533144,
30.8560171242128)) ;
#63417 = CARTESIAN_POINT('Origin',(-2.77219341593235E-15,-15.3281150963394,
32.4144172942372)) ;
#63418 = CARTESIAN_POINT('Origin',(-2.86927265876946E-15,-15.6195928533144,
30.8560171242128)) ;
#63419 = CARTESIAN_POINT('Origin',(-2.86927265876946E-15,-15.6195928533144,
30.8560171242128)) ;
#63420 = CARTESIAN_POINT('Origin',(-1.65855445878407E-15,-9.028749948904,
29.6232887510362)) ;
#63421 = CARTESIAN_POINT('Origin',(-6.36813142330852,-9.028749948904,28.9307127219973)) ;
#63422 = CARTESIAN_POINT('Origin',(-6.63313158435093,-15.6195928533144,30.1346205908487)) ;
#63423 = CARTESIAN_POINT('Origin',(-6.63313158435093,-15.6195928533144,30.1346205908487)) ;
#63424 = CARTESIAN_POINT('Origin',(-6.968141554926,-15.3281150963394,31.6565862309166)) ;
#63425 = CARTESIAN_POINT('Origin',(-6.63313158435093,-15.6195928533144,30.1346205908487)) ;
#63426 = CARTESIAN_POINT('Origin',(-6.63313158435093,-15.6195928533144,30.1346205908487)) ;
#63427 = CARTESIAN_POINT('Origin',(-6.36813142330852,-9.028749948904,28.9307127219973)) ;
#63428 = CARTESIAN_POINT('Origin',(-12.4384960989329,-9.028749948904,26.8853687202556)) ;
#63429 = CARTESIAN_POINT('Origin',(-12.9561053080139,-15.6195928533144,28.0041626908817)) ;
#63430 = CARTESIAN_POINT('Origin',(-12.9561053080139,-15.6195928533144,28.0041626908817)) ;
#63431 = CARTESIAN_POINT('Origin',(-13.6104605552768,-15.3281150963394,29.4185283792068)) ;
#63432 = CARTESIAN_POINT('Origin',(-12.9561053080139,-15.6195928533144,28.0041626908817)) ;
#63433 = CARTESIAN_POINT('Origin',(-12.9561053080139,-15.6195928533144,28.0041626908817)) ;
#63434 = CARTESIAN_POINT('Origin',(-12.4384960989329,-9.028749948904,26.8853687202556)) ;
#63435 = CARTESIAN_POINT('Origin',(-17.9272505213666,-9.02874994890399,23.5828947580959)) ;
#63436 = CARTESIAN_POINT('Origin',(-18.6732659471509,-15.6195928533144,24.5642612678804)) ;
#63437 = CARTESIAN_POINT('Origin',(-18.6732659471509,-15.6195928533144,24.5642612678804)) ;
#63438 = CARTESIAN_POINT('Origin',(-19.6163695470032,-15.3281150963394,25.8048928368313)) ;
#63439 = CARTESIAN_POINT('Origin',(-18.6732659471509,-15.6195928533144,24.5642612678804)) ;
#63440 = CARTESIAN_POINT('Origin',(-18.6732659471509,-15.6195928533144,24.5642612678804)) ;
#63441 = CARTESIAN_POINT('Origin',(-17.9272505213666,-9.02874994890399,23.5828947580959)) ;
#63442 = CARTESIAN_POINT('Origin',(-22.5777466341291,-9.02874994890399,19.1777108475526)) ;
#63443 = CARTESIAN_POINT('Origin',(-23.5172854244436,-15.6195928533144,19.9757622892086)) ;
#63444 = CARTESIAN_POINT('Origin',(-23.5172854244436,-15.6195928533144,19.9757622892086)) ;
#63445 = CARTESIAN_POINT('Origin',(-24.7050389007406,-15.3281150963394,20.984649185484)) ;
#63446 = CARTESIAN_POINT('Origin',(-23.5172854244436,-15.6195928533144,19.9757622892086)) ;
#63447 = CARTESIAN_POINT('Origin',(-23.5172854244436,-15.6195928533144,19.9757622892086)) ;
#63448 = CARTESIAN_POINT('Origin',(-22.5777466341291,-9.02874994890399,19.1777108475526)) ;
#63449 = CARTESIAN_POINT('Origin',(-26.1725324076428,-9.02874994890399,13.8757984922725)) ;
#63450 = CARTESIAN_POINT('Origin',(-27.2616627728748,-15.6195928533144,14.4532188673586)) ;
#63451 = CARTESIAN_POINT('Origin',(-27.2616627728748,-15.6195928533144,14.4532188673586)) ;
#63452 = CARTESIAN_POINT('Origin',(-28.638528093158,-15.3281150963394,15.183186660986)) ;
#63453 = CARTESIAN_POINT('Origin',(-27.2616627728748,-15.6195928533144,14.4532188673586)) ;
#63454 = CARTESIAN_POINT('Origin',(-27.2616627728748,-15.6195928533144,14.4532188673586)) ;
#63455 = CARTESIAN_POINT('Origin',(-26.1725324076428,-9.02874994890399,13.8757984922725)) ;
#63456 = CARTESIAN_POINT('Origin',(-28.5435196544557,-9.02874994890399,7.92506922133606)) ;
#63457 = CARTESIAN_POINT('Origin',(-29.7313150692083,-15.6195928533144,8.25485899486984)) ;
#63458 = CARTESIAN_POINT('Origin',(-29.7313150692083,-15.6195928533144,8.25485899486984)) ;
#63459 = CARTESIAN_POINT('Origin',(-31.2329115413772,-15.3281150963394,8.67177520312011)) ;
#63460 = CARTESIAN_POINT('Origin',(-29.7313150692083,-15.6195928533144,8.25485899486984)) ;
#63461 = CARTESIAN_POINT('Origin',(-29.7313150692083,-15.6195928533144,8.25485899486984)) ;
#63462 = CARTESIAN_POINT('Origin',(-28.5435196544557,-9.02874994890399,7.92506922133606)) ;
#63463 = CARTESIAN_POINT('Origin',(-29.5798436460697,-9.02874994890399,1.60377252169177)) ;
#63464 = CARTESIAN_POINT('Origin',(-30.810764116889,-15.6195928533144,1.67051109039783)) ;
#63465 = CARTESIAN_POINT('Origin',(-30.810764116889,-15.6195928533144,1.67051109039783)) ;
#63466 = CARTESIAN_POINT('Origin',(-32.3668787588096,-15.3281150963394,1.75488117474228)) ;
#63467 = CARTESIAN_POINT('Origin',(-30.810764116889,-15.6195928533144,1.67051109039783)) ;
#63468 = CARTESIAN_POINT('Origin',(-30.810764116889,-15.6195928533144,1.67051109039783)) ;
#63469 = CARTESIAN_POINT('Origin',(-29.5798436460697,-9.02874994890399,1.60377252169177)) ;
#63470 = CARTESIAN_POINT('Origin',(-29.2330470244285,-9.02874994890399,-4.79251479860169)) ;
#63471 = CARTESIAN_POINT('Origin',(-30.4495360781687,-15.6195928533144,-4.99194805602145)) ;
#63472 = CARTESIAN_POINT('Origin',(-30.4495360781687,-15.6195928533144,-4.99194805602145)) ;
#63473 = CARTESIAN_POINT('Origin',(-31.987406698682,-15.3281150963394,-5.24406914695616)) ;
#63474 = CARTESIAN_POINT('Origin',(-30.4495360781687,-15.6195928533144,-4.99194805602145)) ;
#63475 = CARTESIAN_POINT('Origin',(-30.4495360781687,-15.6195928533144,-4.99194805602145)) ;
#63476 = CARTESIAN_POINT('Origin',(-29.2330470244285,-9.02874994890399,-4.79251479860169)) ;
#63477 = CARTESIAN_POINT('Origin',(-27.5193456141232,-9.02874994890399,-10.9647094534102)) ;
#63478 = CARTESIAN_POINT('Origin',(-28.664521574662,-15.6195928533144,-11.4209892594929)) ;
#63479 = CARTESIAN_POINT('Origin',(-28.664521574662,-15.6195928533144,-11.4209892594929)) ;
#63480 = CARTESIAN_POINT('Origin',(-30.1122390527731,-15.3281150963394,-11.9978126237072)) ;
#63481 = CARTESIAN_POINT('Origin',(-28.664521574662,-15.6195928533144,-11.4209892594929)) ;
#63482 = CARTESIAN_POINT('Origin',(-28.664521574662,-15.6195928533144,-11.4209892594929)) ;
#63483 = CARTESIAN_POINT('Origin',(-27.5193456141232,-9.02874994890399,-10.9647094534102)) ;
#63484 = CARTESIAN_POINT('Origin',(-24.5188701884574,-9.028749948904,-16.6242064805765)) ;
#63485 = CARTESIAN_POINT('Origin',(-25.5391859006516,-15.6195928533144,-17.3159976987084)) ;
#63486 = CARTESIAN_POINT('Origin',(-25.5391859006516,-15.6195928533144,-17.3159976987084)) ;
#63487 = CARTESIAN_POINT('Origin',(-26.8290565761066,-15.3281150963394,-18.1905517167846)) ;
#63488 = CARTESIAN_POINT('Origin',(-25.5391859006516,-15.6195928533144,-17.3159976987084)) ;
#63489 = CARTESIAN_POINT('Origin',(-25.5391859006516,-15.6195928533144,-17.3159976987084)) ;
#63490 = CARTESIAN_POINT('Origin',(-24.5188701884574,-9.028749948904,-16.6242064805765)) ;
#63491 = CARTESIAN_POINT('Origin',(-20.3719196435463,-9.028749948904,-21.5063740891895)) ;
#63492 = CARTESIAN_POINT('Origin',(-21.2196662786931,-15.6195928533144,-22.4013293308814)) ;
#63493 = CARTESIAN_POINT('Origin',(-21.2196662786931,-15.6195928533144,-22.4013293308814)) ;
#63494 = CARTESIAN_POINT('Origin',(-22.2913772322959,-15.3281150963394,-23.5327208289314)) ;
#63495 = CARTESIAN_POINT('Origin',(-21.2196662786931,-15.6195928533144,-22.4013293308814)) ;
#63496 = CARTESIAN_POINT('Origin',(-21.2196662786931,-15.6195928533144,-22.4013293308814)) ;
#63497 = CARTESIAN_POINT('Origin',(-20.3719196435463,-9.028749948904,-21.5063740891895)) ;
#63498 = CARTESIAN_POINT('Origin',(-15.2724007778654,-9.028749948904,-25.38292754801)) ;
#63499 = CARTESIAN_POINT('Origin',(-15.9079386455081,-15.6195928533144,-26.4391997008318)) ;
#63500 = CARTESIAN_POINT('Origin',(-15.9079386455081,-15.6195928533144,-26.4391997008318)) ;
#63501 = CARTESIAN_POINT('Origin',(-16.7113778641895,-15.3281150963394,-27.7745260698579)) ;
#63502 = CARTESIAN_POINT('Origin',(-15.9079386455081,-15.6195928533144,-26.4391997008318)) ;
#63503 = CARTESIAN_POINT('Origin',(-15.9079386455081,-15.6195928533144,-26.4391997008318)) ;
#63504 = CARTESIAN_POINT('Origin',(-15.2724007778654,-9.028749948904,-25.38292754801)) ;
#63505 = CARTESIAN_POINT('Origin',(-9.45876142586579,-9.028749948904,-28.0726035257833)) ;
#63506 = CARTESIAN_POINT('Origin',(-9.85237348166313,-15.6195928533144,-29.2408024778311)) ;
#63507 = CARTESIAN_POINT('Origin',(-9.85237348166313,-15.6195928533144,-29.2408024778311)) ;
#63508 = CARTESIAN_POINT('Origin',(-10.3499730405161,-15.3281150963394,-30.7176253409266)) ;
#63509 = CARTESIAN_POINT('Origin',(-9.85237348166313,-15.6195928533144,-29.2408024778311)) ;
#63510 = CARTESIAN_POINT('Origin',(-9.85237348166313,-15.6195928533144,-29.2408024778311)) ;
#63511 = CARTESIAN_POINT('Origin',(-9.45876142586579,-9.028749948904,-28.0726035257833)) ;
#63512 = CARTESIAN_POINT('Origin',(-3.20284090225101,-9.028749948904,-29.4496357631488)) ;
#63513 = CARTESIAN_POINT('Origin',(-3.33612228394221,-15.6195928533144,-30.6751378297849)) ;
#63514 = CARTESIAN_POINT('Origin',(-3.33612228394221,-15.6195928533144,-30.6751378297849)) ;
#63515 = CARTESIAN_POINT('Origin',(-3.50461498063695,-15.3281150963394,-32.2244025912419)) ;
#63516 = CARTESIAN_POINT('Origin',(-3.33612228394221,-15.6195928533144,-30.6751378297849)) ;
#63517 = CARTESIAN_POINT('Origin',(-3.33612228394221,-15.6195928533144,-30.6751378297849)) ;
#63518 = CARTESIAN_POINT('Origin',(-3.20284090225101,-9.028749948904,-29.4496357631488)) ;
#63519 = CARTESIAN_POINT('Origin',(3.20284090225105,-9.028749948904,-29.4496357631488)) ;
#63520 = CARTESIAN_POINT('Origin',(3.33612228394225,-15.6195928533144,-30.6751378297849)) ;
#63521 = CARTESIAN_POINT('Origin',(3.33612228394225,-15.6195928533144,-30.6751378297849)) ;
#63522 = CARTESIAN_POINT('Origin',(3.50461498063699,-15.3281150963394,-32.2244025912419)) ;
#63523 = CARTESIAN_POINT('Origin',(3.33612228394225,-15.6195928533144,-30.6751378297849)) ;
#63524 = CARTESIAN_POINT('Origin',(3.33612228394225,-15.6195928533144,-30.6751378297849)) ;
#63525 = CARTESIAN_POINT('Origin',(3.20284090225105,-9.028749948904,-29.4496357631488)) ;
#63526 = CARTESIAN_POINT('Origin',(9.45876142586583,-9.028749948904,-28.0726035257833)) ;
#63527 = CARTESIAN_POINT('Origin',(9.85237348166317,-15.6195928533144,-29.2408024778311)) ;
#63528 = CARTESIAN_POINT('Origin',(9.85237348166317,-15.6195928533144,-29.2408024778311)) ;
#63529 = CARTESIAN_POINT('Origin',(10.3499730405161,-15.3281150963394,-30.7176253409265)) ;
#63530 = CARTESIAN_POINT('Origin',(9.85237348166317,-15.6195928533144,-29.2408024778311)) ;
#63531 = CARTESIAN_POINT('Origin',(9.85237348166317,-15.6195928533144,-29.2408024778311)) ;
#63532 = CARTESIAN_POINT('Origin',(9.45876142586583,-9.028749948904,-28.0726035257833)) ;
#63533 = CARTESIAN_POINT('Origin',(15.2724007778654,-9.02874994890401,-25.3829275480099)) ;
#63534 = CARTESIAN_POINT('Origin',(15.9079386455082,-15.6195928533144,-26.4391997008318)) ;
#63535 = CARTESIAN_POINT('Origin',(15.9079386455082,-15.6195928533144,-26.4391997008318)) ;
#63536 = CARTESIAN_POINT('Origin',(16.7113778641896,-15.3281150963394,-27.7745260698579)) ;
#63537 = CARTESIAN_POINT('Origin',(15.9079386455082,-15.6195928533144,-26.4391997008318)) ;
#63538 = CARTESIAN_POINT('Origin',(15.9079386455082,-15.6195928533144,-26.4391997008318)) ;
#63539 = CARTESIAN_POINT('Origin',(15.2724007778654,-9.02874994890401,-25.3829275480099)) ;
#63540 = CARTESIAN_POINT('Origin',(20.3719196435463,-9.02874994890401,-21.5063740891894)) ;
#63541 = CARTESIAN_POINT('Origin',(21.2196662786931,-15.6195928533144,-22.4013293308814)) ;
#63542 = CARTESIAN_POINT('Origin',(21.2196662786931,-15.6195928533144,-22.4013293308814)) ;
#63543 = CARTESIAN_POINT('Origin',(22.291377232296,-15.3281150963394,-23.5327208289313)) ;
#63544 = CARTESIAN_POINT('Origin',(21.2196662786931,-15.6195928533144,-22.4013293308814)) ;
#63545 = CARTESIAN_POINT('Origin',(21.2196662786931,-15.6195928533144,-22.4013293308814)) ;
#63546 = CARTESIAN_POINT('Origin',(20.3719196435463,-9.02874994890401,-21.5063740891894)) ;
#63547 = CARTESIAN_POINT('Origin',(24.5188701884574,-9.02874994890401,-16.6242064805764)) ;
#63548 = CARTESIAN_POINT('Origin',(25.5391859006516,-15.6195928533144,-17.3159976987084)) ;
#63549 = CARTESIAN_POINT('Origin',(25.5391859006516,-15.6195928533144,-17.3159976987084)) ;
#63550 = CARTESIAN_POINT('Origin',(26.8290565761066,-15.3281150963394,-18.1905517167846)) ;
#63551 = CARTESIAN_POINT('Origin',(25.5391859006516,-15.6195928533144,-17.3159976987084)) ;
#63552 = CARTESIAN_POINT('Origin',(25.5391859006516,-15.6195928533144,-17.3159976987084)) ;
#63553 = CARTESIAN_POINT('Origin',(24.5188701884574,-9.02874994890401,-16.6242064805764)) ;
#63554 = CARTESIAN_POINT('Origin',(27.5193456141232,-9.02874994890401,-10.9647094534101)) ;
#63555 = CARTESIAN_POINT('Origin',(28.664521574662,-15.6195928533144,-11.4209892594929)) ;
#63556 = CARTESIAN_POINT('Origin',(28.664521574662,-15.6195928533144,-11.4209892594929)) ;
#63557 = CARTESIAN_POINT('Origin',(30.1122390527732,-15.3281150963394,-11.9978126237071)) ;
#63558 = CARTESIAN_POINT('Origin',(28.664521574662,-15.6195928533144,-11.4209892594929)) ;
#63559 = CARTESIAN_POINT('Origin',(28.664521574662,-15.6195928533144,-11.4209892594929)) ;
#63560 = CARTESIAN_POINT('Origin',(27.5193456141232,-9.02874994890401,-10.9647094534101)) ;
#63561 = CARTESIAN_POINT('Origin',(29.2330470244285,-9.02874994890401,-4.79251479860166)) ;
#63562 = CARTESIAN_POINT('Origin',(30.4495360781687,-15.6195928533144,-4.99194805602142)) ;
#63563 = CARTESIAN_POINT('Origin',(30.4495360781687,-15.6195928533144,-4.99194805602142)) ;
#63564 = CARTESIAN_POINT('Origin',(31.987406698682,-15.3281150963394,-5.24406914695613)) ;
#63565 = CARTESIAN_POINT('Origin',(30.4495360781687,-15.6195928533144,-4.99194805602142)) ;
#63566 = CARTESIAN_POINT('Origin',(30.4495360781687,-15.6195928533144,-4.99194805602142)) ;
#63567 = CARTESIAN_POINT('Origin',(29.2330470244285,-9.02874994890401,-4.79251479860166)) ;
#63568 = CARTESIAN_POINT('Origin',(29.5798436460697,-9.02874994890401,1.6037725216918)) ;
#63569 = CARTESIAN_POINT('Origin',(30.810764116889,-15.6195928533144,1.67051109039787)) ;
#63570 = CARTESIAN_POINT('Origin',(30.810764116889,-15.6195928533144,1.67051109039787)) ;
#63571 = CARTESIAN_POINT('Origin',(32.3668787588096,-15.3281150963394,1.75488117474232)) ;
#63572 = CARTESIAN_POINT('Origin',(30.810764116889,-15.6195928533144,1.67051109039787)) ;
#63573 = CARTESIAN_POINT('Origin',(30.810764116889,-15.6195928533144,1.67051109039787)) ;
#63574 = CARTESIAN_POINT('Origin',(29.5798436460697,-9.02874994890401,1.6037725216918)) ;
#63575 = CARTESIAN_POINT('Origin',(28.5435196544557,-9.02874994890401,7.92506922133609)) ;
#63576 = CARTESIAN_POINT('Origin',(29.7313150692083,-15.6195928533144,8.25485899486987)) ;
#63577 = CARTESIAN_POINT('Origin',(29.7313150692083,-15.6195928533144,8.25485899486987)) ;
#63578 = CARTESIAN_POINT('Origin',(31.2329115413772,-15.3281150963394,8.67177520312015)) ;
#63579 = CARTESIAN_POINT('Origin',(29.7313150692083,-15.6195928533144,8.25485899486987)) ;
#63580 = CARTESIAN_POINT('Origin',(29.7313150692083,-15.6195928533144,8.25485899486987)) ;
#63581 = CARTESIAN_POINT('Origin',(28.5435196544557,-9.02874994890401,7.92506922133609)) ;
#63582 = CARTESIAN_POINT('Origin',(26.1725324076428,-9.02874994890401,13.8757984922725)) ;
#63583 = CARTESIAN_POINT('Origin',(27.2616627728747,-15.6195928533144,14.4532188673586)) ;
#63584 = CARTESIAN_POINT('Origin',(27.2616627728747,-15.6195928533144,14.4532188673586)) ;
#63585 = CARTESIAN_POINT('Origin',(28.638528093158,-15.3281150963394,15.183186660986)) ;
#63586 = CARTESIAN_POINT('Origin',(27.2616627728747,-15.6195928533144,14.4532188673586)) ;
#63587 = CARTESIAN_POINT('Origin',(27.2616627728747,-15.6195928533144,14.4532188673586)) ;
#63588 = CARTESIAN_POINT('Origin',(26.1725324076428,-9.02874994890401,13.8757984922725)) ;
#63589 = CARTESIAN_POINT('Origin',(22.5777466341291,-9.028749948904,19.1777108475526)) ;
#63590 = CARTESIAN_POINT('Origin',(23.5172854244436,-15.6195928533144,19.9757622892086)) ;
#63591 = CARTESIAN_POINT('Origin',(23.5172854244436,-15.6195928533144,19.9757622892086)) ;
#63592 = CARTESIAN_POINT('Origin',(24.7050389007406,-15.3281150963394,20.9846491854841)) ;
#63593 = CARTESIAN_POINT('Origin',(23.5172854244436,-15.6195928533144,19.9757622892086)) ;
#63594 = CARTESIAN_POINT('Origin',(23.5172854244436,-15.6195928533144,19.9757622892086)) ;
#63595 = CARTESIAN_POINT('Origin',(22.5777466341291,-9.028749948904,19.1777108475526)) ;
#63596 = CARTESIAN_POINT('Origin',(17.9272505213666,-9.028749948904,23.5828947580959)) ;
#63597 = CARTESIAN_POINT('Origin',(18.6732659471508,-15.6195928533144,24.5642612678805)) ;
#63598 = CARTESIAN_POINT('Origin',(18.6732659471508,-15.6195928533144,24.5642612678805)) ;
#63599 = CARTESIAN_POINT('Origin',(19.6163695470032,-15.3281150963394,25.8048928368313)) ;
#63600 = CARTESIAN_POINT('Origin',(18.6732659471508,-15.6195928533144,24.5642612678805)) ;
#63601 = CARTESIAN_POINT('Origin',(18.6732659471508,-15.6195928533144,24.5642612678805)) ;
#63602 = CARTESIAN_POINT('Origin',(17.9272505213666,-9.028749948904,23.5828947580959)) ;
#63603 = CARTESIAN_POINT('Origin',(12.4384960989328,-9.028749948904,26.8853687202556)) ;
#63604 = CARTESIAN_POINT('Origin',(12.9561053080138,-15.6195928533144,28.0041626908817)) ;
#63605 = CARTESIAN_POINT('Origin',(12.9561053080138,-15.6195928533144,28.0041626908817)) ;
#63606 = CARTESIAN_POINT('Origin',(13.6104605552767,-15.3281150963394,29.4185283792069)) ;
#63607 = CARTESIAN_POINT('Origin',(12.9561053080138,-15.6195928533144,28.0041626908817)) ;
#63608 = CARTESIAN_POINT('Origin',(12.9561053080138,-15.6195928533144,28.0041626908817)) ;
#63609 = CARTESIAN_POINT('Origin',(12.4384960989328,-9.028749948904,26.8853687202556)) ;
#63610 = CARTESIAN_POINT('Origin',(6.36813142330848,-9.028749948904,28.9307127219973)) ;
#63611 = CARTESIAN_POINT('Origin',(6.63313158435088,-15.6195928533144,30.1346205908487)) ;
#63612 = CARTESIAN_POINT('Origin',(6.63313158435088,-15.6195928533144,30.1346205908487)) ;
#63613 = CARTESIAN_POINT('Origin',(6.96814155492595,-15.3281150963394,31.6565862309166)) ;
#63614 = CARTESIAN_POINT('Origin',(6.63313158435088,-15.6195928533144,30.1346205908487)) ;
#63615 = CARTESIAN_POINT('Origin',(6.63313158435088,-15.6195928533144,30.1346205908487)) ;
#63616 = CARTESIAN_POINT('Origin',(6.36813142330848,-9.028749948904,28.9307127219973)) ;
#63617 = CARTESIAN_POINT('',(0.,0.,0.)) ;
#63618 = CARTESIAN_POINT('Origin',(0.,0.,0.1)) ;
#63619 = CARTESIAN_POINT('',(-36.5,4.46996081688784E-15,0.2)) ;
#63620 = CARTESIAN_POINT('Origin',(0.,0.,0.2)) ;
#63621 = CARTESIAN_POINT('',(-36.3,-4.44546788090489E-15,0.)) ;
#63622 = CARTESIAN_POINT('',(-36.4,-4.45771434889637E-15,0.1)) ;
#63623 = CARTESIAN_POINT('Origin',(0.,0.,0.)) ;
#63624 = CARTESIAN_POINT('Origin',(0.,0.,0.)) ;
#63625 = CARTESIAN_POINT('',(-22.7,2.77994823406449E-15,0.)) ;
#63626 = CARTESIAN_POINT('Origin',(0.,0.,0.)) ;
#63627 = CARTESIAN_POINT('Origin',(0.,0.,0.)) ;
#63628 = CARTESIAN_POINT('',(-36.5,-4.46996081688784E-15,3.8)) ;
#63629 = CARTESIAN_POINT('Origin',(0.,0.,3.8)) ;
#63630 = CARTESIAN_POINT('',(-36.5,-4.46996081688784E-15,0.)) ;
#63631 = CARTESIAN_POINT('Origin',(0.,0.,0.1)) ;
#63632 = CARTESIAN_POINT('',(-22.5,-2.75545529808154E-15,0.2)) ;
#63633 = CARTESIAN_POINT('Origin',(0.,0.,0.2)) ;
#63634 = CARTESIAN_POINT('',(-22.6,2.76770176607302E-15,0.1)) ;
#63635 = CARTESIAN_POINT('Origin',(0.,0.,0.)) ;
#63636 = CARTESIAN_POINT('',(-22.5,2.75545529808154E-15,3.8)) ;
#63637 = CARTESIAN_POINT('',(-22.5,-2.75545529808154E-15,0.)) ;
#63638 = CARTESIAN_POINT('Origin',(0.,0.,3.8)) ;
#63639 = CARTESIAN_POINT('Origin',(0.,0.,3.9)) ;
#63640 = CARTESIAN_POINT('',(-36.3,4.44546788090489E-15,4.)) ;
#63641 = CARTESIAN_POINT('',(-36.4,4.45771434889637E-15,3.9)) ;
#63642 = CARTESIAN_POINT('Origin',(0.,0.,4.)) ;
#63643 = CARTESIAN_POINT('Origin',(0.,0.,4.)) ;
#63644 = CARTESIAN_POINT('',(-22.7,-2.77994823406449E-15,4.)) ;
#63645 = CARTESIAN_POINT('Origin',(0.,0.,4.)) ;
#63646 = CARTESIAN_POINT('Origin',(0.,0.,3.9)) ;
#63647 = CARTESIAN_POINT('',(-22.6,-2.76770176607302E-15,3.9)) ;
#63648 = CARTESIAN_POINT('',(0.,0.,0.)) ;
#63649 = CARTESIAN_POINT('Origin',(45.,354.45,-22.)) ;
#63650 = CARTESIAN_POINT('',(48.3,354.45,-30.)) ;
#63651 = CARTESIAN_POINT('Origin',(45.,354.45,-30.)) ;
#63652 = CARTESIAN_POINT('',(48.3,354.45,-24.)) ;
#63653 = CARTESIAN_POINT('',(48.3,354.45,-22.)) ;
#63654 = CARTESIAN_POINT('Origin',(45.,354.45,-24.)) ;
#63655 = CARTESIAN_POINT('Origin',(-5.51091059616309E-15,399.45,-22.)) ;
#63656 = CARTESIAN_POINT('',(3.29999999999999,399.45,-30.)) ;
#63657 = CARTESIAN_POINT('Origin',(-5.51091059616309E-15,399.45,-30.)) ;
#63658 = CARTESIAN_POINT('',(3.29999999999999,399.45,-24.)) ;
#63659 = CARTESIAN_POINT('',(3.29999999999999,399.45,-22.)) ;
#63660 = CARTESIAN_POINT('Origin',(-5.51091059616309E-15,399.45,-24.)) ;
#63661 = CARTESIAN_POINT('Origin',(-45.,354.45,-22.)) ;
#63662 = CARTESIAN_POINT('',(-41.7,354.45,-30.)) ;
#63663 = CARTESIAN_POINT('Origin',(-45.,354.45,-30.)) ;
#63664 = CARTESIAN_POINT('',(-41.7,354.45,-24.)) ;
#63665 = CARTESIAN_POINT('',(-41.7,354.45,-22.)) ;
#63666 = CARTESIAN_POINT('Origin',(-45.,354.45,-24.)) ;
#63667 = CARTESIAN_POINT('Origin',(0.,309.45,-22.)) ;
#63668 = CARTESIAN_POINT('',(3.3,309.45,-30.)) ;
#63669 = CARTESIAN_POINT('Origin',(0.,309.45,-30.)) ;
#63670 = CARTESIAN_POINT('',(3.3,309.45,-24.)) ;
#63671 = CARTESIAN_POINT('',(3.3,309.45,-22.)) ;
#63672 = CARTESIAN_POINT('Origin',(0.,309.45,-24.)) ;
#63673 = CARTESIAN_POINT('Origin',(-31.8198051533946,322.630194846605,-22.)) ;
#63674 = CARTESIAN_POINT('',(-28.5198051533946,322.630194846605,-30.)) ;
#63675 = CARTESIAN_POINT('Origin',(-31.8198051533946,322.630194846605,-30.)) ;
#63676 = CARTESIAN_POINT('',(-28.5198051533946,322.630194846605,-24.)) ;
#63677 = CARTESIAN_POINT('',(-28.5198051533946,322.630194846605,-22.)) ;
#63678 = CARTESIAN_POINT('Origin',(-31.8198051533946,322.630194846605,-24.)) ;
#63679 = CARTESIAN_POINT('Origin',(-31.8198051533946,386.269805153395,-22.)) ;
#63680 = CARTESIAN_POINT('',(-28.5198051533946,386.269805153395,-30.)) ;
#63681 = CARTESIAN_POINT('Origin',(-31.8198051533946,386.269805153395,-30.)) ;
#63682 = CARTESIAN_POINT('',(-28.5198051533946,386.269805153395,-24.)) ;
#63683 = CARTESIAN_POINT('',(-28.5198051533946,386.269805153395,-22.)) ;
#63684 = CARTESIAN_POINT('Origin',(-31.8198051533946,386.269805153395,-24.)) ;
#63685 = CARTESIAN_POINT('Origin',(31.8198051533946,386.269805153395,-22.)) ;
#63686 = CARTESIAN_POINT('',(35.1198051533946,386.269805153395,-30.)) ;
#63687 = CARTESIAN_POINT('Origin',(31.8198051533946,386.269805153395,-30.)) ;
#63688 = CARTESIAN_POINT('',(35.1198051533946,386.269805153395,-24.)) ;
#63689 = CARTESIAN_POINT('',(35.1198051533946,386.269805153395,-22.)) ;
#63690 = CARTESIAN_POINT('Origin',(31.8198051533946,386.269805153395,-24.)) ;
#63691 = CARTESIAN_POINT('Origin',(31.8198051533946,322.630194846605,-22.)) ;
#63692 = CARTESIAN_POINT('',(35.1198051533946,322.630194846605,-30.)) ;
#63693 = CARTESIAN_POINT('Origin',(31.8198051533946,322.630194846605,-30.)) ;
#63694 = CARTESIAN_POINT('',(35.1198051533946,322.630194846605,-24.)) ;
#63695 = CARTESIAN_POINT('',(35.1198051533946,322.630194846605,-22.)) ;
#63696 = CARTESIAN_POINT('Origin',(31.8198051533946,322.630194846605,-24.)) ;
#63697 = CARTESIAN_POINT('Origin',(0.,354.45,-24.)) ;
#63698 = CARTESIAN_POINT('',(-33.5,354.45,-24.)) ;
#63699 = CARTESIAN_POINT('Origin',(0.,354.45,-24.)) ;
#63700 = CARTESIAN_POINT('',(-33.5,354.45,-30.)) ;
#63701 = CARTESIAN_POINT('',(-33.5,354.45,-24.)) ;
#63702 = CARTESIAN_POINT('Origin',(0.,354.45,-30.)) ;
#63703 = CARTESIAN_POINT('Origin',(0.,354.45,-24.)) ;
#63704 = CARTESIAN_POINT('',(-50.,354.45,-30.)) ;
#63705 = CARTESIAN_POINT('Origin',(0.,354.45,-30.)) ;
#63706 = CARTESIAN_POINT('',(-50.,354.45,-24.)) ;
#63707 = CARTESIAN_POINT('',(-50.,354.45,-24.)) ;
#63708 = CARTESIAN_POINT('Origin',(0.,354.45,-24.)) ;
#63709 = CARTESIAN_POINT('Origin',(0.,354.45,-24.)) ;
#63710 = CARTESIAN_POINT('Origin',(0.,354.45,-30.)) ;
#63711 = CARTESIAN_POINT('',(0.,0.,0.)) ;
#63712 = CARTESIAN_POINT('Origin',(45.,354.45,-156.)) ;
#63713 = CARTESIAN_POINT('',(48.3,354.45,-154.)) ;
#63714 = CARTESIAN_POINT('Origin',(45.,354.45,-154.)) ;
#63715 = CARTESIAN_POINT('',(48.3,354.45,-148.)) ;
#63716 = CARTESIAN_POINT('',(48.3,354.45,-156.)) ;
#63717 = CARTESIAN_POINT('Origin',(45.,354.45,-148.)) ;
#63718 = CARTESIAN_POINT('Origin',(-5.51091059616308E-15,399.45,-156.)) ;
#63719 = CARTESIAN_POINT('',(3.29999999999999,399.45,-154.)) ;
#63720 = CARTESIAN_POINT('Origin',(-5.51091059616308E-15,399.45,-154.)) ;
#63721 = CARTESIAN_POINT('',(3.29999999999999,399.45,-148.)) ;
#63722 = CARTESIAN_POINT('',(3.29999999999999,399.45,-156.)) ;
#63723 = CARTESIAN_POINT('Origin',(-5.51091059616308E-15,399.45,-148.)) ;
#63724 = CARTESIAN_POINT('Origin',(-45.,354.45,-156.)) ;
#63725 = CARTESIAN_POINT('',(-41.7,354.45,-154.)) ;
#63726 = CARTESIAN_POINT('Origin',(-45.,354.45,-154.)) ;
#63727 = CARTESIAN_POINT('',(-41.7,354.45,-148.)) ;
#63728 = CARTESIAN_POINT('',(-41.7,354.45,-156.)) ;
#63729 = CARTESIAN_POINT('Origin',(-45.,354.45,-148.)) ;
#63730 = CARTESIAN_POINT('Origin',(4.10374200494004E-30,309.45,-156.)) ;
#63731 = CARTESIAN_POINT('',(3.3,309.45,-154.)) ;
#63732 = CARTESIAN_POINT('Origin',(4.15304581151636E-30,309.45,-154.)) ;
#63733 = CARTESIAN_POINT('',(3.3,309.45,-148.)) ;
#63734 = CARTESIAN_POINT('',(3.3,309.45,-156.)) ;
#63735 = CARTESIAN_POINT('Origin',(4.3009572312453E-30,309.45,-148.)) ;
#63736 = CARTESIAN_POINT('Origin',(-31.8198051533946,322.630194846605,-156.)) ;
#63737 = CARTESIAN_POINT('',(-28.5198051533946,322.630194846605,-154.)) ;
#63738 = CARTESIAN_POINT('Origin',(-31.8198051533946,322.630194846605,-154.)) ;
#63739 = CARTESIAN_POINT('',(-28.5198051533946,322.630194846605,-148.)) ;
#63740 = CARTESIAN_POINT('',(-28.5198051533946,322.630194846605,-156.)) ;
#63741 = CARTESIAN_POINT('Origin',(-31.8198051533946,322.630194846605,-148.)) ;
#63742 = CARTESIAN_POINT('Origin',(-31.8198051533946,386.269805153395,-156.)) ;
#63743 = CARTESIAN_POINT('',(-28.5198051533946,386.269805153395,-154.)) ;
#63744 = CARTESIAN_POINT('Origin',(-31.8198051533946,386.269805153395,-154.)) ;
#63745 = CARTESIAN_POINT('',(-28.5198051533946,386.269805153395,-148.)) ;
#63746 = CARTESIAN_POINT('',(-28.5198051533946,386.269805153395,-156.)) ;
#63747 = CARTESIAN_POINT('Origin',(-31.8198051533946,386.269805153395,-148.)) ;
#63748 = CARTESIAN_POINT('Origin',(31.8198051533946,386.269805153395,-156.)) ;
#63749 = CARTESIAN_POINT('',(35.1198051533946,386.269805153395,-154.)) ;
#63750 = CARTESIAN_POINT('Origin',(31.8198051533946,386.269805153395,-154.)) ;
#63751 = CARTESIAN_POINT('',(35.1198051533946,386.269805153395,-148.)) ;
#63752 = CARTESIAN_POINT('',(35.1198051533946,386.269805153395,-156.)) ;
#63753 = CARTESIAN_POINT('Origin',(31.8198051533946,386.269805153395,-148.)) ;
#63754 = CARTESIAN_POINT('Origin',(31.8198051533946,322.630194846605,-156.)) ;
#63755 = CARTESIAN_POINT('',(35.1198051533946,322.630194846605,-154.)) ;
#63756 = CARTESIAN_POINT('Origin',(31.8198051533946,322.630194846605,-154.)) ;
#63757 = CARTESIAN_POINT('',(35.1198051533946,322.630194846605,-148.)) ;
#63758 = CARTESIAN_POINT('',(35.1198051533946,322.630194846605,-156.)) ;
#63759 = CARTESIAN_POINT('Origin',(31.8198051533946,322.630194846605,-148.)) ;
#63760 = CARTESIAN_POINT('Origin',(4.67094209837054E-30,354.45,-154.)) ;
#63761 = CARTESIAN_POINT('',(-33.5,354.45,-148.)) ;
#63762 = CARTESIAN_POINT('Origin',(4.81885351809948E-30,354.45,-148.)) ;
#63763 = CARTESIAN_POINT('',(-33.5,354.45,-154.)) ;
#63764 = CARTESIAN_POINT('',(-33.5,354.45,-154.)) ;
#63765 = CARTESIAN_POINT('Origin',(4.67094209837054E-30,354.45,-154.)) ;
#63766 = CARTESIAN_POINT('Origin',(4.67094209837054E-30,354.45,-154.)) ;
#63767 = CARTESIAN_POINT('',(-50.,354.45,-154.)) ;
#63768 = CARTESIAN_POINT('Origin',(4.67094209837054E-30,354.45,-154.)) ;
#63769 = CARTESIAN_POINT('',(-50.,354.45,-148.)) ;
#63770 = CARTESIAN_POINT('',(-50.,354.45,-154.)) ;
#63771 = CARTESIAN_POINT('Origin',(4.81885351809948E-30,354.45,-148.)) ;
#63772 = CARTESIAN_POINT('Origin',(4.67094209837054E-30,354.45,-154.)) ;
#63773 = CARTESIAN_POINT('Origin',(4.81885351809948E-30,354.45,-148.)) ;
#63774 = CARTESIAN_POINT('',(0.,0.,0.)) ;
#63775 = CARTESIAN_POINT('',(0.,0.,0.)) ;
#63776 = CARTESIAN_POINT('',(0.,0.,0.)) ;
#63777 = CARTESIAN_POINT('',(1.4210854715202E-13,354.45,-154.)) ;
#63778 = CARTESIAN_POINT('',(0.,0.,-178.)) ;
#63779 = CARTESIAN_POINT('',(0.,-1.4210854715202E-15,3.5527136788005E-16)) ;
#63780 = CARTESIAN_POINT('',(1.4210854715202E-13,354.45,-233.999999999999)) ;
#63781 = CARTESIAN_POINT('',(1.4210854715202E-13,354.45,-174.)) ;
#63782 = CARTESIAN_POINT('',(5.00000000000007,377.25,19.4999999999999)) ;
#63783 = CARTESIAN_POINT('',(1.4210854715202E-13,354.45,12.9999999999999)) ;
#63784 = CARTESIAN_POINT('',(1.4210854715202E-13,354.45,57.9999999999999)) ;
#63785 = CARTESIAN_POINT('',(1.4210854715202E-13,354.45,57.9999999999999)) ;
#63786 = CARTESIAN_POINT('',(2.1316282072803E-13,354.45,88.0000000000001)) ;
#63787 = CARTESIAN_POINT('',(1.4210854715202E-13,354.45,-23.9999999999999)) ;
#63788 = CARTESIAN_POINT('',(1.4210854715202E-13,354.45,3.5527136788005E-14)) ;
#63789 = CARTESIAN_POINT('',(0.,0.,0.)) ;
#63790 = CARTESIAN_POINT('',(0.,0.,0.)) ;
#63791 = UNCERTAINTY_MEASURE_WITH_UNIT(LENGTH_MEASURE(0.01),#63825,
'DISTANCE_ACCURACY_VALUE',
'Maximum model space distance between geometric entities at asserted c
onnectivities') ;
#63792 = UNCERTAINTY_MEASURE_WITH_UNIT(LENGTH_MEASURE(0.01),#63825,
'DISTANCE_ACCURACY_VALUE',
'Maximum model space distance between geometric entities at asserted c
onnectivities') ;
#63793 = UNCERTAINTY_MEASURE_WITH_UNIT(LENGTH_MEASURE(0.01),#63825,
'DISTANCE_ACCURACY_VALUE',
'Maximum model space distance between geometric entities at asserted c
onnectivities') ;
#63794 = UNCERTAINTY_MEASURE_WITH_UNIT(LENGTH_MEASURE(0.01),#63825,
'DISTANCE_ACCURACY_VALUE',
'Maximum model space distance between geometric entities at asserted c
onnectivities') ;
#63795 = UNCERTAINTY_MEASURE_WITH_UNIT(LENGTH_MEASURE(0.01),#63825,
'DISTANCE_ACCURACY_VALUE',
'Maximum model space distance between geometric entities at asserted c
onnectivities') ;
#63796 = UNCERTAINTY_MEASURE_WITH_UNIT(LENGTH_MEASURE(0.01),#63825,
'DISTANCE_ACCURACY_VALUE',
'Maximum model space distance between geometric entities at asserted c
onnectivities') ;
#63797 = UNCERTAINTY_MEASURE_WITH_UNIT(LENGTH_MEASURE(0.01),#63825,
'DISTANCE_ACCURACY_VALUE',
'Maximum model space distance between geometric entities at asserted c
onnectivities') ;
#63798 = UNCERTAINTY_MEASURE_WITH_UNIT(LENGTH_MEASURE(0.01),#63825,
'DISTANCE_ACCURACY_VALUE',
'Maximum model space distance between geometric entities at asserted c
onnectivities') ;
#63799 = UNCERTAINTY_MEASURE_WITH_UNIT(LENGTH_MEASURE(0.01),#63825,
'DISTANCE_ACCURACY_VALUE',
'Maximum model space distance between geometric entities at asserted c
onnectivities') ;
#63800 = UNCERTAINTY_MEASURE_WITH_UNIT(LENGTH_MEASURE(0.01),#63825,
'DISTANCE_ACCURACY_VALUE',
'Maximum model space distance between geometric entities at asserted c
onnectivities') ;
#63801 = UNCERTAINTY_MEASURE_WITH_UNIT(LENGTH_MEASURE(0.01),#63825,
'DISTANCE_ACCURACY_VALUE',
'Maximum model space distance between geometric entities at asserted c
onnectivities') ;
#63802 = UNCERTAINTY_MEASURE_WITH_UNIT(LENGTH_MEASURE(0.01),#63825,
'DISTANCE_ACCURACY_VALUE',
'Maximum model space distance between geometric entities at asserted c
onnectivities') ;
#63803 = UNCERTAINTY_MEASURE_WITH_UNIT(LENGTH_MEASURE(0.01),#63825,
'DISTANCE_ACCURACY_VALUE',
'Maximum model space distance between geometric entities at asserted c
onnectivities') ;
#63804 = UNCERTAINTY_MEASURE_WITH_UNIT(LENGTH_MEASURE(0.01),#63825,
'DISTANCE_ACCURACY_VALUE',
'Maximum model space distance between geometric entities at asserted c
onnectivities') ;
#63805 = UNCERTAINTY_MEASURE_WITH_UNIT(LENGTH_MEASURE(0.01),#63825,
'DISTANCE_ACCURACY_VALUE',
'Maximum model space distance between geometric entities at asserted c
onnectivities') ;
#63806 = UNCERTAINTY_MEASURE_WITH_UNIT(LENGTH_MEASURE(0.01),#63825,
'DISTANCE_ACCURACY_VALUE',
'Maximum model space distance between geometric entities at asserted c
onnectivities') ;
#63807 = UNCERTAINTY_MEASURE_WITH_UNIT(LENGTH_MEASURE(0.01),#63825,
'DISTANCE_ACCURACY_VALUE',
'Maximum model space distance between geometric entities at asserted c
onnectivities') ;
#63808 = (
GEOMETRIC_REPRESENTATION_CONTEXT(3)
GLOBAL_UNCERTAINTY_ASSIGNED_CONTEXT((#63791))
GLOBAL_UNIT_ASSIGNED_CONTEXT((#63825,#63827,#63828))
REPRESENTATION_CONTEXT('','3D')
) ;
#63809 = (
GEOMETRIC_REPRESENTATION_CONTEXT(3)
GLOBAL_UNCERTAINTY_ASSIGNED_CONTEXT((#63792))
GLOBAL_UNIT_ASSIGNED_CONTEXT((#63825,#63827,#63828))
REPRESENTATION_CONTEXT('','3D')
) ;
#63810 = (
GEOMETRIC_REPRESENTATION_CONTEXT(3)
GLOBAL_UNCERTAINTY_ASSIGNED_CONTEXT((#63793))
GLOBAL_UNIT_ASSIGNED_CONTEXT((#63825,#63827,#63828))
REPRESENTATION_CONTEXT('','3D')
) ;
#63811 = (
GEOMETRIC_REPRESENTATION_CONTEXT(3)
GLOBAL_UNCERTAINTY_ASSIGNED_CONTEXT((#63794))
GLOBAL_UNIT_ASSIGNED_CONTEXT((#63825,#63827,#63828))
REPRESENTATION_CONTEXT('','3D')
) ;
#63812 = (
GEOMETRIC_REPRESENTATION_CONTEXT(3)
GLOBAL_UNCERTAINTY_ASSIGNED_CONTEXT((#63795))
GLOBAL_UNIT_ASSIGNED_CONTEXT((#63825,#63827,#63828))
REPRESENTATION_CONTEXT('','3D')
) ;
#63813 = (
GEOMETRIC_REPRESENTATION_CONTEXT(3)
GLOBAL_UNCERTAINTY_ASSIGNED_CONTEXT((#63796))
GLOBAL_UNIT_ASSIGNED_CONTEXT((#63825,#63827,#63828))
REPRESENTATION_CONTEXT('','3D')
) ;
#63814 = (
GEOMETRIC_REPRESENTATION_CONTEXT(3)
GLOBAL_UNCERTAINTY_ASSIGNED_CONTEXT((#63797))
GLOBAL_UNIT_ASSIGNED_CONTEXT((#63825,#63827,#63828))
REPRESENTATION_CONTEXT('','3D')
) ;
#63815 = (
GEOMETRIC_REPRESENTATION_CONTEXT(3)
GLOBAL_UNCERTAINTY_ASSIGNED_CONTEXT((#63798))
GLOBAL_UNIT_ASSIGNED_CONTEXT((#63825,#63827,#63828))
REPRESENTATION_CONTEXT('','3D')
) ;
#63816 = (
GEOMETRIC_REPRESENTATION_CONTEXT(3)
GLOBAL_UNCERTAINTY_ASSIGNED_CONTEXT((#63799))
GLOBAL_UNIT_ASSIGNED_CONTEXT((#63825,#63827,#63828))
REPRESENTATION_CONTEXT('','3D')
) ;
#63817 = (
GEOMETRIC_REPRESENTATION_CONTEXT(3)
GLOBAL_UNCERTAINTY_ASSIGNED_CONTEXT((#63800))
GLOBAL_UNIT_ASSIGNED_CONTEXT((#63825,#63827,#63828))
REPRESENTATION_CONTEXT('','3D')
) ;
#63818 = (
GEOMETRIC_REPRESENTATION_CONTEXT(3)
GLOBAL_UNCERTAINTY_ASSIGNED_CONTEXT((#63801))
GLOBAL_UNIT_ASSIGNED_CONTEXT((#63825,#63827,#63828))
REPRESENTATION_CONTEXT('','3D')
) ;
#63819 = (
GEOMETRIC_REPRESENTATION_CONTEXT(3)
GLOBAL_UNCERTAINTY_ASSIGNED_CONTEXT((#63802))
GLOBAL_UNIT_ASSIGNED_CONTEXT((#63825,#63827,#63828))
REPRESENTATION_CONTEXT('','3D')
) ;
#63820 = (
GEOMETRIC_REPRESENTATION_CONTEXT(3)
GLOBAL_UNCERTAINTY_ASSIGNED_CONTEXT((#63803))
GLOBAL_UNIT_ASSIGNED_CONTEXT((#63825,#63827,#63828))
REPRESENTATION_CONTEXT('','3D')
) ;
#63821 = (
GEOMETRIC_REPRESENTATION_CONTEXT(3)
GLOBAL_UNCERTAINTY_ASSIGNED_CONTEXT((#63804))
GLOBAL_UNIT_ASSIGNED_CONTEXT((#63825,#63827,#63828))
REPRESENTATION_CONTEXT('','3D')
) ;
#63822 = (
GEOMETRIC_REPRESENTATION_CONTEXT(3)
GLOBAL_UNCERTAINTY_ASSIGNED_CONTEXT((#63805))
GLOBAL_UNIT_ASSIGNED_CONTEXT((#63825,#63827,#63828))
REPRESENTATION_CONTEXT('','3D')
) ;
#63823 = (
GEOMETRIC_REPRESENTATION_CONTEXT(3)
GLOBAL_UNCERTAINTY_ASSIGNED_CONTEXT((#63806))
GLOBAL_UNIT_ASSIGNED_CONTEXT((#63825,#63827,#63828))
REPRESENTATION_CONTEXT('','3D')
) ;
#63824 = (
GEOMETRIC_REPRESENTATION_CONTEXT(3)
GLOBAL_UNCERTAINTY_ASSIGNED_CONTEXT((#63807))
GLOBAL_UNIT_ASSIGNED_CONTEXT((#63825,#63827,#63828))
REPRESENTATION_CONTEXT('','3D')
) ;
#63825 = (
LENGTH_UNIT()
NAMED_UNIT(*)
SI_UNIT(.MILLI.,.METRE.)
) ;
#63826 = (
LENGTH_UNIT()
NAMED_UNIT(*)
SI_UNIT($,.METRE.)
) ;
#63827 = (
NAMED_UNIT(*)
PLANE_ANGLE_UNIT()
SI_UNIT($,.RADIAN.)
) ;
#63828 = (
NAMED_UNIT(*)
SI_UNIT($,.STERADIAN.)
SOLID_ANGLE_UNIT()
) ;
#63829 = SHAPE_DEFINITION_REPRESENTATION(#63845,#63878) ;
#63830 = SHAPE_DEFINITION_REPRESENTATION(#63846,#63879) ;
#63831 = SHAPE_DEFINITION_REPRESENTATION(#63847,#63880) ;
#63832 = SHAPE_DEFINITION_REPRESENTATION(#63848,#63881) ;
#63833 = SHAPE_DEFINITION_REPRESENTATION(#63849,#63882) ;
#63834 = SHAPE_DEFINITION_REPRESENTATION(#63850,#63883) ;
#63835 = SHAPE_DEFINITION_REPRESENTATION(#63851,#63884) ;
#63836 = SHAPE_DEFINITION_REPRESENTATION(#63852,#63885) ;
#63837 = SHAPE_DEFINITION_REPRESENTATION(#63853,#63886) ;
#63838 = SHAPE_DEFINITION_REPRESENTATION(#63854,#63887) ;
#63839 = SHAPE_DEFINITION_REPRESENTATION(#63855,#63888) ;
#63840 = SHAPE_DEFINITION_REPRESENTATION(#63856,#63889) ;
#63841 = SHAPE_DEFINITION_REPRESENTATION(#63857,#63890) ;
#63842 = SHAPE_DEFINITION_REPRESENTATION(#63858,#63891) ;
#63843 = SHAPE_DEFINITION_REPRESENTATION(#63859,#63892) ;
#63844 = SHAPE_DEFINITION_REPRESENTATION(#63860,#63893) ;
#63845 = PRODUCT_DEFINITION_SHAPE('',$,#63895) ;
#63846 = PRODUCT_DEFINITION_SHAPE('',$,#63896) ;
#63847 = PRODUCT_DEFINITION_SHAPE('',$,#63897) ;
#63848 = PRODUCT_DEFINITION_SHAPE('',$,#63898) ;
#63849 = PRODUCT_DEFINITION_SHAPE('',$,#63899) ;
#63850 = PRODUCT_DEFINITION_SHAPE('',$,#63900) ;
#63851 = PRODUCT_DEFINITION_SHAPE('',$,#63901) ;
#63852 = PRODUCT_DEFINITION_SHAPE('',$,#63902) ;
#63853 = PRODUCT_DEFINITION_SHAPE('',$,#63903) ;
#63854 = PRODUCT_DEFINITION_SHAPE('',$,#63904) ;
#63855 = PRODUCT_DEFINITION_SHAPE('',$,#63905) ;
#63856 = PRODUCT_DEFINITION_SHAPE('',$,#63906) ;
#63857 = PRODUCT_DEFINITION_SHAPE('',$,#63907) ;
#63858 = PRODUCT_DEFINITION_SHAPE('',$,#63908) ;
#63859 = PRODUCT_DEFINITION_SHAPE('',$,#63909) ;
#63860 = PRODUCT_DEFINITION_SHAPE('',$,#63910) ;
#63861 = PRODUCT_DEFINITION_SHAPE($,$,#62) ;
#63862 = PRODUCT_DEFINITION_SHAPE($,$,#63) ;
#63863 = PRODUCT_DEFINITION_SHAPE($,$,#64) ;
#63864 = PRODUCT_DEFINITION_SHAPE($,$,#65) ;
#63865 = PRODUCT_DEFINITION_SHAPE($,$,#66) ;
#63866 = PRODUCT_DEFINITION_SHAPE($,$,#67) ;
#63867 = PRODUCT_DEFINITION_SHAPE($,$,#68) ;
#63868 = PRODUCT_DEFINITION_SHAPE($,$,#69) ;
#63869 = PRODUCT_DEFINITION_SHAPE($,$,#70) ;
#63870 = PRODUCT_DEFINITION_SHAPE($,$,#71) ;
#63871 = PRODUCT_DEFINITION_SHAPE($,$,#72) ;
#63872 = PRODUCT_DEFINITION_SHAPE($,$,#73) ;
#63873 = PRODUCT_DEFINITION_SHAPE($,$,#74) ;
#63874 = PRODUCT_DEFINITION_SHAPE($,$,#75) ;
#63875 = PRODUCT_DEFINITION_SHAPE($,$,#76) ;
#63876 = PRODUCT_DEFINITION_SHAPE($,$,#77) ;
#63877 = PRODUCT_DEFINITION_SHAPE($,$,#78) ;
#63878 = SHAPE_REPRESENTATION('',(#15675,#17885,#17886,#17887,#17888,#17889,
#17890,#17891,#17892,#17893,#17894,#17895,#17896,#17897,#17898,#17899,#17900,
#17901),#63808) ;
#63879 = SHAPE_REPRESENTATION('',(#15676),#63809) ;
#63880 = SHAPE_REPRESENTATION('',(#15762),#63810) ;
#63881 = SHAPE_REPRESENTATION('',(#15853),#63811) ;
#63882 = SHAPE_REPRESENTATION('',(#15892),#63812) ;
#63883 = SHAPE_REPRESENTATION('',(#15986),#63813) ;
#63884 = SHAPE_REPRESENTATION('',(#16025),#63814) ;
#63885 = SHAPE_REPRESENTATION('',(#16168),#63815) ;
#63886 = SHAPE_REPRESENTATION('',(#16191),#63816) ;
#63887 = SHAPE_REPRESENTATION('',(#16208),#63817) ;
#63888 = SHAPE_REPRESENTATION('',(#17207),#63818) ;
#63889 = SHAPE_REPRESENTATION('',(#17226),#63819) ;
#63890 = SHAPE_REPRESENTATION('',(#17272),#63820) ;
#63891 = SHAPE_REPRESENTATION('',(#17802),#63821) ;
#63892 = SHAPE_REPRESENTATION('',(#17819),#63822) ;
#63893 = SHAPE_REPRESENTATION('',(#17852),#63823) ;
#63894 = PRODUCT_DEFINITION_CONTEXT('part definition',#63944,'design') ;
#63895 = PRODUCT_DEFINITION('MAS-645','MAS-645',#63911,
#63894) ;
#63896 = PRODUCT_DEFINITION('Back_Plate','Back_Plate',#63912,#63894) ;
#63897 = PRODUCT_DEFINITION('Bottom_Plate','Bottom_Plate',#63913,#63894) ;
#63898 = PRODUCT_DEFINITION('Side_Plate_1','Side_Plate_1',#63914,#63894) ;
#63899 = PRODUCT_DEFINITION('Front_Plate','Front_Plate',#63915,#63894) ;
#63900 = PRODUCT_DEFINITION('Side_Plate_2','Side_Plate_2',#63916,#63894) ;
#63901 = PRODUCT_DEFINITION('Spindle','Spindle',#63917,#63894) ;
#63902 = PRODUCT_DEFINITION('Key','Key',#63918,#63894) ;
#63903 = PRODUCT_DEFINITION('Spacer_2','Spacer_2',#63919,#63894) ;
#63904 = PRODUCT_DEFINITION('Drive_Pulley','Drive_Pulley',#63920,#63894) ;
#63905 = PRODUCT_DEFINITION('Bushing','Bushing',#63921,#63894) ;
#63906 = PRODUCT_DEFINITION('Bearing_Lock_Nut','Bearing_Lock_Nut',#63922,
#63894) ;
#63907 = PRODUCT_DEFINITION('Taper_Roller_Bearing','Taper_Roller_Bearing',
#63923,#63894) ;
#63908 = PRODUCT_DEFINITION('Spacer_1','Spacer_1',#63924,#63894) ;
#63909 = PRODUCT_DEFINITION('Back_Plate_Retainer_Ring',
'Back_Plate_Retainer_Ring',#63925,#63894) ;
#63910 = PRODUCT_DEFINITION('Front_Plate_Retainer_Ring',
'Front_Plate_Retainer_Ring',#63926,#63894) ;
#63911 = PRODUCT_DEFINITION_FORMATION('',$,#63946) ;
#63912 = PRODUCT_DEFINITION_FORMATION('',$,#63947) ;
#63913 = PRODUCT_DEFINITION_FORMATION('',$,#63948) ;
#63914 = PRODUCT_DEFINITION_FORMATION('',$,#63949) ;
#63915 = PRODUCT_DEFINITION_FORMATION('',$,#63950) ;
#63916 = PRODUCT_DEFINITION_FORMATION('',$,#63951) ;
#63917 = PRODUCT_DEFINITION_FORMATION('',$,#63952) ;
#63918 = PRODUCT_DEFINITION_FORMATION('',$,#63953) ;
#63919 = PRODUCT_DEFINITION_FORMATION('',$,#63954) ;
#63920 = PRODUCT_DEFINITION_FORMATION('',$,#63955) ;
#63921 = PRODUCT_DEFINITION_FORMATION('',$,#63956) ;
#63922 = PRODUCT_DEFINITION_FORMATION('',$,#63957) ;
#63923 = PRODUCT_DEFINITION_FORMATION('',$,#63958) ;
#63924 = PRODUCT_DEFINITION_FORMATION('',$,#63959) ;
#63925 = PRODUCT_DEFINITION_FORMATION('',$,#63960) ;
#63926 = PRODUCT_DEFINITION_FORMATION('',$,#63961) ;
#63927 = PRODUCT_RELATED_PRODUCT_CATEGORY('MAS-645',
'MAS-645',(#63946)) ;
#63928 = PRODUCT_RELATED_PRODUCT_CATEGORY('Back_Plate','Back_Plate',(#63947)) ;
#63929 = PRODUCT_RELATED_PRODUCT_CATEGORY('Bottom_Plate','Bottom_Plate',(#63948)) ;
#63930 = PRODUCT_RELATED_PRODUCT_CATEGORY('Side_Plate_1','Side_Plate_1',(#63949)) ;
#63931 = PRODUCT_RELATED_PRODUCT_CATEGORY('Front_Plate','Front_Plate',(#63950)) ;
#63932 = PRODUCT_RELATED_PRODUCT_CATEGORY('Side_Plate_2','Side_Plate_2',(#63951)) ;
#63933 = PRODUCT_RELATED_PRODUCT_CATEGORY('Spindle','Spindle',(#63952)) ;
#63934 = PRODUCT_RELATED_PRODUCT_CATEGORY('Key','Key',(#63953)) ;
#63935 = PRODUCT_RELATED_PRODUCT_CATEGORY('Spacer_2','Spacer_2',(#63954)) ;
#63936 = PRODUCT_RELATED_PRODUCT_CATEGORY('Drive_Pulley','Drive_Pulley',(#63955)) ;
#63937 = PRODUCT_RELATED_PRODUCT_CATEGORY('Bushing','Bushing',(#63956)) ;
#63938 = PRODUCT_RELATED_PRODUCT_CATEGORY('Bearing_Lock_Nut',
'Bearing_Lock_Nut',(#63957)) ;
#63939 = PRODUCT_RELATED_PRODUCT_CATEGORY('Taper_Roller_Bearing',
'Taper_Roller_Bearing',(#63958)) ;
#63940 = PRODUCT_RELATED_PRODUCT_CATEGORY('Spacer_1','Spacer_1',(#63959)) ;
#63941 = PRODUCT_RELATED_PRODUCT_CATEGORY('Back_Plate_Retainer_Ring',
'Back_Plate_Retainer_Ring',(#63960)) ;
#63942 = PRODUCT_RELATED_PRODUCT_CATEGORY('Front_Plate_Retainer_Ring',
'Front_Plate_Retainer_Ring',(#63961)) ;
#63943 = APPLICATION_PROTOCOL_DEFINITION('international standard',
'automotive_design',2009,#63944) ;
#63944 = APPLICATION_CONTEXT(
'Core Data for Automotive Mechanical Design Process') ;
#63945 = PRODUCT_CONTEXT('part definition',#63944,'mechanical') ;
#63946 = PRODUCT('MAS-645','MAS-645',$,(#63945)) ;
#63947 = PRODUCT('Back_Plate','Back_Plate',$,(#63945)) ;
#63948 = PRODUCT('Bottom_Plate','Bottom_Plate',$,(#63945)) ;
#63949 = PRODUCT('Side_Plate_1','Side_Plate_1',$,(#63945)) ;
#63950 = PRODUCT('Front_Plate','Front_Plate',$,(#63945)) ;
#63951 = PRODUCT('Side_Plate_2','Side_Plate_2',$,(#63945)) ;
#63952 = PRODUCT('Spindle','Spindle',$,(#63945)) ;
#63953 = PRODUCT('Key','Key',$,(#63945)) ;
#63954 = PRODUCT('Spacer_2','Spacer_2',$,(#63945)) ;
#63955 = PRODUCT('Drive_Pulley','Drive_Pulley',$,(#63945)) ;
#63956 = PRODUCT('Bushing','Bushing',$,(#63945)) ;
#63957 = PRODUCT('Bearing_Lock_Nut','Bearing_Lock_Nut',$,(#63945)) ;
#63958 = PRODUCT('Taper_Roller_Bearing','Taper_Roller_Bearing',$,(#63945)) ;
#63959 = PRODUCT('Spacer_1','Spacer_1',$,(#63945)) ;
#63960 = PRODUCT('Back_Plate_Retainer_Ring','Back_Plate_Retainer_Ring',$,
(#63945)) ;
#63961 = PRODUCT('Front_Plate_Retainer_Ring','Front_Plate_Retainer_Ring',
$,(#63945)) ;
#63962 = PRESENTATION_STYLE_ASSIGNMENT((#63967)) ;
#63963 = PRESENTATION_STYLE_ASSIGNMENT((#63968)) ;
#63964 = PRESENTATION_STYLE_ASSIGNMENT((#63969)) ;
#63965 = PRESENTATION_STYLE_ASSIGNMENT((#63970)) ;
#63966 = PRESENTATION_STYLE_ASSIGNMENT((#63971)) ;
#63967 = SURFACE_STYLE_USAGE(.BOTH.,#63972) ;
#63968 = SURFACE_STYLE_USAGE(.BOTH.,#63973) ;
#63969 = SURFACE_STYLE_USAGE(.BOTH.,#63974) ;
#63970 = SURFACE_STYLE_USAGE(.BOTH.,#63975) ;
#63971 = SURFACE_STYLE_USAGE(.BOTH.,#63976) ;
#63972 = SURFACE_SIDE_STYLE('',(#63977)) ;
#63973 = SURFACE_SIDE_STYLE('',(#63978)) ;
#63974 = SURFACE_SIDE_STYLE('',(#63979)) ;
#63975 = SURFACE_SIDE_STYLE('',(#63980)) ;
#63976 = SURFACE_SIDE_STYLE('',(#63981)) ;
#63977 = SURFACE_STYLE_FILL_AREA(#63982) ;
#63978 = SURFACE_STYLE_FILL_AREA(#63983) ;
#63979 = SURFACE_STYLE_FILL_AREA(#63984) ;
#63980 = SURFACE_STYLE_FILL_AREA(#63985) ;
#63981 = SURFACE_STYLE_FILL_AREA(#63986) ;
#63982 = FILL_AREA_STYLE('Steel - Satin',(#63987)) ;
#63983 = FILL_AREA_STYLE('Opaque(160,160,160)',(#63988)) ;
#63984 = FILL_AREA_STYLE('Opaque(203,203,203)',(#63989)) ;
#63985 = FILL_AREA_STYLE('Opaque(245,245,246)',(#63990)) ;
#63986 = FILL_AREA_STYLE('Opaque(115,115,115)',(#63991)) ;
#63987 = FILL_AREA_STYLE_COLOUR('Steel - Satin',#63992) ;
#63988 = FILL_AREA_STYLE_COLOUR('Opaque(160,160,160)',#63993) ;
#63989 = FILL_AREA_STYLE_COLOUR('Opaque(203,203,203)',#63994) ;
#63990 = FILL_AREA_STYLE_COLOUR('Opaque(245,245,246)',#63995) ;
#63991 = FILL_AREA_STYLE_COLOUR('Opaque(115,115,115)',#63996) ;
#63992 = COLOUR_RGB('Steel - Satin', 0.09019608, 0.27058824, 0.51372549) ;
#63993 = COLOUR_RGB('Opaque(160,160,160)', 0.09019608, 0.27058824, 0.51372549) ;
#63994 = COLOUR_RGB('Opaque(203,203,203)', 0.08235294, 0.09019608, 0.10196078) ;
#63995 = COLOUR_RGB('Opaque(245,245,246)', 0.31764706, 0.68627451, 0.89019608) ;
#63996 = COLOUR_RGB('Opaque(115,115,115)', 0.72549020, 0.75294118, 0.79215686) ;
ENDSEC;
END-ISO-10303-21;
